#55457 = CARTESIAN_POINT ( 'NONE',  ( -0.1872094492630000107, 1489.066837873730037, 236.5711787574979894 ) ) ;
#55458 = CARTESIAN_POINT ( 'NONE',  ( -1.499721489806784991, 1420.769012360254237, 184.5717010710991701 ) ) ;
#55459 = ORIENTED_EDGE ( 'NONE', *, *, #28161, .F. ) ;
#55460 = CARTESIAN_POINT ( 'NONE',  ( 10.81512807170000023, 1424.921141247430114, 144.1662922863980043 ) ) ;
#55461 = FACE_OUTER_BOUND ( 'NONE', #63696, .T. ) ;
#55462 = CARTESIAN_POINT ( 'NONE',  ( 0.000000000000000000, 1523.051704408389696, 209.1218459616979999 ) ) ;
#55463 = CARTESIAN_POINT ( 'NONE',  ( 7.713117802984999827, 1516.690345681169902, 204.1174038931170003 ) ) ;
#55464 = EDGE_LOOP ( 'NONE', ( #67726, #88657, #12171, #80779 ) ) ;
#55465 = CARTESIAN_POINT ( 'NONE',  ( 9.534480203992039549, 1481.987763606179897, 216.0982299746490014 ) ) ;
#55466 = CIRCLE ( 'NONE', #84057, 30.13701971169416183 ) ;
#55467 = CARTESIAN_POINT ( 'NONE',  ( 12.93986011685568194, 1442.913450493105529, 187.0956378267197238 ) ) ;
#55468 = ORIENTED_EDGE ( 'NONE', *, *, #54207, .T. ) ;
#55469 = VERTEX_POINT ( 'NONE', #31383 ) ;
#55470 = CARTESIAN_POINT ( 'NONE',  ( 2.127574403380531720, 1524.244163922423695, 173.7332312662435925 ) ) ;
#55471 = DIRECTION ( 'NONE',  ( -1.755985294532469921E-16, 1.000000000000000000, -1.338183447452831989E-16 ) ) ;
#55472 = CARTESIAN_POINT ( 'NONE',  ( 10.83634816680000057, 1507.403084768729968, 234.1451693812979897 ) ) ;
#55473 = B_SPLINE_CURVE_WITH_KNOTS ( 'NONE', 3,
 ( #477, #26184, #77174, #59823, #110202, #87220, #10510, #93943, #34601, #97812, #2139, #97266, #96735, #46898, #29509, #37929, #37372, #70450, #11620, #106764, #55294, #21091, #44682, #20542, #36261, #54746 ),
 .UNSPECIFIED., .F., .F.,
 ( 4, 2, 2, 2, 1, 1, 2, 2, 2, 2, 1, 1, 2, 2, 4 ),
 ( 0.000000000000000000, 0.1250000000007177869, 0.2500000000014355739, 0.3750000000021533886, 0.4375000000025118796, 0.4687500000026916247, 0.4843750000027603475, 0.5000000000028289593, 0.6250000000029628522, 0.6875000000030297986, 0.7187500000030208058, 0.7343750000030150327, 0.7421875000029918290, 0.7500000000029686253, 1.000000000000000000 ),
 .UNSPECIFIED. ) ;
#55474 = CARTESIAN_POINT ( 'NONE',  ( -3.364963321921979666, 1469.699125603920038, 218.6607286373120189 ) ) ;
#55475 = CARTESIAN_POINT ( 'NONE',  ( 14.11531660217920070, 1452.420142669970119, 148.4568864021009915 ) ) ;
#55476 = CONICAL_SURFACE ( 'NONE', #98378, 1.000000000000009104, 0.7853981633970000820 ) ;
#55477 = CARTESIAN_POINT ( 'NONE',  ( 8.765535317279999461, 1421.152484001810080, 196.5454161687989938 ) ) ;
#55478 = CARTESIAN_POINT ( 'NONE',  ( 1.874146057977200019, 1474.821289880090035, 220.3858797084459979 ) ) ;
#55479 = CARTESIAN_POINT ( 'NONE',  ( -7.116694769601350501, 1494.227560407549845, 199.0721606401010035 ) ) ;
#55480 = CARTESIAN_POINT ( 'NONE',  ( -119.8718586775642478, 1384.926148861439970, 299.5197653927720580 ) ) ;
#55481 = CARTESIAN_POINT ( 'NONE',  ( -2.500000000000000000, 1440.913060387330006, 209.1218459616979999 ) ) ;
#55483 = CARTESIAN_POINT ( 'NONE',  ( -3.509649680925187365, 1486.092192652074573, 181.9936301291397172 ) ) ;
#55482 = CARTESIAN_POINT ( 'NONE',  ( -18.65765733967990059, 1472.695501767010001, 189.9835944018950329 ) ) ;
#55484 = CARTESIAN_POINT ( 'NONE',  ( -67.00076415386901374, 1379.747503662026475, 277.9341329112440349 ) ) ;
#55485 = CARTESIAN_POINT ( 'NONE',  ( -25.25982536658409927, 1509.711778463150040, 222.8936294031860257 ) ) ;
#55486 = CARTESIAN_POINT ( 'NONE',  ( -7.719525633314999524, 1513.939092156080051, 202.0215813447470055 ) ) ;
#55487 = ORIENTED_EDGE ( 'NONE', *, *, #101556, .F. ) ;
#55488 = CARTESIAN_POINT ( 'NONE',  ( 5.995204332980000249E-15, 1425.981674191730008, 219.6133832206979832 ) ) ;
#55489 = AXIS2_PLACEMENT_3D ( 'NONE', #64370, #99584, #5550 ) ;
#55490 = CARTESIAN_POINT ( 'NONE',  ( -5.257080573758882380, 1517.051704408389924, 199.2452589303538275 ) ) ;
#55491 = CARTESIAN_POINT ( 'NONE',  ( -94.45576590239029713, 1384.959238494370084, 309.9322998303119903 ) ) ;
#55492 = CARTESIAN_POINT ( 'NONE',  ( -9.582177284329999267, 1388.523135097040040, 201.1746843562989966 ) ) ;
#55493 = CARTESIAN_POINT ( 'NONE',  ( -15.48550906000000005, 1416.155796905759871, 210.9866352200689903 ) ) ;
#55495 = ORIENTED_EDGE ( 'NONE', *, *, #80254, .T. ) ;
#55494 = CARTESIAN_POINT ( 'NONE',  ( 3.422247113165846955, 1486.244152127078905, 198.8929547559257287 ) ) ;
#55496 = CARTESIAN_POINT ( 'NONE',  ( 3.483866223379999738, 1429.087410406890058, 216.6553312436790009 ) ) ;
#55497 = DIRECTION ( 'NONE',  ( 0.5224574779883525144, -0.7067418228232951183, -0.4770263929453549823 ) ) ;
#55498 = CARTESIAN_POINT ( 'NONE',  ( -5.569019969264549452, 1475.748224554402441, 217.8649781415279278 ) ) ;
#55499 = CARTESIAN_POINT ( 'NONE',  ( 9.130411372029950456, 1437.290848551490399, 212.9268650149392670 ) ) ;
#55500 = EDGE_CURVE ( 'NONE', #1407, #17819, #52244, .T. ) ;
#55501 = CARTESIAN_POINT ( 'NONE',  ( 14.64758694783500026, 1513.486273623730085, 224.6036928680670144 ) ) ;
#55502 = FACE_OUTER_BOUND ( 'NONE', #45773, .T. ) ;
#55503 = CARTESIAN_POINT ( 'NONE',  ( 2.236590363472370058, 1458.510893503000034, 199.7494169500020007 ) ) ;
#55504 = CARTESIAN_POINT ( 'NONE',  ( 11.87175427299999875, 1419.759279977630058, 229.4984939635980083 ) ) ;
#55505 = CARTESIAN_POINT ( 'NONE',  ( -22.66254714601714326, 1523.342713519622748, 236.8145175431329221 ) ) ;
#55506 = AXIS2_PLACEMENT_3D ( 'NONE', #61340, #95460, #20932 ) ;
#55507 = CARTESIAN_POINT ( 'NONE',  ( -5.013274999515000552, 1517.068517094990057, 206.8347616620369820 ) ) ;
#55508 = CARTESIAN_POINT ( 'NONE',  ( 39.20291624600000091, 1422.646355417429959, 268.9552502776979281 ) ) ;
#55509 = CARTESIAN_POINT ( 'NONE',  ( -18.69670922599999940, 1410.928318842029967, 223.5482325157979915 ) ) ;
#55510 = CARTESIAN_POINT ( 'NONE',  ( 23.19273066879999945, 1435.733997910429935, 140.7572724421980013 ) ) ;
#55511 = CARTESIAN_POINT ( 'NONE',  ( 20.66442127730000067, 1508.014906299830045, 190.0377508468980068 ) ) ;
#55512 = CARTESIAN_POINT ( 'NONE',  ( 19.54819107935938760, 1426.815560993606596, 223.9911639112806654 ) ) ;
#55513 = B_SPLINE_CURVE_WITH_KNOTS ( 'NONE', 3,
 ( #78044, #95956, #44462, #104911, #46134, #96511 ),
 .UNSPECIFIED., .F., .F.,
 ( 4, 2, 4 ),
 ( 8.752084563234713870E-15, 0.0005716314000290802439, 0.001143262800049408374 ),
 .UNSPECIFIED. ) ;
#55514 = CARTESIAN_POINT ( 'NONE',  ( 12.45702690689999947, 1416.837177091229705, 223.4766769983980055 ) ) ;
#55515 = DIRECTION ( 'NONE',  ( -0.000000000000000000, -1.000000000000000000, -0.000000000000000000 ) ) ;
#55516 = CARTESIAN_POINT ( 'NONE',  ( -41.18636360906929639, 1440.753229491839875, 135.3771605954950132 ) ) ;
#55517 = CARTESIAN_POINT ( 'NONE',  ( 0.2111961702294640197, 1456.676537660760005, 183.0956732919689784 ) ) ;
#55518 = CARTESIAN_POINT ( 'NONE',  ( -13.12463360019999925, 1409.312163186730004, 216.5379860103879821 ) ) ;
#55519 = CARTESIAN_POINT ( 'NONE',  ( 0.3823997583379999954, 1418.629108576230010, 184.6943103907979946 ) ) ;
#55520 = VECTOR ( 'NONE', #87014, 1000.000000000000114 ) ;
#55521 = CARTESIAN_POINT ( 'NONE',  ( 20.37381179411471877, 1524.397344074318880, 180.2832293763214579 ) ) ;
#55522 = CARTESIAN_POINT ( 'NONE',  ( 0.1474424791818742808, 1484.358452256622058, 198.4190835461621134 ) ) ;
#55523 = CARTESIAN_POINT ( 'NONE',  ( 13.50135279390000065, 1434.968981356529866, 147.2733250035980177 ) ) ;
#55524 = CARTESIAN_POINT ( 'NONE',  ( -38.86831401713799750, 1437.615293294849835, 134.0999999973729757 ) ) ;
#55525 = CARTESIAN_POINT ( 'NONE',  ( 7.263998328199999577, 1441.808077109380065, 185.0069966186979968 ) ) ;
#55526 = VERTEX_POINT ( 'NONE', #27396 ) ;
#55527 = B_SPLINE_CURVE_WITH_KNOTS ( 'NONE', 3,
 ( #39245, #22412, #56615, #41469, #42558, #76710 ),
 .UNSPECIFIED., .F., .F.,
 ( 4, 2, 4 ),
 ( 1.348807851242469857E-06, 0.1489810127399329998, 0.2938202807443149878 ),
 .UNSPECIFIED. ) ;
#55528 = CARTESIAN_POINT ( 'NONE',  ( 6.023224921602742477, 1510.704533479030715, 216.6230964488122765 ) ) ;
#55529 = CARTESIAN_POINT ( 'NONE',  ( -9.301708524574189951, 1409.237883206610150, 220.8339435818900256 ) ) ;
#55530 = CARTESIAN_POINT ( 'NONE',  ( -11.04529535729999878, 1492.261561399990114, 209.4862125649669906 ) ) ;
#55531 = EDGE_CURVE ( 'NONE', #67122, #99156, #3970, .T. ) ;
#55532 = LINE ( 'NONE', #56070, #24985 ) ;
#55533 = CARTESIAN_POINT ( 'NONE',  ( -15.07741626497340093, 1491.015094518580099, 193.2056053937430136 ) ) ;
#55534 = CARTESIAN_POINT ( 'NONE',  ( 40.49911958459973960, 1425.150115471725485, 269.1156650676614390 ) ) ;
#55535 = CARTESIAN_POINT ( 'NONE',  ( -9.862951377749247683, 1519.551704408389924, 228.3939896778649654 ) ) ;
#55536 = CARTESIAN_POINT ( 'NONE',  ( 18.96350828799999988, 1416.837080254230159, 210.2430641718779896 ) ) ;
#55537 = EDGE_CURVE ( 'NONE', #36366, #77650, #104914, .T. ) ;
#55538 = CARTESIAN_POINT ( 'NONE',  ( 10.73506988043325627, 1424.972993549859893, 139.1354236083641922 ) ) ;
#55539 = CARTESIAN_POINT ( 'NONE',  ( -102.5927908494250005, 1384.595964578270241, 311.0546370185200544 ) ) ;
#55540 = CARTESIAN_POINT ( 'NONE',  ( -32.53064427015559801, 1384.973673283899871, 207.0391211637609956 ) ) ;
#55541 = CARTESIAN_POINT ( 'NONE',  ( -12.02398823846299791, 1491.147743522770043, 206.6805235778679730 ) ) ;
#55542 = CARTESIAN_POINT ( 'NONE',  ( -26.79978786656327827, 1435.433393365130087, 135.4693325801790422 ) ) ;
#55543 = CARTESIAN_POINT ( 'NONE',  ( -27.54197030419999948, 1451.496360562029849, 136.1348864480979728 ) ) ;
#55544 = B_SPLINE_CURVE_WITH_KNOTS ( 'NONE', 5,
 ( #32889, #91153, #99536, #32358, #66537, #92256 ),
 .UNSPECIFIED., .F., .F.,
 ( 6, 6 ),
 ( 330.4685494459999973, 340.5245863399999848 ),
 .UNSPECIFIED. ) ;
#55545 = CARTESIAN_POINT ( 'NONE',  ( -3.350338079455597917, 1523.604703353109699, 176.1628856388066708 ) ) ;
#55547 = EDGE_LOOP ( 'NONE', ( #49595, #89577, #61655, #40431, #77670, #107814 ) ) ;
#55546 = DIRECTION ( 'NONE',  ( -0.6736849260863841948, 0.000000000000000000, 0.7390186874254148774 ) ) ;
#55548 = CARTESIAN_POINT ( 'NONE',  ( -13.92523544520000023, 1509.057792580229943, 183.7758920630979844 ) ) ;
#55549 = CARTESIAN_POINT ( 'NONE',  ( -22.70506393329999995, 1409.705938691230131, 208.9454431684370093 ) ) ;
#55550 = CARTESIAN_POINT ( 'NONE',  ( -4.043437603129999225, 1495.741838748290093, 219.5649473730990167 ) ) ;
#55551 = CARTESIAN_POINT ( 'NONE',  ( -11.59504266670000128, 1415.140114704729967, 195.4687677443980078 ) ) ;
#55552 = AXIS2_PLACEMENT_3D ( 'NONE', #26051, #53512, #44547 ) ;
#55553 = FACE_OUTER_BOUND ( 'NONE', #79822, .T. ) ;
#55554 = CARTESIAN_POINT ( 'NONE',  ( 32.02808312589916540, 1511.187213306747708, 198.2787714533495489 ) ) ;
#55555 = B_SPLINE_SURFACE_WITH_KNOTS ( 'NONE', 5, 1, ( 
 ( #105496, #69147 ),
 ( #53454, #78635 ),
 ( #87599, #9228 ),
 ( #28786, #70830 ),
 ( #37190, #36088 ),
 ( #20362, #10888 ),
 ( #61865, #77534 ),
 ( #43931, #1951 ),
 ( #70273, #104383 ),
 ( #79203, #78075 ),
 ( #69713, #95983 ),
 ( #62986, #103833 ),
 ( #54022, #36634 ),
 ( #27681, #2509 ),
 ( #45060, #97097 ),
 ( #19248, #104940 ),
 ( #28230, #43386 ),
 ( #61319, #62417 ),
 ( #96542, #19817 ),
 ( #88152, #54569 ),
 ( #11440, #3061 ) ),
 .UNSPECIFIED., .F., .F., .F.,
 ( 6, 3, 3, 3, 3, 3, 6 ),
 ( 2, 2 ),
 ( 37.33063420879999939, 38.00991709350000036, 40.59642292560000243, 43.18292875779999918, 44.87875381330000124, 46.52360639289999966, 48.64583233200000478 ),
 ( -0.03002746163920000030, 4.116548514450000695 ),
 .UNSPECIFIED. ) ;
#55556 = CARTESIAN_POINT ( 'NONE',  ( -2.921670480139039849, 1414.947723254120092, 186.4090400968400161 ) ) ;
#55557 = CARTESIAN_POINT ( 'NONE',  ( 0.9782357301829970320, 1463.155161847389991, 230.5295413522989918 ) ) ;
#55558 = CARTESIAN_POINT ( 'NONE',  ( -15.22948377059999814, 1422.122177990030195, 227.7536870161980005 ) ) ;
#55560 = CARTESIAN_POINT ( 'NONE',  ( -12.88669223129999963, 1379.421126886189995, 207.0600552223190221 ) ) ;
#55559 = DIRECTION ( 'NONE',  ( -0.1070030146457249254, 0.000000000000000000, 0.9942586961433763637 ) ) ;
#55561 = CARTESIAN_POINT ( 'NONE',  ( 19.84434320180000100, 1475.251313466289957, 205.2746163281789791 ) ) ;
#55562 = CARTESIAN_POINT ( 'NONE',  ( -102.0933292004540220, 1371.894749952189613, 310.3987085186598165 ) ) ;
#55563 = CARTESIAN_POINT ( 'NONE',  ( 16.69343462643233877, 1526.373507135059526, 234.5422045024349984 ) ) ;
#55564 = CARTESIAN_POINT ( 'NONE',  ( -1.801950444790000105, 1417.382180821630072, 235.5933117588980110 ) ) ;
#55565 = CARTESIAN_POINT ( 'NONE',  ( 9.093835586139999094, 1363.023136422000107, 210.6218459616991936 ) ) ;
#55566 = CARTESIAN_POINT ( 'NONE',  ( -0.7568987378019988999, 1516.805675336850072, 205.0906771642370074 ) ) ;
#55567 = ADVANCED_FACE ( 'NONE', ( #59924 ), #35811, .T. ) ;
#55568 = CARTESIAN_POINT ( 'NONE',  ( -8.437274281626629957, 1485.523202050150076, 184.0031257927479942 ) ) ;
#55569 = ORIENTED_EDGE ( 'NONE', *, *, #82960, .F. ) ;
#55570 = CIRCLE ( 'NONE', #30447, 1.000000000000000888 ) ;
#55571 = CARTESIAN_POINT ( 'NONE',  ( 12.02500756018520178, 1501.456221950489862, 211.6043302210539991 ) ) ;
#55572 = CARTESIAN_POINT ( 'NONE',  ( 17.64235773549999919, 1415.063410501330054, 210.6787325816779912 ) ) ;
#55574 = EDGE_LOOP ( 'NONE', ( #96336, #6244, #98094, #40833 ) ) ;
#55573 = CARTESIAN_POINT ( 'NONE',  ( -68.04880748148440262, 1379.746211451220006, 279.5452075350660266 ) ) ;
#55575 = ORIENTED_EDGE ( 'NONE', *, *, #31533, .T. ) ;
#55576 = CARTESIAN_POINT ( 'NONE',  ( 28.83209696159999780, 1509.870577341629996, 212.5368620444479859 ) ) ;
#55577 = EDGE_LOOP ( 'NONE', ( #13158, #95397, #76100, #9259, #31230 ) ) ;
#55578 = CARTESIAN_POINT ( 'NONE',  ( 5.462208593446796989, 1507.217744690670997, 182.0617134843921292 ) ) ;
#55579 = EDGE_CURVE ( 'NONE', #34578, #66863, #7532, .T. ) ;
#55580 = DIRECTION ( 'NONE',  ( 0.6831251091958939758, -0.2299220283779639940, -0.6931637224008919684 ) ) ;
#55582 = CARTESIAN_POINT ( 'NONE',  ( 33.93019615848946557, 1501.977400791986611, 197.6607374645996060 ) ) ;
#55581 = CARTESIAN_POINT ( 'NONE',  ( 15.78306734642190357, 1414.214202364269795, 191.4131174284399890 ) ) ;
#55583 = CARTESIAN_POINT ( 'NONE',  ( -4.997718276504999224, 1516.693851263360102, 210.2547950466569944 ) ) ;
#55584 = EDGE_CURVE ( 'NONE', #60804, #5142, #38063, .T. ) ;
#55585 = B_SPLINE_CURVE_WITH_KNOTS ( 'NONE', 3,
 ( #42236, #76384, #110533, #70792, #799, #95950, #60721, #1346, #36055, #2478, #8611, #42788, #35485, #76948, #26524, #61285, #257, #87564, #17549, #18664, #69679, #10279, #78038, #62379, #10853, #94843, #43894, #44456, #45025, #52315, #9729 ),
 .UNSPECIFIED., .F., .F.,
 ( 4, 3, 3, 3, 3, 3, 3, 3, 3, 3, 4 ),
 ( -14.48744219459999982, -13.44410458394230012, -12.37566277839809992, -11.18777881828939869, -9.902217085923059159, -8.626592106539620275, -8.281559019981870051, -7.395949616050979891, -6.456807838355668849, -5.467544445957390309, -4.410666364560000829 ),
 .UNSPECIFIED. ) ;
#55586 = CARTESIAN_POINT ( 'NONE',  ( -25.29347491494340261, 1450.804999541210009, 137.5161610977569921 ) ) ;
#55587 = CARTESIAN_POINT ( 'NONE',  ( 10.61724680206623717, 1438.780641373634808, 152.5602674268187400 ) ) ;
#55588 = CARTESIAN_POINT ( 'NONE',  ( 12.45985175859999927, 1409.850499117530035, 228.5793928251979992 ) ) ;
#55589 = CARTESIAN_POINT ( 'NONE',  ( 10.94404851108689947, 1480.986328507249937, 213.6237919197210147 ) ) ;
#55590 = DIRECTION ( 'NONE',  ( 0.000000000000000000, 0.000000000000000000, 1.000000000000000000 ) ) ;
#55591 = ADVANCED_FACE ( 'NONE', ( #68331 ), #61509, .T. ) ;
#55592 = CARTESIAN_POINT ( 'NONE',  ( 41.10614458601939702, 1440.770232258479837, 134.0999999980669770 ) ) ;
#55593 = CARTESIAN_POINT ( 'NONE',  ( -17.68237282055029880, 1517.051704408389924, 205.6847408665509818 ) ) ;
#55594 = ORIENTED_EDGE ( 'NONE', *, *, #64856, .F. ) ;
#55595 = CARTESIAN_POINT ( 'NONE',  ( -8.627754863869999014, 1437.492696374190018, 228.3379673428989918 ) ) ;
#55596 = CARTESIAN_POINT ( 'NONE',  ( -16.73010185348729095, 1410.869507590151898, 226.4351792567899508 ) ) ;
#55597 = EDGE_LOOP ( 'NONE', ( #41198, #35370, #60569, #88764 ) ) ;
#55598 = ORIENTED_EDGE ( 'NONE', *, *, #75383, .F. ) ;
#55599 = EDGE_LOOP ( 'NONE', ( #69142, #110641, #44896, #8700, #45952, #15478, #16694, #14251, #9291, #13801 ) ) ;
#55600 = EDGE_CURVE ( 'NONE', #46077, #2310, #87459, .T. ) ;
#55601 = CARTESIAN_POINT ( 'NONE',  ( -6.321172872105000451, 1513.830194289070278, 216.6922650853570076 ) ) ;
#55602 = CARTESIAN_POINT ( 'NONE',  ( -14.59279134157089963, 1436.244781760590058, 149.8708244536879874 ) ) ;
#55603 = AXIS2_PLACEMENT_3D ( 'NONE', #28623, #104227, #105892 ) ;
#55604 = CARTESIAN_POINT ( 'NONE',  ( 12.30351751032840113, 1499.827690331060012, 206.1221001624080031 ) ) ;
#55605 = CARTESIAN_POINT ( 'NONE',  ( -2.959096334900000347, 1485.522887684729994, 182.9002838673980023 ) ) ;
#55606 = CARTESIAN_POINT ( 'NONE',  ( -17.08557393600510821, 1449.031093638705670, 219.2146613812218447 ) ) ;
#55607 = CARTESIAN_POINT ( 'NONE',  ( -66.61252592013686069, 1379.743324869505159, 275.6254950077977242 ) ) ;
#55608 = CARTESIAN_POINT ( 'NONE',  ( -3.160946274158207281, 1370.089580311054988, 210.3387270294440157 ) ) ;
#55609 = CARTESIAN_POINT ( 'NONE',  ( 28.25086641300000068, 1508.135711190629991, 209.3856964555159834 ) ) ;
#55610 = CARTESIAN_POINT ( 'NONE',  ( 6.194272744020000054, 1415.931669658029932, 192.0649073719980038 ) ) ;
#55611 = EDGE_CURVE ( 'NONE', #105306, #68439, #91553, .T. ) ;
#55612 = CARTESIAN_POINT ( 'NONE',  ( -60.11345111107429773, 1384.673691186940005, 244.2542627049520263 ) ) ;
#55613 = VERTEX_POINT ( 'NONE', #98457 ) ;
#55614 = CARTESIAN_POINT ( 'NONE',  ( 6.546001350565000543, 1516.557392317769882, 207.4118413833070065 ) ) ;
#55615 = ORIENTED_EDGE ( 'NONE', *, *, #27805, .T. ) ;
#55616 = CARTESIAN_POINT ( 'NONE',  ( 11.30241272459999990, 1414.983771848930019, 222.3815203751980221 ) ) ;
#55617 = AXIS2_PLACEMENT_3D ( 'NONE', #64754, #14852, #99405 ) ;
#55618 = CARTESIAN_POINT ( 'NONE',  ( -0.002288667334423727731, 1451.798321715683869, 154.0444463031279270 ) ) ;
#55619 = EDGE_LOOP ( 'NONE', ( #14995, #4831, #71179, #88213 ) ) ;
#55620 = CARTESIAN_POINT ( 'NONE',  ( -17.83486663330526767, 1523.678648413191695, 180.3677388339002334 ) ) ;
#55621 = CARTESIAN_POINT ( 'NONE',  ( -15.43255204080000098, 1409.451976979829851, 192.6616394286979812 ) ) ;
#55622 = CARTESIAN_POINT ( 'NONE',  ( -6.871715297787709176, 1517.299312825780135, 183.7897170437481407 ) ) ;
#55623 = EDGE_CURVE ( 'NONE', #97990, #84088, #41440, .T. ) ;
#55624 = CARTESIAN_POINT ( 'NONE',  ( -24.15153490410000359, 1438.063247892820073, 212.1983423404379892 ) ) ;
#55625 = CARTESIAN_POINT ( 'NONE',  ( -7.163586313923399729, 1435.603035147609944, 215.7022475339200014 ) ) ;
#55626 = CARTESIAN_POINT ( 'NONE',  ( -5.570674267431350302, 1511.275365984429982, 201.2227656140939871 ) ) ;
#55627 = CARTESIAN_POINT ( 'NONE',  ( 21.85509849029999785, 1410.191647020929850, 266.7712709411979972 ) ) ;
#55628 = EDGE_CURVE ( 'NONE', #87844, #80209, #55849, .T. ) ;
#55629 = CARTESIAN_POINT ( 'NONE',  ( -5.707844849875344906, 1510.531931279475430, 201.5760423114203377 ) ) ;
#55630 = CARTESIAN_POINT ( 'NONE',  ( -22.03465957474402259, 1522.644714754858796, 182.8300405912373492 ) ) ;
#55632 = CARTESIAN_POINT ( 'NONE',  ( -23.10442739037580040, 1411.095127590459924, 210.9251608898400150 ) ) ;
#55631 = CARTESIAN_POINT ( 'NONE',  ( 6.158422142889999229, 1465.359135116529842, 233.6544522023980051 ) ) ;
#55633 = CARTESIAN_POINT ( 'NONE',  ( 7.718763505904999711, 1516.905946377369901, 216.0642002436470079 ) ) ;
#55634 = ADVANCED_FACE ( 'NONE', ( #90607 ), #30427, .F. ) ;
#55635 = PLANE ( 'NONE',  #28311 ) ;
#55636 = DIRECTION ( 'NONE',  ( 0.9858563016923833633, 0.000000000000000000, 0.1675928173085483863 ) ) ;
#55637 = CARTESIAN_POINT ( 'NONE',  ( 17.29245831912049525, 1448.484397839388748, 218.0081137152410520 ) ) ;
#55638 = CARTESIAN_POINT ( 'NONE',  ( 5.786527562335000319, 1517.025653221279981, 212.5728793591970032 ) ) ;
#55639 = CARTESIAN_POINT ( 'NONE',  ( -11.67352926041350081, 1482.512923242310080, 206.7897318267789899 ) ) ;
#55640 =( BOUNDED_CURVE ( )  B_SPLINE_CURVE ( 3, ( #32930, #92840, #101220, #16116 ),
 .UNSPECIFIED., .F., .F. ) 
 B_SPLINE_CURVE_WITH_KNOTS ( ( 4, 4 ),
 ( 1.104799058897792063, 2.035744924573262615 ),
 .UNSPECIFIED. ) 
 CURVE ( )  GEOMETRIC_REPRESENTATION_ITEM ( )  RATIONAL_B_SPLINE_CURVE ( ( 1.000000000000000000, 0.9290729278587501749, 0.9290729278587501749, 1.000000000000000000 ) ) 
 REPRESENTATION_ITEM ( '' )  );
#55641 = CARTESIAN_POINT ( 'NONE',  ( 14.63781025022767679, 1454.494882998578305, 195.9652644489082149 ) ) ;
#55643 = EDGE_LOOP ( 'NONE', ( #70556, #27726, #109102, #619, #37117 ) ) ;
#55642 = CARTESIAN_POINT ( 'NONE',  ( -10.31471925920000032, 1423.142082606249915, 193.7320793877989900 ) ) ;
#55644 = CARTESIAN_POINT ( 'NONE',  ( -1.912903644476058096, 1526.104292489130557, 177.3592290664108759 ) ) ;
#55645 = CARTESIAN_POINT ( 'NONE',  ( 4.127212203990000106, 1462.218800617230045, 225.7558667919979882 ) ) ;
#55646 = CARTESIAN_POINT ( 'NONE',  ( -11.86315348299999961, 1432.130050080510046, 149.9794296056979874 ) ) ;
#55647 = CARTESIAN_POINT ( 'NONE',  ( -15.11314298410000134, 1415.677402202029953, 207.9092237183590157 ) ) ;
#55648 = CARTESIAN_POINT ( 'NONE',  ( 1.978507516889999929, 1415.911868808130066, 232.2613842265979827 ) ) ;
#55649 = CARTESIAN_POINT ( 'NONE',  ( 11.29707874440000026, 1420.194464914089849, 198.6147532060990102 ) ) ;
#55650 = CARTESIAN_POINT ( 'NONE',  ( -1.736874410247479794, 1445.847355267769899, 215.2372654443830129 ) ) ;
#55652 = CARTESIAN_POINT ( 'NONE',  ( 2.500000000000000000, 1431.146244464689971, 157.4674042686979760 ) ) ;
#55651 = CARTESIAN_POINT ( 'NONE',  ( -18.83990731639999794, 1444.807220488899929, 226.1209739433980133 ) ) ;
#55653 = CARTESIAN_POINT ( 'NONE',  ( -12.47575420717869932, 1379.153280478169791, 210.8825727293119883 ) ) ;
#55654 = ORIENTED_EDGE ( 'NONE', *, *, #43794, .F. ) ;
#55655 = CARTESIAN_POINT ( 'NONE',  ( -4.622842882315000068, 1516.901952101700090, 205.0913314195169903 ) ) ;
#55656 = CARTESIAN_POINT ( 'NONE',  ( 2.731915039460000028, 1406.836420814830035, 269.6477045013979819 ) ) ;
#55657 = AXIS2_PLACEMENT_3D ( 'NONE', #91406, #65662, #14683 ) ;
#55658 = CARTESIAN_POINT ( 'NONE',  ( -22.62861454470000311, 1507.212883763329955, 208.5231287359179930 ) ) ;
#55659 = EDGE_CURVE ( 'NONE', #7904, #98527, #109627, .T. ) ;
#55660 = CARTESIAN_POINT ( 'NONE',  ( 24.16540420446059656, 1436.369459095317779, 213.4347722490431352 ) ) ;
#55661 = EDGE_CURVE ( 'NONE', #53402, #98048, #59436, .T. ) ;
#55662 = CARTESIAN_POINT ( 'NONE',  ( 3.350944662710000355, 1464.628126271390101, 199.8699733667390035 ) ) ;
#55663 = DIRECTION ( 'NONE',  ( 0.4035202328300511176, 0.000000000000000000, 0.9149707217702551798 ) ) ;
#55664 = CARTESIAN_POINT ( 'NONE',  ( -10.27502231191230031, 1447.498783342189881, 210.3549345117849896 ) ) ;
#55665 = CARTESIAN_POINT ( 'NONE',  ( -2.500592283260189674, 1448.944489445770159, 154.5202668489739892 ) ) ;
#55666 = CARTESIAN_POINT ( 'NONE',  ( -1.574589970354772550, 1451.357591668891246, 183.8674059166829693 ) ) ;
#55667 = CARTESIAN_POINT ( 'NONE',  ( 1.456572784391380049, 1450.690862361819882, 154.5176451698619928 ) ) ;
#55668 = CARTESIAN_POINT ( 'NONE',  ( -105.4624709189999834, 1391.255327103129957, 304.2078109453590287 ) ) ;
#55669 = CARTESIAN_POINT ( 'NONE',  ( 0.000000000000000000, 1523.382868172864164, 209.1218459616979999 ) ) ;
#55670 = VECTOR ( 'NONE', #79755, 999.9999999999998863 ) ;
#55671 = CARTESIAN_POINT ( 'NONE',  ( -21.37693747720000204, 1438.522492593769812, 224.8635562210979799 ) ) ;
#55672 = EDGE_CURVE ( 'NONE', #18275, #107129, #54163, .T. ) ;
#55673 = CARTESIAN_POINT ( 'NONE',  ( 10.85996935512256201, 1424.791572806463819, 138.1869648445997996 ) ) ;
#55674 = CARTESIAN_POINT ( 'NONE',  ( 2.711756486579999681, 1440.323160983029993, 158.1834442036979738 ) ) ;
#55675 = CIRCLE ( 'NONE', #7370, 2.000000000000001776 ) ;
#55676 = CARTESIAN_POINT ( 'NONE',  ( -0.7781449114299999748, 1476.045365520429868, 268.4835185334979997 ) ) ;
#55677 = DIRECTION ( 'NONE',  ( 1.149679124779773953E-17, 1.000000000000000000, -1.829746454213089849E-16 ) ) ;
#55678 = CARTESIAN_POINT ( 'NONE',  ( -11.11248229347330430, 1512.836812602111877, 193.0596162085393814 ) ) ;
#55679 = CARTESIAN_POINT ( 'NONE',  ( -2.971350363272212025, 1448.268441440509150, 184.4301633348362657 ) ) ;
#55680 = CARTESIAN_POINT ( 'NONE',  ( -37.03571219771700385, 1384.800574037690012, 237.2200498466380054 ) ) ;
#55681 = CARTESIAN_POINT ( 'NONE',  ( -3.727807290641250049, 1517.051706635029859, 215.7383534543289727 ) ) ;
#55682 = CARTESIAN_POINT ( 'NONE',  ( 0.7162863658319988946, 1429.709265593189912, 217.4063670190490143 ) ) ;
#55683 = CARTESIAN_POINT ( 'NONE',  ( 30.90487439922549484, 1525.907212628473644, 216.4335774778779466 ) ) ;
#55684 = CARTESIAN_POINT ( 'NONE',  ( 8.335839316101193219, 1511.410080502129176, 204.6879527979276929 ) ) ;
#55685 = CARTESIAN_POINT ( 'NONE',  ( -8.049959547940961357, 1396.194171169660194, 216.6974182996600007 ) ) ;
#55686 = VECTOR ( 'NONE', #29762, 999.9999999999998863 ) ;
#55687 = CARTESIAN_POINT ( 'NONE',  ( -15.51819189429999923, 1420.489765463529920, 227.0243196332980062 ) ) ;
#55688 = EDGE_CURVE ( 'NONE', #85013, #21616, #57039, .T. ) ;
#55689 = CARTESIAN_POINT ( 'NONE',  ( -45.63712941939999723, 1440.717835916950207, 268.9747522934979997 ) ) ;
#55690 = ORIENTED_EDGE ( 'NONE', *, *, #52210, .T. ) ;
#55691 = CARTESIAN_POINT ( 'NONE',  ( -6.907011062519999633, 1472.523400736590020, 209.7330543039639963 ) ) ;
#55692 = CARTESIAN_POINT ( 'NONE',  ( -15.59264667799007498, 1415.962102148422218, 208.0126982715246697 ) ) ;
#55693 = CARTESIAN_POINT ( 'NONE',  ( -11.78818130396880015, 1426.417830932260131, 148.5075460829759777 ) ) ;
#55694 = AXIS2_PLACEMENT_3D ( 'NONE', #98456, #82766, #64889 ) ;
#55696 = CARTESIAN_POINT ( 'NONE',  ( -11.92849872886499973, 1511.839858410419993, 194.1166199672670132 ) ) ;
#55695 = CARTESIAN_POINT ( 'NONE',  ( 11.34209814579999964, 1426.458889724530081, 115.7217992701980052 ) ) ;
#55697 = CARTESIAN_POINT ( 'NONE',  ( 11.62807272172398498, 1428.982488964479899, 136.1186897298417477 ) ) ;
#55698 = EDGE_CURVE ( 'NONE', #34842, #25016, #8698, .T. ) ;
#55699 = CARTESIAN_POINT ( 'NONE',  ( -30.30080019752890053, 1526.189892541618974, 201.5450448376013810 ) ) ;
#55700 = CARTESIAN_POINT ( 'NONE',  ( -6.555393155154999540, 1516.809497469189864, 201.7937966518470034 ) ) ;
#55701 = CARTESIAN_POINT ( 'NONE',  ( 8.054683762439999839, 1427.717696033889979, 212.5858566009490005 ) ) ;
#55702 = CARTESIAN_POINT ( 'NONE',  ( -4.705736654490000781, 1479.984769897790102, 230.9466533013989817 ) ) ;
#55703 = CARTESIAN_POINT ( 'NONE',  ( 5.462208597450000092, 1507.217744391630049, 182.0617134992979800 ) ) ;
#55704 = DIRECTION ( 'NONE',  ( -0.000000000000000000, -1.000000000000000000, -0.000000000000000000 ) ) ;
#55705 = CARTESIAN_POINT ( 'NONE',  ( -86.17839381677090671, 1377.185129373109930, 302.3619043579220147 ) ) ;
#55706 = TOROIDAL_SURFACE ( 'NONE', #48582, 8.013264357029999729, 0.5000000000000000000 ) ;
#55707 = CARTESIAN_POINT ( 'NONE',  ( 6.018929517001535778, 1367.483508091049089, 207.6218459616988241 ) ) ;
#55709 = ORIENTED_EDGE ( 'NONE', *, *, #78836, .F. ) ;
#55708 = CARTESIAN_POINT ( 'NONE',  ( 8.503372964620000474, 1452.005661874290126, 212.9202014103589988 ) ) ;
#55710 = ORIENTED_EDGE ( 'NONE', *, *, #91022, .T. ) ;
#55711 = CARTESIAN_POINT ( 'NONE',  ( -10.86323185920000078, 1396.351599766229810, 203.8926020820279916 ) ) ;
#55712 = DIRECTION ( 'NONE',  ( -0.8926073982886787439, -0.4508348173337058951, 0.000000000000000000 ) ) ;
#55713 = CARTESIAN_POINT ( 'NONE',  ( -0.9518847404100000409, 1415.296882282229944, 227.0497707501980074 ) ) ;
#55714 = CARTESIAN_POINT ( 'NONE',  ( -13.51610093808350754, 1443.925812197481491, 169.3501091255432982 ) ) ;
#55715 = EDGE_CURVE ( 'NONE', #73362, #39044, #21965, .T. ) ;
#55716 = CARTESIAN_POINT ( 'NONE',  ( -113.3764034147090882, 1389.413060387289988, 303.2221243954415968 ) ) ;
#55717 = CARTESIAN_POINT ( 'NONE',  ( 15.23962836178434799, 1416.181292664740113, 211.4166089860522106 ) ) ;
#55719 = CARTESIAN_POINT ( 'NONE',  ( 17.29603771190000217, 1410.862603898330008, 225.9904529778980304 ) ) ;
#55718 = CARTESIAN_POINT ( 'NONE',  ( -7.767750813309999280, 1384.590689248749868, 218.9085672489989918 ) ) ;
#55720 = FACE_OUTER_BOUND ( 'NONE', #84786, .T. ) ;
#55721 = EDGE_CURVE ( 'NONE', #13675, #49086, #110722, .T. ) ;
#55722 = CARTESIAN_POINT ( 'NONE',  ( -2.280862363224759992, 1463.582457375659942, 199.5877073955589935 ) ) ;
#55723 = CARTESIAN_POINT ( 'NONE',  ( -40.62462454117719801, 1446.670089421630109, 136.4950496779409832 ) ) ;
#55724 = CARTESIAN_POINT ( 'NONE',  ( 10.91486054658139970, 1396.294215716539838, 207.2818781998020086 ) ) ;
#55725 = DIRECTION ( 'NONE',  ( 1.836970198721029688E-16, 1.000000000000000000, 0.000000000000000000 ) ) ;
#55726 = CARTESIAN_POINT ( 'NONE',  ( 11.82844634479999968, 1429.628886368029953, 149.7692666886979964 ) ) ;
#55727 = DIRECTION ( 'NONE',  ( 1.224646799147350002E-16, -1.836970198721029688E-16, -1.000000000000000000 ) ) ;
#55728 = EDGE_LOOP ( 'NONE', ( #9167, #64146, #15966, #17662 ) ) ;
#55729 = CARTESIAN_POINT ( 'NONE',  ( 20.92528168611880091, 1525.790286462510039, 233.2531892700154685 ) ) ;
#55730 = EDGE_LOOP ( 'NONE', ( #19760, #100454, #37880 ) ) ;
#55731 = VERTEX_POINT ( 'NONE', #102308 ) ;
#55732 = ADVANCED_FACE ( 'NONE', ( #18300 ), #33443, .T. ) ;
#55733 = CARTESIAN_POINT ( 'NONE',  ( -18.33192216791169926, 1488.027226577300098, 229.1094005703429843 ) ) ;
#55734 = CARTESIAN_POINT ( 'NONE',  ( 20.99932333639999982, 1495.227718574589971, 211.1881774286989923 ) ) ;
#55735 = CARTESIAN_POINT ( 'NONE',  ( -13.34220071569999888, 1434.810047171210044, 195.4053903379979999 ) ) ;
#55736 = CARTESIAN_POINT ( 'NONE',  ( -28.49879435372614722, 1526.382868172571079, 198.4011524119066507 ) ) ;
#55737 = CARTESIAN_POINT ( 'NONE',  ( -3.449777353855000062, 1516.974592746400049, 214.1332139170270068 ) ) ;
#55738 = CARTESIAN_POINT ( 'NONE',  ( -13.07885320302169951, 1380.091007900090062, 209.8378948098500132 ) ) ;
#55739 = PRESENTATION_LAYER_ASSIGNMENT (  '', '', ( #68204 ) ) ;
#55740 = EDGE_CURVE ( 'NONE', #9564, #42097, #73749, .T. ) ;
#55741 = ORIENTED_EDGE ( 'NONE', *, *, #23070, .F. ) ;
#55742 = CARTESIAN_POINT ( 'NONE',  ( -17.90721988768679651, 1508.493835039639862, 211.9093185509239845 ) ) ;
#55743 = CARTESIAN_POINT ( 'NONE',  ( 2.500000000000000000, 1448.668275834809947, 158.2599144857439910 ) ) ;
#55744 = CARTESIAN_POINT ( 'NONE',  ( -50.85477211639999950, 1380.010081756269983, 242.1550097551590000 ) ) ;
#55745 = TOROIDAL_SURFACE ( 'NONE', #57500, 12.73448142120000171, 1.000000000000000000 ) ;
#55746 = CARTESIAN_POINT ( 'NONE',  ( 17.56697300799999795, 1414.971439108430104, 210.2828043877179880 ) ) ;
#55747 = CARTESIAN_POINT ( 'NONE',  ( -5.785582951674999919, 1516.981965530290154, 205.0894480302270040 ) ) ;
#55748 = ORIENTED_EDGE ( 'NONE', *, *, #49017, .F. ) ;
#55749 = CARTESIAN_POINT ( 'NONE',  ( -11.80334333584940154, 1489.554055793390035, 212.2407443684180066 ) ) ;
#55750 = CARTESIAN_POINT ( 'NONE',  ( -39.37261225819499799, 1430.225544555710712, 269.5993096230814672 ) ) ;
#55751 = CARTESIAN_POINT ( 'NONE',  ( -1.541545454019999983, 1409.134736275329942, 232.3518812819980326 ) ) ;
#55753 = ORIENTED_EDGE ( 'NONE', *, *, #106886, .T. ) ;
#55752 = CARTESIAN_POINT ( 'NONE',  ( -1.910176461450000064E-10, 1497.713060387329961, 187.5067198890980080 ) ) ;
#55754 = EDGE_CURVE ( 'NONE', #98450, #44161, #43534, .T. ) ;
#55755 = CYLINDRICAL_SURFACE ( 'NONE', #31497, 0.4999999999999449329 ) ;
#55756 = CARTESIAN_POINT ( 'NONE',  ( -30.92058080866769743, 1440.913060387919813, 241.1530792290629961 ) ) ;
#55757 = CARTESIAN_POINT ( 'NONE',  ( -1.364749936328269942E-15, 1384.563555726449977, 218.6218459572590120 ) ) ;
#55758 = CARTESIAN_POINT ( 'NONE',  ( -0.3266760126305189860, 1466.747039041310018, 235.5969266249480256 ) ) ;
#55759 = AXIS2_PLACEMENT_3D ( 'NONE', #94619, #7316, #101902 ) ;
#55760 = CARTESIAN_POINT ( 'NONE',  ( 19.91918620360440428, 1413.854353960929984, 269.3861823084499747 ) ) ;
#55761 = EDGE_CURVE ( 'NONE', #7383, #62909, #76732, .T. ) ;
#55762 = CARTESIAN_POINT ( 'NONE',  ( -3.253462098795000035, 1516.874084700499907, 212.5832060635069922 ) ) ;
#55763 = CARTESIAN_POINT ( 'NONE',  ( -59.96754922390000075, 1379.749011644449865, 261.8279529299589967 ) ) ;
#55764 = B_SPLINE_CURVE_WITH_KNOTS ( 'NONE', 3,
 ( #36318, #98292, #21566, #95683 ),
 .UNSPECIFIED., .F., .F.,
 ( 4, 4 ),
 ( 55.36930458839999858, 55.41785034089999584 ),
 .UNSPECIFIED. ) ;
#55765 = CARTESIAN_POINT ( 'NONE',  ( 23.71865610989999951, 1410.976819930530155, 207.9578859000980060 ) ) ;
#55766 = FACE_OUTER_BOUND ( 'NONE', #72888, .T. ) ;
#55767 = CARTESIAN_POINT ( 'NONE',  ( 10.29570781656459921, 1425.935951659160082, 194.3061580000300239 ) ) ;
#55768 = CARTESIAN_POINT ( 'NONE',  ( -11.60004869885203505, 1425.328126621067440, 136.8077491627233542 ) ) ;
#55769 = CARTESIAN_POINT ( 'NONE',  ( -1.117840124865000062, 1516.949031626070109, 210.8389850543470061 ) ) ;
#55770 = CARTESIAN_POINT ( 'NONE',  ( 4.173620666753329544, 1421.345241524500125, 185.1232336757030055 ) ) ;
#55771 = CARTESIAN_POINT ( 'NONE',  ( -2.809255954350000195, 1417.912686254329856, 232.9149847042980070 ) ) ;
#55772 = CARTESIAN_POINT ( 'NONE',  ( -89.65022158889999560, 1384.970293222339933, 308.7482827413589348 ) ) ;
#55773 = VERTEX_POINT ( 'NONE', #84421 ) ;
#55775 = VECTOR ( 'NONE', #50537, 1000.000000000000000 ) ;
#55774 = CARTESIAN_POINT ( 'NONE',  ( -28.44980152130050044, 1385.240686751639942, 226.4935510166359904 ) ) ;
#55776 = CARTESIAN_POINT ( 'NONE',  ( 42.46024960829999628, 1454.582938856229930, 266.3335672127980160 ) ) ;
#55777 =( BOUNDED_SURFACE ( )  B_SPLINE_SURFACE ( 3, 2, ( 
 ( #96402, #92659, #35949 ),
 ( #33299, #70135, #76419 ),
 ( #110573, #93745, #16480 ),
 ( #93211, #52754, #19110 ),
 ( #78499, #101597, #1813 ),
 ( #19679, #24882, #104798 ),
 ( #104247, #87455, #79068 ),
 ( #27537, #61720, #95842 ),
 ( #70685, #59089, #28086 ),
 ( #53313, #50670, #15934 ) ),
 .UNSPECIFIED., .F., .F., .T. ) 
 B_SPLINE_SURFACE_WITH_KNOTS ( ( 4, 2, 2, 2, 4 ),
 ( 3, 3 ),
 ( 0.000000000000000000, 0.3926990816987241395, 0.7853981633974482790, 1.178097245096172418, 1.570796326794896558 ),
 ( 0.000000000000000000, 1.000000000000000000 ),
 .UNSPECIFIED. ) 
 GEOMETRIC_REPRESENTATION_ITEM ( )  RATIONAL_B_SPLINE_SURFACE ( (
 ( 1.000000000000000000, 0.7763623250684352772, 1.000000000000000000),
 ( 1.000000000000000000, 0.7763684247034601249, 1.000000000000000000),
 ( 1.000000000000000000, 0.7746454561798020721, 1.000000000000000000),
 ( 1.000000000000000000, 0.7679730451972409666, 1.000000000000000000),
 ( 1.000000000000000000, 0.7630177051947608646, 1.000000000000000000),
 ( 1.000000000000000000, 0.7504512394527353969, 1.000000000000000000),
 ( 1.000000000000000000, 0.7428408967928123996, 1.000000000000000000),
 ( 1.000000000000000000, 0.7259222650909311625, 1.000000000000000000),
 ( 1.000000000000000000, 0.7166207884820420260, 1.000000000000000000),
 ( 1.000000000000000000, 0.7071067811865825448, 1.000000000000000000) ) ) 
 REPRESENTATION_ITEM ( '' )  SURFACE ( )  );
#55778 = CARTESIAN_POINT ( 'NONE',  ( 4.678155166859202296, 1508.611350403214146, 206.6339108396268784 ) ) ;
#55779 = CARTESIAN_POINT ( 'NONE',  ( -108.2502590933346198, 1306.913060387289988, 307.0351622366206357 ) ) ;
#55780 = CARTESIAN_POINT ( 'NONE',  ( 10.94554652600000111, 1425.626382808379958, 206.1464673162289785 ) ) ;
#55781 = CARTESIAN_POINT ( 'NONE',  ( 0.07104776210500948763, 1498.478595971874256, 197.7944178200672809 ) ) ;
#55782 = CARTESIAN_POINT ( 'NONE',  ( 5.005071008295000290, 1516.710692850270107, 216.4473877573669824 ) ) ;
#55783 = CARTESIAN_POINT ( 'NONE',  ( 18.18137294690000161, 1507.546748832429785, 186.5307135875980009 ) ) ;
#55784 = CARTESIAN_POINT ( 'NONE',  ( 10.05617058044520107, 1469.475797196530038, 208.7796867827769915 ) ) ;
#55785 = ORIENTED_EDGE ( 'NONE', *, *, #24089, .T. ) ;
#55786 = CARTESIAN_POINT ( 'NONE',  ( 6.941727252324999320, 1516.882217593000178, 201.7906628411569727 ) ) ;
#55787 = CARTESIAN_POINT ( 'NONE',  ( -15.90990259576500065, 1512.830284628050094, 220.0820010595669771 ) ) ;
#55788 = ORIENTED_EDGE ( 'NONE', *, *, #92675, .F. ) ;
#55789 = VECTOR ( 'NONE', #73107, 1000.000000000000000 ) ;
#55790 = CARTESIAN_POINT ( 'NONE',  ( 12.93678125246493593, 1396.364822743412560, 211.1704015715083358 ) ) ;
#55791 = CARTESIAN_POINT ( 'NONE',  ( 10.76227128012812173, 1434.602751777355252, 151.9483663934211108 ) ) ;
#55792 = CARTESIAN_POINT ( 'NONE',  ( 7.762807725464860198, 1423.432002036965287, 195.8271426519320073 ) ) ;
#55793 = CARTESIAN_POINT ( 'NONE',  ( 2.254749836789999851, 1442.631473631490053, 217.8400976104589972 ) ) ;
#55794 = CARTESIAN_POINT ( 'NONE',  ( -26.60410256373840099, 1508.905103705679949, 201.4398633433799830 ) ) ;
#55795 = CARTESIAN_POINT ( 'NONE',  ( 5.020440211750000437, 1420.408409142929941, 185.9185919516980334 ) ) ;
#55796 = CARTESIAN_POINT ( 'NONE',  ( -18.69185054180000094, 1425.386843902630062, 225.0351303875980022 ) ) ;
#55797 = CARTESIAN_POINT ( 'NONE',  ( -24.31326452180000075, 1436.157794028729995, 139.2594885554979953 ) ) ;
#55798 = CARTESIAN_POINT ( 'NONE',  ( -105.1057160200000027, 1389.703205635770018, 300.9611973728590328 ) ) ;
#55799 = CARTESIAN_POINT ( 'NONE',  ( 17.74011895019999940, 1509.475909745830222, 187.0027172725980051 ) ) ;
#55801 = CARTESIAN_POINT ( 'NONE',  ( 28.47876010940000313, 1509.161042319729859, 209.2859733393400177 ) ) ;
#55800 = CARTESIAN_POINT ( 'NONE',  ( -106.4020475519999991, 1391.913060387289988, 304.2007934394590620 ) ) ;
#55802 = DIRECTION ( 'NONE',  ( 0.3090169943749582204, 0.000000000000000000, 0.9510565162951500895 ) ) ;
#55803 = ORIENTED_EDGE ( 'NONE', *, *, #88465, .T. ) ;
#55804 = CARTESIAN_POINT ( 'NONE',  ( -104.1991720430000186, 1379.825027202220099, 304.0120836943589779 ) ) ;
#55805 = CARTESIAN_POINT ( 'NONE',  ( -8.229715745860000098, 1508.551704408389924, 218.8951070726089938 ) ) ;
#55806 = LINE ( 'NONE', #46853, #8510 ) ;
#55807 = CARTESIAN_POINT ( 'NONE',  ( 11.32877768939290064, 1470.635785175149977, 208.0137898554069977 ) ) ;
#55808 = CARTESIAN_POINT ( 'NONE',  ( -6.025153380789999957, 1484.743691390089907, 198.8560516573990071 ) ) ;
#55809 = CARTESIAN_POINT ( 'NONE',  ( -18.54307511480000059, 1508.238692188029972, 229.7339851843979943 ) ) ;
#55810 = CARTESIAN_POINT ( 'NONE',  ( -2.744860007232919674, 1525.790287071781449, 240.9440838819185160 ) ) ;
#55811 = CARTESIAN_POINT ( 'NONE',  ( -12.71757234210196863, 1442.815512338947428, 186.1937126296973588 ) ) ;
#55812 = CARTESIAN_POINT ( 'NONE',  ( 6.251338861372889966, 1407.163727730510118, 197.0599927605450148 ) ) ;
#55813 = CARTESIAN_POINT ( 'NONE',  ( 2.551826806925589608, 1494.220102795730099, 219.9851886801529872 ) ) ;
#55814 = CARTESIAN_POINT ( 'NONE',  ( -22.19118107542460194, 1483.601927841320048, 216.8115131704170153 ) ) ;
#55815 = CARTESIAN_POINT ( 'NONE',  ( -14.78101880266670065, 1415.677402202059966, 206.5097581168130034 ) ) ;
#55816 = CYLINDRICAL_SURFACE ( 'NONE', #10746, 7.500000000000000000 ) ;
#55817 = CARTESIAN_POINT ( 'NONE',  ( 7.039730798329999928, 1428.888324978490118, 214.9446073011990279 ) ) ;
#55818 = FACE_OUTER_BOUND ( 'NONE', #82007, .T. ) ;
#55819 = CARTESIAN_POINT ( 'NONE',  ( -109.9987472859999968, 1381.043808635240111, 309.4164141372589825 ) ) ;
#55820 = CARTESIAN_POINT ( 'NONE',  ( -0.4967073565345429542, 1415.438070636819930, 233.3911243540180180 ) ) ;
#55821 = VERTEX_POINT ( 'NONE', #7706 ) ;
#55822 = ORIENTED_EDGE ( 'NONE', *, *, #40027, .T. ) ;
#55823 = CARTESIAN_POINT ( 'NONE',  ( 16.93235272047269646, 1414.913060387399810, 210.7966751255959821 ) ) ;
#55824 = CARTESIAN_POINT ( 'NONE',  ( -109.7178227269999979, 1384.906453685299994, 297.0861895859590049 ) ) ;
#55825 = CARTESIAN_POINT ( 'NONE',  ( -8.860592775618536976, 1381.856380555122996, 200.4166704413667333 ) ) ;
#55827 = CARTESIAN_POINT ( 'NONE',  ( -25.82475785010000280, 1456.303105448329916, 244.3435519225979817 ) ) ;
#55826 = CARTESIAN_POINT ( 'NONE',  ( 38.34354232409781815, 1428.425844903683128, 269.5819412675198237 ) ) ;
#55828 = CARTESIAN_POINT ( 'NONE',  ( -19.96238765929999914, 1499.092665092829975, 189.4473116693979762 ) ) ;
#55829 = CARTESIAN_POINT ( 'NONE',  ( -11.30827943520000112, 1433.910506711959897, 151.5171036033979988 ) ) ;
#55830 = CIRCLE ( 'NONE', #7529, 2.000000000000000000 ) ;
#55831 = LINE ( 'NONE', #65877, #106931 ) ;
#55832 = CARTESIAN_POINT ( 'NONE',  ( -19.49048793740000107, 1485.728846214529995, 189.9928713767980071 ) ) ;
#55833 = CARTESIAN_POINT ( 'NONE',  ( 31.54050948178826985, 1436.927678415763012, 136.6348573598288567 ) ) ;
#55834 = CARTESIAN_POINT ( 'NONE',  ( -26.06696396060000254, 1439.602491171669953, 137.5099056270979929 ) ) ;
#55835 = CARTESIAN_POINT ( 'NONE',  ( -1.059358656752720007, 1515.104045403560121, 213.4502668743000129 ) ) ;
#55836 = CARTESIAN_POINT ( 'NONE',  ( 16.73334775859999723, 1413.089575119930259, 226.5682721348979953 ) ) ;
#55837 = CARTESIAN_POINT ( 'NONE',  ( -7.722301029971450070, 1478.317878138009974, 217.8058796438500053 ) ) ;
#55838 = CARTESIAN_POINT ( 'NONE',  ( 5.320869478628496907, 1362.102029591487508, 207.6218459616988241 ) ) ;
#55839 = CARTESIAN_POINT ( 'NONE',  ( 33.45065857238096640, 1524.841055067849084, 198.7780394437808127 ) ) ;
#55841 = ORIENTED_EDGE ( 'NONE', *, *, #41460, .F. ) ;
#55840 = CARTESIAN_POINT ( 'NONE',  ( 6.466160837060870069E-09, 1406.204995675689815, 266.5559840362960244 ) ) ;
#55842 = ORIENTED_EDGE ( 'NONE', *, *, #9048, .F. ) ;
#55843 = CARTESIAN_POINT ( 'NONE',  ( -11.86587318112040101, 1432.320133528169890, 149.9823971726779916 ) ) ;
#55844 = CARTESIAN_POINT ( 'NONE',  ( -22.17228250857910155, 1484.784770550770190, 217.0496227037889980 ) ) ;
#55845 = CARTESIAN_POINT ( 'NONE',  ( -27.66276471549999982, 1464.092292077029924, 269.4444540537980401 ) ) ;
#55846 = CARTESIAN_POINT ( 'NONE',  ( 12.40160258794860049, 1420.584110727309962, 200.5244627772079866 ) ) ;
#55847 = DIRECTION ( 'NONE',  ( 3.828588921590000582E-16, 0.000000000000000000, 1.000000000000000000 ) ) ;
#55848 = CARTESIAN_POINT ( 'NONE',  ( 35.28259859119749819, 1451.607675694110185, 135.1248536069400075 ) ) ;
#55849 = CIRCLE ( 'NONE', #79101, 3.058258088409981923 ) ;
#55850 = EDGE_CURVE ( 'NONE', #61100, #48273, #68206, .T. ) ;
#55851 = CARTESIAN_POINT ( 'NONE',  ( 0.2056231781062039798, 1452.457109619009998, 183.2046317473360091 ) ) ;
#55852 = ADVANCED_FACE ( 'NONE', ( #77139 ), #27513, .T. ) ;
#55853 = CARTESIAN_POINT ( 'NONE',  ( 4.371513128651370650, 1484.373699270089901, 220.1281034412249937 ) ) ;
#55854 = CARTESIAN_POINT ( 'NONE',  ( 2.994691737410922094, 1448.276535295347912, 183.8510770426177885 ) ) ;
#55855 = CARTESIAN_POINT ( 'NONE',  ( -5.518833401969999386, 1458.218094844590041, 217.1129845543590022 ) ) ;
#55856 = CARTESIAN_POINT ( 'NONE',  ( 8.801875223506129942, 1360.481346938555589, 208.3718459617010978 ) ) ;
#55857 = CARTESIAN_POINT ( 'NONE',  ( -37.43441710386299803, 1420.282330175009974, 266.6710652364679959 ) ) ;
#55858 = ORIENTED_EDGE ( 'NONE', *, *, #57013, .T. ) ;
#55859 = CARTESIAN_POINT ( 'NONE',  ( -3.529581353950369760, 1488.333655974519843, 181.7769974444219940 ) ) ;
#55860 = ORIENTED_EDGE ( 'NONE', *, *, #109927, .F. ) ;
#55861 = ORIENTED_EDGE ( 'NONE', *, *, #94562, .T. ) ;
#55862 = CARTESIAN_POINT ( 'NONE',  ( -2.282622950494999969, 1516.861367446839949, 211.4218295478370067 ) ) ;
#55863 = CARTESIAN_POINT ( 'NONE',  ( 38.13540227561171747, 1444.994950788472124, 136.8611909968648490 ) ) ;
#55865 = CARTESIAN_POINT ( 'NONE',  ( -17.62094095786948600, 1419.757685654823035, 206.8396910412140244 ) ) ;
#55864 = CARTESIAN_POINT ( 'NONE',  ( -4.608417544644999531, 1516.691389976299888, 211.6120918846570191 ) ) ;
#55866 = CARTESIAN_POINT ( 'NONE',  ( -16.55052382899999941, 1440.438682495240073, 190.2157002606980143 ) ) ;
#55867 = EDGE_CURVE ( 'NONE', #39608, #35904, #69051, .T. ) ;
#55868 = CARTESIAN_POINT ( 'NONE',  ( -2.430884947309378319, 1449.420338891706024, 183.0400647790289383 ) ) ;
#55869 = ORIENTED_EDGE ( 'NONE', *, *, #101556, .T. ) ;
#55870 = CARTESIAN_POINT ( 'NONE',  ( -26.32958567590000243, 1435.437712720879972, 135.5714638756980150 ) ) ;
#55871 = CARTESIAN_POINT ( 'NONE',  ( -0.01010286742719850028, 1516.939452820819952, 201.4022050290969901 ) ) ;
#55872 = DIRECTION ( 'NONE',  ( 0.8672669759446586246, -1.225281874271768203E-16, -0.4978433412588814111 ) ) ;
#55873 = CARTESIAN_POINT ( 'NONE',  ( -10.32431769148769973, 1384.511448824909849, 200.0654769700809936 ) ) ;
#55874 = CARTESIAN_POINT ( 'NONE',  ( -35.21702932733460045, 1419.789484414370236, 270.0611807039360315 ) ) ;
#55875 = CARTESIAN_POINT ( 'NONE',  ( 4.320487685200830263, 1417.954612720860041, 234.1150779680949938 ) ) ;
#55876 = LINE ( 'NONE', #66908, #26844 ) ;
#55878 = ORIENTED_EDGE ( 'NONE', *, *, #18520, .F. ) ;
#55877 = CARTESIAN_POINT ( 'NONE',  ( -9.934709065799999905, 1365.494406819939968, 207.6218459616989946 ) ) ;
#55879 = VERTEX_POINT ( 'NONE', #88422 ) ;
#55880 = CARTESIAN_POINT ( 'NONE',  ( 42.12435291735053511, 1454.070699221729001, 269.0724519205328988 ) ) ;
#55881 = CARTESIAN_POINT ( 'NONE',  ( 0.2255696094212939762, 1467.412027614160024, 220.2065905680840103 ) ) ;
#55882 = CARTESIAN_POINT ( 'NONE',  ( -13.32470456501929768, 1436.115206346340074, 150.5929143813179962 ) ) ;
#55883 = CARTESIAN_POINT ( 'NONE',  ( -1.590905593539999829, 1484.788648626130225, 182.5874796677979930 ) ) ;
#55884 = EDGE_CURVE ( 'NONE', #24144, #79544, #88054, .T. ) ;
#55885 = CARTESIAN_POINT ( 'NONE',  ( 0.01265818781360149997, 1516.959716008189844, 210.8316124642570060 ) ) ;
#55886 = CARTESIAN_POINT ( 'NONE',  ( -20.58544668775375186, 1506.578946204038630, 217.1750514325470647 ) ) ;
#55887 = CARTESIAN_POINT ( 'NONE',  ( -18.83008980160000334, 1435.775426850719896, 225.4210710169979848 ) ) ;
#55888 = CARTESIAN_POINT ( 'NONE',  ( 15.68102603203800172, 1473.621980054030018, 269.4240265004769981 ) ) ;
#55889 = CARTESIAN_POINT ( 'NONE',  ( 12.71684466930000035, 1416.535385209229844, 223.1239581433979993 ) ) ;
#55890 = CARTESIAN_POINT ( 'NONE',  ( 7.937216453355000034, 1511.802450769970164, 205.9560045756870181 ) ) ;
#55891 = CARTESIAN_POINT ( 'NONE',  ( -2.493073867885000183, 1516.826109302209943, 206.2575198447970024 ) ) ;
#55892 = ADVANCED_FACE ( 'NONE', ( #54837 ), #26155, .F. ) ;
#55893 = EDGE_LOOP ( 'NONE', ( #56698, #60508, #15852, #109078, #85311 ) ) ;
#55894 = CARTESIAN_POINT ( 'NONE',  ( -36.37832870507119765, 1451.642701156129988, 135.0584859581319961 ) ) ;
#55895 = CARTESIAN_POINT ( 'NONE',  ( -3.254300203878770503, 1516.622698719769687, 202.3553198114061047 ) ) ;
#55896 = ORIENTED_EDGE ( 'NONE', *, *, #106249, .T. ) ;
#55897 = CARTESIAN_POINT ( 'NONE',  ( 17.87794079919627066, 1458.605263598233250, 228.2755591390006202 ) ) ;
#55898 = CARTESIAN_POINT ( 'NONE',  ( 24.97086024365579959, 1451.596742172109998, 137.2431907379429958 ) ) ;
#55899 = CARTESIAN_POINT ( 'NONE',  ( -4.096381100208427384, 1440.262533769546963, 185.3780353409536588 ) ) ;
#55900 = CARTESIAN_POINT ( 'NONE',  ( -0.5717982397045180409, 1450.893092752919983, 154.2461502927169761 ) ) ;
#55901 = CARTESIAN_POINT ( 'NONE',  ( 22.12147071639999751, 1410.179604348530120, 204.7719268904379817 ) ) ;
#55902 = CARTESIAN_POINT ( 'NONE',  ( 0.000000000000000000, 1526.382868172863937, 177.3106345060153046 ) ) ;
#55903 = CARTESIAN_POINT ( 'NONE',  ( 11.21247613359999917, 1490.926120241489798, 206.9376360906590264 ) ) ;
#55904 = CARTESIAN_POINT ( 'NONE',  ( 31.33756686635661026, 1523.580204110582372, 221.9021554030050538 ) ) ;
#55905 = CARTESIAN_POINT ( 'NONE',  ( 24.40381529368770330, 1445.062036062823609, 213.9252878650337379 ) ) ;
#55906 = CARTESIAN_POINT ( 'NONE',  ( 2.500000000000000000, 1439.384186984200142, 161.5055418213960081 ) ) ;
#55907 = CARTESIAN_POINT ( 'NONE',  ( -3.257220640824999958, 1517.040132827679827, 214.9086836491569841 ) ) ;
#55908 = ORIENTED_EDGE ( 'NONE', *, *, #69548, .F. ) ;
#55909 = CARTESIAN_POINT ( 'NONE',  ( 7.709748394418160622, 1516.561673159430029, 207.5610261272159960 ) ) ;
#55910 = CARTESIAN_POINT ( 'NONE',  ( -44.93135410500000404, 1442.582777215279975, 269.6838066175980089 ) ) ;
#55911 = LINE ( 'NONE', #90029, #100060 ) ;
#55912 = CARTESIAN_POINT ( 'NONE',  ( 1.887381601534039764E-14, 1421.846727242609859, 101.6566346230980002 ) ) ;
#55913 = CARTESIAN_POINT ( 'NONE',  ( -39.12047235985080107, 1447.561823957390061, 136.5584948024710172 ) ) ;
#55914 = CARTESIAN_POINT ( 'NONE',  ( 10.86957190218895697, 1424.809467336535363, 138.2051722130555333 ) ) ;
#55915 = CARTESIAN_POINT ( 'NONE',  ( 2.501965634382995241, 1417.708848509867494, 233.7485306405076813 ) ) ;
#55916 = CARTESIAN_POINT ( 'NONE',  ( -2.500000000000000000, 1419.365678373030050, 145.1702656710979795 ) ) ;
#55917 = CARTESIAN_POINT ( 'NONE',  ( -0.4564753465201519811, 1455.552155115309915, 198.6001949275529910 ) ) ;
#55918 = CARTESIAN_POINT ( 'NONE',  ( -0.8946033002169070381, 1474.169686496259828, 270.1375980655809599 ) ) ;
#55919 = CARTESIAN_POINT ( 'NONE',  ( 30.68660490123130202, 1440.913060384770006, 240.4674097414240066 ) ) ;
#55920 = CARTESIAN_POINT ( 'NONE',  ( -109.1656546789999993, 1384.956445596120147, 297.1328575266589951 ) ) ;
#55921 = CARTESIAN_POINT ( 'NONE',  ( -4.363122647530000009, 1422.407399603929889, 168.7758374889979791 ) ) ;
#55922 = ORIENTED_EDGE ( 'NONE', *, *, #19245, .T. ) ;
#55923 = ORIENTED_EDGE ( 'NONE', *, *, #20799, .F. ) ;
#55924 = CARTESIAN_POINT ( 'NONE',  ( -3.054816033052110136, 1485.996906143959905, 182.1538611115439892 ) ) ;
#55925 = CARTESIAN_POINT ( 'NONE',  ( -1.356522590142140050, 1410.335674017130032, 185.6037846924129724 ) ) ;
#55926 = CARTESIAN_POINT ( 'NONE',  ( 2.121808125839999892, 1499.002874645929978, 235.8090782458980073 ) ) ;
#55927 = CARTESIAN_POINT ( 'NONE',  ( -15.69795926999090163, 1519.551704408389924, 195.4758181584410011 ) ) ;
#55928 = CARTESIAN_POINT ( 'NONE',  ( -1.506737911117850048, 1508.551704408389924, 220.0821560122830078 ) ) ;
#55929 = CARTESIAN_POINT ( 'NONE',  ( -38.95288734898669958, 1383.829750491509913, 239.9923225223510030 ) ) ;
#55930 =( BOUNDED_SURFACE ( )  B_SPLINE_SURFACE ( 3, 2, ( 
 ( #109355, #41592, #32635 ),
 ( #24210, #75747, #81922 ),
 ( #109891, #67361, #24747 ),
 ( #93076, #16351, #5227 ) ),
 .UNSPECIFIED., .F., .F., .F. ) 
 B_SPLINE_SURFACE_WITH_KNOTS ( ( 4, 4 ),
 ( 3, 3 ),
 ( 0.000000000000000000, 0.0002960034161023851105 ),
 ( 0.000000000000000000, 1.000000000000000000 ),
 .UNSPECIFIED. ) 
 GEOMETRIC_REPRESENTATION_ITEM ( )  RATIONAL_B_SPLINE_SURFACE ( (
 ( 1.000000000000000000, 0.8072480644198088973, 1.000000000000000000),
 ( 1.000000000000000000, 0.8072480346917787486, 1.000000000000000000),
 ( 1.000000000000000000, 0.8071723757218290940, 1.000000000000000000),
 ( 1.000000000000000000, 0.8070209408750043112, 1.000000000000000000) ) ) 
 REPRESENTATION_ITEM ( '' )  SURFACE ( )  );
#55931 = CARTESIAN_POINT ( 'NONE',  ( -4.826478521064999860, 1511.220390575160081, 201.2328893641169714 ) ) ;
#55932 = CARTESIAN_POINT ( 'NONE',  ( 22.83806540279999808, 1452.115537569730122, 139.3226699072980068 ) ) ;
#55933 = CARTESIAN_POINT ( 'NONE',  ( -12.36724210910779931, 1502.518749642870034, 208.9800501045910153 ) ) ;
#55934 = CARTESIAN_POINT ( 'NONE',  ( 1.678290706950000155, 1466.627378388229999, 234.7758880048979790 ) ) ;
#55936 = EDGE_LOOP ( 'NONE', ( #15669, #16950, #4808, #51519, #16947 ) ) ;
#55935 = CARTESIAN_POINT ( 'NONE',  ( 31.79839622030615587, 1525.159196711359755, 216.1507387728551066 ) ) ;
#55937 = CARTESIAN_POINT ( 'NONE',  ( -1.148217067119999824, 1451.929923922529952, 183.5619105232980246 ) ) ;
#55938 = CARTESIAN_POINT ( 'NONE',  ( -25.90756897309999829, 1384.546519395709765, 203.4684288897289832 ) ) ;
#55939 = CARTESIAN_POINT ( 'NONE',  ( 4.141018395973380173, 1508.551704408389924, 204.7583302192930148 ) ) ;
#55941 = ORIENTED_EDGE ( 'NONE', *, *, #81590, .F. ) ;
#55940 = CARTESIAN_POINT ( 'NONE',  ( -31.79806488007560361, 1525.506916460679349, 217.0230655909559800 ) ) ;
#55942 = CARTESIAN_POINT ( 'NONE',  ( 0.9103554862159439764, 1462.760092965149852, 230.5111408766040029 ) ) ;
#55943 = ORIENTED_EDGE ( 'NONE', *, *, #26492, .T. ) ;
#55944 = CARTESIAN_POINT ( 'NONE',  ( -9.285067551966019295, 1387.122678197030154, 218.0550403871500009 ) ) ;
#55945 = CARTESIAN_POINT ( 'NONE',  ( 34.75665256036710105, 1437.096089887269954, 136.5416360476299928 ) ) ;
#55946 = CARTESIAN_POINT ( 'NONE',  ( 3.487592428935230249, 1508.551704408389924, 214.1089243929580164 ) ) ;
#55947 = CARTESIAN_POINT ( 'NONE',  ( -2.372478608332516892, 1512.187213306747481, 174.8996806668726549 ) ) ;
#55948 = CARTESIAN_POINT ( 'NONE',  ( -2.321631234430000301, 1421.242214399630257, 184.0178362275980248 ) ) ;
#55949 = CARTESIAN_POINT ( 'NONE',  ( 7.739917900360000047, 1490.431902873490117, 209.0953228043489958 ) ) ;
#55950 = CARTESIAN_POINT ( 'NONE',  ( 6.155896025694070239, 1409.128029013429796, 195.4707178546539978 ) ) ;
#55951 = CARTESIAN_POINT ( 'NONE',  ( 18.80338089039999971, 1425.953332570529938, 225.0197130250980138 ) ) ;
#55952 = CARTESIAN_POINT ( 'NONE',  ( 18.62883413325391047, 1458.551313265810677, 214.8531784976841550 ) ) ;
#55953 = CARTESIAN_POINT ( 'NONE',  ( -17.63150429730000113, 1440.791932874859867, 190.8949773138979822 ) ) ;
#55954 = CARTESIAN_POINT ( 'NONE',  ( 11.86529747189999817, 1432.285508799240006, 150.3971901177980044 ) ) ;
#55955 = DIRECTION ( 'NONE',  ( 0.9786619618251657382, 0.000000000000000000, 0.2054769195713180285 ) ) ;
#55956 = EDGE_LOOP ( 'NONE', ( #46114, #16529, #101272, #70109 ) ) ;
#55957 = ORIENTED_EDGE ( 'NONE', *, *, #48546, .T. ) ;
#55958 = CARTESIAN_POINT ( 'NONE',  ( 18.72690275719072517, 1526.278758871496393, 236.1309272327557949 ) ) ;
#55959 = CARTESIAN_POINT ( 'NONE',  ( -12.26355851482949966, 1416.702560754919887, 194.6703901714200242 ) ) ;
#55960 =( BOUNDED_CURVE ( )  B_SPLINE_CURVE ( 3, ( #81746, #30246, #55483, #89608 ),
 .UNSPECIFIED., .F., .T. ) 
 B_SPLINE_CURVE_WITH_KNOTS ( ( 4, 4 ),
 ( 0.9859787944923890102, 2.095227079056804609 ),
 .UNSPECIFIED. ) 
 CURVE ( )  GEOMETRIC_REPRESENTATION_ITEM ( )  RATIONAL_B_SPLINE_CURVE ( ( 1.000000000000000000, 0.9000656239593909369, 0.9000656239593909369, 1.000000000000000000 ) ) 
 REPRESENTATION_ITEM ( '' )  );
#55961 = CARTESIAN_POINT ( 'NONE',  ( -11.92218722690000021, 1434.273876409569993, 150.9668191998980262 ) ) ;
#55962 = CARTESIAN_POINT ( 'NONE',  ( 12.62249134276009954, 1420.706334970369880, 201.4123180351149927 ) ) ;
#55963 = CARTESIAN_POINT ( 'NONE',  ( 11.86610049460949945, 1432.336025080309810, 149.9824239092829998 ) ) ;
#55964 = CARTESIAN_POINT ( 'NONE',  ( -14.61959290290000091, 1420.357143390019928, 213.8552925859189884 ) ) ;
#55965 = CARTESIAN_POINT ( 'NONE',  ( -109.5110906019999959, 1386.650732619270002, 311.1668118922589770 ) ) ;
#55966 = CARTESIAN_POINT ( 'NONE',  ( -8.474723756492620552, 1511.779111711370206, 215.2118351801979941 ) ) ;
#55967 = CARTESIAN_POINT ( 'NONE',  ( -11.09489115964376360, 1365.835216822674965, 210.6218459617030021 ) ) ;
#55968 = CARTESIAN_POINT ( 'NONE',  ( -46.16774349130800204, 1440.697242589380039, 266.9714508753160089 ) ) ;
#55969 = CARTESIAN_POINT ( 'NONE',  ( -20.59710966430000312, 1507.771223779230013, 191.2037110683980075 ) ) ;
#55970 = CARTESIAN_POINT ( 'NONE',  ( 4.608021669135000664, 1516.660388280709867, 207.4085285224269910 ) ) ;
#55971 = CARTESIAN_POINT ( 'NONE',  ( -8.796828982357618898, 1448.417242874349995, 211.5920706533679834 ) ) ;
#55972 = CARTESIAN_POINT ( 'NONE',  ( 5.135462867024300770, 1408.035052394380045, 221.3338201871839885 ) ) ;
#55973 = CARTESIAN_POINT ( 'NONE',  ( -13.03770669738669952, 1434.798218780290199, 149.1309000377920029 ) ) ;
#55974 = CARTESIAN_POINT ( 'NONE',  ( -7.556639502920000417, 1385.398637304449949, 219.0631512379790138 ) ) ;
#55975 = CARTESIAN_POINT ( 'NONE',  ( 9.236167301360001858, 1423.625854809029988, 144.1549878472980026 ) ) ;
#55976 = CARTESIAN_POINT ( 'NONE',  ( 7.450732447323310303, 1425.217176014760071, 212.3482398299129841 ) ) ;
#55977 = CARTESIAN_POINT ( 'NONE',  ( 5426.659240076989590, 2833.746317950241519, 8449.939303198118068 ) ) ;
#55978 = ORIENTED_EDGE ( 'NONE', *, *, #17846, .T. ) ;
#55979 = EDGE_CURVE ( 'NONE', #103332, #62022, #102317, .T. ) ;
#55980 = CARTESIAN_POINT ( 'NONE',  ( 36.52133868079999957, 1436.268774900949893, 254.5789811318979616 ) ) ;
#55981 = CARTESIAN_POINT ( 'NONE',  ( -15.22583482770000174, 1419.426620482320004, 199.2582349955389986 ) ) ;
#55983 = CARTESIAN_POINT ( 'NONE',  ( -17.22039985489999836, 1409.679124340329963, 195.0448976402979895 ) ) ;
#55982 = CARTESIAN_POINT ( 'NONE',  ( -3.480938413559999667, 1458.418752667929994, 183.0457556368980079 ) ) ;
#55984 = CARTESIAN_POINT ( 'NONE',  ( 21.97938480441199971, 1506.433683733499947, 208.7396655020440051 ) ) ;
#55985 = CARTESIAN_POINT ( 'NONE',  ( -7.523989352620000126, 1422.078425209429952, 216.2367226431979930 ) ) ;
#55986 = CARTESIAN_POINT ( 'NONE',  ( -4.639453685896637758, 1378.135666831742583, 214.4485485313242066 ) ) ;
#55987 = ADVANCED_FACE ( 'NONE', ( #72199 ), #78367, .F. ) ;
#55988 = CARTESIAN_POINT ( 'NONE',  ( -4.468407265335279988, 1452.757020167219935, 152.1700944353500233 ) ) ;
#55989 = CARTESIAN_POINT ( 'NONE',  ( -18.89924256150000303, 1416.831925117730179, 207.5749492501780082 ) ) ;
#55990 = VERTEX_POINT ( 'NONE', #62714 ) ;
#55991 = CARTESIAN_POINT ( 'NONE',  ( -0.02816757767735129925, 1396.454736580349845, 196.6640986795260062 ) ) ;
#55992 = CARTESIAN_POINT ( 'NONE',  ( 13.24891926068781878, 1513.564960623643401, 225.9057560452617963 ) ) ;
#55993 = CARTESIAN_POINT ( 'NONE',  ( 2.970284549810000119, 1509.150405704829836, 239.1320982052979787 ) ) ;
#55994 = EDGE_LOOP ( 'NONE', ( #29442, #78298 ) ) ;
#55995 = ORIENTED_EDGE ( 'NONE', *, *, #6290, .F. ) ;
#55996 = CARTESIAN_POINT ( 'NONE',  ( -10.62939606198754738, 1424.058470519482398, 137.5671174789835618 ) ) ;
#55997 = CARTESIAN_POINT ( 'NONE',  ( 6.339003235429999883, 1424.106680004219925, 194.5877290424989781 ) ) ;
#55998 = VERTEX_POINT ( 'NONE', #95168 ) ;
#55999 = CARTESIAN_POINT ( 'NONE',  ( 3.487586041942699833, 1508.611352721110052, 204.4436967962270160 ) ) ;
#56000 = CARTESIAN_POINT ( 'NONE',  ( -107.2899050854710055, 1379.886892357829993, 309.1794776302379546 ) ) ;
#56001 = CARTESIAN_POINT ( 'NONE',  ( -16.14907631359999840, 1479.767009654729918, 229.2046367109979883 ) ) ;
#56002 = CARTESIAN_POINT ( 'NONE',  ( -0.7790226144181949808, 1442.687261678630193, 200.2740145696140246 ) ) ;
#56003 = ORIENTED_EDGE ( 'NONE', *, *, #98574, .F. ) ;
#56004 = CARTESIAN_POINT ( 'NONE',  ( 11.43737779389999965, 1425.481201409729920, 144.1652972826979635 ) ) ;
#56005 = CARTESIAN_POINT ( 'NONE',  ( -13.00574619272840060, 1416.230844595159851, 221.8287990380179906 ) ) ;
#56006 = CARTESIAN_POINT ( 'NONE',  ( 19.63722818192610120, 1522.051704408389924, 218.2362632616380154 ) ) ;
#56007 = CARTESIAN_POINT ( 'NONE',  ( 1.705466410464999916, 1517.120861839400050, 204.1076508302870138 ) ) ;
#56008 = ORIENTED_EDGE ( 'NONE', *, *, #36332, .T. ) ;
#56009 = CARTESIAN_POINT ( 'NONE',  ( 10.00658443562149991, 1481.688797028250065, 215.3953389918819710 ) ) ;
#56010 = CARTESIAN_POINT ( 'NONE',  ( 13.31869894295501311, 1443.265307952794501, 187.7487017255434125 ) ) ;
#56011 = ORIENTED_EDGE ( 'NONE', *, *, #104717, .F. ) ;
#56012 = ORIENTED_EDGE ( 'NONE', *, *, #26837, .T. ) ;
#56013 = CARTESIAN_POINT ( 'NONE',  ( 2.397475438394585989, 1525.713797967456685, 175.0187375749330272 ) ) ;
#56014 = CARTESIAN_POINT ( 'NONE',  ( -3.238204166650680005, 1508.087190631079920, 220.8316669474850187 ) ) ;
#56015 = CARTESIAN_POINT ( 'NONE',  ( 4.836615265953239096, 1498.177351943570102, 198.3432821877800052 ) ) ;
#56016 = CARTESIAN_POINT ( 'NONE',  ( -4.653281936863520762, 1425.827070423550140, 186.2156739099499987 ) ) ;
#56017 = CARTESIAN_POINT ( 'NONE',  ( 23.64676265546030010, 1452.087297239420195, 137.4473122821260063 ) ) ;
#56018 = CARTESIAN_POINT ( 'NONE',  ( 0.4742219137227159931, 1409.781081933909945, 270.0713786262579674 ) ) ;
#56019 = LINE ( 'NONE', #89055, #97799 ) ;
#56020 = CARTESIAN_POINT ( 'NONE',  ( -109.0982299788821024, 1382.066543485014108, 297.5654259004551818 ) ) ;
#56021 = CARTESIAN_POINT ( 'NONE',  ( -19.50212806963730472, 1509.609157136526619, 231.3489388162998637 ) ) ;
#56022 = CARTESIAN_POINT ( 'NONE',  ( 0.02070843297204195618, 1409.009641154224255, 232.2968665989713202 ) ) ;
#56024 = CARTESIAN_POINT ( 'NONE',  ( -107.2902884299589914, 1391.913060387289988, 307.3027227297359900 ) ) ;
#56023 = CARTESIAN_POINT ( 'NONE',  ( -13.26406613303420023, 1434.886401268850022, 148.9734610765700040 ) ) ;
#56025 = CARTESIAN_POINT ( 'NONE',  ( 10.72591451257290096, 1424.883072988620142, 206.5517914635169916 ) ) ;
#56026 = CARTESIAN_POINT ( 'NONE',  ( -24.89153249345189778, 1509.523145840989855, 222.7250669980219868 ) ) ;
#56027 = CARTESIAN_POINT ( 'NONE',  ( -7.891962451154999059, 1514.771170611759999, 203.1042818683069981 ) ) ;
#56028 = VERTEX_POINT ( 'NONE', #18424 ) ;
#56029 = CARTESIAN_POINT ( 'NONE',  ( 18.57221589319999921, 1434.150321779219894, 219.6133833291980011 ) ) ;
#56030 = CARTESIAN_POINT ( 'NONE',  ( -10.81518761075750135, 1424.921099531289883, 144.1705495212430037 ) ) ;
#56031 = CARTESIAN_POINT ( 'NONE',  ( -81.22482676457471484, 1384.990768542609885, 304.6421476864239253 ) ) ;
#56032 = CARTESIAN_POINT ( 'NONE',  ( -9.721596386979999949, 1387.218309458520253, 200.7551491867290281 ) ) ;
#56033 = CARTESIAN_POINT ( 'NONE',  ( -15.70029802240000016, 1416.147372738109880, 210.3646106849990076 ) ) ;
#56035 = VERTEX_POINT ( 'NONE', #12252 ) ;
#56034 = CARTESIAN_POINT ( 'NONE',  ( 3.629220049600000220, 1485.493215689190038, 199.0019176958990101 ) ) ;
#56036 = CARTESIAN_POINT ( 'NONE',  ( 2.696703656820000017, 1429.897299915890017, 217.1506436859089888 ) ) ;
#56037 = CARTESIAN_POINT ( 'NONE',  ( 1.300519565079999921E-15, 1440.444625599219989, 150.6821045058979962 ) ) ;
#56038 = CARTESIAN_POINT ( 'NONE',  ( -8.749343725295464225, 1477.568838901969912, 214.8427604742473704 ) ) ;
#56039 = CARTESIAN_POINT ( 'NONE',  ( 1.376928043298436322, 1517.151704408390060, 191.7575736759021936 ) ) ;
#56040 = CARTESIAN_POINT ( 'NONE',  ( 14.32514190893500050, 1513.248517198770060, 225.3451382666669929 ) ) ;
#56041 = CARTESIAN_POINT ( 'NONE',  ( -17.15254157612219643, 1516.551704399882283, 221.3246399025400706 ) ) ;
#56042 = CARTESIAN_POINT ( 'NONE',  ( 1.408266058077070060, 1457.262924391489832, 199.5821088331159956 ) ) ;
#56043 = CARTESIAN_POINT ( 'NONE',  ( 0.000000000000000000, 1512.187213306747481, 243.9330574173806951 ) ) ;
#56044 = CARTESIAN_POINT ( 'NONE',  ( 14.23529166910000043, 1422.104100209229955, 228.4651581752980007 ) ) ;
#56045 = CARTESIAN_POINT ( 'NONE',  ( -32.80316127680809757, 1523.919934424249959, 201.0769002502127023 ) ) ;
#56046 = CARTESIAN_POINT ( 'NONE',  ( 7.321169230994999388, 1516.531533746980131, 207.4131249475269954 ) ) ;
#56047 = DIRECTION ( 'NONE',  ( 1.755985294532469921E-16, -1.000000000000000000, 1.338183447452831989E-16 ) ) ;
#56048 = CARTESIAN_POINT ( 'NONE',  ( -17.84388054299999737, 1409.536182426630148, 223.0592386858980092 ) ) ;
#56049 = CARTESIAN_POINT ( 'NONE',  ( 1.549965084495990020, 1416.007771869960152, 190.4473925629179973 ) ) ;
#56050 = CARTESIAN_POINT ( 'NONE',  ( 4.468129420396740770, 1440.960114341679855, 155.7399635850599680 ) ) ;
#56051 = CARTESIAN_POINT ( 'NONE',  ( 29.35128621234889934, 1441.653456125289949, 137.2693277896180177 ) ) ;
#56052 = CARTESIAN_POINT ( 'NONE',  ( 5.376511155560629973, 1429.663370564680235, 154.2340444031499942 ) ) ;
#56053 = CARTESIAN_POINT ( 'NONE',  ( 12.26979143420000007, 1416.828042686930075, 223.5793547218980279 ) ) ;
#56054 = CARTESIAN_POINT ( 'NONE',  ( -14.75552471225380025, 1417.657372812460153, 203.2383312169210114 ) ) ;
#56055 = CARTESIAN_POINT ( 'NONE',  ( -41.01355532634549661, 1442.086579808119950, 136.7422881729029882 ) ) ;
#56056 = CARTESIAN_POINT ( 'NONE',  ( -1.241866690459999978, 1415.088275290230058, 226.9681039297979908 ) ) ;
#56057 = DIRECTION ( 'NONE',  ( -4.648609652910299899E-17, -1.000000000000000000, 2.252106476759999926E-16 ) ) ;
#56058 = CARTESIAN_POINT ( 'NONE',  ( -8.168076443215248617, 1407.240959200780026, 219.8347814960359869 ) ) ;
#56059 = CARTESIAN_POINT ( 'NONE',  ( 2.248963467334999855, 1512.851027015570025, 217.7347704682469782 ) ) ;
#56060 = CARTESIAN_POINT ( 'NONE',  ( 18.10570579382015310, 1525.713797967457140, 180.1226510103675196 ) ) ;
#56061 = CARTESIAN_POINT ( 'NONE',  ( -29.22959469711409852, 1509.933780326070064, 211.7723416727030212 ) ) ;
#56062 = CARTESIAN_POINT ( 'NONE',  ( 13.80530362780000075, 1434.979595110789887, 149.0261668940979973 ) ) ;
#56063 = CARTESIAN_POINT ( 'NONE',  ( -27.25232428270000185, 1436.344188865190063, 136.7193557181979884 ) ) ;
#56064 = CARTESIAN_POINT ( 'NONE',  ( 7.185297835940000155, 1440.193071586459837, 185.7613749676980035 ) ) ;
#56065 = ORIENTED_EDGE ( 'NONE', *, *, #37244, .T. ) ;
#56066 = CARTESIAN_POINT ( 'NONE',  ( 3.004219500040000046, 1486.176588069189847, 198.6256029144990123 ) ) ;
#56067 = CARTESIAN_POINT ( 'NONE',  ( 7.415490016120000583, 1477.911609511289953, 201.0119040078689920 ) ) ;
#56068 = CARTESIAN_POINT ( 'NONE',  ( -0.6034434167798160553, 1408.934133095820016, 224.1097741871060123 ) ) ;
#56069 = CARTESIAN_POINT ( 'NONE',  ( -11.80902463480000009, 1490.509434397089990, 209.3574457513870186 ) ) ;
#56070 = CARTESIAN_POINT ( 'NONE',  ( -2.234923479105000332, 1512.341036988540054, 201.5226187854269995 ) ) ;
#56071 = CARTESIAN_POINT ( 'NONE',  ( -13.14670073217260082, 1428.477643202489844, 195.1720996079020267 ) ) ;
#56072 = CARTESIAN_POINT ( 'NONE',  ( 31.99315161004722441, 1416.540825925197851, 269.3158597989070131 ) ) ;
#56073 = FACE_OUTER_BOUND ( 'NONE', #3352, .T. ) ;
#56074 = CARTESIAN_POINT ( 'NONE',  ( -13.64835502960000113, 1380.295393291809887, 210.2814589097189923 ) ) ;
#56075 = CARTESIAN_POINT ( 'NONE',  ( -95.83152833198130338, 1384.608534833750127, 310.2052327687620163 ) ) ;
#56076 = B_SPLINE_SURFACE_WITH_KNOTS ( 'NONE', 5, 5, ( 
 ( #94781, #18601, #19150, #102064, #25901, #85262 ),
 ( #52253, #1289, #59539, #104292, #60099, #35429 ),
 ( #53357, #26462, #69616, #43292, #94215, #77440 ),
 ( #86379, #44962, #60657, #17490, #79110, #18059 ),
 ( #741, #9665, #86932, #8559, #34872, #2417 ),
 ( #103737, #67954, #42731, #27038, #61226, #76890 ),
 ( #52801, #51688, #27579, #85828, #10223, #44401 ),
 ( #78543, #35992, #16934, #61764, #51136, #96447 ),
 ( #63967, #98082, #29238, #62896, #97545, #46062 ),
 ( #54470, #81275, #107040, #19726, #38725, #80747 ),
 ( #53927, #98631, #37082, #97006, #38182, #105399 ),
 ( #4056, #89685, #72362, #80195, #29779, #79661 ),
 ( #20269, #28692, #88062, #88608, #106494, #47697 ),
 ( #11347, #63427, #21353, #55560, #12967, #47150 ),
 ( #45519, #2965, #28131, #89141, #11890, #71286 ) ),
 .UNSPECIFIED., .F., .F., .F.,
 ( 6, 3, 3, 3, 6 ),
 ( 6, 6 ),
 ( 7.411273261979999916, 10.46453992930000076, 15.62038767109999959, 19.62991602479999997, 26.81730491820000140 ),
 ( 0.000000000000000000, 2.000000000000000000 ),
 .UNSPECIFIED. ) ;
#56077 = CARTESIAN_POINT ( 'NONE',  ( -50.37285252689139980, 1385.020400592789883, 225.8367497718959953 ) ) ;
#56078 = CARTESIAN_POINT ( 'NONE',  ( -12.11449315257920212, 1490.976347222529967, 207.1920171886079913 ) ) ;
#56079 = DIRECTION ( 'NONE',  ( -0.9455185755993177343, 0.000000000000000000, 0.3255681544571540909 ) ) ;
#56080 = CARTESIAN_POINT ( 'NONE',  ( -27.28811781800000347, 1451.810925661529836, 135.7818030516980059 ) ) ;
#56081 = B_SPLINE_CURVE_WITH_KNOTS ( 'NONE', 3,
 ( #33762, #75248, #25352, #84170 ),
 .UNSPECIFIED., .F., .F.,
 ( 4, 4 ),
 ( 0.000000000000000000, 1.000000000000000000 ),
 .UNSPECIFIED. ) ;
#56082 = CARTESIAN_POINT ( 'NONE',  ( 2.596261494520243573, 1525.907212628473644, 177.4701144822248011 ) ) ;
#56083 = CARTESIAN_POINT ( 'NONE',  ( -16.76087985708559813, 1410.448050361750120, 226.3463234497499741 ) ) ;
#56085 = ORIENTED_EDGE ( 'NONE', *, *, #8408, .T. ) ;
#56084 = CARTESIAN_POINT ( 'NONE',  ( 0.5042866867199140568, 1413.080632846199933, 184.9534695539459790 ) ) ;
#56086 = CARTESIAN_POINT ( 'NONE',  ( -109.8257969779999854, 1384.899434086499923, 311.3808307492589620 ) ) ;
#56087 = CARTESIAN_POINT ( 'NONE',  ( 9.927196207040308806, 1470.874197623729970, 211.7260430095500112 ) ) ;
#56088 = CARTESIAN_POINT ( 'NONE',  ( 24.84138244430000242, 1449.855123928979992, 207.3631881002280295 ) ) ;
#56089 = FILL_AREA_STYLE_COLOUR ( '', #51719 ) ;
#56090 = CARTESIAN_POINT ( 'NONE',  ( -0.3072900061734130106, 1418.957554290649796, 184.6599555451460049 ) ) ;
#56091 = LINE ( 'NONE', #105954, #19291 ) ;
#56092 = CARTESIAN_POINT ( 'NONE',  ( 22.43553758490000050, 1409.860968200830030, 213.4417271402680285 ) ) ;
#56093 = DIRECTION ( 'NONE',  ( 1.224646799147353207E-16, -1.836970198721029688E-16, -1.000000000000000000 ) ) ;
#56094 = CARTESIAN_POINT ( 'NONE',  ( -18.73311320389999679, 1469.013380241389996, 201.1621679275489782 ) ) ;
#56095 = CARTESIAN_POINT ( 'NONE',  ( -17.58819996659999774, 1424.269664099130068, 227.8357312002980279 ) ) ;
#56096 = CARTESIAN_POINT ( 'NONE',  ( -11.30116487869999986, 1432.303974762190137, 151.5220930523979916 ) ) ;
#56097 = CARTESIAN_POINT ( 'NONE',  ( 27.47789372709499744, 1488.737009538180018, 209.0498192191509759 ) ) ;
#56098 = CARTESIAN_POINT ( 'NONE',  ( -104.0812585028399582, 1311.832804576490389, 294.9031044600990867 ) ) ;
#56099 = CARTESIAN_POINT ( 'NONE',  ( 25.48623307864125920, 1509.803059086864550, 194.5187256612674673 ) ) ;
#56100 = CARTESIAN_POINT ( 'NONE',  ( 14.13195592840999915, 1452.421092199690065, 222.7290593210850034 ) ) ;
#56101 = CARTESIAN_POINT ( 'NONE',  ( 3.756023522780000068, 1369.098589419769951, 210.6218459616991936 ) ) ;
#56102 = CARTESIAN_POINT ( 'NONE',  ( -0.01322039564809850132, 1516.939819969850078, 205.0847949345169923 ) ) ;
#56103 = CARTESIAN_POINT ( 'NONE',  ( -17.97825106899999881, 1424.673537191730020, 227.3634650722979984 ) ) ;
#56104 = CARTESIAN_POINT ( 'NONE',  ( 11.46293682908580003, 1502.175680543279896, 213.7711866132059981 ) ) ;
#56105 = CARTESIAN_POINT ( 'NONE',  ( -4.260246875749409412, 1441.234673244090118, 159.4002643389130185 ) ) ;
#56107 = ORIENTED_EDGE ( 'NONE', *, *, #68632, .F. ) ;
#56106 = CARTESIAN_POINT ( 'NONE',  ( -67.33396345445230224, 1379.744479302740046, 278.5401087013319739 ) ) ;
#56108 = EDGE_LOOP ( 'NONE', ( #781, #54303, #33672, #24400 ) ) ;
#56109 = CARTESIAN_POINT ( 'NONE',  ( 4.086314401636647275, 1515.499673572144275, 207.2788822313456762 ) ) ;
#56110 = VERTEX_POINT ( 'NONE', #36356 ) ;
#56111 = CARTESIAN_POINT ( 'NONE',  ( -2.184771148224290194, 1486.435642548830174, 220.8481228361289936 ) ) ;
#56112 = CARTESIAN_POINT ( 'NONE',  ( 12.41076581919999988, 1499.916734172390079, 206.5417464095490061 ) ) ;
#56114 = CARTESIAN_POINT ( 'NONE',  ( 15.70031134094579706, 1410.429114820810128, 191.5836651352509818 ) ) ;
#56113 = CARTESIAN_POINT ( 'NONE',  ( -11.44042036928753170, 1425.479427483456220, 144.3717380689928689 ) ) ;
#56115 = CARTESIAN_POINT ( 'NONE',  ( -7.323390445344999833, 1516.613712827999962, 210.2512321725070024 ) ) ;
#56116 = CARTESIAN_POINT ( 'NONE',  ( -25.25892285357279832, 1450.980737957350129, 137.4961021865089776 ) ) ;
#56117 = CARTESIAN_POINT ( 'NONE',  ( -107.1397530847460047, 1378.913060387289988, 307.3765361525499316 ) ) ;
#56118 = CARTESIAN_POINT ( 'NONE',  ( 11.20515980299999903, 1409.304353190929987, 228.2703101120980023 ) ) ;
#56119 = CARTESIAN_POINT ( 'NONE',  ( 10.42050379654340020, 1481.382441556200092, 211.7093090774899906 ) ) ;
#56120 = CARTESIAN_POINT ( 'NONE',  ( 41.62352936865920583, 1444.515901152170045, 134.0999999983539794 ) ) ;
#56121 = LINE ( 'NONE', #57249, #59726 ) ;
#56122 = CARTESIAN_POINT ( 'NONE',  ( 2.487935123020000194, 1508.551704408389924, 204.1347675455010062 ) ) ;
#56123 = CARTESIAN_POINT ( 'NONE',  ( -8.301987938657498844, 1512.913060387330006, 186.6498241004079262 ) ) ;
#56124 = ORIENTED_EDGE ( 'NONE', *, *, #41183, .T. ) ;
#56125 = ORIENTED_EDGE ( 'NONE', *, *, #20912, .F. ) ;
#56126 = AXIS2_PLACEMENT_3D ( 'NONE', #64547, #90813, #14656 ) ;
#56127 = CARTESIAN_POINT ( 'NONE',  ( 13.23760251530267595, 1410.748325464791151, 228.4239685329596057 ) ) ;
#56128 = CARTESIAN_POINT ( 'NONE',  ( 34.35673732775180156, 1445.503283704120122, 137.0830489816779902 ) ) ;
#56129 = CARTESIAN_POINT ( 'NONE',  ( 12.21820660407649939, 1499.761928509490190, 205.8071831984830169 ) ) ;
#56130 = CARTESIAN_POINT ( 'NONE',  ( -3.066838699319999861, 1484.261994786129890, 183.3371859551980094 ) ) ;
#56131 = CONICAL_SURFACE ( 'NONE', #7831, 23.60271693650006952, 1.047191723200000313 ) ;
#56132 = CARTESIAN_POINT ( 'NONE',  ( -28.19408351100000232, 1508.123162623830012, 208.4952225986349958 ) ) ;
#56133 = CARTESIAN_POINT ( 'NONE',  ( -62.99661746870935275, 1379.733886384323114, 268.0375848082739481 ) ) ;
#56134 = CARTESIAN_POINT ( 'NONE',  ( -21.53565904410000087, 1506.077647802389947, 209.2113159668039941 ) ) ;
#56135 = CARTESIAN_POINT ( 'NONE',  ( 15.72751745975079984, 1517.151704408390060, 206.8816388537309763 ) ) ;
#56136 = CARTESIAN_POINT ( 'NONE',  ( 3.949232805999999929, 1416.520322350429979, 190.9327904293980112 ) ) ;
#56137 = CARTESIAN_POINT ( 'NONE',  ( -86.19296323747759914, 1384.823008793549889, 289.8026865565949493 ) ) ;
#56138 = ORIENTED_EDGE ( 'NONE', *, *, #104725, .F. ) ;
#56139 = CARTESIAN_POINT ( 'NONE',  ( 9.526054245020199929, 1462.325501871250026, 207.0857702337349906 ) ) ;
#56140 = CARTESIAN_POINT ( 'NONE',  ( -4.625790014595000166, 1517.104192383289956, 208.0004623403669939 ) ) ;
#56141 = EDGE_LOOP ( 'NONE', ( #36971, #68718, #27, #43871 ) ) ;
#56142 = CARTESIAN_POINT ( 'NONE',  ( 35.39978664942150033, 1440.913060387330006, 261.4306008630139786 ) ) ;
#56143 = CARTESIAN_POINT ( 'NONE',  ( -0.0007575016918736815529, 1451.923243585050386, 153.9989249036371177 ) ) ;
#56144 = EDGE_LOOP ( 'NONE', ( #58235, #72573, #73244, #40184 ) ) ;
#56145 = CARTESIAN_POINT ( 'NONE',  ( -0.3637087824265209934, 1450.900359396770000, 181.9077912123260035 ) ) ;
#56146 = CARTESIAN_POINT ( 'NONE',  ( -15.57473716419999832, 1409.623569226230074, 191.7218289598980050 ) ) ;
#56147 = CARTESIAN_POINT ( 'NONE',  ( -17.96416104880992748, 1508.456897258907929, 211.9435951326316001 ) ) ;
#56148 = LINE ( 'NONE', #74065, #25721 ) ;
#56149 = CARTESIAN_POINT ( 'NONE',  ( -4.609549296629079862, 1434.018457786650060, 217.5596424976919820 ) ) ;
#56150 = VECTOR ( 'NONE', #39604, 1000.000000000000000 ) ;
#56151 = CARTESIAN_POINT ( 'NONE',  ( 0.8775825618903718706, 1380.371560387289946, 208.6424204230947907 ) ) ;
#56152 = CARTESIAN_POINT ( 'NONE',  ( 6.178286635010000083, 1406.300107697530166, 266.9460459613980561 ) ) ;
#56153 = CARTESIAN_POINT ( 'NONE',  ( -13.19913408319999881, 1434.900406177449895, 146.4345302607979988 ) ) ;
#56155 = ADVANCED_FACE ( 'NONE', ( #96833 ), #84430, .T. ) ;
#56154 = FACE_OUTER_BOUND ( 'NONE', #44704, .T. ) ;
#56157 = CARTESIAN_POINT ( 'NONE',  ( -11.60004869885203682, 1422.941213647143968, 135.6422426697142782 ) ) ;
#56156 = CARTESIAN_POINT ( 'NONE',  ( 17.04804198250000269, 1458.590950340129893, 229.8098020277979856 ) ) ;
#56158 = CARTESIAN_POINT ( 'NONE',  ( 2.873958851594999864, 1516.588006113850042, 216.0563744999969913 ) ) ;
#56159 = LINE ( 'NONE', #47761, #53426 ) ;
#56160 = CARTESIAN_POINT ( 'NONE',  ( -0.1562604339309009993, 1507.298388591709909, 180.8861905666690006 ) ) ;
#56161 = CARTESIAN_POINT ( 'NONE',  ( 16.95285180472732378, 1449.028869222066305, 218.6259880166646496 ) ) ;
#56162 = CARTESIAN_POINT ( 'NONE',  ( 0.7568986996720019622, 1516.805675336850072, 213.1530147380969993 ) ) ;
#56163 = CARTESIAN_POINT ( 'NONE',  ( 18.62830136119999835, 1508.852446408229753, 188.2546778553979721 ) ) ;
#56164 = CARTESIAN_POINT ( 'NONE',  ( -1.191524307911311809, 1526.382868172863937, 179.0083900503167911 ) ) ;
#56166 = EDGE_LOOP ( 'NONE', ( #73916, #35845, #91528 ) ) ;
#56165 = CARTESIAN_POINT ( 'NONE',  ( -13.33252017900000119, 1422.271663147810159, 196.2999248757990074 ) ) ;
#56167 = CARTESIAN_POINT ( 'NONE',  ( -8.847782810029999112, 1384.881200155019997, 199.9249090898990175 ) ) ;
#56168 = CARTESIAN_POINT ( 'NONE',  ( 16.14278285189999806, 1456.434606976529949, 217.4272506521679702 ) ) ;
#56169 = CARTESIAN_POINT ( 'NONE',  ( -11.57591907649999996, 1432.294438222789950, 151.1967649998980221 ) ) ;
#56170 = CARTESIAN_POINT ( 'NONE',  ( -15.51493367179999971, 1415.867981975840166, 207.8251654569390325 ) ) ;
#56171 = CARTESIAN_POINT ( 'NONE',  ( -8.228434171293290689, 1441.487951933999966, 203.2737819892520008 ) ) ;
#56172 = CARTESIAN_POINT ( 'NONE',  ( 2.425235212390000061, 1410.367075232029947, 231.7449734550979770 ) ) ;
#56173 = CARTESIAN_POINT ( 'NONE',  ( 16.56816485275348683, 1526.186458717539153, 182.6341057012125191 ) ) ;
#56174 = CARTESIAN_POINT ( 'NONE',  ( 12.08639211120000034, 1446.204391809530080, 187.8374895246980145 ) ) ;
#56176 = CARTESIAN_POINT ( 'NONE',  ( 19.46473663940000165, 1455.600668601630105, 226.0207017425979927 ) ) ;
#56175 = CARTESIAN_POINT ( 'NONE',  ( -20.58378676590000111, 1457.443618353330066, 224.2614987732980012 ) ) ;
#56177 = CARTESIAN_POINT ( 'NONE',  ( -2.153510090440000191, 1485.578724168830149, 182.5440842283980203 ) ) ;
#56178 = B_SPLINE_CURVE_WITH_KNOTS ( 'NONE', 3,
 ( #76546, #8779, #92796, #68185, #59767, #100632, #23918, #93888, #23379, #58113, #109607, #50270, #92246 ),
 .UNSPECIFIED., .F., .F.,
 ( 4, 3, 3, 3, 4 ),
 ( 0.9325643982709880264, 0.9611848085218949178, 1.006251133202479942, 1.031824629410019956, 1.051317457883059969 ),
 .UNSPECIFIED. ) ;
#56179 = VERTEX_POINT ( 'NONE', #95716 ) ;
#56180 = CARTESIAN_POINT ( 'NONE',  ( -2.490245952555000031, 1516.691389976299888, 204.5134284255869943 ) ) ;
#56181 = CARTESIAN_POINT ( 'NONE',  ( 6.178286635010000083, 1406.300107697530166, 266.9460459613980561 ) ) ;
#56182 = CARTESIAN_POINT ( 'NONE',  ( 0.7398872337349989836, 1515.545288638290003, 213.2458252406289887 ) ) ;
#56183 = DIRECTION ( 'NONE',  ( -0.1669062194215500117, 0.3715217273458689684, 0.9132983740423209484 ) ) ;
#56184 = EDGE_CURVE ( 'NONE', #97980, #23359, #58110, .T. ) ;
#56185 = CARTESIAN_POINT ( 'NONE',  ( 23.66594833135497566, 1434.290763647069980, 214.6250708475496936 ) ) ;
#56186 = EDGE_CURVE ( 'NONE', #30404, #76248, #3888, .T. ) ;
#56187 = CARTESIAN_POINT ( 'NONE',  ( -7.150360519070535936, 1512.239113741255551, 202.0236829662010791 ) ) ;
#56188 = CARTESIAN_POINT ( 'NONE',  ( 17.14319438672604434, 1499.112856636860215, 222.9242983244725167 ) ) ;
#56189 = EDGE_CURVE ( 'NONE', #96843, #35341, #49739, .T. ) ;
#56190 = FACE_OUTER_BOUND ( 'NONE', #33041, .T. ) ;
#56191 = CARTESIAN_POINT ( 'NONE',  ( -0.8767898181709999905, 1450.882442212199976, 155.6080925170979867 ) ) ;
#56192 = CARTESIAN_POINT ( 'NONE',  ( -1.673374938852186133, 1450.582197054855669, 183.1029605669776288 ) ) ;
#56193 = ADVANCED_FACE ( 'NONE', ( #70547 ), #82770, .F. ) ;
#56194 = CARTESIAN_POINT ( 'NONE',  ( 2.500000002650000219, 1449.201558846790022, 155.6080914321979947 ) ) ;
#56195 = EDGE_CURVE ( 'NONE', #84984, #110163, #87005, .T. ) ;
#56196 = CARTESIAN_POINT ( 'NONE',  ( -13.46591419205600104, 1415.020374539180011, 220.3865122175670024 ) ) ;
#56197 = CARTESIAN_POINT ( 'NONE',  ( 11.99447453070000158, 1410.787978747230227, 219.9627944869979785 ) ) ;
#56198 = CARTESIAN_POINT ( 'NONE',  ( -23.03655027839999647, 1423.631548418229841, 255.3819207742980097 ) ) ;
#56199 = B_SPLINE_CURVE_WITH_KNOTS ( 'NONE', 5,
 ( #41957, #92899, #15613, #85589, #76111, #528, #8885, #17265, #50913, #94001, #102938, #49820 ),
 .UNSPECIFIED., .F., .F.,
 ( 6, 3, 3, 6 ),
 ( 0.000000000000000000, 0.2862565181357951682, 0.7620907940255700064, 1.000000000000000000 ),
 .UNSPECIFIED. ) ;
#56200 = B_SPLINE_CURVE_WITH_KNOTS ( 'NONE', 3,
 ( #70395, #104513, #11011, #94434, #12660, #29449, #72055, #64188, #56325, #63646, #71513, #46839, #3190, #80425, #39519, #55794, #65288, #105632, #98310, #55236, #99401, #38403, #80968, #89369, #72579, #29997, #4273, #79876, #38944, #3737, #46297, #37318, #106170, #21588, #54141, #106707, #13735, #28919, #89909, #13183, #47372, #81497, #4799 ),
 .UNSPECIFIED., .F., .F.,
 ( 4, 3, 3, 3, 3, 3, 3, 3, 3, 3, 3, 3, 3, 3, 4 ),
 ( -1.999999996503429855, -1.941402971639760056, -1.796657287308599971, -1.649920620429889961, -1.501917604718239874, -1.352028961624889947, -1.201168230678989923, -1.049651953167649809, -0.8978420048550590504, -0.7403908631910058880, -0.5896658738122080301, -0.4400322845055311127, -0.2917605857772640476, -0.1450427803553220318, 0.000000000000000000 ),
 .UNSPECIFIED. ) ;
#56201 = CARTESIAN_POINT ( 'NONE',  ( -27.33473054107770039, 1507.985401980800134, 210.9306764114709836 ) ) ;
#56202 = CARTESIAN_POINT ( 'NONE',  ( 2.500000000000000000, 1439.245504089100223, 159.3587695534980071 ) ) ;
#56203 = CARTESIAN_POINT ( 'NONE',  ( -2.776816374990000114, 1476.015124969530007, 267.5339340712980061 ) ) ;
#56204 = CARTESIAN_POINT ( 'NONE',  ( -11.44378745049835544, 1425.812029265508500, 138.6329405890633666 ) ) ;
#56205 = CARTESIAN_POINT ( 'NONE',  ( -21.12212911286992068, 1511.187213306747708, 235.8226600804187285 ) ) ;
#56206 = DIRECTION ( 'NONE',  ( 0.000000000000000000, 1.000000000000000000, 0.000000000000000000 ) ) ;
#56207 = CARTESIAN_POINT ( 'NONE',  ( -27.53652019058529987, 1384.837329755710016, 225.6946210897860112 ) ) ;
#56208 = FACE_OUTER_BOUND ( 'NONE', #32284, .T. ) ;
#56209 = CIRCLE ( 'NONE', #106313, 24.69926344187880929 ) ;
#56210 = DIRECTION ( 'NONE',  ( -1.755985294532469921E-16, 1.000000000000000000, -1.338183447452831989E-16 ) ) ;
#56211 = B_SPLINE_SURFACE_WITH_KNOTS ( 'NONE', 4, 5, ( 
 ( #89404, #11597, #46873, #71550, #19983, #38435 ),
 ( #47409, #53626, #19424, #106742, #54177, #30029 ),
 ( #54726, #64223, #107302, #88305, #105671, #89944 ),
 ( #30595, #64783, #14880, #107849, #5394, #41748 ),
 ( #49071, #74818, #31138, #57478, #56361, #66974 ) ),
 .UNSPECIFIED., .F., .F., .F.,
 ( 5, 5 ),
 ( 6, 6 ),
 ( 0.000000000000000000, 1.224053340420000024 ),
 ( 0.000000000000000000, 2.000000000000000000 ),
 .UNSPECIFIED. ) ;
#56212 = CARTESIAN_POINT ( 'NONE',  ( -105.1701305670000011, 1379.114535495230029, 304.0350737403589960 ) ) ;
#56213 = CARTESIAN_POINT ( 'NONE',  ( 32.16567119605107195, 1524.523992613102564, 216.1007008506254579 ) ) ;
#56214 = CARTESIAN_POINT ( 'NONE',  ( 0.2253789646234576893, 1420.493552874686429, 182.7575710290123823 ) ) ;
#56215 = CARTESIAN_POINT ( 'NONE',  ( -1.793404623366990247, 1395.975687456799960, 219.9892326746640094 ) ) ;
#56216 = ADVANCED_FACE ( 'NONE', ( #12805 ), #48642, .F. ) ;
#56217 = CARTESIAN_POINT ( 'NONE',  ( 12.51197819060429950, 1421.582269804420093, 207.2823425885030133 ) ) ;
#56218 = CARTESIAN_POINT ( 'NONE',  ( 19.57339925981531792, 1455.491367452954591, 225.8543147067736641 ) ) ;
#56219 = ORIENTED_EDGE ( 'NONE', *, *, #27677, .F. ) ;
#56220 = CARTESIAN_POINT ( 'NONE',  ( -5.074604691638342047, 1410.465630996212440, 231.8427962307575001 ) ) ;
#56222 = EDGE_CURVE ( 'NONE', #108882, #89343, #62590, .T. ) ;
#56221 = DIRECTION ( 'NONE',  ( 4.465978680329379737E-17, 1.000000000000000000, -2.349386720892264891E-16 ) ) ;
#56223 = CARTESIAN_POINT ( 'NONE',  ( 19.03958014025380052, 1453.804227312760077, 200.7927590372679845 ) ) ;
#56225 = CARTESIAN_POINT ( 'NONE',  ( -11.46842534956499904, 1512.169992403149990, 193.0028033113669892 ) ) ;
#56224 = CARTESIAN_POINT ( 'NONE',  ( 11.67304687340000058, 1426.321999969329909, 139.6389216567980043 ) ) ;
#56226 = CARTESIAN_POINT ( 'NONE',  ( 10.47043688597563005, 1517.151704408390060, 197.0050518223378333 ) ) ;
#56227 = EDGE_CURVE ( 'NONE', #51438, #53542, #98150, .T. ) ;
#56228 = CARTESIAN_POINT ( 'NONE',  ( -5.788280361890000059, 1452.919697783089987, 200.3898760574089977 ) ) ;
#56229 = CARTESIAN_POINT ( 'NONE',  ( 1.124894050234999998, 1517.194816588360027, 202.1703287997270309 ) ) ;
#56230 = CARTESIAN_POINT ( 'NONE',  ( 11.45577226660000036, 1502.286415424589904, 208.3140783707030153 ) ) ;
#56231 = CARTESIAN_POINT ( 'NONE',  ( -18.80014186020000011, 1505.319236276690162, 222.5373108268989881 ) ) ;
#56232 = CARTESIAN_POINT ( 'NONE',  ( 6.820844401089999565, 1507.852259759629987, 182.4337134681979933 ) ) ;
#56233 = CARTESIAN_POINT ( 'NONE',  ( -20.32951113500139684, 1418.531963503440011, 207.2355206635010063 ) ) ;
#56234 = CARTESIAN_POINT ( 'NONE',  ( -55.69680533319999682, 1376.605089213109977, 260.2049226822590526 ) ) ;
#56235 = EDGE_CURVE ( 'NONE', #76242, #94251, #46018, .T. ) ;
#56236 = CARTESIAN_POINT ( 'NONE',  ( 3.756023522788400015, 1369.098589419797918, 210.6218459616987957 ) ) ;
#56238 = ORIENTED_EDGE ( 'NONE', *, *, #102675, .T. ) ;
#56237 = CARTESIAN_POINT ( 'NONE',  ( 3.487592431604999987, 1508.551704408389924, 204.1347675156769981 ) ) ;
#56239 = ORIENTED_EDGE ( 'NONE', *, *, #18001, .F. ) ;
#56240 = CARTESIAN_POINT ( 'NONE',  ( -11.64940060459999849, 1396.319866421030156, 207.5851092805380063 ) ) ;
#56241 = CARTESIAN_POINT ( 'NONE',  ( -20.51953016590000090, 1409.793898084230023, 218.1559997793979733 ) ) ;
#56242 = CARTESIAN_POINT ( 'NONE',  ( 0.04641543339558022729, 1519.551704408389924, 187.8934844797931305 ) ) ;
#56243 = CARTESIAN_POINT ( 'NONE',  ( -13.05984560479545209, 1444.833622568467035, 169.4122135708499286 ) ) ;
#56244 = CARTESIAN_POINT ( 'NONE',  ( 21.29766439678459733, 1509.704854597507619, 229.9147211563969506 ) ) ;
#56245 = CARTESIAN_POINT ( 'NONE',  ( -7.684243113244999535, 1511.930588878439949, 211.8885908927369996 ) ) ;
#56247 = CARTESIAN_POINT ( 'NONE',  ( 17.00560939319999676, 1410.862827255230059, 226.2920145422980340 ) ) ;
#56246 = CARTESIAN_POINT ( 'NONE',  ( -7.991901621120000243, 1383.415651595959844, 218.6863616538790041 ) ) ;
#56248 = CARTESIAN_POINT ( 'NONE',  ( 8.785620242860000317, 1429.761447237529865, 187.0031388449980057 ) ) ;
#56249 = CARTESIAN_POINT ( 'NONE',  ( -7.388976461649999550, 1415.087797054229895, 193.5183541347980167 ) ) ;
#56250 = CARTESIAN_POINT ( 'NONE',  ( -41.63068410086079751, 1444.585398277480181, 136.0329946082410117 ) ) ;
#56251 = FILL_AREA_STYLE ('',( #23179 ) ) ;
#56252 = CARTESIAN_POINT ( 'NONE',  ( 10.35233951385729867, 1396.274572049960170, 213.0386826886810070 ) ) ;
#56253 = DIRECTION ( 'NONE',  ( 0.9995237709234254808, 0.03085824620771311644, 1.984178880230842443E-13 ) ) ;
#56254 = CARTESIAN_POINT ( 'NONE',  ( 11.82873555240000130, 1429.816408930329999, 149.3973828046979975 ) ) ;
#56255 = CARTESIAN_POINT ( 'NONE',  ( 8.991744574390811096, 1509.227061438039982, 181.2342617849590169 ) ) ;
#56256 = ORIENTED_EDGE ( 'NONE', *, *, #15827, .F. ) ;
#56257 = CARTESIAN_POINT ( 'NONE',  ( 4.156129378920000228, 1425.920013205530040, 185.3798846555979765 ) ) ;
#56258 = FACE_OUTER_BOUND ( 'NONE', #106106, .T. ) ;
#56259 = ORIENTED_EDGE ( 'NONE', *, *, #64711, .F. ) ;
#56260 = ORIENTED_EDGE ( 'NONE', *, *, #31669, .T. ) ;
#56261 = CARTESIAN_POINT ( 'NONE',  ( -15.22583482770000174, 1419.426620482320004, 199.2582349955389986 ) ) ;
#56262 = CARTESIAN_POINT ( 'NONE',  ( 3.756023522790000069, 1369.098589419769951, 207.6218459616989946 ) ) ;
#56263 = CARTESIAN_POINT ( 'NONE',  ( -108.7866006633440179, 1388.050027694506070, 310.6579109707056432 ) ) ;
#56264 = CARTESIAN_POINT ( 'NONE',  ( -28.54794148642340090, 1526.382868172864164, 198.4382598900959351 ) ) ;
#56265 = CARTESIAN_POINT ( 'NONE',  ( -7.716252091104999877, 1516.810037859429940, 216.0641906620670056 ) ) ;
#56266 = CARTESIAN_POINT ( 'NONE',  ( -3.054816033052110136, 1485.996906143959905, 182.1538611115439892 ) ) ;
#56267 = ORIENTED_EDGE ( 'NONE', *, *, #34587, .T. ) ;
#56268 = CARTESIAN_POINT ( 'NONE',  ( -16.66297624725529758, 1508.551704407369925, 213.1726019329240103 ) ) ;
#56269 = CARTESIAN_POINT ( 'NONE',  ( 2.500000000000000000, 1448.594374933610197, 159.2313818852420013 ) ) ;
#56270 = CARTESIAN_POINT ( 'NONE',  ( -36.43074434249999172, 1375.172836988449944, 219.9641098163590129 ) ) ;
#56271 =( BOUNDED_CURVE ( )  B_SPLINE_CURVE ( 3, ( #13705, #47892, #12636, #4242 ),
 .UNSPECIFIED., .F., .F. ) 
 B_SPLINE_CURVE_WITH_KNOTS ( ( 4, 4 ),
 ( 5.474490172796000031, 5.884916938985190527 ),
 .UNSPECIFIED. ) 
 CURVE ( )  GEOMETRIC_REPRESENTATION_ITEM ( )  RATIONAL_B_SPLINE_CURVE ( ( 1.000000000000000000, 0.9860116829598833954, 0.9860116829598833954, 1.000000000000000000 ) ) 
 REPRESENTATION_ITEM ( '' )  );
#56272 = CARTESIAN_POINT ( 'NONE',  ( 0.2707600216770000290, 1415.088016306429836, 226.0844321790980018 ) ) ;
#56273 = CARTESIAN_POINT ( 'NONE',  ( 4.611879685325000366, 1516.858533673840157, 204.4999481076869756 ) ) ;
#56274 = ORIENTED_EDGE ( 'NONE', *, *, #35047, .T. ) ;
#56275 = CARTESIAN_POINT ( 'NONE',  ( -0.7468175536419978666, 1517.006509894990131, 209.1289748073840258 ) ) ;
#56276 = CARTESIAN_POINT ( 'NONE',  ( -20.81411743600000008, 1509.690291818130163, 230.4138254417979681 ) ) ;
#56277 = CARTESIAN_POINT ( 'NONE',  ( -38.90820051305949079, 1429.376674070663967, 269.5913902092726744 ) ) ;
#56278 = CARTESIAN_POINT ( 'NONE',  ( 6.681558910155000142, 1511.816633140289923, 216.4059013884869955 ) ) ;
#56280 = ORIENTED_EDGE ( 'NONE', *, *, #49510, .T. ) ;
#56279 = CARTESIAN_POINT ( 'NONE',  ( -45.97229537702650504, 1578.884344667429787, 229.9350315244390117 ) ) ;
#56281 = CARTESIAN_POINT ( 'NONE',  ( 2.500000000000000000, 1432.232933817210096, 157.4922851969979831 ) ) ;
#56282 = CARTESIAN_POINT ( 'NONE',  ( -30.14115132559009780, 1440.913060386970074, 238.7996103749989913 ) ) ;
#56283 = VECTOR ( 'NONE', #22647, 1000.000000000000227 ) ;
#56284 = CARTESIAN_POINT ( 'NONE',  ( -47.43982414079999899, 1384.124103258099922, 256.2477275100589509 ) ) ;
#56286 = EDGE_CURVE ( 'NONE', #8260, #51946, #108868, .T. ) ;
#56285 = CARTESIAN_POINT ( 'NONE',  ( -0.06137319429855010722, 1466.040928358300107, 235.8553063735670037 ) ) ;
#56287 = CARTESIAN_POINT ( 'NONE',  ( 20.06106135328079887, 1413.496800473840267, 269.8982105628270460 ) ) ;
#56288 = AXIS2_PLACEMENT_3D ( 'NONE', #109335, #48333, #57836 ) ;
#56289 = CARTESIAN_POINT ( 'NONE',  ( 6.561686423234999843, 1517.069378699710114, 212.5741351528070027 ) ) ;
#56290 = CARTESIAN_POINT ( 'NONE',  ( -62.81000518919999109, 1379.749407722699971, 268.0377337381589768 ) ) ;
#56291 = VECTOR ( 'NONE', #88283, 1000.000000000000000 ) ;
#56292 = CARTESIAN_POINT ( 'NONE',  ( 22.92012589049999960, 1409.721659010730036, 209.2345283292779925 ) ) ;
#56293 = CARTESIAN_POINT ( 'NONE',  ( -20.99310762600000047, 1509.712614273529880, 187.9175820947980071 ) ) ;
#56294 = CARTESIAN_POINT ( 'NONE',  ( 11.86100282799569960, 1492.894947744830006, 212.5846961511890072 ) ) ;
#56295 = CARTESIAN_POINT ( 'NONE',  ( -11.60004869885203505, 1425.798876189259772, 137.3569514552391695 ) ) ;
#56296 = CARTESIAN_POINT ( 'NONE',  ( -6.546001388695000145, 1516.557392317769882, 210.8318505190270002 ) ) ;
#56297 = CARTESIAN_POINT ( 'NONE',  ( 4.235082444282669556, 1421.836746427100024, 184.3796511902140196 ) ) ;
#56298 = CARTESIAN_POINT ( 'NONE',  ( 0.4649457434059999783, 1418.687271102530076, 184.7086881091979933 ) ) ;
#56299 = CARTESIAN_POINT ( 'NONE',  ( 6.736113117885867752, 1420.681901958687149, 137.0999999980981841 ) ) ;
#56301 = ORIENTED_EDGE ( 'NONE', *, *, #15964, .F. ) ;
#56300 = CARTESIAN_POINT ( 'NONE',  ( -22.66379694789999988, 1390.973251371299966, 211.6870299638790129 ) ) ;
#56302 = CARTESIAN_POINT ( 'NONE',  ( -33.87156971251739890, 1385.214877942069961, 232.6218372687270062 ) ) ;
#56303 = ADVANCED_FACE ( 'NONE', ( #107965 ), #51372, .T. ) ;
#56304 = CARTESIAN_POINT ( 'NONE',  ( 31.32995031131192931, 1523.678648413191695, 196.3423562208913324 ) ) ;
#56305 = CARTESIAN_POINT ( 'NONE',  ( 0.5533832822140000163, 1417.008313040729945, 234.1272609293980054 ) ) ;
#56306 = DIRECTION ( 'NONE',  ( -0.02616798426450838572, 0.9993150019883944024, -0.02616798426450848286 ) ) ;
#56307 = CARTESIAN_POINT ( 'NONE',  ( -24.90665996499999935, 1442.497388197319879, 210.4939798944579934 ) ) ;
#56308 = CARTESIAN_POINT ( 'NONE',  ( 10.66733264550000015, 1424.097486430830031, 205.6386333492189920 ) ) ;
#56309 = PLANE ( 'NONE',  #89802 ) ;
#56311 = CARTESIAN_POINT ( 'NONE',  ( 21.54116136303176532, 1523.462669333491021, 183.9310736449011188 ) ) ;
#56310 = CARTESIAN_POINT ( 'NONE',  ( -3.453544863754999472, 1517.106845464700200, 216.4586906126469898 ) ) ;
#56312 = DIRECTION ( 'NONE',  ( -0.9993902469235412811, -0.03489947644508390595, 0.001077449749359510062 ) ) ;
#56313 = CARTESIAN_POINT ( 'NONE',  ( 33.42844755915471211, 1522.861859112238790, 222.1271778627165929 ) ) ;
#56314 = ORIENTED_EDGE ( 'NONE', *, *, #51655, .T. ) ;
#56315 = CARTESIAN_POINT ( 'NONE',  ( -4.617490504904999682, 1516.685667699390024, 201.7969310139470167 ) ) ;
#56316 = CARTESIAN_POINT ( 'NONE',  ( -15.00522600296499931, 1511.839858410419993, 221.0503446609669993 ) ) ;
#56317 = EDGE_LOOP ( 'NONE', ( #69669, #67825, #8952, #100834 ) ) ;
#56318 = DIRECTION ( 'NONE',  ( -0.000000000000000000, -1.000000000000000000, -0.000000000000000000 ) ) ;
#56319 = B_SPLINE_CURVE_WITH_KNOTS ( 'NONE', 3,
 ( #38054, #71137, #3373, #81145, #20137, #53790, #72231, #47020, #29641, #61621, #53220 ),
 .UNSPECIFIED., .F., .F.,
 ( 4, 2, 1, 2, 2, 4 ),
 ( 0.000000000000000000, 0.2500000000000126565, 0.3750000000000736078, 0.4375000000000877076, 0.5000000000001018075, 1.000000000000000000 ),
 .UNSPECIFIED. ) ;
#56320 = EDGE_CURVE ( 'NONE', #79053, #28929, #25945, .T. ) ;
#56321 = CARTESIAN_POINT ( 'NONE',  ( 23.85401727289999840, 1447.123143008870102, 216.1985342456480055 ) ) ;
#56322 = CARTESIAN_POINT ( 'NONE',  ( 8.292451526740862278, 1437.777547255205945, 153.5278875412344632 ) ) ;
#56323 = CARTESIAN_POINT ( 'NONE',  ( 9.439522638037985303, 1425.330077423237753, 195.5546044094537876 ) ) ;
#56324 = CARTESIAN_POINT ( 'NONE',  ( 2.723688281249999843, 1443.346472895189891, 217.6079121182089864 ) ) ;
#56325 = CARTESIAN_POINT ( 'NONE',  ( -26.41719155878330128, 1508.429547602710045, 201.5167586753940157 ) ) ;
#56326 = CARTESIAN_POINT ( 'NONE',  ( -3.117854675340000270, 1446.609948778509988, 165.9235426434980241 ) ) ;
#56328 = EDGE_CURVE ( 'NONE', #51048, #37552, #37627, .T. ) ;
#56327 = CARTESIAN_POINT ( 'NONE',  ( -19.80431309490000302, 1426.801393628430105, 224.9940485357979867 ) ) ;
#56329 = CARTESIAN_POINT ( 'NONE',  ( -24.39385583620000020, 1435.492268184149907, 137.6392094220979914 ) ) ;
#56330 = CARTESIAN_POINT ( 'NONE',  ( -103.8055019550000111, 1389.814814112089834, 301.7479020532589971 ) ) ;
#56331 = CARTESIAN_POINT ( 'NONE',  ( 17.25705130249999897, 1509.016679772330008, 187.6328010954979959 ) ) ;
#56333 = CARTESIAN_POINT ( 'NONE',  ( -18.83575481127647677, 1438.179160179573500, 211.0549776618481701 ) ) ;
#56332 = CARTESIAN_POINT ( 'NONE',  ( 0.2723178306860529752, 1409.428891657669737, 233.0102446141029873 ) ) ;
#56334 = AXIS2_PLACEMENT_3D ( 'NONE', #100724, #8325, #110795 ) ;
#56335 = CARTESIAN_POINT ( 'NONE',  ( -30.25377815386013935, 1462.061561754708464, 269.4735075012114294 ) ) ;
#56336 = ORIENTED_EDGE ( 'NONE', *, *, #33687, .T. ) ;
#56337 = CARTESIAN_POINT ( 'NONE',  ( 10.41132050455482982, 1517.151704408390060, 228.7775216444308342 ) ) ;
#56338 = CARTESIAN_POINT ( 'NONE',  ( -11.44378878220000040, 1508.484295304989928, 218.0962685049790082 ) ) ;
#56339 = CARTESIAN_POINT ( 'NONE',  ( -10.76706410755489429, 1424.951753425542847, 141.1458295590867067 ) ) ;
#56340 = EDGE_CURVE ( 'NONE', #98544, #43306, #49091, .T. ) ;
#56341 = CARTESIAN_POINT ( 'NONE',  ( 10.82738100200000098, 1427.328250305469965, 209.3702396267119923 ) ) ;
#56342 = CARTESIAN_POINT ( 'NONE',  ( -8.407921469289998839, 1475.513060387329915, 228.4380765505979980 ) ) ;
#56343 = CARTESIAN_POINT ( 'NONE',  ( 1.460159494251919821, 1495.777843760759879, 181.6077353377199870 ) ) ;
#56344 = CARTESIAN_POINT ( 'NONE',  ( -0.1157304452309999981, 1415.757619356030091, 233.4560891803980098 ) ) ;
#56345 = CARTESIAN_POINT ( 'NONE',  ( -13.47420130509332914, 1443.596551666932100, 187.1131726174379821 ) ) ;
#56346 = B_SPLINE_SURFACE_WITH_KNOTS ( 'NONE', 5, 5, ( 
 ( #45629, #78651, #27694, #10332, #71396, #106058 ),
 ( #35534, #44504, #20374, #28802, #88165, #54579 ),
 ( #71946, #105512, #88714, #69729, #3075, #87613 ),
 ( #103847, #11994, #63537, #11453, #55127, #29336 ),
 ( #79216, #1966, #19830, #45073, #89249, #18716 ),
 ( #37202, #80857, #36103, #97653, #20923, #12545 ),
 ( #46723, #46177, #2524, #27147, #80307, #95451 ),
 ( #36646, #37752, #28243, #61880, #70289, #52912 ),
 ( #87044, #104399, #95996, #19265, #53468, #10900 ) ),
 .UNSPECIFIED., .F., .F., .F.,
 ( 6, 3, 6 ),
 ( 6, 6 ),
 ( 8.882670574839030664, 17.48889048929999745, 28.89006134397099856 ),
 ( -0.0006675929709739749978, 2.000000000000000000 ),
 .UNSPECIFIED. ) ;
#56347 = CARTESIAN_POINT ( 'NONE',  ( -17.09817538394500147, 1414.913526854310021, 207.6506234252330216 ) ) ;
#56348 = CARTESIAN_POINT ( 'NONE',  ( -4.987078467906759904, 1508.551704408389924, 213.0804802153340063 ) ) ;
#56349 = EDGE_CURVE ( 'NONE', #52504, #16564, #101839, .T. ) ;
#56350 = CARTESIAN_POINT ( 'NONE',  ( -13.86092847646930082, 1410.765486861110048, 227.1170286572800023 ) ) ;
#56351 = CARTESIAN_POINT ( 'NONE',  ( -15.23530766198840247, 1415.677402202029953, 208.5045630004590009 ) ) ;
#56352 = CARTESIAN_POINT ( 'NONE',  ( 23.87593678670000230, 1435.337375081109940, 137.1350274835979803 ) ) ;
#56353 = FACE_OUTER_BOUND ( 'NONE', #94472, .T. ) ;
#56355 = EDGE_LOOP ( 'NONE', ( #104692, #2272, #89177, #107319 ) ) ;
#56354 = CARTESIAN_POINT ( 'NONE',  ( -18.26023438560000045, 1443.256148476890075, 213.5656046648789754 ) ) ;
#56356 = CARTESIAN_POINT ( 'NONE',  ( -96.92558477839999398, 1380.099996794379877, 306.8584593190589658 ) ) ;
#56357 = CARTESIAN_POINT ( 'NONE',  ( 14.35493910357529934, 1513.426431439630278, 224.2887426523980139 ) ) ;
#56358 = VERTEX_POINT ( 'NONE', #93912 ) ;
#56359 = ORIENTED_EDGE ( 'NONE', *, *, #64067, .T. ) ;
#56360 = CARTESIAN_POINT ( 'NONE',  ( -11.59590396400000145, 1501.577258705189934, 209.7806602242469864 ) ) ;
#56361 = CARTESIAN_POINT ( 'NONE',  ( 12.70314174409999985, 1508.075973130829880, 233.3727141454980085 ) ) ;
#56363 = CARTESIAN_POINT ( 'NONE',  ( -30.28727319840000121, 1444.847842080029977, 240.1330978262979841 ) ) ;
#56362 = CARTESIAN_POINT ( 'NONE',  ( 20.75139895264628009, 1414.320554380318072, 269.3935123240341341 ) ) ;
#56364 = CARTESIAN_POINT ( 'NONE',  ( -20.51588922700000239, 1505.140427506229798, 190.4683942995980033 ) ) ;
#56365 = EDGE_CURVE ( 'NONE', #50617, #53780, #32374, .T. ) ;
#56366 = CARTESIAN_POINT ( 'NONE',  ( -11.87470928319999963, 1433.125601036669877, 150.1735720417980247 ) ) ;
#56367 = CARTESIAN_POINT ( 'NONE',  ( -3.744312463830716364, 1509.032014876046560, 213.3627910111590325 ) ) ;
#56368 = CARTESIAN_POINT ( 'NONE',  ( 11.69192323821640045, 1426.725590720729997, 140.9428211002000069 ) ) ;
#56369 = CARTESIAN_POINT ( 'NONE',  ( 9.379383068953968561, 1464.448945081789816, 212.0712950165349753 ) ) ;
#56370 = CARTESIAN_POINT ( 'NONE',  ( -0.4681535437661810684, 1524.397344074319335, 244.4282029790937827 ) ) ;
#56372 = EDGE_CURVE ( 'NONE', #30502, #106529, #67097, .T. ) ;
#56371 = CARTESIAN_POINT ( 'NONE',  ( -1.364625987752019931, 1515.082030188920044, 213.4508433624550037 ) ) ;
#56373 = CARTESIAN_POINT ( 'NONE',  ( 5.630091722370000440, 1441.487383641189808, 154.7801822668979810 ) ) ;
#56374 = CARTESIAN_POINT ( 'NONE',  ( -11.31069869211509982, 1480.704413556870122, 212.4820440049689978 ) ) ;
#56375 = CARTESIAN_POINT ( 'NONE',  ( 3.426613460960000079, 1360.656565846710009, 207.6218459616989946 ) ) ;
#56376 = CARTESIAN_POINT ( 'NONE',  ( -10.68607904894687444, 1509.411632735550029, 237.1549078682182312 ) ) ;
#56378 = ORIENTED_EDGE ( 'NONE', *, *, #75055, .T. ) ;
#56377 = CARTESIAN_POINT ( 'NONE',  ( -1.599724557440349957E-10, 1412.168762487870026, 253.0958361106100369 ) ) ;
#56379 = ORIENTED_EDGE ( 'NONE', *, *, #87675, .T. ) ;
#56380 = DIRECTION ( 'NONE',  ( 0.9858563016923833633, 0.000000000000000000, 0.1675928173085483863 ) ) ;
#56381 = AXIS2_PLACEMENT_3D ( 'NONE', #24087, #66146, #7851 ) ;
#56382 = CARTESIAN_POINT ( 'NONE',  ( 24.14616426090000090, 1497.622512133290002, 206.6541300447790093 ) ) ;
#56383 = CARTESIAN_POINT ( 'NONE',  ( -28.35914775050000003, 1465.186344805629915, 270.3509322670980168 ) ) ;
#56384 = CARTESIAN_POINT ( 'NONE',  ( 0.1569171403356077743, 1473.463532820902628, 219.3464626023122150 ) ) ;
#56385 = CARTESIAN_POINT ( 'NONE',  ( -107.2836002040342152, 1378.528619065189787, 314.5328508192586128 ) ) ;
#56386 = CARTESIAN_POINT ( 'NONE',  ( 33.91363303768119408, 1450.440614253119975, 136.2454530761589808 ) ) ;
#56387 = CARTESIAN_POINT ( 'NONE',  ( 0.2058156135791029961, 1452.245535141509890, 183.1437243635440097 ) ) ;
#56388 = DIRECTION ( 'NONE',  ( -0.9417419115949053898, -0.3363363969979660806, 0.000000000000000000 ) ) ;
#56389 = CARTESIAN_POINT ( 'NONE',  ( -2.470168521978398424, 1523.382868172864164, 175.3649660270905315 ) ) ;
#56390 = CARTESIAN_POINT ( 'NONE',  ( -4.816250906239999630, 1456.991639154389986, 217.3233113361989979 ) ) ;
#56391 = CARTESIAN_POINT ( 'NONE',  ( 10.88871838020139826, 1364.006426590386127, 207.6218459616987673 ) ) ;
#56392 = CARTESIAN_POINT ( 'NONE',  ( -42.13315488374279738, 1426.265673821560085, 268.3403209545570007 ) ) ;
#56393 = ORIENTED_EDGE ( 'NONE', *, *, #54357, .F. ) ;
#56394 = CARTESIAN_POINT ( 'NONE',  ( -20.99310762600000047, 1509.712614273529880, 187.9175820947980071 ) ) ;
#56395 = ORIENTED_EDGE ( 'NONE', *, *, #2861, .T. ) ;
#56396 = EDGE_LOOP ( 'NONE', ( #3549, #4851, #1452, #93135, #12878 ) ) ;
#56397 = CARTESIAN_POINT ( 'NONE',  ( 4.625693865015000128, 1517.042661899400173, 211.4082922958669997 ) ) ;
#56398 = PLANE ( 'NONE',  #51963 ) ;
#56399 = B_SPLINE_CURVE_WITH_KNOTS ( 'NONE', 3,
 ( #11314, #37046, #96971, #20235, #54436, #11853, #86345, #35396, #46026, #80154 ),
 .UNSPECIFIED., .F., .F.,
 ( 4, 2, 2, 2, 4 ),
 ( 0.000000000000000000, 0.2500000000000000000, 0.5000000000000000000, 0.7500000000000000000, 1.000000000000000000 ),
 .UNSPECIFIED. ) ;
#56401 = CARTESIAN_POINT ( 'NONE',  ( -17.63428006580305762, 1419.704475380900021, 206.9647618039389272 ) ) ;
#56400 = CARTESIAN_POINT ( 'NONE',  ( -6.934528567894999718, 1516.588006113850042, 211.9958048218269937 ) ) ;
#56402 = CARTESIAN_POINT ( 'NONE',  ( -12.73123357059999883, 1455.447220867429905, 187.4137537217980025 ) ) ;
#56403 = CARTESIAN_POINT ( 'NONE',  ( -2.399591520910798970, 1449.521109860346769, 183.0206712615461413 ) ) ;
#56404 = VERTEX_POINT ( 'NONE', #43538 ) ;
#56405 = CARTESIAN_POINT ( 'NONE',  ( -26.65016812680000058, 1436.423441677409983, 136.7215463643979945 ) ) ;
#56406 = CIRCLE ( 'NONE', #108260, 12.50000000000001066 ) ;
#56407 = B_SPLINE_CURVE_WITH_KNOTS ( 'NONE', 3,
 ( #84132, #8521, #66275, #57859, #94184, #41598, #42698 ),
 .UNSPECIFIED., .F., .F.,
 ( 4, 3, 4 ),
 ( -157.7301682620000065, -100.4765462162850014, -30.40177460649999830 ),
 .UNSPECIFIED. ) ;
#56408 = CARTESIAN_POINT ( 'NONE',  ( 7.328676169885000036, 1516.833844030519913, 202.1788723028969912 ) ) ;
#56409 = CARTESIAN_POINT ( 'NONE',  ( 1.546943247107299912, 1416.828039266790029, 190.2227890105679933 ) ) ;
#56411 = AXIS2_PLACEMENT_3D ( 'NONE', #17102, #67023, #24425 ) ;
#56410 = CARTESIAN_POINT ( 'NONE',  ( -20.87069991009999725, 1506.658021081189872, 214.5368842940590071 ) ) ;
#56412 =( BOUNDED_CURVE ( )  B_SPLINE_CURVE ( 3, ( #23585, #65619, #58860, #16266 ),
 .UNSPECIFIED., .F., .T. ) 
 B_SPLINE_CURVE_WITH_KNOTS ( ( 4, 4 ),
 ( 5.447131716497097820, 6.315249268837944463 ),
 .UNSPECIFIED. ) 
 CURVE ( )  GEOMETRIC_REPRESENTATION_ITEM ( )  RATIONAL_B_SPLINE_CURVE ( ( 1.000000000000000000, 0.9381775213689819148, 0.9381775213689819148, 1.000000000000000000 ) ) 
 REPRESENTATION_ITEM ( '' )  );
#56413 = CARTESIAN_POINT ( 'NONE',  ( -17.66551557828621455, 1519.551704408389924, 200.3426142980228519 ) ) ;
#56414 = CARTESIAN_POINT ( 'NONE',  ( -11.15625518848249875, 1488.131838085029813, 191.4014358787470087 ) ) ;
#56415 = CARTESIAN_POINT ( 'NONE',  ( -1.248605592450000135, 1397.026870444829910, 196.3012639762980029 ) ) ;
#56417 = EDGE_LOOP ( 'NONE', ( #48497, #34235, #18749, #40058 ) ) ;
#56416 = CARTESIAN_POINT ( 'NONE',  ( -8.988712649806421595, 1365.105188660967315, 207.6218459616988241 ) ) ;
#56418 = VERTEX_POINT ( 'NONE', #109092 ) ;
#56419 = CARTESIAN_POINT ( 'NONE',  ( 3.756948166784984444, 1425.519882450703790, 185.1998084200467360 ) ) ;
#56420 = CARTESIAN_POINT ( 'NONE',  ( -9.171139168049998958, 1384.273561242960113, 200.0050165398689899 ) ) ;
#56421 = EDGE_CURVE ( 'NONE', #80510, #15749, #32904, .T. ) ;
#56422 = CARTESIAN_POINT ( 'NONE',  ( -14.15891404902520101, 1436.253324085039822, 150.1419714444780027 ) ) ;
#56423 = CARTESIAN_POINT ( 'NONE',  ( -0.03301841822632249623, 1409.280491802830056, 185.5015438497439959 ) ) ;
#56424 = CARTESIAN_POINT ( 'NONE',  ( 2.882325979385000014, 1516.969638403840008, 210.8235757905769674 ) ) ;
#56425 = CARTESIAN_POINT ( 'NONE',  ( -68.78237022239999021, 1379.747949065490047, 280.2620412852589880 ) ) ;
#56426 = CARTESIAN_POINT ( 'NONE',  ( 2.877999451269170006, 1440.267615723689914, 157.3979800045339914 ) ) ;
#56427 = CARTESIAN_POINT ( 'NONE',  ( 6.020898984694619038, 1441.354597694899894, 215.7047724842319667 ) ) ;
#56428 = CARTESIAN_POINT ( 'NONE',  ( -0.3530891408735000181, 1467.116854267079816, 235.6078141451939985 ) ) ;
#56429 = CARTESIAN_POINT ( 'NONE',  ( 7.556166211784999476, 1510.696675236759802, 204.6602201360370259 ) ) ;
#56430 = CARTESIAN_POINT ( 'NONE',  ( 6.935801261535000428, 1516.621991115350056, 207.9918434378369909 ) ) ;
#56431 = ORIENTED_EDGE ( 'NONE', *, *, #71701, .T. ) ;
#56432 = CARTESIAN_POINT ( 'NONE',  ( -40.71747596219490362, 1448.637563214449983, 135.0584856682299915 ) ) ;
#56433 = CARTESIAN_POINT ( 'NONE',  ( -1.275439650553358728, 1516.597747113053174, 201.7236143332039546 ) ) ;
#56434 = ORIENTED_EDGE ( 'NONE', *, *, #106265, .T. ) ;
#56435 = CARTESIAN_POINT ( 'NONE',  ( 6.284459336901857540, 1456.900407391064164, 227.9284455267091971 ) ) ;
#56436 = EDGE_CURVE ( 'NONE', #27843, #56695, #24496, .T. ) ;
#56437 = CARTESIAN_POINT ( 'NONE',  ( 24.04111616115019956, 1452.073549554080046, 136.7274035651190047 ) ) ;
#56438 = CARTESIAN_POINT ( 'NONE',  ( -4.120589916571496758, 1440.000613734177932, 185.4544762516224807 ) ) ;
#56439 = CARTESIAN_POINT ( 'NONE',  ( 2.439001525050000119, 1430.488531030629929, 150.2249694046979869 ) ) ;
#56440 = CARTESIAN_POINT ( 'NONE',  ( 22.00429000609999974, 1410.601272653630076, 203.2767770488879933 ) ) ;
#56441 = CARTESIAN_POINT ( 'NONE',  ( -25.47400523009999773, 1435.387084339240118, 135.4904355849980107 ) ) ;
#56442 = CARTESIAN_POINT ( 'NONE',  ( -14.07423802120690759, 1379.606304211416273, 211.7193776285950833 ) ) ;
#56443 = FACE_OUTER_BOUND ( 'NONE', #68217, .T. ) ;
#56444 = CARTESIAN_POINT ( 'NONE',  ( 4.264584969141440141, 1441.193324268380138, 158.8347230198679938 ) ) ;
#56445 = DIRECTION ( 'NONE',  ( -0.6736849260863841948, 0.000000000000000000, 0.7390186874254148774 ) ) ;
#56446 = CARTESIAN_POINT ( 'NONE',  ( -1.708102627415000185, 1517.199196846569976, 215.6864246554469844 ) ) ;
#56447 = ORIENTED_EDGE ( 'NONE', *, *, #54906, .T. ) ;
#56448 = CARTESIAN_POINT ( 'NONE',  ( 7.708922318049459932, 1516.530126575629993, 206.7990132384589970 ) ) ;
#56449 = CARTESIAN_POINT ( 'NONE',  ( -7.722580352405000070, 1517.051704408389924, 207.5526846776770071 ) ) ;
#56450 = CARTESIAN_POINT ( 'NONE',  ( 31.22294729666630531, 1523.678648413191695, 222.8955943986478019 ) ) ;
#56451 = CYLINDRICAL_SURFACE ( 'NONE', #80591, 1.000000000000000888 ) ;
#56452 = AXIS2_PLACEMENT_3D ( 'NONE', #62006, #11028, #96126 ) ;
#56453 = CARTESIAN_POINT ( 'NONE',  ( -0.3775284373670010352, 1473.627497755890090, 219.3729426502989952 ) ) ;
#56454 = CARTESIAN_POINT ( 'NONE',  ( 10.88555504727585799, 1424.831830838460974, 138.2234079619712190 ) ) ;
#56455 = CARTESIAN_POINT ( 'NONE',  ( -21.38516915558007270, 1522.382868172863937, 180.3939891059723664 ) ) ;
#56456 = CARTESIAN_POINT ( 'NONE',  ( 17.86566981212778416, 1423.742594241267398, 225.9114519548369913 ) ) ;
#56458 = EDGE_CURVE ( 'NONE', #81793, #93757, #59505, .T. ) ;
#56457 = CARTESIAN_POINT ( 'NONE',  ( -105.3716458700000089, 1379.306619424940209, 302.1984682570590053 ) ) ;
#56459 = CARTESIAN_POINT ( 'NONE',  ( -22.08327125186962192, 1523.604703353109699, 184.4267662568473725 ) ) ;
#56460 = B_SPLINE_SURFACE_WITH_KNOTS ( 'NONE', 5, 5, ( 
 ( #6648, #47019, #4988, #109128, #91203, #4459, #74980, #21207, #81144 ),
 ( #13371, #83349, #72766, #30743, #23441, #106893, #32409, #49223, #30181 ),
 ( #21764, #15025, #57635, #22314, #12839, #81682, #82252, #31294, #31847 ),
 ( #66590, #65478, #99587, #64373, #55416, #39703, #89550, #98496, #39132 ),
 ( #14484, #55965, #90088, #47560, #73311, #107447, #82800, #64924, #22870 ),
 ( #13927, #99037, #56517, #90644, #73869, #48114, #107997, #57079, #6094 ),
 ( #48677, #74431, #66033, #108557, #100156, #60382, #75532, #16130, #23977 ),
 ( #9413, #94502, #8842, #7209, #17219, #33484, #50868, #93952, #34609 ),
 ( #58171, #101231, #85546, #67686, #17775, #84997, #100693, #50336, #24531 ),
 ( #77183, #101794, #102356, #76068, #110211, #2563, #93405, #25084, #51977 ),
 ( #36686, #59287, #8292, #15570, #76614, #7749, #43025, #110766, #86119 ),
 ( #34056, #43575, #68248, #41365, #16670, #42455, #51414, #68795, #25639 ),
 ( #59831, #58719, #486, #92854, #92300, #102895, #26194, #84462, #77724 ),
 ( #49772, #83903, #41914, #109667, #32942, #67132, #107192, #106634, #29923 ),
 ( #88199, #80896, #22049, #3665, #54618, #4728, #47843, #30481, #38872 ) ),
 .UNSPECIFIED., .F., .F., .F.,
 ( 6, 3, 3, 3, 6 ),
 ( 6, 3, 6 ),
 ( 7.927024885419999833, 11.42826484960000144, 13.38558606099999970, 18.01519608889999802, 29.56630841140000143 ),
 ( 0.000000000000000000, 1.000000000000000000, 2.000000000000000000 ),
 .UNSPECIFIED. ) ;
#56461 = CARTESIAN_POINT ( 'NONE',  ( 28.04879799853789990, 1440.913060387349788, 231.3508241056970292 ) ) ;
#56462 = CARTESIAN_POINT ( 'NONE',  ( -10.91660068633870040, 1470.741030163299911, 210.0515589738539859 ) ) ;
#56463 = DIRECTION ( 'NONE',  ( 1.000000000000000000, 2.249639673992789970E-32, 1.224646799147350002E-16 ) ) ;
#56464 = VERTEX_POINT ( 'NONE', #110726 ) ;
#56465 = EDGE_CURVE ( 'NONE', #33840, #42195, #103621, .T. ) ;
#56466 = ORIENTED_EDGE ( 'NONE', *, *, #39576, .F. ) ;
#56467 = CARTESIAN_POINT ( 'NONE',  ( 11.31759557404070016, 1479.526143735280129, 208.6190374719330123 ) ) ;
#56468 = EDGE_CURVE ( 'NONE', #1934, #70504, #91420, .T. ) ;
#56469 = CARTESIAN_POINT ( 'NONE',  ( -19.06723915664710134, 1485.490521620860136, 189.6150037022410118 ) ) ;
#56470 = CARTESIAN_POINT ( 'NONE',  ( -3.888849094689999841, 1441.863784636489981, 201.1563154678690069 ) ) ;
#56471 = DIRECTION ( 'NONE',  ( -0.03489949669041918917, 0.9993908270195176469, 2.562551298407829116E-09 ) ) ;
#56472 = LINE ( 'NONE', #90604, #60760 ) ;
#56473 = ADVANCED_FACE ( 'NONE', ( #56208 ), #87188, .T. ) ;
#56474 = CARTESIAN_POINT ( 'NONE',  ( -11.00301372470000061, 1492.094802143589959, 210.0154403701209844 ) ) ;
#56475 = DIRECTION ( 'NONE',  ( -1.956929670128506950E-14, 1.000000000000000000, 0.000000000000000000 ) ) ;
#56476 = CARTESIAN_POINT ( 'NONE',  ( -49.38114550753920184, 1383.812931905830055, 260.0689200899579419 ) ) ;
#56477 = CIRCLE ( 'NONE', #106585, 8.013264357029999729 ) ;
#56478 = CARTESIAN_POINT ( 'NONE',  ( -3.173602190014999991, 1510.830536680500245, 201.5621726280170094 ) ) ;
#56479 = CARTESIAN_POINT ( 'NONE',  ( 2.499945018050090173, 1419.382888684849831, 144.1035832394360057 ) ) ;
#56480 = CARTESIAN_POINT ( 'NONE',  ( -9.095279969299012279, 1384.912302393732489, 199.9427318356120793 ) ) ;
#56481 = CARTESIAN_POINT ( 'NONE',  ( 1.522424741549999849, 1465.680318652129927, 235.2040100185980123 ) ) ;
#56483 = EDGE_LOOP ( 'NONE', ( #36420, #86482, #103461, #60978 ) ) ;
#56482 = CARTESIAN_POINT ( 'NONE',  ( -6.958472253045926870, 1439.213523565861578, 154.2072493331847056 ) ) ;
#56484 = CARTESIAN_POINT ( 'NONE',  ( -0.5568085941520000137, 1452.298961472929932, 183.2685725910980068 ) ) ;
#56485 = CARTESIAN_POINT ( 'NONE',  ( -15.77939734220000112, 1380.225294738999992, 203.9934837876090228 ) ) ;
#56486 = CARTESIAN_POINT ( 'NONE',  ( 2.801140078911729780, 1508.551704408389924, 204.1530204508169959 ) ) ;
#56488 = VERTEX_POINT ( 'NONE', #90340 ) ;
#56487 = FACE_OUTER_BOUND ( 'NONE', #63137, .T. ) ;
#56489 = CARTESIAN_POINT ( 'NONE',  ( -2.775532924494999776, 1468.867458220450089, 187.4507044347560054 ) ) ;
#56490 = ORIENTED_EDGE ( 'NONE', *, *, #65041, .T. ) ;
#56491 = CIRCLE ( 'NONE', #31454, 3.000000000000002665 ) ;
#56492 = B_SPLINE_CURVE_WITH_KNOTS ( 'NONE', 3,
 ( #11411, #10281, #36596, #103803, #45579, #10855, #52865, #79721, #37151, #71347 ),
 .UNSPECIFIED., .F., .F.,
 ( 4, 2, 2, 2, 4 ),
 ( 4.187893579585400145E-10, 0.05103584884158749585, 0.1118202684977770006, 0.1535261566792579802, 0.2248365559521849910 ),
 .UNSPECIFIED. ) ;
#56493 = CARTESIAN_POINT ( 'NONE',  ( -10.77049225859999915, 1390.002812723860188, 215.5109487511890052 ) ) ;
#56494 = CARTESIAN_POINT ( 'NONE',  ( -3.542288683788669790, 1515.375307391110027, 205.1014397700139966 ) ) ;
#56495 = CARTESIAN_POINT ( 'NONE',  ( -1.368191914778909890, 1419.344528075180278, 185.2221190139939893 ) ) ;
#56496 = CARTESIAN_POINT ( 'NONE',  ( -11.60004869885204037, 1426.320647100494170, 137.6121510302394029 ) ) ;
#56497 = CARTESIAN_POINT ( 'NONE',  ( -105.6627448849999951, 1378.306900235799958, 302.9594593028589884 ) ) ;
#56498 = CARTESIAN_POINT ( 'NONE',  ( 4.334458048930000196, 1466.050308755590095, 219.2818749650989787 ) ) ;
#56499 = CARTESIAN_POINT ( 'NONE',  ( -10.06503061548759881, 1473.016423777250111, 207.3581855507599983 ) ) ;
#56500 = CARTESIAN_POINT ( 'NONE',  ( 0.9835760575869921807, 1408.947407620089962, 194.1588551325519916 ) ) ;
#56501 = CARTESIAN_POINT ( 'NONE',  ( 18.02091189525600257, 1424.326076159014065, 225.2020075002020008 ) ) ;
#56502 = CARTESIAN_POINT ( 'NONE',  ( 0.4863421998530879642, 1418.702335047680208, 184.7127968358159933 ) ) ;
#56503 = EDGE_CURVE ( 'NONE', #94490, #73277, #5314, .T. ) ;
#56504 = CARTESIAN_POINT ( 'NONE',  ( -19.68379069659999914, 1478.188077225129973, 191.4618426609980020 ) ) ;
#56505 = CARTESIAN_POINT ( 'NONE',  ( 20.71343476517535365, 1524.726013923371511, 238.3377464195763764 ) ) ;
#56506 = B_SPLINE_CURVE_WITH_KNOTS ( 'NONE', 3,
 ( #72233, #37502, #98499, #2283, #105259, #88997, #20674, #53222, #97942, #55419, #44826, #89553, #104703, #21210, #106357, #105826, #27998, #87929, #29643, #62183, #96870, #54333, #80054, #29104, #96309, #12842, #12285 ),
 .UNSPECIFIED., .F., .F.,
 ( 4, 2, 2, 1, 2, 2, 2, 2, 2, 2, 1, 1, 2, 2, 4 ),
 ( 0.000000000000000000, 0.06250000000007284451, 0.09375000000011163293, 0.1093750000001466327, 0.1171875000001659506, 0.1250000000001852685, 0.1875000000003016198, 0.2187500000003661516, 0.2500000000004307110, 0.3750000000006306067, 0.4375000000007188694, 0.4687500000007518430, 0.4843750000007574497, 0.5000000000007630563, 1.000000000000000000 ),
 .UNSPECIFIED. ) ;
#56507 = CARTESIAN_POINT ( 'NONE',  ( -3.697944654365331818, 1424.333247977674091, 185.3305522059991972 ) ) ;
#56508 = ORIENTED_EDGE ( 'NONE', *, *, #83012, .F. ) ;
#56509 = EDGE_LOOP ( 'NONE', ( #1604, #74180, #30420, #29815, #83360, #2019, #109312, #85402, #1210, #107345, #28171, #32244 ) ) ;
#56510 = ADVANCED_FACE ( 'NONE', ( #2661 ), #69863, .F. ) ;
#56511 = CARTESIAN_POINT ( 'NONE',  ( -6.766140062282060441, 1508.878901399440110, 216.3823901328790100 ) ) ;
#56512 = CARTESIAN_POINT ( 'NONE',  ( 18.18178698398020288, 1457.548798095479924, 228.6382434660380056 ) ) ;
#56513 = CARTESIAN_POINT ( 'NONE',  ( -11.56247775979999837, 1434.196947835160017, 151.3456684532980034 ) ) ;
#56514 = CARTESIAN_POINT ( 'NONE',  ( 12.87775475449820028, 1420.952780459589803, 203.1693138811060066 ) ) ;
#56515 = CARTESIAN_POINT ( 'NONE',  ( -31.81407709659898941, 1522.644714754857659, 221.9534378623325210 ) ) ;
#56516 = CARTESIAN_POINT ( 'NONE',  ( -15.41602167210000118, 1420.398127465669859, 211.2285070405490046 ) ) ;
#56517 = CARTESIAN_POINT ( 'NONE',  ( -109.1219531280000012, 1387.080370060750056, 310.9323500322590235 ) ) ;
#56518 = CARTESIAN_POINT ( 'NONE',  ( -7.494431781837549877, 1510.714321716100130, 215.2145461046430057 ) ) ;
#56519 = CARTESIAN_POINT ( 'NONE',  ( -8.538839991170000587, 1362.569232148550100, 207.6218459616989946 ) ) ;
#56520 = CARTESIAN_POINT ( 'NONE',  ( -45.66496797010459829, 1440.259989335280125, 266.1886939491620296 ) ) ;
#56521 = CARTESIAN_POINT ( 'NONE',  ( 3.351013500467394213, 1524.082740465118604, 176.2279750478597862 ) ) ;
#56522 = CARTESIAN_POINT ( 'NONE',  ( -2.881325412095000260, 1517.003078582959688, 208.0029426616869728 ) ) ;
#56523 = CARTESIAN_POINT ( 'NONE',  ( -9.035311967128309973, 1449.310921972689812, 210.7160965195329823 ) ) ;
#56524 = DIRECTION ( 'NONE',  ( -0.9455185755993177343, 0.000000000000000000, 0.3255681544571540909 ) ) ;
#56525 = CARTESIAN_POINT ( 'NONE',  ( -13.45595297782609912, 1435.788356003630042, 150.3939031303400213 ) ) ;
#56526 = CARTESIAN_POINT ( 'NONE',  ( -8.860009088490000906, 1384.987333740160011, 218.6842292965490060 ) ) ;
#56527 = CARTESIAN_POINT ( 'NONE',  ( -14.40559916593009859, 1379.612683021279963, 208.0847104623620112 ) ) ;
#56528 = CARTESIAN_POINT ( 'NONE',  ( 7.356777505606249434, 1425.075287227600029, 212.5424154620459944 ) ) ;
#56529 = AXIS2_PLACEMENT_3D ( 'NONE', #103640, #79555, #53258 ) ;
#56530 = VERTEX_POINT ( 'NONE', #54168 ) ;
#56531 = CARTESIAN_POINT ( 'NONE',  ( 9.545816653330000179, 1416.905270224830019, 240.4008508550979855 ) ) ;
#56532 = CARTESIAN_POINT ( 'NONE',  ( -28.02912970359999889, 1508.133041382029887, 207.5417885384179897 ) ) ;
#56534 = CARTESIAN_POINT ( 'NONE',  ( 26.80143075489152693, 1509.848986972751618, 220.9835789632684850 ) ) ;
#56533 = CARTESIAN_POINT ( 'NONE',  ( -11.54280425992789993, 1491.460494414069899, 206.8284951956839848 ) ) ;
#56535 = CARTESIAN_POINT ( 'NONE',  ( -0.6192716172230079419, 1407.650954247345226, 270.1377424647723728 ) ) ;
#56536 = CARTESIAN_POINT ( 'NONE',  ( -29.87496801699999693, 1440.913060384889832, 238.0574310451980296 ) ) ;
#56537 = CARTESIAN_POINT ( 'NONE',  ( -2.298816249929999778, 1486.462377136390160, 220.8289805357989906 ) ) ;
#56538 = CARTESIAN_POINT ( 'NONE',  ( -13.00495165122699959, 1452.458917468459958, 149.1238935609289911 ) ) ;
#56539 = CARTESIAN_POINT ( 'NONE',  ( -18.90720652019999903, 1416.826388498430106, 208.2175296474880213 ) ) ;
#56540 = EDGE_LOOP ( 'NONE', ( #80515, #10383, #91899, #2305 ) ) ;
#56541 = CARTESIAN_POINT ( 'NONE',  ( -108.0096200556839960, 1378.913060387299993, 299.9536600820459853 ) ) ;
#56542 = CARTESIAN_POINT ( 'NONE',  ( 5.170554601400000116, 1484.055082523290139, 219.7711189574989703 ) ) ;
#56543 = CARTESIAN_POINT ( 'NONE',  ( 14.39613795285440112, 1421.809772777419994, 229.5322598158189749 ) ) ;
#56544 = CARTESIAN_POINT ( 'NONE',  ( 11.45170634509999985, 1502.273088946489906, 208.2658935923350043 ) ) ;
#56545 = ORIENTED_EDGE ( 'NONE', *, *, #20171, .F. ) ;
#56546 = VERTEX_POINT ( 'NONE', #52497 ) ;
#56547 = CARTESIAN_POINT ( 'NONE',  ( -10.43328091272586455, 1423.403754337453620, 137.2810607916168522 ) ) ;
#56548 = CARTESIAN_POINT ( 'NONE',  ( -23.34267830565680057, 1409.843235500860146, 209.1109834998750046 ) ) ;
#56549 = EDGE_LOOP ( 'NONE', ( #35762, #1151, #77879, #13361 ) ) ;
#56550 = CARTESIAN_POINT ( 'NONE',  ( 3.958644637644479491, 1508.551704408389924, 204.1347649932010029 ) ) ;
#56551 = CARTESIAN_POINT ( 'NONE',  ( -9.126915939008458878, 1516.551188146008599, 204.3103848001327663 ) ) ;
#56552 = CARTESIAN_POINT ( 'NONE',  ( -21.65994954781430337, 1436.484406330281899, 143.5049664100171185 ) ) ;
#56554 = AXIS2_PLACEMENT_3D ( 'NONE', #89053, #21266, #105874 ) ;
#56553 = CARTESIAN_POINT ( 'NONE',  ( 5.430576746648560160, 1440.816380464289978, 154.8042786433940137 ) ) ;
#56555 = ORIENTED_EDGE ( 'NONE', *, *, #51379, .T. ) ;
#56556 = CARTESIAN_POINT ( 'NONE',  ( 45.02435768011299899, 1448.514094220139896, 266.7106273715389761 ) ) ;
#56557 = CARTESIAN_POINT ( 'NONE',  ( -3.801724410738229754, 1509.034524880150002, 204.6344874940000125 ) ) ;
#56558 = CARTESIAN_POINT ( 'NONE',  ( -0.1387231356229999824, 1418.535612649829773, 184.6749245791980059 ) ) ;
#56559 = CARTESIAN_POINT ( 'NONE',  ( -0.01322039564809850132, 1516.939819969850078, 205.0847949345169923 ) ) ;
#56560 = VERTEX_POINT ( 'NONE', #35675 ) ;
#56561 = CARTESIAN_POINT ( 'NONE',  ( 8.026143276357348810, 1482.798742743219918, 217.8006291142289967 ) ) ;
#56562 = CARTESIAN_POINT ( 'NONE',  ( 13.47253432440122367, 1443.597697226354512, 187.9990502360145683 ) ) ;
#56563 = ORIENTED_EDGE ( 'NONE', *, *, #104723, .T. ) ;
#56564 = ORIENTED_EDGE ( 'NONE', *, *, #85787, .T. ) ;
#56565 = CARTESIAN_POINT ( 'NONE',  ( -10.53746316515110060, 1480.488129968620115, 209.0885347073749756 ) ) ;
#56566 = PLANE ( 'NONE',  #59171 ) ;
#56567 = CARTESIAN_POINT ( 'NONE',  ( -4.491579513878525276, 1425.338252514831993, 186.1547051059805540 ) ) ;
#56568 = CARTESIAN_POINT ( 'NONE',  ( 6.210571358314980195, 1452.696182456529868, 151.8216972714639894 ) ) ;
#56569 = CARTESIAN_POINT ( 'NONE',  ( 0.4691007450668729928, 1410.389848773719905, 269.3346290167360166 ) ) ;
#56570 = CARTESIAN_POINT ( 'NONE',  ( 19.32263322520000060, 1455.378559704889767, 209.1218459616989946 ) ) ;
#56571 = CARTESIAN_POINT ( 'NONE',  ( -109.0845216409653489, 1382.044982048102383, 297.5749921241352922 ) ) ;
#56572 = DIRECTION ( 'NONE',  ( 5.980589973904019347E-17, -1.000000000000000000, 1.736889445713099699E-16 ) ) ;
#56573 = FACE_OUTER_BOUND ( 'NONE', #81529, .T. ) ;
#56575 = DIRECTION ( 'NONE',  ( -1.000000000000000000, 0.000000000000000000, 0.000000000000000000 ) ) ;
#56574 = CARTESIAN_POINT ( 'NONE',  ( -13.56684817831589918, 1434.956907115119748, 148.7388511781440172 ) ) ;
#56576 = CARTESIAN_POINT ( 'NONE',  ( 10.98521726274509902, 1425.641609558600067, 206.4994411935269909 ) ) ;
#56577 = CARTESIAN_POINT ( 'NONE',  ( -9.801729170509650757, 1440.029616514400004, 207.0728283516110082 ) ) ;
#56578 = CARTESIAN_POINT ( 'NONE',  ( 7.320561577120000329, 1432.353341358199941, 149.5448088695980005 ) ) ;
#56579 = ORIENTED_EDGE ( 'NONE', *, *, #45387, .T. ) ;
#56580 = CARTESIAN_POINT ( 'NONE',  ( 18.41412373400000035, 1436.828957585569924, 209.1218459616979999 ) ) ;
#56581 = CARTESIAN_POINT ( 'NONE',  ( -11.73652925619994569, 1426.280330920429833, 144.1708004945943173 ) ) ;
#56582 = CARTESIAN_POINT ( 'NONE',  ( -91.62647196664750027, 1384.965762749710166, 309.2156490120800072 ) ) ;
#56583 = CARTESIAN_POINT ( 'NONE',  ( -9.503490513250000049, 1386.215136675220037, 200.2136258941289952 ) ) ;
#56584 =( BOUNDED_CURVE ( )  B_SPLINE_CURVE ( 5, ( #109191, #8907, #43084, #18399, #33005, #94019 ),
 .UNSPECIFIED., .F., .F. ) 
 B_SPLINE_CURVE_WITH_KNOTS ( ( 6, 6 ),
 ( 0.000000000000000000, 1.000000000000000000 ),
 .UNSPECIFIED. ) 
 CURVE ( )  GEOMETRIC_REPRESENTATION_ITEM ( )  RATIONAL_B_SPLINE_CURVE ( ( 1.000000000000000000, 0.8718535683296719796, 0.7642340215966414441, 0.6738533009783809202, 0.5979500389088989731, 0.5342895590787407611 ) ) 
 REPRESENTATION_ITEM ( '' )  );
#56585 = CARTESIAN_POINT ( 'NONE',  ( 9.687496139252409932, 1422.985733114659979, 210.5042674169859822 ) ) ;
#56587 = ORIENTED_EDGE ( 'NONE', *, *, #104725, .T. ) ;
#56586 = CARTESIAN_POINT ( 'NONE',  ( -15.84429307296400147, 1419.853224566099925, 210.7451948333090002 ) ) ;
#56588 = CARTESIAN_POINT ( 'NONE',  ( 2.370970874524633398, 1427.002265528473799, 137.0999999980980135 ) ) ;
#56589 = CARTESIAN_POINT ( 'NONE',  ( -2.953748537521290185, 1440.359176245339995, 157.3263145227589916 ) ) ;
#56590 = CARTESIAN_POINT ( 'NONE',  ( -14.20165763179999807, 1416.819759806430056, 221.7375114452979972 ) ) ;
#56592 = EDGE_CURVE ( 'NONE', #4376, #43234, #106087, .T. ) ;
#56591 = DIRECTION ( 'NONE',  ( -1.755985294532469921E-16, 1.000000000000000000, -1.338183447452831989E-16 ) ) ;
#56593 = DIRECTION ( 'NONE',  ( 0.06989148164378741757, -0.9716773222564312196, -0.2257395893639560502 ) ) ;
#56594 = DIRECTION ( 'NONE',  ( -0.4978433412588795792, 0.000000000000000000, -0.8672669759446596238 ) ) ;
#56595 = CARTESIAN_POINT ( 'NONE',  ( 1.676153920926429786, 1456.565163720139935, 199.0597771984899964 ) ) ;
#56596 = CARTESIAN_POINT ( 'NONE',  ( -107.6011828208343672, 1389.768012669342397, 298.8907520829743021 ) ) ;
#56597 = DIRECTION ( 'NONE',  ( -9.056288633775531119E-47, 1.000000000000000000, -1.836970198721029688E-16 ) ) ;
#56598 = CARTESIAN_POINT ( 'NONE',  ( -21.41758936356487908, 1524.330813522192102, 234.0369194964266626 ) ) ;
#56599 = CARTESIAN_POINT ( 'NONE',  ( 2.051922892142530319, 1474.778080336890071, 220.3551958197380145 ) ) ;
#56600 = CARTESIAN_POINT ( 'NONE',  ( 44.93138466476950299, 1440.913053015859987, 269.6837875441360097 ) ) ;
#56601 = DIRECTION ( 'NONE',  ( 0.000000000000000000, 1.000000000000000000, 0.000000000000000000 ) ) ;
#56602 = CARTESIAN_POINT ( 'NONE',  ( -1.546097701929999957, 1418.675484806429949, 228.1029857612980152 ) ) ;
#56603 = PRODUCT_DEFINITION_FORMATION_WITH_SPECIFIED_SOURCE ( 'ANY', '', #14279, .NOT_KNOWN. ) ;
#56604 = CARTESIAN_POINT ( 'NONE',  ( -3.200208250563545853, 1370.366478648552174, 206.6667948705140532 ) ) ;
#56605 = CARTESIAN_POINT ( 'NONE',  ( 20.69714284706258312, 1525.848196786131666, 184.2818640063567557 ) ) ;
#56606 = EDGE_CURVE ( 'NONE', #38713, #35962, #13620, .T. ) ;
#56607 = CARTESIAN_POINT ( 'NONE',  ( 1.205374332583420191E-06, 1407.922920318890192, 195.8673945273630181 ) ) ;
#56608 = CARTESIAN_POINT ( 'NONE',  ( -14.65960690603279915, 1417.542028598340039, 203.2496943021490097 ) ) ;
#56609 = CARTESIAN_POINT ( 'NONE',  ( -6.587888517611229844, 1432.346495048320094, 154.2385474615439875 ) ) ;
#56610 = CARTESIAN_POINT ( 'NONE',  ( -1.543257077560000079, 1416.522662137829911, 228.0084432390979998 ) ) ;
#56611 = CARTESIAN_POINT ( 'NONE',  ( 0.2117380174047990005, 1456.372610658380154, 183.1087122574759860 ) ) ;
#56612 = CARTESIAN_POINT ( 'NONE',  ( -12.51283845067499989, 1408.316739414530048, 203.8172553575790005 ) ) ;
#56613 = CARTESIAN_POINT ( 'NONE',  ( -16.04707966200000158, 1416.518532928429977, 200.6156669267779762 ) ) ;
#56614 = ADVANCED_FACE ( 'NONE', ( #27276 ), #110811, .T. ) ;
#56615 = CARTESIAN_POINT ( 'NONE',  ( -7.229059265610779939, 1441.096153944170055, 154.2643636803950073 ) ) ;
#56616 = CARTESIAN_POINT ( 'NONE',  ( 11.87965657760000049, 1433.311156085379935, 147.2728768370980106 ) ) ;
#56617 = CARTESIAN_POINT ( 'NONE',  ( -28.12790489320000020, 1436.808336956589756, 136.7412132036979813 ) ) ;
#56618 = CARTESIAN_POINT ( 'NONE',  ( 10.30092211480000053, 1440.660729465949998, 187.2403783651980120 ) ) ;
#56619 = ORIENTED_EDGE ( 'NONE', *, *, #106908, .F. ) ;
#56620 = CARTESIAN_POINT ( 'NONE',  ( -0.6157351208539989518, 1485.064490564490143, 198.2544660199990005 ) ) ;
#56621 = CARTESIAN_POINT ( 'NONE',  ( 5.452465356810000330, 1477.448037175989839, 199.6888371653989793 ) ) ;
#56622 = CARTESIAN_POINT ( 'NONE',  ( -103.9443829322484447, 1380.156439096358099, 306.3198609861664750 ) ) ;
#56623 = CARTESIAN_POINT ( 'NONE',  ( -11.65409527809999979, 1491.241274884490167, 207.0635266648489790 ) ) ;
#56624 = DIRECTION ( 'NONE',  ( -0.000000000000000000, -1.000000000000000000, -0.000000000000000000 ) ) ;
#56625 = CARTESIAN_POINT ( 'NONE',  ( 14.12036593068209989, 1509.406339180530040, 234.8413270297230042 ) ) ;
#56626 = CARTESIAN_POINT ( 'NONE',  ( 2.852619981334113763, 1406.777728849647247, 269.6500679739756947 ) ) ;
#56627 = CARTESIAN_POINT ( 'NONE',  ( -5.080289282479999002, 1480.093209919690253, 228.8812397303989883 ) ) ;
#56628 = CARTESIAN_POINT ( 'NONE',  ( -13.53521852579999951, 1379.959041148089909, 211.1154580547890021 ) ) ;
#56629 = CARTESIAN_POINT ( 'NONE',  ( 2.984390131719999673, 1428.733266614430022, 184.7181844846980141 ) ) ;
#56630 = CARTESIAN_POINT ( 'NONE',  ( -66.14216747191879620, 1385.092570033629954, 257.5864158085420286 ) ) ;
#56631 = FACE_OUTER_BOUND ( 'NONE', #15069, .T. ) ;
#56632 = CARTESIAN_POINT ( 'NONE',  ( -26.81185573016960078, 1435.692944580150424, 136.1507310960283235 ) ) ;
#56633 = CARTESIAN_POINT ( 'NONE',  ( -28.30911832768390113, 1508.554176145409883, 208.8345150349300070 ) ) ;
#56634 = AXIS2_PLACEMENT_3D ( 'NONE', #69484, #77859, #18471 ) ;
#56635 = CARTESIAN_POINT ( 'NONE',  ( -15.97071713983319974, 1409.722728690500162, 226.1176614794329964 ) ) ;
#56637 = EDGE_LOOP ( 'NONE', ( #32016, #36421, #101958, #65221 ) ) ;
#56636 = FACE_OUTER_BOUND ( 'NONE', #36681, .T. ) ;
#56638 = DIRECTION ( 'NONE',  ( 0.4794255386042021172, -2.935634756405659236E-17, -0.8775825618903732028 ) ) ;
#56639 = CARTESIAN_POINT ( 'NONE',  ( 11.16766711165429982, 1471.636180864200014, 211.5731661215769748 ) ) ;
#56640 = EDGE_CURVE ( 'NONE', #21777, #38998, #996, .T. ) ;
#56641 = DIRECTION ( 'NONE',  ( -5.980589973904019347E-17, 1.000000000000000000, -1.736889445713099699E-16 ) ) ;
#56642 = CARTESIAN_POINT ( 'NONE',  ( -109.3106548430000089, 1384.781303703980029, 311.2625950142589772 ) ) ;
#56643 = CARTESIAN_POINT ( 'NONE',  ( -0.1427736395143110182, 1420.459881824180002, 182.9082046469020213 ) ) ;
#56644 = CARTESIAN_POINT ( 'NONE',  ( 1.121350373659999899, 1465.842768926529970, 235.5471876029980081 ) ) ;
#56645 = CARTESIAN_POINT ( 'NONE',  ( 23.01825460670000112, 1410.638272742329946, 213.3724494741479987 ) ) ;
#56646 = DIRECTION ( 'NONE',  ( 0.000000000000000000, 1.000000000000000000, 0.000000000000000000 ) ) ;
#56647 = CARTESIAN_POINT ( 'NONE',  ( -18.28219863529999856, 1466.655046000689936, 217.8387514274990053 ) ) ;
#56648 = CARTESIAN_POINT ( 'NONE',  ( -17.85552477759999945, 1424.537816727530071, 227.5382918161980115 ) ) ;
#56649 = B_SPLINE_CURVE_WITH_KNOTS ( 'NONE', 1,
 ( #6390, #55717 ),
 .UNSPECIFIED., .F., .F.,
 ( 2, 2 ),
 ( -0.4927803034759909440, 3.525362120492052220 ),
 .UNSPECIFIED. ) ;
#56651 = FACE_OUTER_BOUND ( 'NONE', #64412, .T. ) ;
#56650 = CARTESIAN_POINT ( 'NONE',  ( -4.873140598966017478, 1511.395875706939250, 200.6411893189262798 ) ) ;
#56652 = CARTESIAN_POINT ( 'NONE',  ( 20.14625858819999848, 1475.555764171690043, 207.1910292336289672 ) ) ;
#56653 = CARTESIAN_POINT ( 'NONE',  ( -123.6375682760757115, 1340.114449826969576, 286.9633900369482831 ) ) ;
#56654 = CARTESIAN_POINT ( 'NONE',  ( 16.65100080374359237, 1526.335487865669847, 234.8974115816864128 ) ) ;
#56655 = CARTESIAN_POINT ( 'NONE',  ( -18.11269319780000231, 1504.989642490190136, 208.9951304212659977 ) ) ;
#56656 = CARTESIAN_POINT ( 'NONE',  ( -5.187810489148779958, 1375.027207977500211, 203.4482692765930096 ) ) ;
#56657 = CARTESIAN_POINT ( 'NONE',  ( 3.447264348965000558, 1516.858765657450249, 205.6607986404769974 ) ) ;
#56658 = CARTESIAN_POINT ( 'NONE',  ( -17.64330431710000013, 1423.732166419529904, 226.4225726569979997 ) ) ;
#56659 = ORIENTED_EDGE ( 'NONE', *, *, #96826, .F. ) ;
#56660 = DIRECTION ( 'NONE',  ( 0.000000000000000000, 0.8286769424886156754, -0.5597271880011900347 ) ) ;
#56661 = CARTESIAN_POINT ( 'NONE',  ( -4.222911213134699970, 1441.593106041759938, 167.4128785044850076 ) ) ;
#56663 = ORIENTED_EDGE ( 'NONE', *, *, #94287, .F. ) ;
#56662 = CARTESIAN_POINT ( 'NONE',  ( -67.99816612459999021, 1379.747625308320039, 279.4122903082590028 ) ) ;
#56664 = ORIENTED_EDGE ( 'NONE', *, *, #6690, .T. ) ;
#56665 = CARTESIAN_POINT ( 'NONE',  ( -8.813399063861234950, 1381.146817608087304, 217.8464237413924707 ) ) ;
#56666 = VERTEX_POINT ( 'NONE', #36786 ) ;
#56667 = CARTESIAN_POINT ( 'NONE',  ( 8.313287170068500487, 1507.316777277299934, 183.0869016502879845 ) ) ;
#56668 = CARTESIAN_POINT ( 'NONE',  ( 11.15438547699999994, 1501.800732394090119, 206.4593492666689940 ) ) ;
#56670 = CARTESIAN_POINT ( 'NONE',  ( 15.82996380996429941, 1409.474171035389872, 192.7642349844859950 ) ) ;
#56669 = FACE_OUTER_BOUND ( 'NONE', #67597, .T. ) ;
#56671 = CARTESIAN_POINT ( 'NONE',  ( 5.788691325514999875, 1517.157901477309906, 210.2449475486469908 ) ) ;
#56672 = CARTESIAN_POINT ( 'NONE',  ( -26.88456506701299986, 1450.694694235800171, 136.4506520073810236 ) ) ;
#56673 = CARTESIAN_POINT ( 'NONE',  ( -11.43732278620000109, 1425.481241381329937, 144.1613654190979901 ) ) ;
#56674 = CARTESIAN_POINT ( 'NONE',  ( 2.326513286163319538, 1476.258183507229887, 197.8633931498989966 ) ) ;
#56675 = CARTESIAN_POINT ( 'NONE',  ( 16.33500296837753041, 1517.051704408389924, 214.0369884316988305 ) ) ;
#56676 = APPLICATION_PROTOCOL_DEFINITION ( 'draft international standard', 'automotive_design', 1998, #43481 ) ;
#56677 = CARTESIAN_POINT ( 'NONE',  ( 36.91977620337090116, 1451.033275236259897, 134.0999999987079718 ) ) ;
#56678 = ORIENTED_EDGE ( 'NONE', *, *, #82141, .T. ) ;
#56679 = CARTESIAN_POINT ( 'NONE',  ( 16.66442743440000029, 1492.498864364090196, 193.3249227319990098 ) ) ;
#56680 = DIRECTION ( 'NONE',  ( 0.000000000000000000, 1.000000000000000000, 0.000000000000000000 ) ) ;
#56681 = ORIENTED_EDGE ( 'NONE', *, *, #63863, .F. ) ;
#56682 = ORIENTED_EDGE ( 'NONE', *, *, #39094, .T. ) ;
#56683 = CARTESIAN_POINT ( 'NONE',  ( -7.100264625464999924, 1513.939092156100060, 216.8413715654270106 ) ) ;
#56684 = CARTESIAN_POINT ( 'NONE',  ( 31.34491295179421400, 1525.848198008145346, 217.0523385987458482 ) ) ;
#56685 = CARTESIAN_POINT ( 'NONE',  ( 0.05562598889329999768, 1452.349460780129903, 183.2669973655980016 ) ) ;
#56686 = CARTESIAN_POINT ( 'NONE',  ( -3.176595525550000243, 1485.137864157130025, 183.1894384333979815 ) ) ;
#56687 = CARTESIAN_POINT ( 'NONE',  ( -2.500000000000000000, 1439.396215995059947, 161.7067243754309800 ) ) ;
#56688 = CIRCLE ( 'NONE', #35173, 11.73448142120001059 ) ;
#56689 = CARTESIAN_POINT ( 'NONE',  ( -2.470168521978409970, 1523.382868172864164, 242.8787258963054398 ) ) ;
#56690 = CARTESIAN_POINT ( 'NONE',  ( -66.04910042496936740, 1379.741981372295641, 274.4777133012353261 ) ) ;
#56691 = CARTESIAN_POINT ( 'NONE',  ( -3.088273073808346147, 1369.577046551927879, 210.5855487400704078 ) ) ;
#56692 = CARTESIAN_POINT ( 'NONE',  ( 7.509485228916700454E-15, 1517.551704408389924, 209.1218459616989946 ) ) ;
#56693 = CARTESIAN_POINT ( 'NONE',  ( 22.12673984907599944, 1409.685743169220132, 208.3470065775269973 ) ) ;
#56694 = CARTESIAN_POINT ( 'NONE',  ( -79.38279021894339849, 1384.791171274589942, 282.2745212356039701 ) ) ;
#56695 = VERTEX_POINT ( 'NONE', #70979 ) ;
#56696 = CARTESIAN_POINT ( 'NONE',  ( 9.664422427686080397, 1462.605350418599983, 207.8072316276789877 ) ) ;
#56697 = CARTESIAN_POINT ( 'NONE',  ( 1.701850457105000158, 1516.908147884120126, 207.9845492812970065 ) ) ;
#56698 = ORIENTED_EDGE ( 'NONE', *, *, #31621, .F. ) ;
#56699 = CARTESIAN_POINT ( 'NONE',  ( 36.38905843718290356, 1440.913060387330006, 262.8310855799430215 ) ) ;
#56700 = CARTESIAN_POINT ( 'NONE',  ( -0.0002653596066196077410, 1452.517597898977101, 153.5752998968471275 ) ) ;
#56701 = EDGE_LOOP ( 'NONE', ( #107384, #91364 ) ) ;
#56702 = CARTESIAN_POINT ( 'NONE',  ( -0.1174241404373970038, 1452.347189664339794, 183.2668478624919999 ) ) ;
#56703 = CARTESIAN_POINT ( 'NONE',  ( -16.57642552269999925, 1409.993768750830213, 191.9233248414979869 ) ) ;
#56704 = CARTESIAN_POINT ( 'NONE',  ( 4.602958218326069779E-16, 1426.918876943007945, 134.0999999980979851 ) ) ;
#56705 = CARTESIAN_POINT ( 'NONE',  ( -9.403517712975409282, 1461.589092010630111, 206.6946280230779962 ) ) ;
#56706 = B_SPLINE_CURVE_WITH_KNOTS ( 'NONE', 5,
 ( #48702, #20859, #40827, #56544, #75005, #90672, #6118, #66062, #13956, #99613, #48145, #109155 ),
 .UNSPECIFIED., .F., .F.,
 ( 6, 3, 3, 6 ),
 ( -7.762943620309999737, -7.625232449769999477, -3.361916338479999489, -3.182123501529999565 ),
 .UNSPECIFIED. ) ;
#56707 = CARTESIAN_POINT ( 'NONE',  ( -13.25186809610000083, 1419.889586077830018, 222.0034080458980270 ) ) ;
#56708 = CARTESIAN_POINT ( 'NONE',  ( 16.50400130224750583, 1525.907212628473644, 181.9890130758377040 ) ) ;
#56709 = CARTESIAN_POINT ( 'NONE',  ( -1.436086187699999961, 1508.900106475729899, 179.8313947826979984 ) ) ;
#56710 = CARTESIAN_POINT ( 'NONE',  ( -13.80580293259999891, 1434.979613021240084, 147.1507279520979807 ) ) ;
#56711 = CARTESIAN_POINT ( 'NONE',  ( -20.98221433428875216, 1524.841055067848174, 181.0917269138568884 ) ) ;
#56713 = CARTESIAN_POINT ( 'NONE',  ( -11.60004869885203682, 1424.622146315513419, 136.2523473544339083 ) ) ;
#56712 = CARTESIAN_POINT ( 'NONE',  ( 13.80393196719999871, 1462.044328216929898, 230.7224726401980206 ) ) ;
#56714 = FACE_OUTER_BOUND ( 'NONE', #92580, .T. ) ;
#56715 = TOROIDAL_SURFACE ( 'NONE', #35273, 1.000000000000000000, 1.000000000000000000 ) ;
#56716 = CARTESIAN_POINT ( 'NONE',  ( -2.872836660654999985, 1517.158319634930194, 216.8472181024670249 ) ) ;
#56717 = ORIENTED_EDGE ( 'NONE', *, *, #28161, .T. ) ;
#56718 = CARTESIAN_POINT ( 'NONE',  ( -0.3657342159832346895, 1486.413194173067495, 181.7790224318463856 ) ) ;
#56719 = CARTESIAN_POINT ( 'NONE',  ( -10.01326586723869916, 1481.014341800280135, 205.7823588363200145 ) ) ;
#56720 = CARTESIAN_POINT ( 'NONE',  ( 4.311024656403059652, 1407.085546270103578, 221.5801435630039009 ) ) ;
#56721 = CARTESIAN_POINT ( 'NONE',  ( 6.561686423234999843, 1517.069378699710114, 212.5741351528070027 ) ) ;
#56722 = FACE_OUTER_BOUND ( 'NONE', #78737, .T. ) ;
#56723 = CARTESIAN_POINT ( 'NONE',  ( -1.637258856660000150, 1483.893433971690001, 198.5669146070989939 ) ) ;
#56725 = ORIENTED_EDGE ( 'NONE', *, *, #39266, .F. ) ;
#56724 = CARTESIAN_POINT ( 'NONE',  ( 3.487587010931929576, 1508.884219112060009, 213.6131341179649894 ) ) ;
#56726 = DIRECTION ( 'NONE',  ( -0.1402804634180424004, -0.9901118076173111016, 0.000000000000000000 ) ) ;
#56727 = CARTESIAN_POINT ( 'NONE',  ( 1.871813672400000073, 1508.233053297490187, 220.5554446848989869 ) ) ;
#56728 = CARTESIAN_POINT ( 'NONE',  ( -11.55098531880000046, 1430.396653715230059, 150.9171824720979771 ) ) ;
#56729 = DIRECTION ( 'NONE',  ( -0.6736849260863841948, 0.000000000000000000, 0.7390186874254148774 ) ) ;
#56730 = CARTESIAN_POINT ( 'NONE',  ( -109.6762529225470075, 1383.331248784420040, 311.2558314816980101 ) ) ;
#56731 = CARTESIAN_POINT ( 'NONE',  ( -3.774750576832590096E-15, 1432.353310171170051, 155.3998098058200128 ) ) ;
#56732 = DIRECTION ( 'NONE',  ( 1.755985294532464991E-16, -1.000000000000000000, 1.338183447452830017E-16 ) ) ;
#56733 = CARTESIAN_POINT ( 'NONE',  ( 12.54302623819999951, 1445.073512831690095, 186.6024346732980064 ) ) ;
#56734 = B_SPLINE_CURVE_WITH_KNOTS ( 'NONE', 3,
 ( #72743, #11191, #63802, #80587, #12264, #97918 ),
 .UNSPECIFIED., .F., .F.,
 ( 4, 2, 4 ),
 ( 0.000000000000000000, 0.5000000000000000000, 1.000000000000000000 ),
 .UNSPECIFIED. ) ;
#56736 = CARTESIAN_POINT ( 'NONE',  ( -11.12625634799329966, 1482.488446798920222, 206.3854409893099842 ) ) ;
#56735 = CARTESIAN_POINT ( 'NONE',  ( -23.70830759550000266, 1457.436638280929856, 216.7744869258079916 ) ) ;
#56738 = FACE_OUTER_BOUND ( 'NONE', #34922, .T. ) ;
#56737 = AXIS2_PLACEMENT_3D ( 'NONE', #70527, #79997, #43642 ) ;
#56739 = VERTEX_POINT ( 'NONE', #45208 ) ;
#56740 = CARTESIAN_POINT ( 'NONE',  ( -5.009478105444999940, 1516.886345593249871, 204.5093386581970094 ) ) ;
#56741 = CARTESIAN_POINT ( 'NONE',  ( 3.776163893200000121, 1405.832946398430067, 267.8478556236980239 ) ) ;
#56742 = CARTESIAN_POINT ( 'NONE',  ( 0.1886752042949999819, 1409.088270638030053, 185.5766010327979814 ) ) ;
#56743 = CARTESIAN_POINT ( 'NONE',  ( 18.18607966929999975, 1410.878986942329902, 193.7902918041979774 ) ) ;
#56744 = EDGE_CURVE ( 'NONE', #36172, #101207, #39278, .T. ) ;
#56745 = CARTESIAN_POINT ( 'NONE',  ( 23.62496399655424284, 1434.148717771737438, 214.7198664209217611 ) ) ;
#56746 = CARTESIAN_POINT ( 'NONE',  ( 8.991744574390811096, 1509.227061438039982, 181.2342617849590169 ) ) ;
#56747 = CARTESIAN_POINT ( 'NONE',  ( 27.12603011487975380, 1508.017486813007508, 214.4686767731490988 ) ) ;
#56748 = B_SPLINE_CURVE_WITH_KNOTS ( 'NONE', 3,
 ( #99179, #22459, #82411, #39850, #67820, #68378, #51008, #51558, #85141, #52119, #8429, #52669 ),
 .UNSPECIFIED., .F., .F.,
 ( 4, 2, 2, 2, 2, 4 ),
 ( 0.000000000000000000, 0.0007194225121792416702, 0.001079133768269177141, 0.001438845024359112828, 0.002158267536538995262, 0.002877690048718877912 ),
 .UNSPECIFIED. ) ;
#56749 = CARTESIAN_POINT ( 'NONE',  ( -6.588623528374058402, 1439.966844091445864, 203.3438421578153168 ) ) ;
#56750 = CARTESIAN_POINT ( 'NONE',  ( -2.310870060038839657, 1449.824111060830091, 154.7919463925260004 ) ) ;
#56751 = CARTESIAN_POINT ( 'NONE',  ( -1.595915170252538928, 1451.462758934706926, 183.9376596482218815 ) ) ;
#56752 = EDGE_CURVE ( 'NONE', #40624, #98891, #30321, .T. ) ;
#56753 = DIRECTION ( 'NONE',  ( 0.000000000000000000, 1.000000000000000000, 0.000000000000000000 ) ) ;
#56754 = DIRECTION ( 'NONE',  ( -0.6736849260149578855, 0.000000000000000000, 0.7390186874905266823 ) ) ;
#56755 = CARTESIAN_POINT ( 'NONE',  ( -3.829620175029999629, 1515.551704176389876, 210.9648099296190082 ) ) ;
#56756 = CARTESIAN_POINT ( 'NONE',  ( -7.417345643215089268, 1409.172079804809982, 196.1196827968989851 ) ) ;
#56757 = CIRCLE ( 'NONE', #65712, 1.638701816490922836 ) ;
#56758 = CARTESIAN_POINT ( 'NONE',  ( -27.19943328049049924, 1507.991540615329995, 211.1058746345759971 ) ) ;
#56759 = CARTESIAN_POINT ( 'NONE',  ( 2.500000004939999965, 1439.742886558890177, 158.2293697702980069 ) ) ;
#56760 = CARTESIAN_POINT ( 'NONE',  ( -3.426102627740000184, 1475.665556257130220, 269.0410120623980106 ) ) ;
#56761 = CARTESIAN_POINT ( 'NONE',  ( -105.4624709189999834, 1391.255327103129957, 304.2078109453590287 ) ) ;
#56762 = DIRECTION ( 'NONE',  ( -0.000000000000000000, -1.000000000000000000, -0.000000000000000000 ) ) ;
#56763 = CARTESIAN_POINT ( 'NONE',  ( 1.336192060408132321, 1526.382868172863937, 239.5677422944788475 ) ) ;
#56764 = CARTESIAN_POINT ( 'NONE',  ( -23.61108870869020393, 1384.850736334059775, 222.7912172758710199 ) ) ;
#56765 = CARTESIAN_POINT ( 'NONE',  ( -30.17514222261029744, 1525.712835404586031, 221.2664189270033432 ) ) ;
#56766 = VECTOR ( 'NONE', #99570, 1000.000000000000114 ) ;
#56767 = CARTESIAN_POINT ( 'NONE',  ( 2.487935142314050108, 1509.038615934839981, 213.6090957367470082 ) ) ;
#56768 = CARTESIAN_POINT ( 'NONE',  ( -105.9362968920000014, 1378.913060259759959, 302.4576468725590530 ) ) ;
#56769 = CARTESIAN_POINT ( 'NONE',  ( 31.79805362023550330, 1525.506926151470907, 217.0230659451404733 ) ) ;
#56770 = CARTESIAN_POINT ( 'NONE',  ( 8.100258108500456800, 1511.553933485576636, 205.4225227818773476 ) ) ;
#56771 = CARTESIAN_POINT ( 'NONE',  ( -21.62801678940000016, 1409.668327376230081, 205.1400470743279811 ) ) ;
#56772 = CARTESIAN_POINT ( 'NONE',  ( 12.65229159338619880, 1421.485625842520221, 206.6964318454880072 ) ) ;
#56773 = CARTESIAN_POINT ( 'NONE',  ( 19.56843215269274339, 1455.495710568705817, 225.8468362473698505 ) ) ;
#56774 = ORIENTED_EDGE ( 'NONE', *, *, #62048, .T. ) ;
#56775 = CARTESIAN_POINT ( 'NONE',  ( -3.500000000000000000, 1420.857604035629947, 170.3256330572980062 ) ) ;
#56776 = CARTESIAN_POINT ( 'NONE',  ( -7.428892777654675150, 1510.947107019768737, 215.4107650370616795 ) ) ;
#56777 = CARTESIAN_POINT ( 'NONE',  ( -17.51440058699769864, 1442.103999578969933, 219.2287822569540197 ) ) ;
#56779 = CARTESIAN_POINT ( 'NONE',  ( -14.08099615227689938, 1379.586030346570169, 211.7531778911580034 ) ) ;
#56778 = CARTESIAN_POINT ( 'NONE',  ( 11.73643847070000135, 1426.280399246029901, 144.1643001595979854 ) ) ;
#56780 = CARTESIAN_POINT ( 'NONE',  ( 16.66231036550726685, 1523.604703353109699, 237.7554842931445478 ) ) ;
#56781 = CARTESIAN_POINT ( 'NONE',  ( -3.827327205999999649, 1424.046157813729906, 172.2701767054979882 ) ) ;
#56782 = CARTESIAN_POINT ( 'NONE',  ( -4.668925449930000582, 1453.940455793189813, 200.5491111697690201 ) ) ;
#56783 = CARTESIAN_POINT ( 'NONE',  ( -4.618119704395000191, 1516.706638732659940, 202.1845071865270143 ) ) ;
#56784 = CARTESIAN_POINT ( 'NONE',  ( 7.589021600739999762, 1426.918624641610222, 212.4071224751090199 ) ) ;
#56786 = CARTESIAN_POINT ( 'NONE',  ( -11.91590827042684886, 1398.266372442801185, 203.9246104138306350 ) ) ;
#56785 = VECTOR ( 'NONE', #74109, 1000.000000000000227 ) ;
#56787 = CARTESIAN_POINT ( 'NONE',  ( 15.56957301243500069, 1512.571022561229938, 195.5563796964669905 ) ) ;
#56788 = FACE_BOUND ( 'NONE', #13584, .T. ) ;
#56789 = CARTESIAN_POINT ( 'NONE',  ( -7.513427089629229449, 1380.366186910970100, 210.0680633349269897 ) ) ;
#56790 = CARTESIAN_POINT ( 'NONE',  ( 8.040263484913412029, 1366.379670611970141, 207.6218459616988241 ) ) ;
#56792 = EDGE_LOOP ( 'NONE', ( #100280, #65597, #9507, #28240, #56395, #90132, #12443, #7105, #24380 ) ) ;
#56791 = CARTESIAN_POINT ( 'NONE',  ( -19.23044006891440105, 1379.597748850580047, 212.7363834275300007 ) ) ;
#56793 = ORIENTED_EDGE ( 'NONE', *, *, #49993, .T. ) ;
#56794 = CARTESIAN_POINT ( 'NONE',  ( -12.78033923309999942, 1396.878026447830052, 207.4324367705480086 ) ) ;
#56795 = CARTESIAN_POINT ( 'NONE',  ( -20.84521127210000202, 1410.135590990030096, 218.2730277501279943 ) ) ;
#56796 = CARTESIAN_POINT ( 'NONE',  ( -1.249587849150000096, 1415.128105756529976, 226.9283669200980000 ) ) ;
#56797 = CARTESIAN_POINT ( 'NONE',  ( -12.80792181777679239, 1444.977435535784252, 169.4484251894283489 ) ) ;
#56798 = CARTESIAN_POINT ( 'NONE',  ( -24.66760647159999920, 1507.924356353729991, 197.5571972356979984 ) ) ;
#56799 = CARTESIAN_POINT ( 'NONE',  ( -7.594504679555000415, 1512.160709093490141, 211.5076181542869733 ) ) ;
#56801 = CARTESIAN_POINT ( 'NONE',  ( -21.53022416006009720, 1505.950189135809978, 209.2005961044559967 ) ) ;
#56800 = CARTESIAN_POINT ( 'NONE',  ( 2.737982081959999814, 1444.818524895790006, 200.5605189733490192 ) ) ;
#56802 = CARTESIAN_POINT ( 'NONE',  ( 2.254275791129999984, 1429.771643255829986, 184.6574991238979919 ) ) ;
#56803 = FACE_OUTER_BOUND ( 'NONE', #25203, .T. ) ;
#56804 = DIRECTION ( 'NONE',  ( 0.000000000000000000, 1.000000000000000000, 0.000000000000000000 ) ) ;
#56805 = CARTESIAN_POINT ( 'NONE',  ( 10.74800670940959968, 1396.288389052329876, 211.7634410043349931 ) ) ;
#56806 = CARTESIAN_POINT ( 'NONE',  ( 14.44521984438589968, 1416.640375558050209, 196.8647061789440045 ) ) ;
#56807 = CARTESIAN_POINT ( 'NONE',  ( 11.73918745480000148, 1430.041041296030016, 150.4070077459980155 ) ) ;
#56808 = CARTESIAN_POINT ( 'NONE',  ( 8.778933807423072722, 1427.705008372408884, 144.1938086916980524 ) ) ;
#56809 = ORIENTED_EDGE ( 'NONE', *, *, #19177, .F. ) ;
#56810 = CYLINDRICAL_SURFACE ( 'NONE', #33948, 1.999999999999995559 ) ;
#56811 = CARTESIAN_POINT ( 'NONE',  ( -22.75273496409615603, 1518.913060387330006, 183.6728937936775310 ) ) ;
#56812 = VERTEX_POINT ( 'NONE', #27835 ) ;
#56813 = EDGE_LOOP ( 'NONE', ( #102002, #103346, #70912, #63141 ) ) ;
#56814 = FACE_OUTER_BOUND ( 'NONE', #99316, .T. ) ;
#56815 = CARTESIAN_POINT ( 'NONE',  ( -14.41342808100000106, 1461.324647189130246, 229.5770031318979818 ) ) ;
#56816 = AXIS2_PLACEMENT_3D ( 'NONE', #47387, #5372, #105646 ) ;
#56817 = CARTESIAN_POINT ( 'NONE',  ( -108.5763715352423162, 1388.342241357154990, 310.4916696162636640 ) ) ;
#56818 = B_SPLINE_CURVE_WITH_KNOTS ( 'NONE', 3,
 ( #58918, #83543, #24179, #17420 ),
 .UNSPECIFIED., .F., .F.,
 ( 4, 4 ),
 ( -0.5072555466292649751, -1.464889561797466655E-05 ),
 .UNSPECIFIED. ) ;
#56819 = CARTESIAN_POINT ( 'NONE',  ( -33.28034951413935971, 1512.187213306747481, 200.8029765415142549 ) ) ;
#56820 = CARTESIAN_POINT ( 'NONE',  ( -2.290256301855000398, 1517.170721208160103, 216.0730210990169837 ) ) ;
#56821 = CARTESIAN_POINT ( 'NONE',  ( -13.15130281770530019, 1380.001591251920217, 209.0581075734310161 ) ) ;
#56822 = ORIENTED_EDGE ( 'NONE', *, *, #46251, .F. ) ;
#56823 = CARTESIAN_POINT ( 'NONE',  ( -12.78494549719999895, 1502.727917388590186, 208.9468085136539912 ) ) ;
#56824 = CARTESIAN_POINT ( 'NONE',  ( -5.967056112589649075, 1509.202713547270150, 179.6294632429990088 ) ) ;
#56825 = CARTESIAN_POINT ( 'NONE',  ( -44.32302097390000029, 1375.083786706710043, 232.1686497034590104 ) ) ;
#56826 = EDGE_CURVE ( 'NONE', #26117, #61054, #15232, .T. ) ;
#56827 = EDGE_CURVE ( 'NONE', #18900, #32788, #79526, .T. ) ;
#56828 = CARTESIAN_POINT ( 'NONE',  ( 1.702754371344999962, 1517.014196759610059, 205.6580786742169948 ) ) ;
#56829 = ORIENTED_EDGE ( 'NONE', *, *, #40810, .T. ) ;
#56830 = CARTESIAN_POINT ( 'NONE',  ( -2.480427292634999947, 1516.872851364150165, 209.8797317620669673 ) ) ;
#56831 = CARTESIAN_POINT ( 'NONE',  ( -20.81915287150000182, 1509.403205472729951, 229.3701441624979793 ) ) ;
#56832 = EDGE_CURVE ( 'NONE', #61362, #41878, #27345, .T. ) ;
#56834 = EDGE_CURVE ( 'NONE', #39961, #54634, #81944, .T. ) ;
#56833 = CARTESIAN_POINT ( 'NONE',  ( -37.04769550936495648, 1426.517324163738976, 269.5612620262075438 ) ) ;
#56835 = CARTESIAN_POINT ( 'NONE',  ( -2.295852000570000495, 1409.930597616830028, 232.7102332357979719 ) ) ;
#56837 = ORIENTED_EDGE ( 'NONE', *, *, #37742, .T. ) ;
#56836 = CARTESIAN_POINT ( 'NONE',  ( -30.87183381296014062, 1524.816846803860926, 196.4948539558456844 ) ) ;
#56838 = CARTESIAN_POINT ( 'NONE',  ( -0.01061436087871939909, 1451.719132097020065, 182.8647455669690203 ) ) ;
#56839 = CARTESIAN_POINT ( 'NONE',  ( -33.56105288671160025, 1440.913060389879774, 247.8846291584730182 ) ) ;
#56841 = CARTESIAN_POINT ( 'NONE',  ( -32.10112702670000573, 1384.491500786489951, 229.9526432747589979 ) ) ;
#56840 = AXIS2_PLACEMENT_3D ( 'NONE', #2387, #43804, #105929 ) ;
#56842 = CARTESIAN_POINT ( 'NONE',  ( -0.1401266656683599898, 1467.139399683509737, 235.6380456311810008 ) ) ;
#56843 = CARTESIAN_POINT ( 'NONE',  ( 5.184301943030460436, 1410.264407675250141, 269.8675697800640023 ) ) ;
#56844 = CARTESIAN_POINT ( 'NONE',  ( 3.265407117845000151, 1516.754149861460064, 213.7315192116670062 ) ) ;
#56845 = AXIS2_PLACEMENT_3D ( 'NONE', #33782, #25369, #36013 ) ;
#56846 = CARTESIAN_POINT ( 'NONE',  ( 24.11881256550000074, 1411.115306210429708, 209.4847445257949801 ) ) ;
#56847 = CARTESIAN_POINT ( 'NONE',  ( -20.42683341999999769, 1508.879048844430145, 189.1348644687979856 ) ) ;
#56848 = CARTESIAN_POINT ( 'NONE',  ( 12.32325568688510131, 1492.223109645010027, 209.7154455344569897 ) ) ;
#56849 = CARTESIAN_POINT ( 'NONE',  ( -11.60004869885203505, 1424.622146314968859, 136.2523473539528140 ) ) ;
#56850 = CARTESIAN_POINT ( 'NONE',  ( -7.708745685915000756, 1516.523379810429788, 210.8299382363969983 ) ) ;
#56851 = CARTESIAN_POINT ( 'NONE',  ( 4.192373415348820131, 1421.117595978020063, 185.3194811860539915 ) ) ;
#56853 = EDGE_CURVE ( 'NONE', #8029, #57810, #23164, .T. ) ;
#56852 = CARTESIAN_POINT ( 'NONE',  ( -109.8896697524407671, 1305.913060387289988, 306.1395481116745145 ) ) ;
#56854 = CARTESIAN_POINT ( 'NONE',  ( 3.187570095870436937, 1421.874552375644726, 137.0999999983294799 ) ) ;
#56856 = ORIENTED_EDGE ( 'NONE', *, *, #9110, .T. ) ;
#56855 = CARTESIAN_POINT ( 'NONE',  ( -36.25711517340000256, 1386.837822767809939, 235.3814274622590119 ) ) ;
#56857 = CARTESIAN_POINT ( 'NONE',  ( -43.39262373593199840, 1385.162178046419967, 248.3670905914219986 ) ) ;
#56858 = CARTESIAN_POINT ( 'NONE',  ( 16.66094735743510213, 1410.867388111209948, 226.5061907891179942 ) ) ;
#56859 = DIRECTION ( 'NONE',  ( 0.7384854939282339270, -4.299975059343909233E-13, -0.6742693640212139572 ) ) ;
#56860 = EDGE_CURVE ( 'NONE', #93599, #57270, #106296, .T. ) ;
#56861 = CARTESIAN_POINT ( 'NONE',  ( 0.7236364578855678520, 1494.203192619447236, 220.2307484109624909 ) ) ;
#56862 = CARTESIAN_POINT ( 'NONE',  ( -5.387550183790000169, 1432.551483143010046, 154.6121797508980080 ) ) ;
#56863 = CARTESIAN_POINT ( 'NONE',  ( 11.15048149399999922, 1425.206633195839913, 203.7517032637389889 ) ) ;
#56864 = CARTESIAN_POINT ( 'NONE',  ( -19.37374569213963582, 1526.382868172863937, 183.8768763279542213 ) ) ;
#56866 = CARTESIAN_POINT ( 'NONE',  ( -8.861964488639999971, 1384.888492400790028, 218.6850885747989821 ) ) ;
#56865 = CARTESIAN_POINT ( 'NONE',  ( 7.329925222404999552, 1516.833976295079992, 216.8387248732070134 ) ) ;
#56867 = CARTESIAN_POINT ( 'NONE',  ( -21.13431252044160047, 1409.651086843229905, 211.8287216663260040 ) ) ;
#56868 = CARTESIAN_POINT ( 'NONE',  ( -1.249673188667893342, 1515.565594798684742, 205.1760501711441691 ) ) ;
#56869 = AXIS2_PLACEMENT_3D ( 'NONE', #103556, #53756, #68892 ) ;
#56870 = EDGE_LOOP ( 'NONE', ( #87828, #96666, #9519, #75278 ) ) ;
#56871 = CARTESIAN_POINT ( 'NONE',  ( 4.034908559714999399, 1517.068717944079935, 201.7859449365070077 ) ) ;
#56872 = CARTESIAN_POINT ( 'NONE',  ( 10.33096665759340027, 1480.828053585820044, 206.9964859125329895 ) ) ;
#56873 = ORIENTED_EDGE ( 'NONE', *, *, #6407, .F. ) ;
#56874 = CARTESIAN_POINT ( 'NONE',  ( -0.1685274451060000123, 1477.411888517829993, 230.0191311744979998 ) ) ;
#56875 = CARTESIAN_POINT ( 'NONE',  ( 23.84753075949999968, 1447.297452739720029, 215.9843744054980164 ) ) ;
#56876 = CARTESIAN_POINT ( 'NONE',  ( 10.78336580500200093, 1461.892577084380036, 211.1578546862259884 ) ) ;
#56877 = CARTESIAN_POINT ( 'NONE',  ( 9.412160733855756689, 1425.314313998383568, 195.5625766667135395 ) ) ;
#56878 = CARTESIAN_POINT ( 'NONE',  ( 0.7253268807889989844, 1442.591808607289977, 218.6790638971189935 ) ) ;
#56879 = CARTESIAN_POINT ( 'NONE',  ( 10.69985963648862004, 1418.135228670047809, 229.9018306247701275 ) ) ;
#56880 = CARTESIAN_POINT ( 'NONE',  ( 10.99882366966150116, 1470.803487868729917, 192.2106042945659965 ) ) ;
#56881 = CARTESIAN_POINT ( 'NONE',  ( -19.05061113289999852, 1426.018939432130082, 224.9263685105979960 ) ) ;
#56882 = CARTESIAN_POINT ( 'NONE',  ( 6.857062643409833846, 1486.827203759812164, 200.7504989922479979 ) ) ;
#56883 = CARTESIAN_POINT ( 'NONE',  ( -104.1870796810000002, 1390.019597513000008, 303.0474178122589706 ) ) ;
#56884 = EDGE_CURVE ( 'NONE', #86968, #53118, #83058, .T. ) ;
#56885 = CARTESIAN_POINT ( 'NONE',  ( 17.18006689280000288, 1461.960330296729808, 189.9390536651980028 ) ) ;
#56886 = CARTESIAN_POINT ( 'NONE',  ( -105.5460821599999974, 1391.484866075830041, 304.2071864700590140 ) ) ;
#56887 = CARTESIAN_POINT ( 'NONE',  ( -34.42417634216256772, 1458.387040857726333, 269.5237062428848844 ) ) ;
#56888 = ORIENTED_EDGE ( 'NONE', *, *, #51811, .T. ) ;
#56889 = CARTESIAN_POINT ( 'NONE',  ( -104.4934867380000014, 1379.706082156179946, 304.0189722064590114 ) ) ;
#56890 = CARTESIAN_POINT ( 'NONE',  ( -14.11093413346683612, 1408.367734284578319, 269.5873373858704554 ) ) ;
#56891 = VECTOR ( 'NONE', #20682, 1000.000000000000114 ) ;
#56892 = CARTESIAN_POINT ( 'NONE',  ( 11.22682033204820051, 1470.417118964590145, 207.3383776542460168 ) ) ;
#56893 = CARTESIAN_POINT ( 'NONE',  ( -5.020870921430000244, 1483.991119631089987, 199.5319357661589947 ) ) ;
#56894 = CARTESIAN_POINT ( 'NONE',  ( -15.48407483730515644, 1451.379909330961709, 222.5591913156476949 ) ) ;
#56895 = CARTESIAN_POINT ( 'NONE',  ( -13.15765241484907300, 1444.750370938229707, 186.5139969393457307 ) ) ;
#56896 = LINE ( 'NONE', #108393, #84254 ) ;
#56897 = CARTESIAN_POINT ( 'NONE',  ( -5.276062718737005497, 1507.211508871218712, 236.2464138374867844 ) ) ;
#56898 = DIRECTION ( 'NONE',  ( 0.000000000000000000, -1.000000000000000000, -2.307067265786200309E-16 ) ) ;
#56899 = DIRECTION ( 'NONE',  ( 0.000000000000000000, 1.000000000000000000, 0.000000000000000000 ) ) ;
#56900 = CARTESIAN_POINT ( 'NONE',  ( 24.92861831849999987, 1436.146573568669965, 137.7188798219979731 ) ) ;
#56901 = CARTESIAN_POINT ( 'NONE',  ( -17.18726318579999912, 1440.321463842890125, 217.4344804300990290 ) ) ;
#56903 = ORIENTED_EDGE ( 'NONE', *, *, #97593, .F. ) ;
#56902 = CARTESIAN_POINT ( 'NONE',  ( -14.52033150799999994, 1409.926738554830081, 226.5601352792980094 ) ) ;
#56904 = CARTESIAN_POINT ( 'NONE',  ( -106.4241660069999966, 1383.759861017009825, 311.1380007012590454 ) ) ;
#56905 = CARTESIAN_POINT ( 'NONE',  ( 12.57832847022450018, 1512.205851781549882, 224.1512894226670198 ) ) ;
#56906 = ORIENTED_EDGE ( 'NONE', *, *, #38752, .T. ) ;
#56907 = ORIENTED_EDGE ( 'NONE', *, *, #18438, .T. ) ;
#56908 = CARTESIAN_POINT ( 'NONE',  ( -11.39916848899999913, 1500.963021451090071, 210.1012423875770025 ) ) ;
#56909 = CARTESIAN_POINT ( 'NONE',  ( 6.354226016189142179, 1516.697111559987889, 205.1358369536649775 ) ) ;
#56911 = CARTESIAN_POINT ( 'NONE',  ( 3.176504636720000085E-09, 1468.737548874529921, 250.5651368536980215 ) ) ;
#56910 = CARTESIAN_POINT ( 'NONE',  ( 5.126901366830000306, 1455.691003689690206, 218.4326852860489794 ) ) ;
#56912 = B_SPLINE_CURVE_WITH_KNOTS ( 'NONE', 3,
 ( #63532, #71940, #28795, #104392 ),
 .UNSPECIFIED., .F., .F.,
 ( 4, 4 ),
 ( 1.502771284927900908, 1.508489632590340079 ),
 .UNSPECIFIED. ) ;
#56913 = CARTESIAN_POINT ( 'NONE',  ( -20.02495950560000182, 1491.257731268429779, 190.2391440648979994 ) ) ;
#56914 = CIRCLE ( 'NONE', #46231, 4.004360693725719678 ) ;
#56915 = CARTESIAN_POINT ( 'NONE',  ( -11.00793686009999917, 1433.412981438380029, 151.7533247267980130 ) ) ;
#56916 = EDGE_CURVE ( 'NONE', #20305, #7608, #61216, .T. ) ;
#56917 = DIRECTION ( 'NONE',  ( 0.9455185755993178454, 0.000000000000000000, -0.3255681544571537578 ) ) ;
#56918 = CARTESIAN_POINT ( 'NONE',  ( -5.106893094710000192, 1391.877272790489997, 203.8075142969990168 ) ) ;
#56919 = CARTESIAN_POINT ( 'NONE',  ( 9.492563787872798642, 1464.256798853970167, 211.6513489870939964 ) ) ;
#56920 = ADVANCED_FACE ( 'NONE', ( #43818 ), #51121, .F. ) ;
#56921 = CARTESIAN_POINT ( 'NONE',  ( -25.59514252499999998, 1439.610094980949953, 138.2637330278979846 ) ) ;
#56922 = CARTESIAN_POINT ( 'NONE',  ( -0.7783252048265130174, 1515.125841190099891, 213.4496961315290093 ) ) ;
#56923 = CARTESIAN_POINT ( 'NONE',  ( -3.271538019026510202, 1454.292002138270163, 199.1638778078030043 ) ) ;
#56924 = CARTESIAN_POINT ( 'NONE',  ( 3.102049425449999731, 1451.170629086630015, 183.9343634219979720 ) ) ;
#56925 = VECTOR ( 'NONE', #104809, 1000.000000000000000 ) ;
#56926 = CARTESIAN_POINT ( 'NONE',  ( -5.364860563355343004, 1363.173009576943059, 209.6218459617148824 ) ) ;
#56927 = CARTESIAN_POINT ( 'NONE',  ( -12.51566962417496143, 1509.474120198974106, 236.3954631667255626 ) ) ;
#56930 = VERTEX_POINT ( 'NONE', #61208 ) ;
#56929 = CARTESIAN_POINT ( 'NONE',  ( 1.013095580766330129E-08, 1409.267137198459977, 260.2682267152229656 ) ) ;
#56928 = B_SPLINE_CURVE_WITH_KNOTS ( 'NONE', 3,
 ( #36443, #103656, #36994, #35348, #26383, #104757 ),
 .UNSPECIFIED., .F., .F.,
 ( 4, 2, 4 ),
 ( 0.4999572393258174818, 0.7499786196629087964, 1.000000000000000000 ),
 .UNSPECIFIED. ) ;
#56931 = ORIENTED_EDGE ( 'NONE', *, *, #25623, .F. ) ;
#56932 = CARTESIAN_POINT ( 'NONE',  ( -11.85846968594809958, 1431.803688344790089, 149.9564276896689989 ) ) ;
#56933 = CIRCLE ( 'NONE', #39071, 4.000000000000003553 ) ;
#56934 = CARTESIAN_POINT ( 'NONE',  ( -0.1743923092878569836, 1501.248403096799848, 233.2153375875180075 ) ) ;
#56935 = CARTESIAN_POINT ( 'NONE',  ( -7.395436080089999642, 1472.163566644230059, 270.3697506832979798 ) ) ;
#56936 = CARTESIAN_POINT ( 'NONE',  ( -21.38516915557943321, 1501.977400791986611, 237.8497028174240313 ) ) ;
#56937 =( BOUNDED_CURVE ( )  B_SPLINE_CURVE ( 3, ( #88953, #70540, #72724, #3882 ),
 .UNSPECIFIED., .F., .T. ) 
 B_SPLINE_CURVE_WITH_KNOTS ( ( 4, 4 ),
 ( 4.310049633749867937, 4.645868665744727011 ),
 .UNSPECIFIED. ) 
 CURVE ( )  GEOMETRIC_REPRESENTATION_ITEM ( )  RATIONAL_B_SPLINE_CURVE ( ( 1.000000000000000000, 0.9906241907223192200, 0.9906241907223192200, 1.000000000000000000 ) ) 
 REPRESENTATION_ITEM ( '' )  );
#56938 = CARTESIAN_POINT ( 'NONE',  ( 1.600048698852036821, 1411.254281879943164, 137.0999999980979851 ) ) ;
#56939 = CARTESIAN_POINT ( 'NONE',  ( 35.80456163590090313, 1451.000443318900125, 135.9277141877360293 ) ) ;
#56940 = CIRCLE ( 'NONE', #26544, 11.73460161499999899 ) ;
#56941 = CARTESIAN_POINT ( 'NONE',  ( 0.2335509722129010257, 1451.541237093220161, 182.7232813895910226 ) ) ;
#56942 = CARTESIAN_POINT ( 'NONE',  ( -9.093004793099998651, 1384.764870898179879, 199.9460030570490119 ) ) ;
#56943 = CARTESIAN_POINT ( 'NONE',  ( 12.27023112330000032, 1416.839692136459917, 223.5796784318309847 ) ) ;
#56944 = CARTESIAN_POINT ( 'NONE',  ( -4.228037575960000183, 1457.658301557489949, 217.8226702182289785 ) ) ;
#56945 = CARTESIAN_POINT ( 'NONE',  ( 10.80894745490800624, 1367.705630506329499, 208.3718459617010978 ) ) ;
#56946 = CARTESIAN_POINT ( 'NONE',  ( -39.78160441305559658, 1422.810119569090148, 268.4168317394310179 ) ) ;
#56947 = ORIENTED_EDGE ( 'NONE', *, *, #59577, .T. ) ;
#56948 = CARTESIAN_POINT ( 'NONE',  ( -3.534341588258910427, 1492.696478981339851, 181.5914780206049954 ) ) ;
#56949 = VERTEX_POINT ( 'NONE', #51672 ) ;
#56950 = VERTEX_POINT ( 'NONE', #110464 ) ;
#56951 = CARTESIAN_POINT ( 'NONE',  ( -6.935801299664999142, 1516.621991115350056, 210.2518484644969874 ) ) ;
#56952 = CARTESIAN_POINT ( 'NONE',  ( -8.866734544810560337, 1447.658174592660089, 212.1401281790719793 ) ) ;
#56953 = CARTESIAN_POINT ( 'NONE',  ( -2.500000000000000000, 1425.929641636930000, 184.1455913746980002 ) ) ;
#56954 = CIRCLE ( 'NONE', #10498, 2.000000000000003553 ) ;
#56955 = EDGE_CURVE ( 'NONE', #101745, #94269, #98437, .T. ) ;
#56957 = CARTESIAN_POINT ( 'NONE',  ( -3.497130751176168673, 1441.358031377314319, 170.5351636631657755 ) ) ;
#56956 = CARTESIAN_POINT ( 'NONE',  ( -6.547556969464999987, 1516.633288330999903, 212.3841106205370011 ) ) ;
#56958 = CARTESIAN_POINT ( 'NONE',  ( -16.07232597160000154, 1440.437412726279945, 189.9216664607980078 ) ) ;
#56959 = CARTESIAN_POINT ( 'NONE',  ( -17.74184486700000107, 1415.163755984229965, 208.0694140301980326 ) ) ;
#56960 = ORIENTED_EDGE ( 'NONE', *, *, #16997, .F. ) ;
#56961 = CARTESIAN_POINT ( 'NONE',  ( -25.99289974769999745, 1436.215948439619979, 136.7796492369979831 ) ) ;
#56962 = EDGE_CURVE ( 'NONE', #110163, #91726, #103274, .T. ) ;
#56963 = ADVANCED_FACE ( 'NONE', ( #15012 ), #73298, .F. ) ;
#56964 = CARTESIAN_POINT ( 'NONE',  ( -3.456007423304999993, 1516.647534046129977, 202.5739645571870255 ) ) ;
#56965 = CARTESIAN_POINT ( 'NONE',  ( 1.999999980934999977, 1520.551704408390151, 195.7913026028670060 ) ) ;
#56966 = CARTESIAN_POINT ( 'NONE',  ( -21.15898116937230000, 1384.535980822740157, 202.0007022378129875 ) ) ;
#56967 = CARTESIAN_POINT ( 'NONE',  ( 0.06333900032629999344, 1408.725629451930217, 195.0481631164979888 ) ) ;
#56968 = CARTESIAN_POINT ( 'NONE',  ( -111.6465390607511097, 1305.714868215269917, 299.0089331859842332 ) ) ;
#56969 = FACE_OUTER_BOUND ( 'NONE', #41485, .T. ) ;
#56971 = ORIENTED_EDGE ( 'NONE', *, *, #57916, .F. ) ;
#56970 = CARTESIAN_POINT ( 'NONE',  ( -8.725041378416754867, 1365.289353615551363, 210.6218459617142003 ) ) ;
#56972 = ORIENTED_EDGE ( 'NONE', *, *, #7034, .T. ) ;
#56973 = B_SPLINE_CURVE_WITH_KNOTS ( 'NONE', 3,
 ( #47270, #57886, #81953, #100419, #64641, #5260, #74138, #57349, #92021, #49483, #31554, #98762, #74687, #23702, #108820, #73590, #56220, #15291, #14197, #83606, #6904, #32665, #90351, #31005, #66843, #65185, #91474, #90913, #100953, #89813, #82526, #13084, #5823, #39962, #108268, #65732, #77977, #58429 ),
 .UNSPECIFIED., .F., .F.,
 ( 4, 2, 2, 1, 1, 1, 1, 2, 2, 2, 1, 1, 1, 1, 2, 2, 2, 2, 2, 2, 2, 2, 4 ),
 ( 0.000000000000000000, 0.2499999999999851230, 0.3749999999999770184, 0.4374999999999749090, 0.4687499999999736877, 0.4843749999999719669, 0.4921874999999717448, 0.4960937499999722444, 0.4999999999999726885, 0.6249999999999740208, 0.6874999999999745759, 0.7187499999999750200, 0.7343749999999742428, 0.7421874999999739098, 0.7460937499999727995, 0.7499999999999716893, 0.8124999999999706901, 0.8437499999999695799, 0.8593749999999681366, 0.8671874999999682476, 0.8710937499999690248, 0.8749999999999698019, 1.000000000000000000 ),
 .UNSPECIFIED. ) ;
#56974 = PLANE ( 'NONE',  #38601 ) ;
#56975 = CARTESIAN_POINT ( 'NONE',  ( 32.52417149305044575, 1464.889216426557823, 269.3047436042317599 ) ) ;
#56976 = ADVANCED_FACE ( 'NONE', ( #5539 ), #14471, .F. ) ;
#56977 = CARTESIAN_POINT ( 'NONE',  ( 4.900781089548089220, 1426.655589109569746, 191.7260386988809842 ) ) ;
#56978 = CARTESIAN_POINT ( 'NONE',  ( 2.500574528909250027, 1448.942056006560051, 154.5733147652059927 ) ) ;
#56979 = CARTESIAN_POINT ( 'NONE',  ( -1.857324058419999924, 1485.892948864229993, 182.0392558147979969 ) ) ;
#56980 = CARTESIAN_POINT ( 'NONE',  ( -2.477975353594999763, 1516.839862955080207, 210.2583935552169976 ) ) ;
#56981 = ADVANCED_FACE ( 'NONE', ( #99573 ), #40789, .F. ) ;
#56982 = CARTESIAN_POINT ( 'NONE',  ( -68.78439012009999942, 1379.747952156290012, 280.2618955346589473 ) ) ;
#56983 = CARTESIAN_POINT ( 'NONE',  ( -1.725662463192670248, 1484.236887848700007, 182.7463278875050037 ) ) ;
#56984 = CARTESIAN_POINT ( 'NONE',  ( 7.716990237357959970, 1439.907775640959926, 213.4893468860780104 ) ) ;
#56985 = CARTESIAN_POINT ( 'NONE',  ( 18.80431614589912925, 1425.839298383276855, 225.4579118312513799 ) ) ;
#56986 = CARTESIAN_POINT ( 'NONE',  ( 7.983219816825001480, 1511.369014903080142, 203.7222546344770251 ) ) ;
#56987 = CARTESIAN_POINT ( 'NONE',  ( 2.476450664134999702, 1516.843453247299749, 206.8221896160070230 ) ) ;
#56988 = ORIENTED_EDGE ( 'NONE', *, *, #106963, .F. ) ;
#56989 = CARTESIAN_POINT ( 'NONE',  ( -38.81202643688960308, 1436.797832322100021, 134.7398497853949948 ) ) ;
#56991 = ADVANCED_FACE ( 'NONE', ( #39690 ), #65466, .F. ) ;
#56990 = CARTESIAN_POINT ( 'NONE',  ( -11.22397442029999937, 1471.293743228789936, 207.0223102294889941 ) ) ;
#56992 = CARTESIAN_POINT ( 'NONE',  ( -12.78749341904959991, 1416.842625005220043, 196.1051283137009875 ) ) ;
#56993 = EDGE_LOOP ( 'NONE', ( #35344, #46974, #400, #84474 ) ) ;
#56994 = DIRECTION ( 'NONE',  ( -0.9996573249755574819, -0.02617694830786557875, 0.000000000000000000 ) ) ;
#56995 = CARTESIAN_POINT ( 'NONE',  ( 12.52716981047909961, 1435.792588977599962, 150.9477529820620134 ) ) ;
#56996 = CARTESIAN_POINT ( 'NONE',  ( 13.36846539799999967, 1415.041103189330215, 197.6149988125980030 ) ) ;
#56997 = EDGE_CURVE ( 'NONE', #104898, #105852, #72575, .T. ) ;
#56998 = CARTESIAN_POINT ( 'NONE',  ( 22.96901158543817090, 1517.151704408390060, 206.5493031772561778 ) ) ;
#56999 = DIRECTION ( 'NONE',  ( 1.000000000000000000, 0.000000000000000000, 0.000000000000000000 ) ) ;
#57000 = CARTESIAN_POINT ( 'NONE',  ( 17.13440814598840234, 1415.954755712160022, 210.5946189592040128 ) ) ;
#57001 = CARTESIAN_POINT ( 'NONE',  ( -23.77630258579999634, 1416.435788914229988, 210.4864640035480079 ) ) ;
#57002 = EDGE_CURVE ( 'NONE', #50173, #2195, #81868, .T. ) ;
#57003 = CARTESIAN_POINT ( 'NONE',  ( -0.02610323598444003190, 1506.535970902593817, 187.0533209056380315 ) ) ;
#57004 = CARTESIAN_POINT ( 'NONE',  ( 4.273772382725350205, 1441.086506954710103, 157.4487869396440090 ) ) ;
#57005 = CARTESIAN_POINT ( 'NONE',  ( 2.500000000000000000, 1439.396215927459934, 161.7067232356089903 ) ) ;
#57006 = AXIS2_PLACEMENT_3D ( 'NONE', #35153, #52526, #69896 ) ;
#57007 = CARTESIAN_POINT ( 'NONE',  ( -16.68599179819999989, 1461.099982565929849, 230.2790296985980092 ) ) ;
#57008 = CARTESIAN_POINT ( 'NONE',  ( 3.261007131564999995, 1516.596789218710001, 216.4445556570670135 ) ) ;
#57009 = EDGE_LOOP ( 'NONE', ( #65070, #2520, #62910, #71488, #104468 ) ) ;
#57010 = CARTESIAN_POINT ( 'NONE',  ( 7.709220066765960055, 1516.541497140389993, 207.3539078949219743 ) ) ;
#57011 = CARTESIAN_POINT ( 'NONE',  ( -22.59589776172869691, 1507.700906949889941, 190.9355226902430047 ) ) ;
#57012 = AXIS2_PLACEMENT_3D ( 'NONE', #45395, #35876, #96882 ) ;
#57013 = EDGE_CURVE ( 'NONE', #30027, #72223, #66169, .T. ) ;
#57014 = DIRECTION ( 'NONE',  ( -0.8775825618903760894, 0.000000000000000000, -0.4794255386041968436 ) ) ;
#57015 = CIRCLE ( 'NONE', #31973, 2.000006057866878351 ) ;
#57016 = CARTESIAN_POINT ( 'NONE',  ( -16.43897083077359866, 1508.454179826399923, 213.9817428091590159 ) ) ;
#57017 = CARTESIAN_POINT ( 'NONE',  ( 1.396949333800000081, 1473.097534632089946, 219.2356275978989970 ) ) ;
#57018 = CARTESIAN_POINT ( 'NONE',  ( 12.92703571545800045, 1509.364482422050060, 181.5834217730510147 ) ) ;
#57019 = CARTESIAN_POINT ( 'NONE',  ( 11.11955572112504598, 1425.169096886590978, 138.4856970310274278 ) ) ;
#57020 = CARTESIAN_POINT ( 'NONE',  ( 3.043251597425320032, 1417.779699503100119, 234.3208248802520188 ) ) ;
#57021 = CARTESIAN_POINT ( 'NONE',  ( -2.500000000000000000, 1421.191390850129892, 151.1105839291980146 ) ) ;
#57022 = CARTESIAN_POINT ( 'NONE',  ( -109.1672625384930058, 1385.040948060030132, 297.1348415520359367 ) ) ;
#57023 = CARTESIAN_POINT ( 'NONE',  ( -21.54116136303384721, 1523.462669333493295, 183.9310736449068884 ) ) ;
#57024 = CARTESIAN_POINT ( 'NONE',  ( 31.09959380193599898, 1440.913060384139953, 241.6673604977229957 ) ) ;
#57026 = CARTESIAN_POINT ( 'NONE',  ( 33.36586802512172767, 1518.913060387330006, 201.9069332299488622 ) ) ;
#57025 = FACE_OUTER_BOUND ( 'NONE', #110513, .T. ) ;
#57027 = LINE ( 'NONE', #6049, #68968 ) ;
#57028 = ORIENTED_EDGE ( 'NONE', *, *, #66126, .T. ) ;
#57029 = ORIENTED_EDGE ( 'NONE', *, *, #70627, .F. ) ;
#57030 = CARTESIAN_POINT ( 'NONE',  ( -2.487935123034410001, 1508.551704413348716, 213.9802063494123558 ) ) ;
#57031 = CARTESIAN_POINT ( 'NONE',  ( -11.66183466779353672, 1506.404057808254720, 227.7379997552472730 ) ) ;
#57032 = CARTESIAN_POINT ( 'NONE',  ( -3.463912908579999783, 1443.361677142989947, 200.0971741339589869 ) ) ;
#57033 = CARTESIAN_POINT ( 'NONE',  ( 11.81247832421080091, 1501.731194366300087, 211.4919564201209710 ) ) ;
#57034 = AXIS2_PLACEMENT_3D ( 'NONE', #56135, #9851, #106538 ) ;
#57035 = CARTESIAN_POINT ( 'NONE',  ( 2.688586027246119947, 1509.006950727750109, 238.2845013960090057 ) ) ;
#57036 = CARTESIAN_POINT ( 'NONE',  ( 10.60523232130659999, 1422.322173433070020, 211.3613908351649968 ) ) ;
#57037 = CARTESIAN_POINT ( 'NONE',  ( -11.00154618500000048, 1492.089968578990010, 210.0309033811119832 ) ) ;
#57038 = EDGE_CURVE ( 'NONE', #35225, #24399, #3185, .T. ) ;
#57039 = LINE ( 'NONE', #73268, #50480 ) ;
#57040 = CARTESIAN_POINT ( 'NONE',  ( -45.63068801059250035, 1383.819138085639906, 252.4128947413499873 ) ) ;
#57041 = CARTESIAN_POINT ( 'NONE',  ( -4.542415428115000431, 1511.388520542559945, 200.7513169665770079 ) ) ;
#57042 = CARTESIAN_POINT ( 'NONE',  ( -13.59753454029999808, 1453.151875978430098, 193.6408191069980091 ) ) ;
#57043 = ADVANCED_FACE ( 'NONE', ( #74418 ), #108544, .T. ) ;
#57044 = CARTESIAN_POINT ( 'NONE',  ( -11.88383462049809935, 1433.642778087510123, 147.6544717980860355 ) ) ;
#57045 = CARTESIAN_POINT ( 'NONE',  ( -23.55087667009999919, 1411.110693366829764, 210.4794020521279947 ) ) ;
#57047 = EDGE_LOOP ( 'NONE', ( #87804, #50655, #64904, #60828 ) ) ;
#57046 = CARTESIAN_POINT ( 'NONE',  ( -1.008560136250000072, 1456.416633368590055, 218.7046624972589939 ) ) ;
#57048 = DIRECTION ( 'NONE',  ( -0.03489949670246857150, 0.9993908270190969834, 0.000000000000000000 ) ) ;
#57049 = CARTESIAN_POINT ( 'NONE',  ( -9.645382992169999170, 1380.202965523560124, 203.3638893722689716 ) ) ;
#57050 = CARTESIAN_POINT ( 'NONE',  ( -3.739222493130000213, 1474.769836386989937, 198.3144648466990247 ) ) ;
#57052 = ORIENTED_EDGE ( 'NONE', *, *, #51473, .F. ) ;
#57051 = CARTESIAN_POINT ( 'NONE',  ( -17.55992563626299940, 1415.427621830080170, 208.9996007598010124 ) ) ;
#57053 = ORIENTED_EDGE ( 'NONE', *, *, #95934, .T. ) ;
#57054 = CARTESIAN_POINT ( 'NONE',  ( -7.720734276493420367, 1386.472163584720192, 218.9022333215830258 ) ) ;
#57055 = CARTESIAN_POINT ( 'NONE',  ( -4.329448802989709577, 1515.064791341159889, 206.7919475917079808 ) ) ;
#57056 = LINE ( 'NONE', #80588, #26150 ) ;
#57057 = CARTESIAN_POINT ( 'NONE',  ( 5.597778194180000888, 1506.679269386989972, 219.3685102149989916 ) ) ;
#57058 = CARTESIAN_POINT ( 'NONE',  ( -106.7722198320000047, 1381.894365751589930, 298.4459716942589580 ) ) ;
#57059 = EDGE_CURVE ( 'NONE', #35548, #21410, #64659, .T. ) ;
#57060 = CARTESIAN_POINT ( 'NONE',  ( -8.991629940588330427, 1509.227055023859975, 237.0095830223739881 ) ) ;
#57061 = APPLICATION_CONTEXT ( 'automotive_design' ) ;
#57062 = CARTESIAN_POINT ( 'NONE',  ( -3.327638442502410143, 1485.035901024235045, 183.3370786331138902 ) ) ;
#57063 = CARTESIAN_POINT ( 'NONE',  ( 4.898545953690760513, 1409.084121381390105, 194.9685614766650019 ) ) ;
#57064 = CARTESIAN_POINT ( 'NONE',  ( 18.52260186970000433, 1425.593317732829973, 225.5454236923980034 ) ) ;
#57065 = CARTESIAN_POINT ( 'NONE',  ( 3.741709429870000214, 1419.924742150030170, 185.5167356432980057 ) ) ;
#57066 = CARTESIAN_POINT ( 'NONE',  ( -19.82310150189999831, 1485.643326822829977, 190.4781767699980151 ) ) ;
#57067 = CARTESIAN_POINT ( 'NONE',  ( 11.57581721370000061, 1432.288378390559956, 151.1967356790979977 ) ) ;
#57068 = DIRECTION ( 'NONE',  ( 0.000000000000000000, 1.000000000000000000, 0.000000000000000000 ) ) ;
#57069 = ORIENTED_EDGE ( 'NONE', *, *, #48250, .T. ) ;
#57070 = CARTESIAN_POINT ( 'NONE',  ( -2.189600725003922665, 1397.978978549970634, 196.1218685907498696 ) ) ;
#57071 = CARTESIAN_POINT ( 'NONE',  ( 19.01768856890259940, 1456.707458847550015, 226.2400544105869926 ) ) ;
#57072 = CARTESIAN_POINT ( 'NONE',  ( -12.28572370999999919, 1434.398876809329977, 150.4686729132979792 ) ) ;
#57073 = AXIS2_PLACEMENT_3D ( 'NONE', #107036, #64512, #30323 ) ;
#57074 = EDGE_CURVE ( 'NONE', #59250, #35478, #98265, .T. ) ;
#57075 = AXIS2_PLACEMENT_3D ( 'NONE', #99481, #5995, #40147 ) ;
#57076 = CARTESIAN_POINT ( 'NONE',  ( -6.617837785385730167E-10, 1467.263505378270111, 245.8824296936540179 ) ) ;
#57077 = CARTESIAN_POINT ( 'NONE',  ( -20.20716384489490025, 1495.140560500310130, 190.7583971611010156 ) ) ;
#57078 = CARTESIAN_POINT ( 'NONE',  ( -15.32768421809999992, 1420.023183193880186, 211.9636741928989920 ) ) ;
#57079 = CARTESIAN_POINT ( 'NONE',  ( -108.3907530290000096, 1386.531684817010046, 310.8877082452589775 ) ) ;
#57080 = CARTESIAN_POINT ( 'NONE',  ( -8.424736004331359496, 1511.534310205860038, 214.8401254943979950 ) ) ;
#57081 = CARTESIAN_POINT ( 'NONE',  ( -10.47377929740979141, 1362.785267724748564, 210.6218459617030021 ) ) ;
#57082 = CARTESIAN_POINT ( 'NONE',  ( -45.85451249346039759, 1440.699916666199897, 268.7563676993480044 ) ) ;
#57083 = CARTESIAN_POINT ( 'NONE',  ( -20.07368861760000200, 1427.190829891029807, 224.4645657875979907 ) ) ;
#57084 = EDGE_CURVE ( 'NONE', #51188, #105370, #47188, .T. ) ;
#57085 = CARTESIAN_POINT ( 'NONE',  ( -20.01067139950000140, 1507.877425041529932, 188.9709217985979706 ) ) ;
#57086 = CARTESIAN_POINT ( 'NONE',  ( 1.117840086735000016, 1516.949031626070109, 207.4047068479870006 ) ) ;
#57087 = DIRECTION ( 'NONE',  ( -1.000000000000000000, 0.000000000000000000, 0.000000000000000000 ) ) ;
#57088 = CARTESIAN_POINT ( 'NONE',  ( 30.45769963431402871, 1526.208281990536307, 201.0929247824067829 ) ) ;
#57089 = CARTESIAN_POINT ( 'NONE',  ( -2.320366121469999879E-14, 1422.005499580429841, 112.3240130698980010 ) ) ;
#57090 = CARTESIAN_POINT ( 'NONE',  ( 7.481606250500309585, 1425.290164852929820, 212.2841966316389914 ) ) ;
#57091 = CIRCLE ( 'NONE', #62467, 2.000000000549930324 ) ;
#57092 = ORIENTED_EDGE ( 'NONE', *, *, #40027, .F. ) ;
#57093 = CARTESIAN_POINT ( 'NONE',  ( 29.66529949999999971, 1430.834809503430051, 244.2516413529979786 ) ) ;
#57094 = CARTESIAN_POINT ( 'NONE',  ( -6.466996272939999457, 1422.019461440550231, 192.0563668886989888 ) ) ;
#57096 = CARTESIAN_POINT ( 'NONE',  ( -15.00007760880209950, 1512.191474810040063, 221.6539140102569831 ) ) ;
#57095 = CARTESIAN_POINT ( 'NONE',  ( -2.509552835650000091, 1469.876049247530091, 182.4287443342980168 ) ) ;
#57097 = CARTESIAN_POINT ( 'NONE',  ( -19.75056259240000145, 1465.177823603190063, 209.1218459616989946 ) ) ;
#57098 = CARTESIAN_POINT ( 'NONE',  ( -4.694071438699999987, 1416.682256490530108, 238.2947547715980079 ) ) ;
#57099 = CARTESIAN_POINT ( 'NONE',  ( -4.642747618861698733, 1378.261778813269530, 214.5306460145334313 ) ) ;
#57100 = EDGE_CURVE ( 'NONE', #89175, #27764, #29912, .T. ) ;
#57101 = CARTESIAN_POINT ( 'NONE',  ( -19.22419269387500051, 1452.241736785570083, 144.1488803750449961 ) ) ;
#57102 = CARTESIAN_POINT ( 'NONE',  ( 27.43971470800000034, 1451.956092027530076, 135.3397597194980051 ) ) ;
#57103 = ORIENTED_EDGE ( 'NONE', *, *, #35723, .F. ) ;
#57104 = CARTESIAN_POINT ( 'NONE',  ( -5.366169653819650165, 1425.895367196510051, 152.2258176257520290 ) ) ;
#57105 = CARTESIAN_POINT ( 'NONE',  ( 16.10004403616710178, 1421.719552068429948, 227.3840503930599937 ) ) ;
#57106 = CARTESIAN_POINT ( 'NONE',  ( -3.708479360574112871, 1448.977613576670137, 184.9605879005348470 ) ) ;
#57107 = ORIENTED_EDGE ( 'NONE', *, *, #83741, .F. ) ;
#57108 = ORIENTED_EDGE ( 'NONE', *, *, #34951, .T. ) ;
#57109 = CARTESIAN_POINT ( 'NONE',  ( -58.30163007960000243, 1385.052442321870103, 240.0694839391589994 ) ) ;
#57110 = CARTESIAN_POINT ( 'NONE',  ( -24.09440364030000126, 1410.858583525330005, 209.4069519282039948 ) ) ;
#57111 = EDGE_CURVE ( 'NONE', #40948, #17784, #41033, .T. ) ;
#57112 = ORIENTED_EDGE ( 'NONE', *, *, #33184, .T. ) ;
#57113 = CARTESIAN_POINT ( 'NONE',  ( 0.2223819999059999941, 1416.825245919329973, 227.1889460349979970 ) ) ;
#57114 = AXIS2_PLACEMENT_3D ( 'NONE', #17178, #44090, #50826 ) ;
#57115 = ADVANCED_FACE ( 'NONE', ( #25066 ), #10530, .F. ) ;
#57116 = CARTESIAN_POINT ( 'NONE',  ( -4.763329158539999497, 1498.348145572129852, 235.9684822528980135 ) ) ;
#57117 = CARTESIAN_POINT ( 'NONE',  ( 4.987078397334300028, 1508.551704408389924, 211.6097676058329853 ) ) ;
#57118 = CARTESIAN_POINT ( 'NONE',  ( 44.98134005857980355, 1448.496320712010174, 268.5302312373070208 ) ) ;
#57119 = B_SPLINE_CURVE_WITH_KNOTS ( 'NONE', 3,
 ( #22581, #6918, #75252, #23712, #109942, #93128, #48395, #108830, #109401, #50590, #32127, #24262, #83082, #32677, #56786, #58442, #15841, #16395, #50046, #7473, #91484, #24795, #99861, #82538, #23158, #5834, #8019, #14763, #25354, #59547, #51695, #102608, #18067, #34332, #85836, #93660, #51143, #16941, #94223, #8567, #18609, #35436, #25908, #60106, #9674, #85269, #77990, #208, #94790, #68510, #42738, #9136, #52261, #27047, #110488, #86386, #76899, #52808, #102072, #69068, #17498, #43299 ),
 .UNSPECIFIED., .F., .F.,
 ( 4, 2, 2, 2, 1, 1, 1, 1, 2, 2, 2, 2, 2, 1, 1, 1, 2, 2, 2, 2, 2, 1, 1, 1, 1, 2, 2, 2, 2, 2, 1, 1, 1, 1, 1, 2, 2, 2, 4 ),
 ( 0.000000000000000000, 0.1249999999997849776, 0.1874999999996783406, 0.2187499999996239675, 0.2343749999995965727, 0.2421874999995830280, 0.2460937499995761168, 0.2480468749995727862, 0.2490234374995723421, 0.2499999999995718425, 0.3749999999996110334, 0.4374999999996306843, 0.4687499999996404543, 0.4843749999996453948, 0.4921874999996478373, 0.4960937499996490030, 0.4980468749996495581, 0.4999999999996500577, 0.6249999999997927214, 0.6874999999998652189, 0.7187499999999015232, 0.7343749999999198419, 0.7421874999999285016, 0.7460937499999318323, 0.7480468749999337197, 0.7490234374999340528, 0.7499999999999342748, 0.8124999999999202860, 0.8437499999999132916, 0.8593749999999095168, 0.8671874999999076294, 0.8710937499999068523, 0.8730468749999071854, 0.8740234374999071854, 0.8745117187499068523, 0.8747558593749064082, 0.8749999999999058531, 0.9374999999999529265, 1.000000000000000000 ),
 .UNSPECIFIED. ) ;
#57120 = CARTESIAN_POINT ( 'NONE',  ( -4.115862995762159748, 1509.032029411810072, 204.7576468414000033 ) ) ;
#57121 = CARTESIAN_POINT ( 'NONE',  ( -6.632177051280000235, 1428.092653318189832, 204.0245593685589824 ) ) ;
#57122 = CARTESIAN_POINT ( 'NONE',  ( -4.622842882315000068, 1516.901952101700090, 205.0913314195169903 ) ) ;
#57123 = EDGE_LOOP ( 'NONE', ( #55176, #20589, #18616, #78136 ) ) ;
#57124 = CYLINDRICAL_SURFACE ( 'NONE', #23956, 2.000000000000040856 ) ;
#57125 = CARTESIAN_POINT ( 'NONE',  ( 14.82736035860130031, 1512.135905030570029, 196.8226469024940002 ) ) ;
#57126 = CARTESIAN_POINT ( 'NONE',  ( 13.49999674949678763, 1444.108888658031219, 187.9769059414830963 ) ) ;
#57127 = ORIENTED_EDGE ( 'NONE', *, *, #96749, .T. ) ;
#57128 = ORIENTED_EDGE ( 'NONE', *, *, #44360, .F. ) ;
#57129 = DIRECTION ( 'NONE',  ( 0.9993902469235412811, -0.03489947644508390595, -0.001077449749359510062 ) ) ;
#57130 = CARTESIAN_POINT ( 'NONE',  ( -2.636066701933580170, 1508.551704408389924, 220.0370691182650091 ) ) ;
#57131 = CARTESIAN_POINT ( 'NONE',  ( -12.26154103078309987, 1512.129944624190102, 194.3268994079789991 ) ) ;
#57132 = CARTESIAN_POINT ( 'NONE',  ( 7.938530459438009501, 1504.028730547460100, 219.0969020694710139 ) ) ;
#57133 = CARTESIAN_POINT ( 'NONE',  ( 12.24199275630000017, 1420.231738084499966, 199.7476432072489843 ) ) ;
#57134 = ADVANCED_FACE ( 'NONE', ( #88314 ), #11607, .F. ) ;
#57135 = CARTESIAN_POINT ( 'NONE',  ( 19.01172303400000274, 1456.124536704289767, 212.8719163663189988 ) ) ;
#57136 = CARTESIAN_POINT ( 'NONE',  ( -109.4064894422378558, 1382.584668033352500, 297.3600029045636006 ) ) ;
#57137 = CARTESIAN_POINT ( 'NONE',  ( 10.33130932227850174, 1479.485470067400001, 205.9989652718629713 ) ) ;
#57138 = CARTESIAN_POINT ( 'NONE',  ( 0.03595598587303577842, 1409.477698216540603, 232.9236783021701171 ) ) ;
#57140 = CARTESIAN_POINT ( 'NONE',  ( -18.18137495006879689, 1507.546748573479817, 231.7129843945920129 ) ) ;
#57139 = CARTESIAN_POINT ( 'NONE',  ( 30.36938634820355176, 1525.506926151471134, 196.8236402350184449 ) ) ;
#57141 = CARTESIAN_POINT ( 'NONE',  ( 12.19798263851669873, 1426.952519236690023, 206.6044100701579680 ) ) ;
#57142 = CARTESIAN_POINT ( 'NONE',  ( -25.65004514716680362, 1509.804860194309867, 223.0705507710869995 ) ) ;
#57143 = EDGE_CURVE ( 'NONE', #104582, #65829, #18873, .T. ) ;
#57144 = CARTESIAN_POINT ( 'NONE',  ( 11.44291537990000052, 1428.994970000029980, 123.0297916884979941 ) ) ;
#57145 = ORIENTED_EDGE ( 'NONE', *, *, #109801, .F. ) ;
#57146 = CARTESIAN_POINT ( 'NONE',  ( 16.27172383310000114, 1476.104910058290216, 222.3698031616989965 ) ) ;
#57147 = CARTESIAN_POINT ( 'NONE',  ( -0.1806136374258420219, 1424.270560426740076, 227.7175953970750015 ) ) ;
#57148 = CARTESIAN_POINT ( 'NONE',  ( -89.61126119283551361, 1384.970433313389776, 308.5825330499230290 ) ) ;
#57149 = B_SPLINE_CURVE_WITH_KNOTS ( 'NONE', 3,
 ( #31906, #109186, #30245, #24032, #75035, #39767, #56574, #6151, #39197, #13991, #40859, #32471, #74490, #56023, #48178, #108617, #66645, #22934, #66094, #15087, #100221, #58230 ),
 .UNSPECIFIED., .F., .F.,
 ( 4, 3, 3, 3, 3, 3, 3, 4 ),
 ( -8.338844738667910761, -8.272689705420921413, -7.702803945130000329, -7.620147254847129403, -7.073208901094860224, -6.549836289219999941, -6.379554812754880011, -5.901451788533909948 ),
 .UNSPECIFIED. ) ;
#57150 = B_SPLINE_SURFACE_WITH_KNOTS ( 'NONE', 5, 5, ( 
 ( #98049, #108104, #73426, #81248, #89654, #65023 ),
 ( #72334, #20784, #4563, #54984, #22418, #106464 ),
 ( #21323, #31400, #38697, #96978, #107008, #30296 ),
 ( #14036, #20241, #64489, #56621, #54442, #88576 ),
 ( #98604, #21868, #46032, #56067, #90194, #13478 ),
 ( #48227, #82367, #47668, #81796, #5098, #40904 ),
 ( #110316, #59391, #57740, #41475, #42565, #49876 ),
 ( #8395, #91313, #66689, #42020, #33590, #75084 ),
 ( #84009, #33051, #7310, #91859, #24624, #15134 ) ),
 .UNSPECIFIED., .F., .F., .F.,
 ( 6, 3, 6 ),
 ( 6, 6 ),
 ( 13.60177910350000019, 23.50904048570000171, 33.41630186789999613 ),
 ( 0.000000000000000000, 2.000000000000000000 ),
 .UNSPECIFIED. ) ;
#57151 = CARTESIAN_POINT ( 'NONE',  ( -8.978047223340000826, 1387.343619535879952, 200.4278112474989939 ) ) ;
#57152 = CARTESIAN_POINT ( 'NONE',  ( 10.14203510082409920, 1422.829087935100006, 209.7690348518279961 ) ) ;
#57154 = VERTEX_POINT ( 'NONE', #5957 ) ;
#57153 = CARTESIAN_POINT ( 'NONE',  ( 11.07868621362170103, 1422.904854153429824, 203.3190901071859855 ) ) ;
#57155 = CARTESIAN_POINT ( 'NONE',  ( 1.398091756599999957, 1429.447055348990034, 217.3181151331990009 ) ) ;
#57156 = CARTESIAN_POINT ( 'NONE',  ( -0.8307690413430001142, 1441.600846913440137, 150.7224806086979640 ) ) ;
#57157 = AXIS2_PLACEMENT_3D ( 'NONE', #107588, #22448, #1160 ) ;
#57158 = CARTESIAN_POINT ( 'NONE',  ( -16.75075978319999948, 1417.136094290510073, 208.0073609310889822 ) ) ;
#57159 = CARTESIAN_POINT ( 'NONE',  ( 11.69137462480000167, 1433.691468119869796, 151.0156487431979997 ) ) ;
#57160 = CARTESIAN_POINT ( 'NONE',  ( -17.54272989919999759, 1417.931783365949968, 206.8684744458689977 ) ) ;
#57161 = B_SPLINE_SURFACE_WITH_KNOTS ( 'NONE', 5, 5, ( 
 ( #62017, #102860, #35125, #69307, #44652, #87759 ),
 ( #60343, #104541, #17181, #26157, #76576, #34018 ),
 ( #103414, #27837, #94464, #42419, #26720, #18308 ),
 ( #96137, #110729, #51375, #35676, #69865, #103982 ),
 ( #95587, #78793, #81524, #54719, #21060, #55266 ),
 ( #62588, #63136, #30022, #3765, #88846, #36789 ),
 ( #70981, #12685, #79349, #12131, #37899, #19976 ),
 ( #28947, #22153, #11041, #88296, #3216, #46324 ),
 ( #45210, #89396, #97237, #11590, #64776, #46865 ) ),
 .UNSPECIFIED., .F., .F., .F.,
 ( 6, 3, 6 ),
 ( 6, 6 ),
 ( 52.44345828979999879, 59.24089506869999866, 65.18833056040000429 ),
 ( 0.000000000000000000, 2.000000000000000000 ),
 .UNSPECIFIED. ) ;
#57162 = CARTESIAN_POINT ( 'NONE',  ( 0.6690161404288550440, 1450.887226503660031, 181.3223526815230002 ) ) ;
#57163 = CARTESIAN_POINT ( 'NONE',  ( -16.19492410612830113, 1409.478599598990058, 194.0661808939520085 ) ) ;
#57164 = TOROIDAL_SURFACE ( 'NONE', #87610, 1.000000000000000000, 1.000000000000000000 ) ;
#57165 = CARTESIAN_POINT ( 'NONE',  ( 9.267170318294839504, 1460.193123049920132, 205.0415981645240038 ) ) ;
#57166 = CARTESIAN_POINT ( 'NONE',  ( -108.3688902241231062, 1388.809589294943862, 298.1335643587438540 ) ) ;
#57167 = CARTESIAN_POINT ( 'NONE',  ( 2.948872346249999943, 1422.097626302630033, 232.1500477468979966 ) ) ;
#57168 = CARTESIAN_POINT ( 'NONE',  ( -21.61625474793734369, 1526.178928173327904, 234.4801574852453996 ) ) ;
#57169 = CARTESIAN_POINT ( 'NONE',  ( 8.178501070643639181, 1441.152429762079919, 153.9860758848200248 ) ) ;
#57170 = CARTESIAN_POINT ( 'NONE',  ( -18.19301384260000276, 1410.911466596229957, 224.4445374971980129 ) ) ;
#57171 = AXIS2_PLACEMENT_3D ( 'NONE', #106584, #64058, #98177 ) ;
#57172 = CARTESIAN_POINT ( 'NONE',  ( -20.61932039460000254, 1486.434366909889832, 211.1021073309690053 ) ) ;
#57173 = FACE_OUTER_BOUND ( 'NONE', #31042, .T. ) ;
#57174 = CARTESIAN_POINT ( 'NONE',  ( -17.29627815805059754, 1410.879850359289776, 192.2521459216479798 ) ) ;
#57175 = FACE_OUTER_BOUND ( 'NONE', #26516, .T. ) ;
#57176 = CARTESIAN_POINT ( 'NONE',  ( -2.792392588003332232, 1526.382868172863937, 176.8996806668727118 ) ) ;
#57177 = CARTESIAN_POINT ( 'NONE',  ( 19.66678637246580053, 1517.151704408390060, 202.3500283489900085 ) ) ;
#57178 = CARTESIAN_POINT ( 'NONE',  ( -8.513184503609998899, 1416.823418193129783, 225.1807616044980023 ) ) ;
#57179 = CARTESIAN_POINT ( 'NONE',  ( 0.2095880431046339976, 1457.579896474360112, 183.0569165344279838 ) ) ;
#57181 = ORIENTED_EDGE ( 'NONE', *, *, #101059, .T. ) ;
#57180 = CARTESIAN_POINT ( 'NONE',  ( 17.99954443082109989, 1410.904693892220166, 222.9872220945560173 ) ) ;
#57182 = CARTESIAN_POINT ( 'NONE',  ( -14.17095083369999919, 1415.425644477329797, 198.8594078928979911 ) ) ;
#57183 = CARTESIAN_POINT ( 'NONE',  ( -28.69260574566120070, 1509.783796149900127, 211.3048446392940320 ) ) ;
#57184 = CARTESIAN_POINT ( 'NONE',  ( 12.06097065039999983, 1433.903642588860066, 149.1895464303979963 ) ) ;
#57185 = CARTESIAN_POINT ( 'NONE',  ( -36.90142499642229978, 1436.372079655220205, 134.0999999968939846 ) ) ;
#57186 = CARTESIAN_POINT ( 'NONE',  ( 8.884500389519999430, 1442.039659523320097, 185.7099986671979934 ) ) ;
#57187 = ORIENTED_EDGE ( 'NONE', *, *, #106350, .T. ) ;
#57188 = CARTESIAN_POINT ( 'NONE',  ( -16.55384015340527526, 1524.739915903632664, 180.7880258469990338 ) ) ;
#57189 = CARTESIAN_POINT ( 'NONE',  ( -33.36586802512182715, 1511.187213306747708, 201.9069332299493169 ) ) ;
#57190 = CARTESIAN_POINT ( 'NONE',  ( -104.5461312646103949, 1380.583296262659132, 307.6660463617352548 ) ) ;
#57191 = CARTESIAN_POINT ( 'NONE',  ( -12.25773961910000054, 1490.408449763890076, 209.0370346857240236 ) ) ;
#57192 = CARTESIAN_POINT ( 'NONE',  ( 19.79581223833070069, 1456.560079648279952, 208.7498543415190113 ) ) ;
#57193 = CARTESIAN_POINT ( 'NONE',  ( -4.992349863779999453, 1391.620913471789891, 214.4361776263990009 ) ) ;
#57194 = CARTESIAN_POINT ( 'NONE',  ( 30.61211140304735423, 1415.566367963669336, 269.3440436895404559 ) ) ;
#57195 = CIRCLE ( 'NONE', #46482, 9.341369339569999042 ) ;
#57196 = CARTESIAN_POINT ( 'NONE',  ( 8.482142651180000215, 1423.325760005520124, 211.9865074947389871 ) ) ;
#57197 = CARTESIAN_POINT ( 'NONE',  ( -12.32664273690000023, 1378.996295195989887, 209.7960013046609902 ) ) ;
#57198 = CARTESIAN_POINT ( 'NONE',  ( 2.662122199679999746, 1434.188649408250058, 184.0358250344979751 ) ) ;
#57199 = CARTESIAN_POINT ( 'NONE',  ( -67.03515295860771062, 1385.097188996120167, 259.5578629473649812 ) ) ;
#57200 = CARTESIAN_POINT ( 'NONE',  ( -9.200421138165051360, 1422.937291722789951, 210.7384568321920142 ) ) ;
#57201 = CARTESIAN_POINT ( 'NONE',  ( -4.958796112629440422, 1508.551704408389924, 206.2486321841020072 ) ) ;
#57202 = ORIENTED_EDGE ( 'NONE', *, *, #5421, .F. ) ;
#57203 = CARTESIAN_POINT ( 'NONE',  ( -27.53435635780000013, 1451.950595041229917, 135.3364336049980068 ) ) ;
#57204 = CARTESIAN_POINT ( 'NONE',  ( -15.90322118183840061, 1409.851032194339950, 226.2872105686589919 ) ) ;
#57206 = ORIENTED_EDGE ( 'NONE', *, *, #82268, .F. ) ;
#57205 = CARTESIAN_POINT ( 'NONE',  ( 0.4931964325117270675, 1416.531771736229985, 184.8057391746860105 ) ) ;
#57207 = CARTESIAN_POINT ( 'NONE',  ( -109.6579480409999974, 1384.895131905899916, 311.3230545792589510 ) ) ;
#57208 = CARTESIAN_POINT ( 'NONE',  ( 40.26396420611710170, 1444.186530323160014, 137.1012295353969819 ) ) ;
#57209 = CARTESIAN_POINT ( 'NONE',  ( 22.05719136570000316, 1509.683314482830156, 226.9345908605980071 ) ) ;
#57210 = SURFACE_STYLE_USAGE ( .BOTH. , #5688 ) ;
#57211 = CARTESIAN_POINT ( 'NONE',  ( -11.27186231780000014, 1414.983773854429955, 195.8113391393980294 ) ) ;
#57212 = CARTESIAN_POINT ( 'NONE',  ( 1.140627099109999820, 1464.949969008629978, 237.1896079457980022 ) ) ;
#57213 = AXIS2_PLACEMENT_3D ( 'NONE', #70420, #104538, #35123 ) ;
#57214 = CARTESIAN_POINT ( 'NONE',  ( 22.19412108519999904, 1411.048331459529891, 215.6222843390580124 ) ) ;
#57215 = DIRECTION ( 'NONE',  ( 0.4826573169212934888, -0.01052729488162659072, -0.8757460193942152582 ) ) ;
#57216 = CARTESIAN_POINT ( 'NONE',  ( -9.792514563870629019, 1462.664719234569930, 228.0127671146719877 ) ) ;
#57217 = CARTESIAN_POINT ( 'NONE',  ( -17.51054297519999992, 1422.888992222730167, 226.4554417862979960 ) ) ;
#57219 = CARTESIAN_POINT ( 'NONE',  ( -2.695375846180000146, 1439.665988598389958, 184.6458907360980106 ) ) ;
#57218 = DIRECTION ( 'NONE',  ( 5.980589973904019347E-17, -1.000000000000000000, 1.736889445713099699E-16 ) ) ;
#57220 = CARTESIAN_POINT ( 'NONE',  ( 28.30907522670739951, 1508.149947046400030, 209.0156582300560331 ) ) ;
#57221 = CARTESIAN_POINT ( 'NONE',  ( -117.5191658986970253, 1358.631207110789092, 297.2777708435188515 ) ) ;
#57222 = CARTESIAN_POINT ( 'NONE',  ( 22.66506344571072162, 1509.725666982945995, 190.0484376440009271 ) ) ;
#57223 = CARTESIAN_POINT ( 'NONE',  ( -1.182106891199999898, 1417.417339269829881, 235.0246372144980000 ) ) ;
#57224 = CARTESIAN_POINT ( 'NONE',  ( -6.561686461364999445, 1517.069378699710114, 205.6695567495270041 ) ) ;
#57225 = CARTESIAN_POINT ( 'NONE',  ( -12.72876562435690140, 1485.205841511860172, 185.8648739181089979 ) ) ;
#57226 = ORIENTED_EDGE ( 'NONE', *, *, #3811, .T. ) ;
#57227 = CARTESIAN_POINT ( 'NONE',  ( -109.1205638390440100, 1384.635319001860125, 311.2541790391259724 ) ) ;
#57228 = CARTESIAN_POINT ( 'NONE',  ( -4.223394594500030408, 1441.589115646509981, 167.1325015425969980 ) ) ;
#57230 = ORIENTED_EDGE ( 'NONE', *, *, #68778, .T. ) ;
#57229 = CARTESIAN_POINT ( 'NONE',  ( -68.43942151631850379, 1379.747151545919905, 280.0290128201230573 ) ) ;
#57231 = EDGE_LOOP ( 'NONE', ( #73351, #69671, #69116, #72797 ) ) ;
#57232 = CARTESIAN_POINT ( 'NONE',  ( -18.00891391817198439, 1424.550919037707899, 228.0707037805817663 ) ) ;
#57233 = ORIENTED_EDGE ( 'NONE', *, *, #50557, .F. ) ;
#57234 = CARTESIAN_POINT ( 'NONE',  ( -1.104917627860029894, 1486.166445081519896, 220.9774509037769974 ) ) ;
#57235 = DIRECTION ( 'NONE',  ( 0.2054769195713296581, -0.000000000000000000, 0.9786619618251632957 ) ) ;
#57237 = CARTESIAN_POINT ( 'NONE',  ( 15.78068549015720201, 1410.430256014650013, 191.5841938278840075 ) ) ;
#57236 = CARTESIAN_POINT ( 'NONE',  ( 2.244413413239999766, 1428.081157166129969, 101.8807690336980016 ) ) ;
#57238 = CARTESIAN_POINT ( 'NONE',  ( 7.726684687535000151, 1517.208444099459939, 210.2479840788170122 ) ) ;
#57239 = CARTESIAN_POINT ( 'NONE',  ( 35.93245376812059533, 1437.277850137440055, 136.5217339136529802 ) ) ;
#57240 = ADVANCED_FACE ( 'NONE', ( #39560 ), #32195, .F. ) ;
#57241 = AXIS2_PLACEMENT_3D ( 'NONE', #8862, #79828, #58736 ) ;
#57242 = CARTESIAN_POINT ( 'NONE',  ( -106.1750857939740058, 1378.913060388029862, 305.7883907182979897 ) ) ;
#57243 = DIRECTION ( 'NONE',  ( -9.066331650111889066E-17, 1.000000000000000000, -7.714096702464409664E-17 ) ) ;
#57245 = ADVANCED_FACE ( 'NONE', ( #4317 ), #90501, .F. ) ;
#57244 = CARTESIAN_POINT ( 'NONE',  ( 17.10909533037560948, 1460.315389741178024, 228.6693725169167521 ) ) ;
#57246 = DIRECTION ( 'NONE',  ( 1.000000000000000000, 0.000000000000000000, 0.000000000000000000 ) ) ;
#57247 = PRODUCT_DEFINITION_SHAPE ( 'NONE', 'NONE',  #61723 ) ;
#57248 = CARTESIAN_POINT ( 'NONE',  ( 34.20278863698899841, 1451.714767517949895, 134.0999999981149813 ) ) ;
#57249 = CARTESIAN_POINT ( 'NONE',  ( -9.849896899200842881, 1512.913060387330006, 185.5490084180013923 ) ) ;
#57250 = ORIENTED_EDGE ( 'NONE', *, *, #57628, .T. ) ;
#57251 = CARTESIAN_POINT ( 'NONE',  ( 22.24401587272570069, 1475.958667601430079, 209.7631782834160106 ) ) ;
#57252 = AXIS2_PLACEMENT_3D ( 'NONE', #63180, #44702, #97286 ) ;
#57253 = CARTESIAN_POINT ( 'NONE',  ( -18.58939038020000112, 1457.838465768930064, 227.5494389216979982 ) ) ;
#57254 = ORIENTED_EDGE ( 'NONE', *, *, #105505, .T. ) ;
#57255 = EDGE_LOOP ( 'NONE', ( #49125, #49237, #107922, #85294 ) ) ;
#57256 = CARTESIAN_POINT ( 'NONE',  ( -7.179127119344999919, 1513.978875661350230, 216.9309098834470149 ) ) ;
#57257 = CARTESIAN_POINT ( 'NONE',  ( -16.63505975150000182, 1409.493969474430060, 194.0661809352979787 ) ) ;
#57258 = CARTESIAN_POINT ( 'NONE',  ( 0.07955197424319999933, 1452.993118421130021, 183.2407363517980343 ) ) ;
#57259 = CARTESIAN_POINT ( 'NONE',  ( -2.330134118790000208, 1515.551704408389924, 212.9514660756190096 ) ) ;
#57260 = CARTESIAN_POINT ( 'NONE',  ( -2.500000000000000000, 1439.569237629489862, 165.5254341707220078 ) ) ;
#57261 = AXIS2_PLACEMENT_3D ( 'NONE', #1882, #60685, #52281 ) ;
#57262 = CARTESIAN_POINT ( 'NONE',  ( -13.84960889600000122, 1379.721631702780087, 208.1907843145939694 ) ) ;
#57263 = EDGE_CURVE ( 'NONE', #12028, #84553, #83213, .T. ) ;
#57264 = CARTESIAN_POINT ( 'NONE',  ( 38.81202643689640297, 1450.612734567539974, 134.7402675994790116 ) ) ;
#57265 = CARTESIAN_POINT ( 'NONE',  ( 17.71193101246160140, 1517.051704408389924, 196.6727161460330251 ) ) ;
#57266 = CARTESIAN_POINT ( 'NONE',  ( 26.25207344680000077, 1438.555629842469898, 137.1352270321980029 ) ) ;
#57267 =( BOUNDED_CURVE ( )  B_SPLINE_CURVE ( 3, ( #94641, #84586, #103599, #17916 ),
 .UNSPECIFIED., .F., .F. ) 
 B_SPLINE_CURVE_WITH_KNOTS ( ( 4, 4 ),
 ( 2.055417531154359878, 2.292695976159725202 ),
 .UNSPECIFIED. ) 
 CURVE ( )  GEOMETRIC_REPRESENTATION_ITEM ( )  RATIONAL_B_SPLINE_CURVE ( ( 1.000000000000000000, 0.9953137455213650897, 0.9953137455213650897, 1.000000000000000000 ) ) 
 REPRESENTATION_ITEM ( '' )  );
#57268 = CARTESIAN_POINT ( 'NONE',  ( 3.954004997530000232, 1416.825421875629900, 190.9202402641980143 ) ) ;
#57269 = CARTESIAN_POINT ( 'NONE',  ( -67.24941355666288700, 1384.719574498639986, 260.0378906380789772 ) ) ;
#57270 = VERTEX_POINT ( 'NONE', #32259 ) ;
#57271 = CARTESIAN_POINT ( 'NONE',  ( 5.778999773775000293, 1516.955859323880077, 201.7887757972170277 ) ) ;
#57272 = CARTESIAN_POINT ( 'NONE',  ( -2.299668004004999933, 1516.965971551240045, 208.0037412025070012 ) ) ;
#57273 = VERTEX_POINT ( 'NONE', #47419 ) ;
#57274 = CARTESIAN_POINT ( 'NONE',  ( 39.56090833897850700, 1440.913060387330006, 266.8640727595400222 ) ) ;
#57275 = CARTESIAN_POINT ( 'NONE',  ( -5.623474965688048840E-07, 1451.660737107639989, 154.0815186765750013 ) ) ;
#57276 = VERTEX_POINT ( 'NONE', #97802 ) ;
#57277 = CARTESIAN_POINT ( 'NONE',  ( -15.12003195112066933, 1522.051704408389924, 218.5174026476448432 ) ) ;
#57278 = CYLINDRICAL_SURFACE ( 'NONE', #5507, 0.9999999999999988898 ) ;
#57279 = CARTESIAN_POINT ( 'NONE',  ( -4.329448776040000446, 1515.064792882589927, 211.4519800877889963 ) ) ;
#57280 = CARTESIAN_POINT ( 'NONE',  ( 8.212347910089999203, 1503.127208973789948, 210.4119479190490267 ) ) ;
#57281 = CARTESIAN_POINT ( 'NONE',  ( -12.83610317870000017, 1419.900230477330069, 222.0779048188979914 ) ) ;
#57282 = DIRECTION ( 'NONE',  ( 0.000000000000000000, -1.000000000000000000, 6.123233995736769734E-17 ) ) ;
#57283 = CARTESIAN_POINT ( 'NONE',  ( -0.7774504691479999785, 1508.162354399930109, 180.6410561175979979 ) ) ;
#57284 = CARTESIAN_POINT ( 'NONE',  ( -13.50121300870000063, 1434.968976328030067, 147.8555663532980020 ) ) ;
#57285 = CARTESIAN_POINT ( 'NONE',  ( 11.73700276280139931, 1426.696010850159837, 144.1682878426319974 ) ) ;
#57287 = FACE_OUTER_BOUND ( 'NONE', #1569, .T. ) ;
#57286 = CARTESIAN_POINT ( 'NONE',  ( 11.98966118179999896, 1463.071801668629860, 231.6035992477980017 ) ) ;
#57288 = CARTESIAN_POINT ( 'NONE',  ( 3.535327679399999923, 1487.160995988090008, 197.6951163675990131 ) ) ;
#57289 = AXIS2_PLACEMENT_3D ( 'NONE', #48223, #5661, #5094 ) ;
#57290 = B_SPLINE_SURFACE_WITH_KNOTS ( 'NONE', 5, 5, ( 
 ( #12184, #29003, #54226, #86689, #35183, #9983 ),
 ( #28446, #53678, #95645, #53111, #45819, #80509 ),
 ( #52555, #18913, #44153, #37399, #103477, #62640 ),
 ( #78289, #88353, #63189, #1603, #11641, #35740 ),
 ( #79952, #54766, #18361, #44713, #79407, #2718 ),
 ( #78865, #26782, #20566, #61518, #46377, #3269 ),
 ( #60970, #71598, #69927, #95095, #104040, #105719 ),
 ( #27332, #87248, #87820, #36286, #36841, #71033 ),
 ( #70478, #96201, #104598, #27892, #62075, #19476 ) ),
 .UNSPECIFIED., .F., .F., .F.,
 ( 6, 3, 6 ),
 ( 6, 6 ),
 ( 3.013370279934989959, 5.176304934450000061, 7.339239588965010164 ),
 ( -1.897240500978929716E-05, 2.000000000000000000 ),
 .UNSPECIFIED. ) ;
#57291 = EDGE_CURVE ( 'NONE', #2313, #75650, #64793, .T. ) ;
#57292 = CARTESIAN_POINT ( 'NONE',  ( -7.717505791104999346, 1516.857914730730045, 216.8393517232070167 ) ) ;
#57293 = ORIENTED_EDGE ( 'NONE', *, *, #4212, .F. ) ;
#57294 = DIRECTION ( 'NONE',  ( 0.000000000000000000, 0.06174578541841399537, -0.9980919085851078787 ) ) ;
#57295 = CARTESIAN_POINT ( 'NONE',  ( -0.1382356955943349897, 1507.743408363169920, 180.7718112797529955 ) ) ;
#57296 = CARTESIAN_POINT ( 'NONE',  ( 5.157704406284129827E-09, 1406.911841301380036, 222.1218459627310153 ) ) ;
#57297 = CARTESIAN_POINT ( 'NONE',  ( 3.267291605165000057, 1516.842852731759876, 212.5687880419470162 ) ) ;
#57298 = CARTESIAN_POINT ( 'NONE',  ( 3.368571795365570054, 1515.551842517600107, 212.9003862705719996 ) ) ;
#57299 = ADVANCED_FACE ( 'NONE', ( #99442 ), #10479, .T. ) ;
#57300 = CARTESIAN_POINT ( 'NONE',  ( 2.344512076345889984, 1516.526058371499857, 216.8306617650070223 ) ) ;
#57302 = VERTEX_POINT ( 'NONE', #85967 ) ;
#57301 = CARTESIAN_POINT ( 'NONE',  ( -12.35342891082190064, 1501.830731195820135, 211.5811800714079993 ) ) ;
#57303 = CIRCLE ( 'NONE', #78690, 1.999999943602009500 ) ;
#57304 = CARTESIAN_POINT ( 'NONE',  ( 23.90675415119999769, 1449.162507167900003, 221.6525748645979945 ) ) ;
#57305 = CARTESIAN_POINT ( 'NONE',  ( -10.96880036559999816, 1432.299257934029811, 151.7701915755980053 ) ) ;
#57306 = DIRECTION ( 'NONE',  ( 1.755985294532469921E-16, -1.000000000000000000, 1.338183447452831989E-16 ) ) ;
#57307 = CARTESIAN_POINT ( 'NONE',  ( -5.010111490926330013, 1441.342207431860061, 201.8184694356190221 ) ) ;
#57308 = DIRECTION ( 'NONE',  ( -1.755985294532469921E-16, 1.000000000000000000, -1.338183447452831989E-16 ) ) ;
#57309 = CARTESIAN_POINT ( 'NONE',  ( -1.906499758064230099E-08, 1508.551704408389924, 201.6218459511669892 ) ) ;
#57310 = CARTESIAN_POINT ( 'NONE',  ( -9.360712814986960950, 1480.861369530930006, 227.8151877844180149 ) ) ;
#57311 = CARTESIAN_POINT ( 'NONE',  ( -21.63676776550000014, 1444.797379379979930, 220.8518329349979865 ) ) ;
#57312 = CARTESIAN_POINT ( 'NONE',  ( -2.695946308289999926, 1485.848501370129952, 182.4462471358980054 ) ) ;
#57313 = ORIENTED_EDGE ( 'NONE', *, *, #100040, .F. ) ;
#57314 = CARTESIAN_POINT ( 'NONE',  ( -2.298048961635000165, 1516.764084769670262, 205.6764383981169715 ) ) ;
#57315 = CARTESIAN_POINT ( 'NONE',  ( 6.156919420700000423, 1406.564961868729824, 269.2805947264979523 ) ) ;
#57316 = CARTESIAN_POINT ( 'NONE',  ( -21.39772323737049931, 1509.704958956720020, 229.7894127843639751 ) ) ;
#57317 = CARTESIAN_POINT ( 'NONE',  ( 10.89207644999670066, 1489.857914366469913, 208.0657199684020213 ) ) ;
#57318 = CARTESIAN_POINT ( 'NONE',  ( 22.91784880816845771, 1432.059886029948530, 216.2703706859424813 ) ) ;
#57319 = CARTESIAN_POINT ( 'NONE',  ( 3.111939779091150271, 1454.307961065650034, 217.9820244081379883 ) ) ;
#57320 = CARTESIAN_POINT ( 'NONE',  ( -15.73574044604409927, 1409.462552572229924, 225.2910003602459881 ) ) ;
#57321 = DIRECTION ( 'NONE',  ( 1.407418274235009893E-17, 1.000000000000000000, -2.576261870300909820E-17 ) ) ;
#57322 = VECTOR ( 'NONE', #15437, 1000.000000000000000 ) ;
#57323 = FACE_OUTER_BOUND ( 'NONE', #62798, .T. ) ;
#57324 = CARTESIAN_POINT ( 'NONE',  ( -11.97778741359999977, 1446.811539678010149, 187.5041641196980038 ) ) ;
#57325 = CARTESIAN_POINT ( 'NONE',  ( 9.722206599239999747, 1428.114070706089933, 212.2005358146490153 ) ) ;
#57326 = DIRECTION ( 'NONE',  ( 1.755985294532469921E-16, -1.000000000000000000, 1.338183447452831989E-16 ) ) ;
#57327 = CARTESIAN_POINT ( 'NONE',  ( -4.217994498519999524, 1515.470302801990101, 209.8638807055999962 ) ) ;
#57328 = VECTOR ( 'NONE', #23146, 999.9999999999998863 ) ;
#57329 = CARTESIAN_POINT ( 'NONE',  ( -9.623804485526918029, 1409.249131045419745, 197.6748203005379878 ) ) ;
#57330 = AXIS2_PLACEMENT_3D ( 'NONE', #22476, #98662, #57246 ) ;
#57331 = DIRECTION ( 'NONE',  ( -5.980589973904019347E-17, 1.000000000000000000, -1.736889445713099699E-16 ) ) ;
#57332 = CARTESIAN_POINT ( 'NONE',  ( 3.116195436109999939, 1441.243535601449821, 166.9150391423980011 ) ) ;
#57333 = CARTESIAN_POINT ( 'NONE',  ( -2.764108551270000103, 1475.699858318429960, 269.0427152816980083 ) ) ;
#57334 = CARTESIAN_POINT ( 'NONE',  ( 3.045280019940000305, 1464.258769156330118, 233.3054829794980094 ) ) ;
#57335 = CARTESIAN_POINT ( 'NONE',  ( -8.178330991719999332, 1439.186084948589951, 206.0664693636589959 ) ) ;
#57336 = CARTESIAN_POINT ( 'NONE',  ( 17.72813534363540100, 1410.891380463280029, 223.4205987578280030 ) ) ;
#57337 = CARTESIAN_POINT ( 'NONE',  ( -49.49141214366390074, 1384.742493838780092, 260.6926740138409855 ) ) ;
#57338 = CARTESIAN_POINT ( 'NONE',  ( -30.47385413848724411, 1525.394081235439444, 221.5015873865095841 ) ) ;
#57339 = VECTOR ( 'NONE', #54759, 999.9999999999998863 ) ;
#57340 = FACE_OUTER_BOUND ( 'NONE', #105196, .T. ) ;
#57341 = CARTESIAN_POINT ( 'NONE',  ( -105.6396896030000079, 1378.913059593480057, 303.5072247312590434 ) ) ;
#57342 = CARTESIAN_POINT ( 'NONE',  ( 31.81429855202634727, 1524.964158026965833, 216.6572713097424128 ) ) ;
#57343 = CARTESIAN_POINT ( 'NONE',  ( 8.480624627922136227, 1511.395873689150676, 204.2487940905495236 ) ) ;
#57344 = CARTESIAN_POINT ( 'NONE',  ( -20.29148499160000085, 1410.117176396729974, 199.0828523262979957 ) ) ;
#57345 = B_SPLINE_CURVE_WITH_KNOTS ( 'NONE', 3,
 ( #79841, #106133, #105032, #87692, #28878, #88236 ),
 .UNSPECIFIED., .F., .F.,
 ( 4, 2, 4 ),
 ( 2.081668171172168513E-17, 0.001087661325621749582, 0.002175322651243478348 ),
 .UNSPECIFIED. ) ;
#57346 = CARTESIAN_POINT ( 'NONE',  ( 12.91341498353999917, 1421.147458452220235, 204.5103631683240337 ) ) ;
#57347 = CARTESIAN_POINT ( 'NONE',  ( -6.597068289630000137, 1407.874253871329756, 270.1316426411979705 ) ) ;
#57348 = VERTEX_POINT ( 'NONE', #101092 ) ;
#57349 = CARTESIAN_POINT ( 'NONE',  ( -7.990695852699508883, 1410.564740250183377, 230.6243468353451078 ) ) ;
#57350 = CARTESIAN_POINT ( 'NONE',  ( -7.481780884509355189, 1510.769285161464495, 215.2273066580793852 ) ) ;
#57351 = CARTESIAN_POINT ( 'NONE',  ( -13.05162051234070120, 1467.538720776440186, 191.8992815354449988 ) ) ;
#57353 = CARTESIAN_POINT ( 'NONE',  ( -14.08980430995099908, 1379.613307177060051, 211.6683369410179978 ) ) ;
#57352 = CARTESIAN_POINT ( 'NONE',  ( 11.60353182090000068, 1425.885547122130220, 141.8419080669979735 ) ) ;
#57354 = CARTESIAN_POINT ( 'NONE',  ( 16.99775931995016620, 1524.964230758899930, 237.0504197537864286 ) ) ;
#57355 = CARTESIAN_POINT ( 'NONE',  ( -124.1574587857000012, 1375.179104070690073, 298.3450194382389782 ) ) ;
#57356 = CARTESIAN_POINT ( 'NONE',  ( 27.42679559861360161, 1448.207338318150050, 136.8613456938669799 ) ) ;
#57357 = AXIS2_PLACEMENT_3D ( 'NONE', #103584, #17903, #27425 ) ;
#57358 = CARTESIAN_POINT ( 'NONE',  ( 4.033653264325000265, 1517.028034847769959, 202.5611037067669997 ) ) ;
#57359 = CARTESIAN_POINT ( 'NONE',  ( 7.517994368920000170, 1425.903866193129943, 212.2671131861389995 ) ) ;
#57360 = CARTESIAN_POINT ( 'NONE',  ( -13.57909981250000087, 1416.568813547830132, 221.8977233994979770 ) ) ;
#57361 = CARTESIAN_POINT ( 'NONE',  ( 15.25940256903500014, 1512.044075975079977, 196.5523931850670181 ) ) ;
#57362 = CARTESIAN_POINT ( 'NONE',  ( -21.60434909035369699, 1417.942671029680014, 208.5651389465070054 ) ) ;
#57363 = CARTESIAN_POINT ( 'NONE',  ( -24.78061434722729928, 1379.805010702669961, 214.9158369873429990 ) ) ;
#57364 = CARTESIAN_POINT ( 'NONE',  ( 20.56174574396830224, 1508.351243507949903, 228.2043451791550126 ) ) ;
#57366 = EDGE_LOOP ( 'NONE', ( #7301, #37476, #103557, #74274, #20976, #5178, #95192, #12185, #17095 ) ) ;
#57365 = CARTESIAN_POINT ( 'NONE',  ( -25.94019285366969996, 1379.613529776539963, 215.4482193062259796 ) ) ;
#57367 = ORIENTED_EDGE ( 'NONE', *, *, #99676, .F. ) ;
#57368 = CARTESIAN_POINT ( 'NONE',  ( -7.841281984380000125, 1397.234782632230008, 219.8176822113979938 ) ) ;
#57369 = CARTESIAN_POINT ( 'NONE',  ( -18.97336374349999844, 1409.575624849130008, 219.6734443658980069 ) ) ;
#57370 = ORIENTED_EDGE ( 'NONE', *, *, #11025, .F. ) ;
#57371 = CARTESIAN_POINT ( 'NONE',  ( -12.98571499817150610, 1444.884868618428754, 169.4235797359238518 ) ) ;
#57372 = CARTESIAN_POINT ( 'NONE',  ( -31.34137657934027388, 1512.187213306747481, 196.3411265156551906 ) ) ;
#57373 = CARTESIAN_POINT ( 'NONE',  ( -7.599119446864999183, 1512.336926113599930, 211.5138630182570125 ) ) ;
#57375 = CARTESIAN_POINT ( 'NONE',  ( -14.25772450459819929, 1509.411936130120012, 183.1493227206160270 ) ) ;
#57374 = CARTESIAN_POINT ( 'NONE',  ( 2.925585596869999527, 1446.021080118789996, 199.8385306598290185 ) ) ;
#57376 = VECTOR ( 'NONE', #42678, 1000.000000000000000 ) ;
#57377 = CARTESIAN_POINT ( 'NONE',  ( 3.333430315160000212, 1468.704004404630041, 183.2171971980980061 ) ) ;
#57378 = CARTESIAN_POINT ( 'NONE',  ( -4.875278699166510243, 1464.496074833199827, 199.2309655485080100 ) ) ;
#57379 = CARTESIAN_POINT ( 'NONE',  ( -17.19445149659999572, 1417.679469902730034, 207.4067394929689954 ) ) ;
#57380 = SURFACE_STYLE_FILL_AREA ( #56251 ) ;
#57381 = CARTESIAN_POINT ( 'NONE',  ( 5.535200594421139542, 1396.106353873259877, 199.5716390489739922 ) ) ;
#57382 = CARTESIAN_POINT ( 'NONE',  ( 0.7692391029780000222, 1415.628674266529742, 190.8565233057979924 ) ) ;
#57383 = CARTESIAN_POINT ( 'NONE',  ( 11.63669227459999966, 1425.864836378729933, 144.1684971660979784 ) ) ;
#57384 = CARTESIAN_POINT ( 'NONE',  ( 6.466214386739325803, 1509.141720294096103, 180.4348274801477316 ) ) ;
#57385 = ORIENTED_EDGE ( 'NONE', *, *, #80132, .F. ) ;
#57386 = CARTESIAN_POINT ( 'NONE',  ( 12.94454588817750107, 1434.758408665909883, 149.3917831800590079 ) ) ;
#57387 = ORIENTED_EDGE ( 'NONE', *, *, #54464, .F. ) ;
#57388 = ORIENTED_EDGE ( 'NONE', *, *, #105951, .F. ) ;
#57389 = CARTESIAN_POINT ( 'NONE',  ( -16.53125420670000167, 1418.541487540729804, 202.7561987471289910 ) ) ;
#57390 = CARTESIAN_POINT ( 'NONE',  ( -8.376976394739999776, 1464.979757639830041, 233.1143827394980121 ) ) ;
#57391 = CARTESIAN_POINT ( 'NONE',  ( -107.8702472922463045, 1389.245402359266791, 309.8450691920539839 ) ) ;
#57392 = CARTESIAN_POINT ( 'NONE',  ( 6.556022194504999234, 1516.833525648419936, 216.0623193043769845 ) ) ;
#57393 = CARTESIAN_POINT ( 'NONE',  ( -12.59193496205820040, 1379.616147050329801, 209.6906596629179944 ) ) ;
#57394 = ORIENTED_EDGE ( 'NONE', *, *, #53523, .F. ) ;
#57395 = DIRECTION ( 'NONE',  ( 0.000000000000000000, -1.000000000000000000, 0.000000000000000000 ) ) ;
#57396 = CARTESIAN_POINT ( 'NONE',  ( -8.998910544736714812, 1424.786834349990158, 213.7129700835037909 ) ) ;
#57397 = CARTESIAN_POINT ( 'NONE',  ( -35.85007572059999603, 1380.172836988449944, 220.5090016197590046 ) ) ;
#57398 = ADVANCED_FACE ( 'NONE', ( #110616 ), #87432, .F. ) ;
#57399 = ORIENTED_EDGE ( 'NONE', *, *, #31524, .F. ) ;
#57400 = CARTESIAN_POINT ( 'NONE',  ( 4.609996581545000360, 1516.769879638719885, 205.6626893540170329 ) ) ;
#57401 = ORIENTED_EDGE ( 'NONE', *, *, #36296, .T. ) ;
#57402 = CARTESIAN_POINT ( 'NONE',  ( -6.556851034704999748, 1516.939568781210028, 209.1335575761840175 ) ) ;
#57403 = CIRCLE ( 'NONE', #39318, 30.13701971169416183 ) ;
#57404 = CARTESIAN_POINT ( 'NONE',  ( -8.320045427150200013, 1452.334357641350152, 204.9523858405019894 ) ) ;
#57405 = EDGE_CURVE ( 'NONE', #4789, #37845, #101877, .T. ) ;
#57406 = CARTESIAN_POINT ( 'NONE',  ( -30.02908938876808875, 1419.599146942571451, 269.4711195632991689 ) ) ;
#57407 = CARTESIAN_POINT ( 'NONE',  ( 6.843878216475000720, 1512.371933174400056, 217.6246419884270153 ) ) ;
#57409 = ORIENTED_EDGE ( 'NONE', *, *, #52057, .T. ) ;
#57408 = CARTESIAN_POINT ( 'NONE',  ( -0.2112786387671690136, 1416.230844595159851, 227.3034699774860030 ) ) ;
#57410 = DIRECTION ( 'NONE',  ( 0.000000000000000000, 1.000000000000000000, 0.000000000000000000 ) ) ;
#57411 = CARTESIAN_POINT ( 'NONE',  ( -34.73433026547840541, 1440.913060388860004, 250.3950812228370353 ) ) ;
#57412 = CARTESIAN_POINT ( 'NONE',  ( -73.55923423229999969, 1384.652831667379814, 298.9494481685590017 ) ) ;
#57413 = CARTESIAN_POINT ( 'NONE',  ( -0.2112467950247060022, 1467.134318679190073, 235.6312670970790180 ) ) ;
#57414 = CARTESIAN_POINT ( 'NONE',  ( 7.260534597404889823, 1410.692748237529941, 269.6205518878410317 ) ) ;
#57415 = CARTESIAN_POINT ( 'NONE',  ( 5.009478067315000338, 1516.886345593249871, 213.7343532441369973 ) ) ;
#57416 = CARTESIAN_POINT ( 'NONE',  ( 24.08125413579999829, 1410.714371472329958, 209.1807164637870073 ) ) ;
#57417 = CARTESIAN_POINT ( 'NONE',  ( -21.07299109810000104, 1509.588070516929974, 188.6993481227979998 ) ) ;
#57418 = FACE_OUTER_BOUND ( 'NONE', #71593, .T. ) ;
#57419 = CARTESIAN_POINT ( 'NONE',  ( -7.708976442096130199, 1516.532192033489991, 211.5084644598540251 ) ) ;
#57420 = CARTESIAN_POINT ( 'NONE',  ( 7.339749335215000059, 1517.224900789629828, 210.8312305431869902 ) ) ;
#57421 = CARTESIAN_POINT ( 'NONE',  ( 9.438883731854119219, 1434.537705308250224, 206.5784376637019761 ) ) ;
#57422 = CARTESIAN_POINT ( 'NONE',  ( 0.07980232208509999148, 1420.214783457930025, 183.9037909274979938 ) ) ;
#57423 = AXIS2_PLACEMENT_3D ( 'NONE', #1349, #58497, #109995 ) ;
#57424 = CARTESIAN_POINT ( 'NONE',  ( -11.64460141611553290, 1486.022579393844580, 184.5329476470979841 ) ) ;
#57426 = ORIENTED_EDGE ( 'NONE', *, *, #92734, .T. ) ;
#57425 = CARTESIAN_POINT ( 'NONE',  ( -58.25011577389999928, 1386.675189637609947, 240.0949551211589892 ) ) ;
#57427 = CARTESIAN_POINT ( 'NONE',  ( -52.23529040485620101, 1385.108628416219972, 266.3036918333839935 ) ) ;
#57428 = CARTESIAN_POINT ( 'NONE',  ( 18.79678650740000023, 1416.830000968129980, 209.8350674583659838 ) ) ;
#57429 = CARTESIAN_POINT ( 'NONE',  ( -4.404634328387945885, 1370.457478306087751, 209.4202803877028600 ) ) ;
#57430 = CIRCLE ( 'NONE', #19826, 1.999999999999999556 ) ;
#57431 = CARTESIAN_POINT ( 'NONE',  ( -12.81872062859999950, 1420.998869512129886, 230.6915806954980042 ) ) ;
#57432 = CARTESIAN_POINT ( 'NONE',  ( -5.519906363166400709, 1440.499855196290127, 154.7645174855159951 ) ) ;
#57433 = CARTESIAN_POINT ( 'NONE',  ( 11.90565451390000007, 1426.735011702260181, 206.1879629638889924 ) ) ;
#57434 = CARTESIAN_POINT ( 'NONE',  ( 0.3863944528677800139, 1452.976072371400051, 183.2761518715429929 ) ) ;
#57435 = AXIS2_PLACEMENT_3D ( 'NONE', #50975, #85653, #43126 ) ;
#57437 = CARTESIAN_POINT ( 'NONE',  ( -7.544964967010000301, 1384.904326039650186, 219.0876571199189868 ) ) ;
#57436 = CARTESIAN_POINT ( 'NONE',  ( 6.942344691835000248, 1516.810037859429940, 216.8380980232070101 ) ) ;
#57438 = FACE_OUTER_BOUND ( 'NONE', #59467, .T. ) ;
#57439 = CARTESIAN_POINT ( 'NONE',  ( 0.3104492304326414986, 1515.598602702714061, 205.0832592253421751 ) ) ;
#57440 = ORIENTED_EDGE ( 'NONE', *, *, #92589, .T. ) ;
#57441 = CARTESIAN_POINT ( 'NONE',  ( -4.618119704395000191, 1516.706638732659940, 202.1845071865270143 ) ) ;
#57442 = CARTESIAN_POINT ( 'NONE',  ( -15.40521419186499941, 1513.907445464710236, 224.1476389979669932 ) ) ;
#57443 = CYLINDRICAL_SURFACE ( 'NONE', #48209, 33.13701971169416538 ) ;
#57444 = CARTESIAN_POINT ( 'NONE',  ( 20.46945555039999931, 1454.918353507129950, 222.9273423791979951 ) ) ;
#57445 = CARTESIAN_POINT ( 'NONE',  ( 7.175204869421878406, 1438.963982221705010, 154.0862487876218836 ) ) ;
#57446 = CARTESIAN_POINT ( 'NONE',  ( 8.390996307492248008, 1424.412614569296466, 195.8273022863984067 ) ) ;
#57447 = CARTESIAN_POINT ( 'NONE',  ( -0.6587146994840009651, 1442.893519126590036, 219.0943606518089837 ) ) ;
#57448 = CARTESIAN_POINT ( 'NONE',  ( 13.48815433605667558, 1419.590937927324376, 228.7311886359687776 ) ) ;
#57449 = VECTOR ( 'NONE', #7567, 1000.000000000000000 ) ;
#57450 = DIRECTION ( 'NONE',  ( -1.755985294532469921E-16, 1.000000000000000000, -1.338183447452831989E-16 ) ) ;
#57451 = CARTESIAN_POINT ( 'NONE',  ( -18.66067488629999715, 1424.984128575629938, 224.8203133075979849 ) ) ;
#57452 = CARTESIAN_POINT ( 'NONE',  ( 1.704192342800000001E-13, 1475.048391919030109, 269.6500679772980220 ) ) ;
#57453 = CARTESIAN_POINT ( 'NONE',  ( -106.6967271639999950, 1389.794052426160079, 299.6927497095589956 ) ) ;
#57454 = DIRECTION ( 'NONE',  ( 3.828568698926946970E-16, 0.000000000000000000, -1.000000000000000000 ) ) ;
#57455 = CARTESIAN_POINT ( 'NONE',  ( 0.003646682923689930148, 1409.082053264339947, 232.6631847236010060 ) ) ;
#57456 = CARTESIAN_POINT ( 'NONE',  ( -28.87437517114842933, 1463.054888223776970, 269.4592160712932127 ) ) ;
#57457 = ORIENTED_EDGE ( 'NONE', *, *, #58975, .F. ) ;
#57458 = DIRECTION ( 'NONE',  ( -5.980589973904019347E-17, 1.000000000000000000, -1.736889445713099699E-16 ) ) ;
#57459 = CARTESIAN_POINT ( 'NONE',  ( 11.66183224573578592, 1506.404057882402867, 190.5056905578398982 ) ) ;
#57460 = CARTESIAN_POINT ( 'NONE',  ( -17.83486663330464950, 1523.678648413191695, 237.8759530894961074 ) ) ;
#57461 = CARTESIAN_POINT ( 'NONE',  ( -0.9786431567949999133, 1497.713060387329961, 231.7156151907979904 ) ) ;
#57462 = CARTESIAN_POINT ( 'NONE',  ( -0.2057087554429999909, 1415.760339075730144, 233.4522620454979744 ) ) ;
#57463 = CARTESIAN_POINT ( 'NONE',  ( -13.13022493104261912, 1443.049912350888235, 186.7023179654335081 ) ) ;
#57464 = CARTESIAN_POINT ( 'NONE',  ( -9.536809216310290438, 1439.025537637410025, 209.1065069698359764 ) ) ;
#57465 = CARTESIAN_POINT ( 'NONE',  ( 1.901515396933940005, 1494.834309937820080, 220.2474388463949992 ) ) ;
#57466 = AXIS2_PLACEMENT_3D ( 'NONE', #39054, #13295, #105748 ) ;
#57467 = CARTESIAN_POINT ( 'NONE',  ( -15.05358279999999915, 1410.831827720429828, 226.7261506157979909 ) ) ;
#57468 = CARTESIAN_POINT ( 'NONE',  ( -107.0308341067140105, 1383.759393728520081, 311.0596185783539340 ) ) ;
#57469 = CARTESIAN_POINT ( 'NONE',  ( 23.92297853920000250, 1435.332916329309910, 136.8723201152980096 ) ) ;
#57470 = CARTESIAN_POINT ( 'NONE',  ( 4.805077557904999352, 1510.399296111369949, 216.6702268425969748 ) ) ;
#57472 = ORIENTED_EDGE ( 'NONE', *, *, #95210, .F. ) ;
#57471 = CARTESIAN_POINT ( 'NONE',  ( -14.54195348929999909, 1410.802016793630173, 226.7659970022979792 ) ) ;
#57473 = CARTESIAN_POINT ( 'NONE',  ( 0.08631495460215440896, 1416.225364278609959, 191.0306605155550130 ) ) ;
#57474 = CARTESIAN_POINT ( 'NONE',  ( -4.049849602479999255, 1409.054484251730173, 230.6815826274979884 ) ) ;
#57475 = ORIENTED_EDGE ( 'NONE', *, *, #5143, .F. ) ;
#57476 = ORIENTED_EDGE ( 'NONE', *, *, #103236, .F. ) ;
#57477 = CARTESIAN_POINT ( 'NONE',  ( -11.42922335639999964, 1500.819224853989908, 209.0445494132570161 ) ) ;
#57478 = CARTESIAN_POINT ( 'NONE',  ( 12.78641131260000030, 1508.670053872629978, 233.6149044717980132 ) ) ;
#57480 = CARTESIAN_POINT ( 'NONE',  ( -21.03384925780000003, 1451.606557712130098, 216.4230814408879837 ) ) ;
#57479 = CARTESIAN_POINT ( 'NONE',  ( -11.60004869885203682, 1428.983126981193436, 134.0999999980979851 ) ) ;
#57481 = CARTESIAN_POINT ( 'NONE',  ( -3.677001408430000229, 1443.877114344990105, 218.5311880179489776 ) ) ;
#57482 = CARTESIAN_POINT ( 'NONE',  ( -11.89654451160000015, 1433.279017673690078, 150.0536589393980194 ) ) ;
#57483 = CYLINDRICAL_SURFACE ( 'NONE', #48131, 3.750000000000000000 ) ;
#57484 = CARTESIAN_POINT ( 'NONE',  ( 9.643555441329038302, 1463.923096898180120, 210.9171137617960028 ) ) ;
#57485 = CARTESIAN_POINT ( 'NONE',  ( -25.67332895650000069, 1437.578766584980031, 137.2860071276980136 ) ) ;
#57486 = CARTESIAN_POINT ( 'NONE',  ( -14.76828617137338284, 1430.034860089873064, 221.9615281545119956 ) ) ;
#57487 = DIRECTION ( 'NONE',  ( 1.000000000000000000, 0.000000000000000000, 0.000000000000000000 ) ) ;
#57488 = CARTESIAN_POINT ( 'NONE',  ( -0.3530891408735000181, 1467.116854267079816, 235.6078141451939985 ) ) ;
#57490 = CARTESIAN_POINT ( 'NONE',  ( 8.257515364769007604, 1363.888049817303681, 210.6218459617142003 ) ) ;
#57489 = B_SPLINE_CURVE_WITH_KNOTS ( 'NONE', 3,
 ( #64300, #98420, #5469, #46403, #39629, #81609 ),
 .UNSPECIFIED., .F., .F.,
 ( 4, 2, 4 ),
 ( 0.000000000000000000, 0.2499786196629087409, 0.4999572393258174818 ),
 .UNSPECIFIED. ) ;
#57491 = CARTESIAN_POINT ( 'NONE',  ( 34.68852446352943986, 1522.382868172864164, 199.9946320047951076 ) ) ;
#57493 = EDGE_LOOP ( 'NONE', ( #11132, #48847, #27552, #63567 ) ) ;
#57492 = CARTESIAN_POINT ( 'NONE',  ( -9.976795219788707390E-10, 1413.055502352579879, 250.5859860138529598 ) ) ;
#57494 = ORIENTED_EDGE ( 'NONE', *, *, #89809, .T. ) ;
#57495 = CARTESIAN_POINT ( 'NONE',  ( -11.73709356416840066, 1426.695943276110029, 144.1748013770919954 ) ) ;
#57496 = CARTESIAN_POINT ( 'NONE',  ( -0.2450088331967839872, 1500.853325256900007, 233.1959501652279982 ) ) ;
#57497 = CARTESIAN_POINT ( 'NONE',  ( -3.437536580710000234, 1471.945857284229987, 270.0719186626980104 ) ) ;
#57498 = CARTESIAN_POINT ( 'NONE',  ( -2.413383470617591620, 1474.356824845931897, 219.0989264923542521 ) ) ;
#57500 = AXIS2_PLACEMENT_3D ( 'NONE', #41543, #101970, #58895 ) ;
#57499 = CARTESIAN_POINT ( 'NONE',  ( -130.5852908491499136, 1331.448250124730293, 321.4071368064091985 ) ) ;
#57501 = CARTESIAN_POINT ( 'NONE',  ( 3.614223185718036913, 1512.187213306747481, 237.6097657867469195 ) ) ;
#57502 = CARTESIAN_POINT ( 'NONE',  ( 0.4151546846821903003, 1512.187213306747481, 244.9330574173806951 ) ) ;
#57503 = CARTESIAN_POINT ( 'NONE',  ( -8.602588863709998535, 1384.842044605820092, 199.8691280033089868 ) ) ;
#57504 = LINE ( 'NONE', #108433, #61013 ) ;
#57505 = CARTESIAN_POINT ( 'NONE',  ( -3.542891930950000212, 1457.744368643689995, 218.3958059026789726 ) ) ;
#57506 = CARTESIAN_POINT ( 'NONE',  ( 10.53407823797624232, 1366.566494964519279, 207.6218459616987673 ) ) ;
#57507 = CARTESIAN_POINT ( 'NONE',  ( -29.09911720097530008, 1413.508132907530126, 267.4910557585119477 ) ) ;
#57508 = ORIENTED_EDGE ( 'NONE', *, *, #26859, .T. ) ;
#57509 = CARTESIAN_POINT ( 'NONE',  ( -4.329294185584100063, 1515.070696454100016, 210.6909417500819757 ) ) ;
#57510 = VERTEX_POINT ( 'NONE', #90360 ) ;
#57511 = ORIENTED_EDGE ( 'NONE', *, *, #60329, .F. ) ;
#57512 = CARTESIAN_POINT ( 'NONE',  ( -7.321455911854999776, 1516.545806094630279, 211.6076919691270177 ) ) ;
#57513 = AXIS2_PLACEMENT_3D ( 'NONE', #81958, #97127, #12566 ) ;
#57514 = CARTESIAN_POINT ( 'NONE',  ( 4.636884161006338267, 1423.705390323189931, 183.8726706823395887 ) ) ;
#57515 = CARTESIAN_POINT ( 'NONE',  ( 40.87172354942210006, 1444.180909089139959, 136.9416239419680039 ) ) ;
#57517 = CARTESIAN_POINT ( 'NONE',  ( -17.64826220104147581, 1419.426078558765312, 207.1977041188345083 ) ) ;
#57516 = CARTESIAN_POINT ( 'NONE',  ( 6.561686423234999843, 1517.069378699710114, 212.5741351528070027 ) ) ;
#57518 = CARTESIAN_POINT ( 'NONE',  ( -17.33962123819999945, 1455.455747421229944, 189.9678388033980241 ) ) ;
#57519 = CARTESIAN_POINT ( 'NONE',  ( -2.500000000000000000, 1448.894380913990062, 183.1110264324979937 ) ) ;
#57520 = ORIENTED_EDGE ( 'NONE', *, *, #15359, .T. ) ;
#57521 = CARTESIAN_POINT ( 'NONE',  ( -26.49667341909999863, 1436.410274429069887, 136.7318106552980055 ) ) ;
#57522 = CARTESIAN_POINT ( 'NONE',  ( 2.870951667784999994, 1517.111322026010157, 202.5592101095969895 ) ) ;
#57523 = AXIS2_PLACEMENT_3D ( 'NONE', #70983, #48932, #21471 ) ;
#57524 = EDGE_CURVE ( 'NONE', #46347, #33692, #32500, .T. ) ;
#57525 = LINE ( 'NONE', #83800, #94564 ) ;
#57526 = CARTESIAN_POINT ( 'NONE',  ( 0.2333221319680495176, 1508.978111603873231, 238.8758415329143645 ) ) ;
#57527 = CARTESIAN_POINT ( 'NONE',  ( -42.28242670489790100, 1436.141010253410059, 269.8809773090360409 ) ) ;
#57528 = PLANE ( 'NONE',  #41827 ) ;
#57529 = CARTESIAN_POINT ( 'NONE',  ( -4.911963663459999907, 1396.617948295830047, 197.5941244856979893 ) ) ;
#57531 = ORIENTED_EDGE ( 'NONE', *, *, #35735, .F. ) ;
#57530 = CARTESIAN_POINT ( 'NONE',  ( 30.87201549882245644, 1524.816548299036640, 196.4947534715130644 ) ) ;
#57532 = ORIENTED_EDGE ( 'NONE', *, *, #33087, .F. ) ;
#57533 = CARTESIAN_POINT ( 'NONE',  ( 0.3241978586559999820, 1451.160671602629918, 182.5582981364979958 ) ) ;
#57534 = CARTESIAN_POINT ( 'NONE',  ( 22.50300749498944342, 1470.712031562941547, 269.4864744541472987 ) ) ;
#57535 = CARTESIAN_POINT ( 'NONE',  ( 1.842963219480119985, 1515.064792700640055, 213.4512947425059792 ) ) ;
#57536 = CARTESIAN_POINT ( 'NONE',  ( -24.93017278910000201, 1436.287966887830180, 137.8924530763979988 ) ) ;
#57537 = CARTESIAN_POINT ( 'NONE',  ( -0.5825634934640000484, 1486.373388144130104, 181.7400882333980121 ) ) ;
#57538 = CARTESIAN_POINT ( 'NONE',  ( 4.625359524845000792, 1517.025470194390209, 211.6020329869469947 ) ) ;
#57539 = AXIS2_PLACEMENT_3D ( 'NONE', #7417, #57308, #16341 ) ;
#57540 = CARTESIAN_POINT ( 'NONE',  ( 6.042571514009714484, 1460.034219164688011, 201.6114123766374462 ) ) ;
#57541 = CARTESIAN_POINT ( 'NONE',  ( 4.500000000000000000, 1411.429641636930000, 146.1721969590979882 ) ) ;
#57542 = CARTESIAN_POINT ( 'NONE',  ( 7.994156842015020636, 1438.386042044900250, 214.3897529291720048 ) ) ;
#57543 = CARTESIAN_POINT ( 'NONE',  ( 11.36018332919999985, 1414.996444518330009, 222.2791104509979903 ) ) ;
#57544 = CARTESIAN_POINT ( 'NONE',  ( 7.888956567984999779, 1511.220390575160081, 204.2953674491570268 ) ) ;
#57545 = CARTESIAN_POINT ( 'NONE',  ( -2.494758036134999912, 1516.937508036699910, 207.4208181092269854 ) ) ;
#57546 = ORIENTED_EDGE ( 'NONE', *, *, #20664, .T. ) ;
#57547 = PLANE ( 'NONE',  #84871 ) ;
#57548 = CARTESIAN_POINT ( 'NONE',  ( -8.809027987900540424, 1438.685400005079828, 208.2563316356740017 ) ) ;
#57549 = CARTESIAN_POINT ( 'NONE',  ( -19.63352108752347291, 1457.018114316206947, 225.8333846437924421 ) ) ;
#57550 = ORIENTED_EDGE ( 'NONE', *, *, #55672, .T. ) ;
#57551 = CARTESIAN_POINT ( 'NONE',  ( -2.857353854284550021, 1525.661275128775742, 241.0960500474518255 ) ) ;
#57552 = CARTESIAN_POINT ( 'NONE',  ( -23.60843796118631488, 1509.747304671633628, 226.8699424759173269 ) ) ;
#57553 = CARTESIAN_POINT ( 'NONE',  ( -4.115381908448215498, 1440.053995635950969, 185.4419112703371013 ) ) ;
#57554 = LINE ( 'NONE', #91677, #12757 ) ;
#57555 = DIRECTION ( 'NONE',  ( -5.980589973904019347E-17, 1.000000000000000000, -1.736889445713099699E-16 ) ) ;
#57556 = CARTESIAN_POINT ( 'NONE',  ( 3.615556770349780180, 1450.594495358166796, 184.1047078091952471 ) ) ;
#57557 = CARTESIAN_POINT ( 'NONE',  ( 6.340491506960000301, 1486.594081419090116, 200.3538830581090053 ) ) ;
#57558 = CARTESIAN_POINT ( 'NONE',  ( -13.10606021074817029, 1522.051704408389924, 192.4222450282478292 ) ) ;
#57559 = CARTESIAN_POINT ( 'NONE',  ( 23.25291252615955884, 1449.806690063141104, 217.4642867579325411 ) ) ;
#57560 = EDGE_CURVE ( 'NONE', #50150, #9923, #75251, .T. ) ;
#57561 = DIRECTION ( 'NONE',  ( 0.9993902469228813645, -0.03489947646212200605, -0.001077449809515390556 ) ) ;
#57562 = CARTESIAN_POINT ( 'NONE',  ( -7.500000019064997581, 1516.051704408390151, 209.1218459511669892 ) ) ;
#57563 = CARTESIAN_POINT ( 'NONE',  ( -6.552897405075000847, 1516.858146885269889, 215.6784973415170157 ) ) ;
#57564 = ORIENTED_EDGE ( 'NONE', *, *, #51073, .T. ) ;
#57565 = CARTESIAN_POINT ( 'NONE',  ( 7.714629857204999830, 1516.748088702300038, 208.4722268118290174 ) ) ;
#57566 = CARTESIAN_POINT ( 'NONE',  ( -13.58968549449999941, 1472.672770405929896, 270.0972160539979541 ) ) ;
#57567 = CARTESIAN_POINT ( 'NONE',  ( 1.326685568770000101, 1419.628109660430027, 184.8664938030979954 ) ) ;
#57568 = CARTESIAN_POINT ( 'NONE',  ( -8.320723051859999941, 1424.406562835429895, 91.09139192869778867 ) ) ;
#57569 = DIRECTION ( 'NONE',  ( -0.9125304618754027652, 0.000000000000000000, -0.4090087482554184417 ) ) ;
#57570 = CARTESIAN_POINT ( 'NONE',  ( 0.6932908832194439874, 1423.656777452399865, 191.1977553446599813 ) ) ;
#57571 = CARTESIAN_POINT ( 'NONE',  ( -31.50799703744288749, 1526.382868172863937, 201.8203724569134749 ) ) ;
#57572 = CARTESIAN_POINT ( 'NONE',  ( -3.990972504867622117, 1508.152871093448766, 220.6701910291383797 ) ) ;
#57573 = CARTESIAN_POINT ( 'NONE',  ( 17.37532935126821698, 1422.700099411153360, 226.5752429006997204 ) ) ;
#57574 = CARTESIAN_POINT ( 'NONE',  ( 0.07025850623888389712, 1455.755685241430001, 198.5793256795659829 ) ) ;
#57575 = CARTESIAN_POINT ( 'NONE',  ( -4.270716396233116718, 1515.320037055801777, 210.9648094544856178 ) ) ;
#57576 = CARTESIAN_POINT ( 'NONE',  ( 35.42325710281800610, 1440.913060386559891, 251.7637193835429628 ) ) ;
#57578 = CARTESIAN_POINT ( 'NONE',  ( 4.327403558811209194, 1515.142896577510101, 208.5979656133399942 ) ) ;
#57577 = CARTESIAN_POINT ( 'NONE',  ( -11.25747325112660135, 1470.382999096749927, 210.8897107907189934 ) ) ;
#57579 = CARTESIAN_POINT ( 'NONE',  ( 13.02791634859999803, 1419.893455390129930, 221.8345185033979874 ) ) ;
#57580 = ORIENTED_EDGE ( 'NONE', *, *, #990, .T. ) ;
#57581 = EDGE_LOOP ( 'NONE', ( #60860, #83869, #106809, #49124, #17962, #64936 ) ) ;
#57582 = CARTESIAN_POINT ( 'NONE',  ( 8.565021413077344548, 1438.455202895904222, 210.8457856774827803 ) ) ;
#57583 = FACE_OUTER_BOUND ( 'NONE', #103037, .T. ) ;
#57584 = TOROIDAL_SURFACE ( 'NONE', #32303, 1.000000000000000000, 1.000000000000000000 ) ;
#57585 = CARTESIAN_POINT ( 'NONE',  ( -5.303263976000000213, 1442.879268891389984, 200.5942805944989971 ) ) ;
#57586 = CARTESIAN_POINT ( 'NONE',  ( 8.228876175890000866, 1424.472806264060182, 195.8277277863990093 ) ) ;
#57587 = B_SPLINE_CURVE_WITH_KNOTS ( 'NONE', 5,
 ( #91693, #14969, #102290, #93339, #32881, #101177 ),
 .UNSPECIFIED., .F., .F.,
 ( 6, 6 ),
 ( 496.9173868270000298, 501.6444997780000108 ),
 .UNSPECIFIED. ) ;
#57588 = CARTESIAN_POINT ( 'NONE',  ( -2197.008826411130485, 11216.44053380570767, 1944.533671213028583 ) ) ;
#57589 = CARTESIAN_POINT ( 'NONE',  ( 21.51466898170138720, 1509.781121651418061, 230.0944450856692640 ) ) ;
#57590 = CARTESIAN_POINT ( 'NONE',  ( -5.389719915088219793, 1440.971386074470047, 154.8246291213590098 ) ) ;
#57591 = CARTESIAN_POINT ( 'NONE',  ( -51.92790261707470023, 1383.808767396460098, 265.2969453248350078 ) ) ;
#57592 = EDGE_CURVE ( 'NONE', #43913, #94111, #19195, .T. ) ;
#57593 = CARTESIAN_POINT ( 'NONE',  ( -5.399591335754999832, 1511.369014903080142, 201.1386261152769919 ) ) ;
#57594 = EDGE_CURVE ( 'NONE', #104584, #64002, #92031, .T. ) ;
#57595 = DIRECTION ( 'NONE',  ( 0.8529498740721102035, 0.5214612423255851059, 0.02355175306912486027 ) ) ;
#57597 =( BOUNDED_SURFACE ( )  B_SPLINE_SURFACE ( 3, 2, ( 
 ( #14408, #74361, #81076 ),
 ( #4392, #106821, #108489 ),
 ( #30112, #21699, #55904 ),
 ( #2032, #34934, #103806 ) ),
 .UNSPECIFIED., .F., .F., .T. ) 
 B_SPLINE_SURFACE_WITH_KNOTS ( ( 4, 4 ),
 ( 3, 3 ),
 ( 0.000000000000000000, 0.0002960034161023845684 ),
 ( 0.000000000000000000, 1.000000000000000000 ),
 .UNSPECIFIED. ) 
 GEOMETRIC_REPRESENTATION_ITEM ( )  RATIONAL_B_SPLINE_SURFACE ( (
 ( 1.000000000000000000, 0.8072480644198078981, 1.000000000000000000),
 ( 1.000000000000000000, 0.8072480346917859650, 1.000000000000000000),
 ( 1.000000000000000000, 0.8071723757218217665, 1.000000000000000000),
 ( 1.000000000000000000, 0.8070209408750090851, 1.000000000000000000) ) ) 
 REPRESENTATION_ITEM ( '' )  SURFACE ( )  );
#57596 = CARTESIAN_POINT ( 'NONE',  ( -12.49544828328139978, 1502.589285090969952, 208.9951533569199853 ) ) ;
#57598 = CARTESIAN_POINT ( 'NONE',  ( 11.40015074134580075, 1491.987826722599948, 210.4762200410769992 ) ) ;
#57599 = EDGE_CURVE ( 'NONE', #23656, #21237, #101507, .T. ) ;
#57601 = EDGE_LOOP ( 'NONE', ( #53762, #100038, #34670, #64241, #60310, #51478 ) ) ;
#57600 = CARTESIAN_POINT ( 'NONE',  ( -3.179033953939999879, 1457.997354107289993, 219.3203918675989996 ) ) ;
#57602 = CARTESIAN_POINT ( 'NONE',  ( 4.873735476160000246, 1472.089320948289924, 218.0431589096889695 ) ) ;
#57603 = AXIS2_PLACEMENT_3D ( 'NONE', #51086, #146, #52743 ) ;
#57604 = B_SPLINE_CURVE_WITH_KNOTS ( 'NONE', 5,
 ( #93715, #92626, #51756, #93177, #16447, #84228, #84773, #263, #78042 ),
 .UNSPECIFIED., .F., .F.,
 ( 6, 3, 6 ),
 ( -13.00939335640000039, -6.504696678220000194, 0.000000000000000000 ),
 .UNSPECIFIED. ) ;
#57605 = CARTESIAN_POINT ( 'NONE',  ( -22.76979002380000239, 1383.850662563309925, 221.8906633995589743 ) ) ;
#57606 = ADVANCED_FACE ( 'NONE', ( #78407 ), #49495, .F. ) ;
#57607 = CARTESIAN_POINT ( 'NONE',  ( 4.804127539630909105, 1508.551704408389924, 205.6959211417370170 ) ) ;
#57608 = ORIENTED_EDGE ( 'NONE', *, *, #74787, .F. ) ;
#57609 = ORIENTED_EDGE ( 'NONE', *, *, #50453, .F. ) ;
#57610 = ADVANCED_FACE ( 'NONE', ( #35858 ), #16394, .F. ) ;
#57611 = CARTESIAN_POINT ( 'NONE',  ( -4.138326088228239996, 1515.492270357839971, 206.7919250756299903 ) ) ;
#57613 = DIRECTION ( 'NONE',  ( 0.5969061220947440294, -0.8023110876747339137, 0.000000000000000000 ) ) ;
#57612 = CARTESIAN_POINT ( 'NONE',  ( -11.87908931286030167, 1481.928125358580019, 208.8953011241800084 ) ) ;
#57615 = EDGE_CURVE ( 'NONE', #61659, #64952, #18961, .T. ) ;
#57614 = CARTESIAN_POINT ( 'NONE',  ( 11.77367730374300159, 1479.442738960109864, 208.9990535504570062 ) ) ;
#57616 = B_SPLINE_CURVE_WITH_KNOTS ( 'NONE', 3,
 ( #23619, #79889, #30009, #11575 ),
 .UNSPECIFIED., .F., .F.,
 ( 4, 4 ),
 ( 0.000000000000000000, 0.0002220129587134777476 ),
 .UNSPECIFIED. ) ;
#57617 = CARTESIAN_POINT ( 'NONE',  ( -105.3098427040000047, 1380.581413796420065, 300.2387618876589954 ) ) ;
#57618 = CARTESIAN_POINT ( 'NONE',  ( -15.16921353568702102, 1420.050152274720858, 212.3982990353912328 ) ) ;
#57619 = FACE_OUTER_BOUND ( 'NONE', #78087, .T. ) ;
#57620 = CARTESIAN_POINT ( 'NONE',  ( 7.365073210101819257, 1409.170254411169935, 196.0898092898519849 ) ) ;
#57621 = CARTESIAN_POINT ( 'NONE',  ( 18.03147918629399982, 1424.668369977461907, 225.2961251598460137 ) ) ;
#57622 = CARTESIAN_POINT ( 'NONE',  ( -109.1450416020000063, 1385.242479493820156, 297.1468691531589457 ) ) ;
#57623 = CARTESIAN_POINT ( 'NONE',  ( 11.86629849080000021, 1432.349867597399907, 149.9824147457980246 ) ) ;
#57624 = AXIS2_PLACEMENT_3D ( 'NONE', #59911, #34682, #97345 ) ;
#57625 = CARTESIAN_POINT ( 'NONE',  ( -3.768408416969716068, 1424.792709689574167, 185.8089501202686904 ) ) ;
#57626 = ORIENTED_EDGE ( 'NONE', *, *, #5898, .T. ) ;
#57628 = EDGE_CURVE ( 'NONE', #5019, #27860, #7072, .T. ) ;
#57627 = CARTESIAN_POINT ( 'NONE',  ( -1.613214857710000061, 1426.534415841129885, 146.0564723340980038 ) ) ;
#57629 = CARTESIAN_POINT ( 'NONE',  ( 18.94445953561779916, 1457.057774993960038, 226.8190492099999744 ) ) ;
#57630 = CIRCLE ( 'NONE', #9328, 2.000000000000003553 ) ;
#57631 = CARTESIAN_POINT ( 'NONE',  ( -12.21221065219999957, 1435.118595363520171, 151.0037181377979891 ) ) ;
#57632 = CARTESIAN_POINT ( 'NONE',  ( -8.040235583480250031E-10, 1467.681589800659822, 247.2443817431000070 ) ) ;
#57633 = DIRECTION ( 'NONE',  ( -1.755985294532469921E-16, 1.000000000000000000, -1.338183447452831989E-16 ) ) ;
#57634 = CARTESIAN_POINT ( 'NONE',  ( 31.32995031131189378, 1523.678648413191695, 196.3423562208913324 ) ) ;
#57635 = CARTESIAN_POINT ( 'NONE',  ( -109.7841757200000075, 1385.685848889800127, 311.3436617802590263 ) ) ;
#57636 = EDGE_CURVE ( 'NONE', #75664, #67655, #50045, .T. ) ;
#57637 = FACE_OUTER_BOUND ( 'NONE', #12044, .T. ) ;
#57638 = CARTESIAN_POINT ( 'NONE',  ( -10.08466507605109719, 1362.620900815653613, 207.6218459616987673 ) ) ;
#57639 = CARTESIAN_POINT ( 'NONE',  ( 3.406450987864870328, 1507.508084575899829, 220.3277226881679951 ) ) ;
#57640 = CARTESIAN_POINT ( 'NONE',  ( 3.959152859930000101, 1428.396642669490120, 216.3690266601789745 ) ) ;
#57641 = CARTESIAN_POINT ( 'NONE',  ( -3.648559762950000174, 1443.531551953690041, 199.7293442341890000 ) ) ;
#57642 = EDGE_CURVE ( 'NONE', #13824, #50505, #78620, .T. ) ;
#57643 = CARTESIAN_POINT ( 'NONE',  ( 4.612671339784999880, 1516.783665406140017, 208.3654117178780041 ) ) ;
#57644 = CARTESIAN_POINT ( 'NONE',  ( 1.398757667669989990, 1408.961906081389998, 223.8083846529389973 ) ) ;
#57645 = CARTESIAN_POINT ( 'NONE',  ( 29.00779973304118542, 1526.382868172864164, 200.9494832830835378 ) ) ;
#57646 = CARTESIAN_POINT ( 'NONE',  ( -14.46232908324019917, 1379.641877967650089, 208.1640365550420029 ) ) ;
#57647 = CARTESIAN_POINT ( 'NONE',  ( 7.506537366674529643, 1425.371641708889911, 212.2338419592690002 ) ) ;
#57648 = EDGE_CURVE ( 'NONE', #105791, #2110, #58953, .T. ) ;
#57649 = ORIENTED_EDGE ( 'NONE', *, *, #72947, .T. ) ;
#57650 = CARTESIAN_POINT ( 'NONE',  ( 25.15583052659999908, 1440.913060404589942, 217.2951523031179875 ) ) ;
#57651 = CARTESIAN_POINT ( 'NONE',  ( -27.95183976699999917, 1508.132394783229984, 207.1324980664579982 ) ) ;
#57653 = CARTESIAN_POINT ( 'NONE',  ( -2.121003584631406813, 1512.187213306747481, 239.6750300321239138 ) ) ;
#57652 = CARTESIAN_POINT ( 'NONE',  ( -3.536030895419999709, 1494.220633993530100, 181.5266943534980157 ) ) ;
#57654 = CARTESIAN_POINT ( 'NONE',  ( -2.050401568548840370, 1419.506371351020107, 185.8591288081520077 ) ) ;
#57655 = CARTESIAN_POINT ( 'NONE',  ( -22.53454638039999836, 1427.366758238030116, 231.7401250235980115 ) ) ;
#57656 = CARTESIAN_POINT ( 'NONE',  ( -29.52155729519625638, 1509.963968224940345, 206.5808354184737254 ) ) ;
#57657 = CARTESIAN_POINT ( 'NONE',  ( -16.66634793421699712, 1452.331058692820079, 146.5832199163500036 ) ) ;
#57658 = CARTESIAN_POINT ( 'NONE',  ( 27.86016249569999914, 1451.782569911029896, 135.7658021331980081 ) ) ;
#57659 = ORIENTED_EDGE ( 'NONE', *, *, #81221, .T. ) ;
#57660 = DIRECTION ( 'NONE',  ( -1.000000000000000000, 0.000000000000000000, 0.000000000000000000 ) ) ;
#57661 = CARTESIAN_POINT ( 'NONE',  ( 6.167425625146620593E-05, 1410.034441586050207, 269.8654409432670036 ) ) ;
#57662 = CARTESIAN_POINT ( 'NONE',  ( 14.47776787345340033, 1421.911392191610048, 229.8149983301250074 ) ) ;
#57663 = CARTESIAN_POINT ( 'NONE',  ( -17.73406580063780069, 1423.343214054229975, 226.1884525926029994 ) ) ;
#57664 = ORIENTED_EDGE ( 'NONE', *, *, #35036, .F. ) ;
#57665 = VERTEX_POINT ( 'NONE', #7472 ) ;
#57666 = CARTESIAN_POINT ( 'NONE',  ( -46.07807520840000137, 1384.601971911739838, 219.0368719419589922 ) ) ;
#57667 = CARTESIAN_POINT ( 'NONE',  ( -23.03199747460190139, 1409.747173909519915, 209.2136270135010250 ) ) ;
#57668 = CARTESIAN_POINT ( 'NONE',  ( -3.853475927979999938, 1424.036818987829975, 184.7819380313979991 ) ) ;
#57669 = CARTESIAN_POINT ( 'NONE',  ( 3.822989240696690327, 1508.729442775010057, 204.5649349260539793 ) ) ;
#57670 = CARTESIAN_POINT ( 'NONE',  ( -10.10023367162169983, 1517.051704408389924, 185.1638560673330005 ) ) ;
#57671 = CARTESIAN_POINT ( 'NONE',  ( -22.69601814784311955, 1436.519530016244289, 142.0928716636521472 ) ) ;
#57672 = ADVANCED_FACE ( 'NONE', ( #109941 ), #33219, .F. ) ;
#57673 = CARTESIAN_POINT ( 'NONE',  ( 4.410752497883399847, 1508.610338626970133, 212.9872707138450210 ) ) ;
#57674 = CARTESIAN_POINT ( 'NONE',  ( 41.87330120854969806, 1455.441274400750217, 268.6302085777389834 ) ) ;
#57675 = CARTESIAN_POINT ( 'NONE',  ( -4.668116808335850187, 1508.551704407329908, 204.7884564220910022 ) ) ;
#57676 = ADVANCED_FACE ( 'NONE', ( #42186 ), #76336, .T. ) ;
#57677 = CARTESIAN_POINT ( 'NONE',  ( -0.01077498392880000058, 1420.442501270029879, 183.2891594270980136 ) ) ;
#57678 = CARTESIAN_POINT ( 'NONE',  ( -6.560742263465000335, 1517.028034847769959, 205.0881926677770082 ) ) ;
#57679 = ORIENTED_EDGE ( 'NONE', *, *, #74922, .F. ) ;
#57680 = CARTESIAN_POINT ( 'NONE',  ( -3.220674668504990290, 1433.265634988960073, 218.1214075394389909 ) ) ;
#57681 = CARTESIAN_POINT ( 'NONE',  ( 15.27803604049760011, 1512.526687531830021, 195.8825387542129874 ) ) ;
#57682 = CARTESIAN_POINT ( 'NONE',  ( 7.605328049712762883, 1479.456294567033865, 201.8411987916495889 ) ) ;
#57683 = VERTEX_POINT ( 'NONE', #63290 ) ;
#57684 = CARTESIAN_POINT ( 'NONE',  ( -10.47977169157950073, 1480.135362529120130, 210.0653170854480152 ) ) ;
#57685 = CARTESIAN_POINT ( 'NONE',  ( 26.81776656861889663, 1451.507007085510168, 136.0705416397969998 ) ) ;
#57686 = CARTESIAN_POINT ( 'NONE',  ( -13.77006425889850050, 1512.900351074040145, 193.8161084199589936 ) ) ;
#57687 = CARTESIAN_POINT ( 'NONE',  ( 9.054615469453679566, 1503.552526581200027, 218.0929084609520032 ) ) ;
#57688 = CARTESIAN_POINT ( 'NONE',  ( 7.403717961100000799, 1422.895866474680133, 195.5966881380989832 ) ) ;
#57689 = CARTESIAN_POINT ( 'NONE',  ( 22.50003437009999629, 1409.698778901130254, 210.1517532643880202 ) ) ;
#57690 = CARTESIAN_POINT ( 'NONE',  ( -8.429455138962469007, 1493.667170337469997, 200.1551273359310130 ) ) ;
#57691 = CARTESIAN_POINT ( 'NONE',  ( 10.03076429248900148, 1480.391079390540199, 205.9105066912069617 ) ) ;
#57692 = CARTESIAN_POINT ( 'NONE',  ( 2.084502382137720211, 1408.985852814510054, 186.9511601598070172 ) ) ;
#57694 = DIRECTION ( 'NONE',  ( 4.657277648632380671E-10, -1.836970198721029688E-16, -1.000000000000000000 ) ) ;
#57693 = CARTESIAN_POINT ( 'NONE',  ( -16.74159367139499821, 1413.343547140530063, 191.6682803937200106 ) ) ;
#57695 = CARTESIAN_POINT ( 'NONE',  ( 2.499999999999999556, 1439.922972988470519, 170.5265280345823840 ) ) ;
#57696 = ADVANCED_FACE ( 'NONE', ( #97404 ), #39365, .T. ) ;
#57697 = CARTESIAN_POINT ( 'NONE',  ( -13.25845773799999883, 1379.879620654849987, 213.4412146779690147 ) ) ;
#57698 = FACE_OUTER_BOUND ( 'NONE', #47302, .T. ) ;
#57699 = ORIENTED_EDGE ( 'NONE', *, *, #261, .F. ) ;
#57700 = CARTESIAN_POINT ( 'NONE',  ( 9.145222436810001909, 1428.303966710129998, 214.3676144192479853 ) ) ;
#57701 = TOROIDAL_SURFACE ( 'NONE', #52349, 30.13701971169416538, 3.000000000000000000 ) ;
#57702 = CARTESIAN_POINT ( 'NONE',  ( 31.41104781486818354, 1511.187213306747708, 202.3296363711535264 ) ) ;
#57703 = CARTESIAN_POINT ( 'NONE',  ( 19.96892221239929910, 1487.423719650039857, 226.6548282969219770 ) ) ;
#57704 = CARTESIAN_POINT ( 'NONE',  ( -9.369334600000000179, 1386.273946184829811, 200.2255685364590079 ) ) ;
#57705 = CARTESIAN_POINT ( 'NONE',  ( 9.089240498862510620, 1424.967503372909960, 209.7705479972250089 ) ) ;
#57706 = CARTESIAN_POINT ( 'NONE',  ( 11.73306708689199951, 1421.776606475200197, 203.4167027637400338 ) ) ;
#57707 = LINE ( 'NONE', #92366, #20902 ) ;
#57708 = CARTESIAN_POINT ( 'NONE',  ( -36.99165393020000181, 1454.692295987030093, 268.3665355201979992 ) ) ;
#57709 = EDGE_CURVE ( 'NONE', #71433, #91018, #7147, .T. ) ;
#57710 = CARTESIAN_POINT ( 'NONE',  ( -14.35456885730000032, 1416.827520116029973, 221.5785008559980156 ) ) ;
#57711 = DIRECTION ( 'NONE',  ( -0.6736849260863841948, 0.000000000000000000, 0.7390186874254148774 ) ) ;
#57712 = CARTESIAN_POINT ( 'NONE',  ( 2.220446049249999903E-15, 1468.063065667029832, 262.6648722463980334 ) ) ;
#57713 = CARTESIAN_POINT ( 'NONE',  ( -16.33500296837753041, 1517.051704408389924, 204.2067034917001536 ) ) ;
#57714 = CARTESIAN_POINT ( 'NONE',  ( -11.60004869885203860, 1428.965959225140750, 137.0999999980979851 ) ) ;
#57715 = EDGE_CURVE ( 'NONE', #100441, #61012, #71708, .T. ) ;
#57716 = CARTESIAN_POINT ( 'NONE',  ( -0.9786431567949999133, 1497.713060387329961, 231.7156151907979904 ) ) ;
#57717 = CARTESIAN_POINT ( 'NONE',  ( 8.605022022878770827, 1464.162231465259993, 214.7347089345799986 ) ) ;
#57718 = CARTESIAN_POINT ( 'NONE',  ( -10.97570570419999925, 1482.624300662889937, 205.8415957027289949 ) ) ;
#57719 = CARTESIAN_POINT ( 'NONE',  ( 2.098165248435849950, 1474.766810392649859, 220.3465733394599795 ) ) ;
#57720 = CARTESIAN_POINT ( 'NONE',  ( -17.37381263529999842, 1410.444759175830086, 225.7669571254979815 ) ) ;
#57721 = CARTESIAN_POINT ( 'NONE',  ( 20.79873180490000095, 1508.014473405230092, 190.2288953139980094 ) ) ;
#57722 = CARTESIAN_POINT ( 'NONE',  ( 15.66262490570000132, 1454.743832497789981, 196.6949010879989999 ) ) ;
#57723 = CARTESIAN_POINT ( 'NONE',  ( -16.47946788473430146, 1409.488508717739933, 192.8607469751509882 ) ) ;
#57724 = CARTESIAN_POINT ( 'NONE',  ( 1.486478317020000217, 1515.456929490889934, 204.9468604023890066 ) ) ;
#57725 = CARTESIAN_POINT ( 'NONE',  ( -2.792392588003544507, 1524.382868172863937, 176.8996806668726549 ) ) ;
#57726 = ADVANCED_FACE ( 'NONE', ( #38590 ), #106897, .F. ) ;
#57727 = CARTESIAN_POINT ( 'NONE',  ( -9.104803375611409066, 1421.479062203829926, 192.1853131441990001 ) ) ;
#57728 = CARTESIAN_POINT ( 'NONE',  ( -0.9908514633770000302, 1414.913060387329779, 226.1016495930979886 ) ) ;
#57729 = CARTESIAN_POINT ( 'NONE',  ( 0.2062144740239800211, 1459.480533006769974, 182.9753669427479963 ) ) ;
#57731 = VERTEX_POINT ( 'NONE', #11749 ) ;
#57730 = CARTESIAN_POINT ( 'NONE',  ( -3.043893720480000287, 1408.958240104829883, 223.4965448387980018 ) ) ;
#57732 = CARTESIAN_POINT ( 'NONE',  ( -27.73716673060003757, 1444.324653571829003, 175.8274728504979976 ) ) ;
#57733 = EDGE_CURVE ( 'NONE', #8806, #78872, #6873, .T. ) ;
#57734 = CARTESIAN_POINT ( 'NONE',  ( -29.12047489647090259, 1509.926054659589909, 211.6780493401929846 ) ) ;
#57735 = CARTESIAN_POINT ( 'NONE',  ( 13.50089340029999896, 1434.968964830010236, 149.1899395279980070 ) ) ;
#57736 = CARTESIAN_POINT ( 'NONE',  ( -40.55649113755679736, 1439.640597909599819, 134.0999999981079895 ) ) ;
#57737 = CARTESIAN_POINT ( 'NONE',  ( -109.1647465200000084, 1384.889898235899864, 297.1327028377589841 ) ) ;
#57738 = ORIENTED_EDGE ( 'NONE', *, *, #15109, .F. ) ;
#57739 = CARTESIAN_POINT ( 'NONE',  ( -17.53704155054333214, 1524.872178180564788, 180.8015429009317074 ) ) ;
#57740 = CARTESIAN_POINT ( 'NONE',  ( 9.336549371730001212, 1479.069783892889973, 203.8813761292790048 ) ) ;
#57741 = CARTESIAN_POINT ( 'NONE',  ( -103.8697664565839887, 1380.102834777972475, 306.0827998670219472 ) ) ;
#57742 = DIRECTION ( 'NONE',  ( -5.980589973904019347E-17, 1.000000000000000000, -1.736889445713099699E-16 ) ) ;
#57744 = EDGE_CURVE ( 'NONE', #3563, #66206, #56506, .T. ) ;
#57743 = CARTESIAN_POINT ( 'NONE',  ( 0.1712571669960009924, 1463.663764520790210, 202.0829161578890023 ) ) ;
#57745 = CARTESIAN_POINT ( 'NONE',  ( 39.76850916013371062, 1424.133492658783780, 269.1346536228787727 ) ) ;
#57746 = CARTESIAN_POINT ( 'NONE',  ( -17.54272989919999759, 1417.931783365949968, 206.8684744458689977 ) ) ;
#57747 = CARTESIAN_POINT ( 'NONE',  ( -14.11636927220000004, 1379.895574107790026, 211.3023527909790005 ) ) ;
#57748 = CARTESIAN_POINT ( 'NONE',  ( 2.982880056399999980, 1425.995092949029868, 184.8396490932979930 ) ) ;
#57749 = CARTESIAN_POINT ( 'NONE',  ( -63.27217475398849444, 1385.077751352280075, 251.1831659201390039 ) ) ;
#57750 = CARTESIAN_POINT ( 'NONE',  ( -18.00465857450842933, 1523.390106123591067, 238.0296012445041072 ) ) ;
#57751 = CARTESIAN_POINT ( 'NONE',  ( 11.18429024643810088, 1422.356073855499972, 207.3872344669040331 ) ) ;
#57752 = ORIENTED_EDGE ( 'NONE', *, *, #22062, .F. ) ;
#57753 = CARTESIAN_POINT ( 'NONE',  ( -32.07183325839999810, 1451.793158448429949, 135.2032643032979990 ) ) ;
#57754 = EDGE_CURVE ( 'NONE', #96120, #101013, #13833, .T. ) ;
#57755 = ADVANCED_FACE ( 'NONE', ( #47022 ), #81147, .F. ) ;
#57756 = CARTESIAN_POINT ( 'NONE',  ( -16.03272477472199853, 1410.858313914460041, 226.7018033498140142 ) ) ;
#57758 = ORIENTED_EDGE ( 'NONE', *, *, #96690, .T. ) ;
#57757 = CARTESIAN_POINT ( 'NONE',  ( 4.026786250540000722, 1422.913060387330006, 172.2701767054979882 ) ) ;
#57759 = CARTESIAN_POINT ( 'NONE',  ( 4.475229445540000128, 1473.172248456590069, 218.4600389222289891 ) ) ;
#57760 = CARTESIAN_POINT ( 'NONE',  ( 11.03246124568249975, 1471.772754036200013, 212.1253387598690097 ) ) ;
#57761 = DIRECTION ( 'NONE',  ( 0.000000000000000000, -1.000000000000000000, 6.123233995736769734E-17 ) ) ;
#57762 = CARTESIAN_POINT ( 'NONE',  ( -109.3085292789999983, 1384.876463481600013, 311.2645431242589780 ) ) ;
#57763 = FACE_OUTER_BOUND ( 'NONE', #25199, .T. ) ;
#57764 = CARTESIAN_POINT ( 'NONE',  ( 19.23182685600000141, 1409.584650579829940, 218.5516146816480045 ) ) ;
#57765 = CARTESIAN_POINT ( 'NONE',  ( -2.184990249054419742, 1419.511891907180143, 185.9735355207210148 ) ) ;
#57766 = CARTESIAN_POINT ( 'NONE',  ( -17.61956548329999706, 1424.285584503029895, 227.5004880819979860 ) ) ;
#57767 = CARTESIAN_POINT ( 'NONE',  ( -4.584004161252830833, 1511.400228778165001, 200.7368584331096599 ) ) ;
#57768 = CARTESIAN_POINT ( 'NONE',  ( 7.875427937609998708, 1449.003968285089968, 202.2333506183190082 ) ) ;
#57769 = CARTESIAN_POINT ( 'NONE',  ( -105.3788045886400369, 1309.112692017090239, 306.2699934482469075 ) ) ;
#57770 = CARTESIAN_POINT ( 'NONE',  ( 25.17249022504864797, 1509.792581934430245, 193.9320483668153088 ) ) ;
#57771 = CARTESIAN_POINT ( 'NONE',  ( -3.835404308833623155, 1396.046995657106436, 202.1011854665750036 ) ) ;
#57772 = CARTESIAN_POINT ( 'NONE',  ( 4.029572640705000985, 1516.858649670339901, 205.0803734583570019 ) ) ;
#57773 = CARTESIAN_POINT ( 'NONE',  ( -10.31340658039999880, 1484.355420805929953, 185.0384118475980131 ) ) ;
#57774 = ORIENTED_EDGE ( 'NONE', *, *, #99266, .F. ) ;
#57775 = EDGE_CURVE ( 'NONE', #7587, #9541, #91223, .T. ) ;
#57776 = CARTESIAN_POINT ( 'NONE',  ( -1.551161424019060098, 1463.265709907049995, 199.4650991780359846 ) ) ;
#57777 = CARTESIAN_POINT ( 'NONE',  ( -4.238155808035029892, 1441.456966744900001, 163.0959397596959946 ) ) ;
#57779 = VERTEX_POINT ( 'NONE', #32413 ) ;
#57778 = CARTESIAN_POINT ( 'NONE',  ( -68.45798957863590317, 1379.747194436310110, 280.0509092537030256 ) ) ;
#57780 = CARTESIAN_POINT ( 'NONE',  ( -11.14562751756762893, 1378.415159664945577, 214.3954126917513179 ) ) ;
#57781 = VERTEX_POINT ( 'NONE', #57639 ) ;
#57782 = CARTESIAN_POINT ( 'NONE',  ( 2.338461258401872023, 1507.140902121078398, 181.2734692029360986 ) ) ;
#57783 = CARTESIAN_POINT ( 'NONE',  ( 12.67382636239999982, 1500.337692531689981, 208.3527651524340172 ) ) ;
#57785 = CARTESIAN_POINT ( 'NONE',  ( 15.85937203857169742, 1410.570398459279886, 191.5484927328450055 ) ) ;
#57784 = CARTESIAN_POINT ( 'NONE',  ( -10.82351740951083308, 1424.916036605491399, 144.6924919310794735 ) ) ;
#57786 = CARTESIAN_POINT ( 'NONE',  ( 1.718203463455000080, 1516.898441858519845, 210.8221056461869978 ) ) ;
#57787 = CARTESIAN_POINT ( 'NONE',  ( 36.33913412423270017, 1436.158733022410161, 135.8962114937069714 ) ) ;
#57788 = CARTESIAN_POINT ( 'NONE',  ( -107.9890416813189944, 1378.913060387289988, 308.4545676344260414 ) ) ;
#57789 = CARTESIAN_POINT ( 'NONE',  ( 10.35181298299999852, 1478.133428305090092, 203.4857779180190107 ) ) ;
#57790 = CARTESIAN_POINT ( 'NONE',  ( 12.65062378175580093, 1500.863489648990026, 210.3581148444430085 ) ) ;
#57791 = CARTESIAN_POINT ( 'NONE',  ( 4.987078416198220232, 1508.551704408389924, 211.6097810847190033 ) ) ;
#57792 = DIRECTION ( 'NONE',  ( 0.000000000000000000, 1.000000000000000000, 0.000000000000000000 ) ) ;
#57793 = EDGE_LOOP ( 'NONE', ( #1827, #35476 ) ) ;
#57794 = CARTESIAN_POINT ( 'NONE',  ( -21.59687355579729839, 1507.523430265019897, 209.4572628990989926 ) ) ;
#57795 = CARTESIAN_POINT ( 'NONE',  ( -20.50000000000000000, 1442.773887286369927, 169.0968414572980123 ) ) ;
#57796 = ORIENTED_EDGE ( 'NONE', *, *, #101731, .T. ) ;
#57797 = ORIENTED_EDGE ( 'NONE', *, *, #180, .F. ) ;
#57798 = FACE_OUTER_BOUND ( 'NONE', #33155, .T. ) ;
#57799 = CARTESIAN_POINT ( 'NONE',  ( 10.39188998415169962, 1453.184289048810115, 211.2438860691320031 ) ) ;
#57800 = DIRECTION ( 'NONE',  ( 0.000000000000000000, -1.000000000000000000, 0.000000000000000000 ) ) ;
#57801 = CARTESIAN_POINT ( 'NONE',  ( -3.344758901520000105, 1485.137791545830169, 183.2117113689980101 ) ) ;
#57802 = CARTESIAN_POINT ( 'NONE',  ( -2.742048936847579998, 1367.348608298013232, 208.3718459617061285 ) ) ;
#57803 = CARTESIAN_POINT ( 'NONE',  ( 2.330134126090001701, 1515.320037165148278, 204.8511296415418599 ) ) ;
#57804 = CARTESIAN_POINT ( 'NONE',  ( 12.12358720160000125, 1442.555572165430021, 187.1519726473979972 ) ) ;
#57805 = CARTESIAN_POINT ( 'NONE',  ( 38.81202641429280220, 1450.612734560829949, 135.3769929298369732 ) ) ;
#57806 = CARTESIAN_POINT ( 'NONE',  ( 3.956111774270300696, 1516.693880335250014, 215.4951837019553977 ) ) ;
#57807 = CARTESIAN_POINT ( 'NONE',  ( 25.97440777459999950, 1440.634477712889975, 137.9745259500980126 ) ) ;
#57808 = CARTESIAN_POINT ( 'NONE',  ( -11.19935432940000020, 1391.089542290570080, 214.3845121043189863 ) ) ;
#57809 = CARTESIAN_POINT ( 'NONE',  ( -67.03180608143330232, 1384.718158239579907, 259.5610210531770008 ) ) ;
#57810 = VERTEX_POINT ( 'NONE', #48680 ) ;
#57811 = CARTESIAN_POINT ( 'NONE',  ( -0.01073133209419849937, 1516.939491476980038, 201.7897819926569980 ) ) ;
#57812 = CARTESIAN_POINT ( 'NONE',  ( -2.493697079054999932, 1516.977201124959947, 208.0034927161370035 ) ) ;
#57813 = ORIENTED_EDGE ( 'NONE', *, *, #45442, .F. ) ;
#57814 = CARTESIAN_POINT ( 'NONE',  ( 37.43385382341080003, 1440.913060387330006, 264.2305522244909639 ) ) ;
#57815 = CARTESIAN_POINT ( 'NONE',  ( -0.002187845253017860030, 1451.807059146780375, 154.0416503108188806 ) ) ;
#57816 = VERTEX_POINT ( 'NONE', #23444 ) ;
#57817 = CARTESIAN_POINT ( 'NONE',  ( -13.50890991390000018, 1415.048591094029916, 220.5416762897979766 ) ) ;
#57818 = CARTESIAN_POINT ( 'NONE',  ( -10.96946876072200006, 1432.347663854339999, 151.7701362700559855 ) ) ;
#57819 = CARTESIAN_POINT ( 'NONE',  ( -3.586377584040013833, 1515.071394843999997, 213.2045508750898364 ) ) ;
#57820 = DIRECTION ( 'NONE',  ( 1.755985294532469921E-16, -1.000000000000000000, 1.338183447452831989E-16 ) ) ;
#57821 = CARTESIAN_POINT ( 'NONE',  ( 21.52851668485050141, 1409.719277583649955, 206.3559433526420150 ) ) ;
#57822 = CARTESIAN_POINT ( 'NONE',  ( -10.80134480061119895, 1446.564900598669965, 153.0805715986579969 ) ) ;
#57823 = CARTESIAN_POINT ( 'NONE',  ( -0.08880850522610000963, 1508.134875444430236, 180.6958675522979831 ) ) ;
#57824 = CARTESIAN_POINT ( 'NONE',  ( -12.91333420139999966, 1434.774326854220135, 147.1504880069980175 ) ) ;
#57825 = CARTESIAN_POINT ( 'NONE',  ( 25.92223975860549601, 1486.880094622480101, 206.2257269294839830 ) ) ;
#57827 = CARTESIAN_POINT ( 'NONE',  ( 0.000000000000000000, 1395.913060387330006, 215.6218459616979999 ) ) ;
#57826 = CARTESIAN_POINT ( 'NONE',  ( 13.66288860260000071, 1461.271167413530065, 231.3349181382980078 ) ) ;
#57828 = DIRECTION ( 'NONE',  ( 5.980589973904019347E-17, -1.000000000000000000, 1.736889445713099699E-16 ) ) ;
#57829 = CARTESIAN_POINT ( 'NONE',  ( -3.259729335964999919, 1517.119374999550018, 216.4589997383470177 ) ) ;
#57830 = ORIENTED_EDGE ( 'NONE', *, *, #95886, .F. ) ;
#57831 = CARTESIAN_POINT ( 'NONE',  ( -11.60004869885203682, -0.000000000000000000, 134.0999999980979851 ) ) ;
#57832 = CYLINDRICAL_SURFACE ( 'NONE', #71458, 1.000000000000070166 ) ;
#57833 = DIRECTION ( 'NONE',  ( -1.836970198721029688E-16, -1.000000000000000000, 0.000000000000000000 ) ) ;
#57834 = CARTESIAN_POINT ( 'NONE',  ( 4.042417777704999438, 1516.904492006980036, 212.5700528489170154 ) ) ;
#57835 = CARTESIAN_POINT ( 'NONE',  ( 18.47399033419999981, 1509.320896582529940, 187.7622940971980086 ) ) ;
#57836 = DIRECTION ( 'NONE',  ( 0.000000000000000000, 0.000000000000000000, 1.000000000000000000 ) ) ;
#57838 = ORIENTED_EDGE ( 'NONE', *, *, #108440, .F. ) ;
#57837 = CARTESIAN_POINT ( 'NONE',  ( -11.93094903640050042, 1501.580206583630115, 211.4284354873250038 ) ) ;
#57839 = CARTESIAN_POINT ( 'NONE',  ( -8.371033105309999556, 1384.892342680180036, 199.7750073836789966 ) ) ;
#57840 = CARTESIAN_POINT ( 'NONE',  ( 7.330199424109999917, 1459.209061203830061, 213.1419610028279692 ) ) ;
#57841 = EDGE_CURVE ( 'NONE', #42229, #25915, #61886, .T. ) ;
#57842 = CARTESIAN_POINT ( 'NONE',  ( -10.96944975070000083, 1432.346411317189904, 151.7703430070979778 ) ) ;
#57843 = CARTESIAN_POINT ( 'NONE',  ( -0.2348491764560019790, 1435.893188924790138, 227.6464390018990116 ) ) ;
#57844 = CARTESIAN_POINT ( 'NONE',  ( -6.176626807815939202, 1440.736226183980079, 202.7885005142740056 ) ) ;
#57845 = CARTESIAN_POINT ( 'NONE',  ( 27.02609455570868846, 1451.901622450774539, 135.4159887955381123 ) ) ;
#57846 = CARTESIAN_POINT ( 'NONE',  ( 3.897009772517886272, 1521.951704408389787, 231.0205787110200788 ) ) ;
#57847 = CARTESIAN_POINT ( 'NONE',  ( 12.71634176899999957, 1445.234570782009996, 187.5504093200979980 ) ) ;
#57849 = CARTESIAN_POINT ( 'NONE',  ( -10.01325982467770004, 1481.014320843050200, 205.7823435180839908 ) ) ;
#57848 = CARTESIAN_POINT ( 'NONE',  ( -20.08153501109999794, 1482.731068538430009, 227.1550935146979953 ) ) ;
#57850 = DIRECTION ( 'NONE',  ( -0.7067625924915348357, 0.03085858548585030531, -0.7067774653711429433 ) ) ;
#57851 = ORIENTED_EDGE ( 'NONE', *, *, #11225, .F. ) ;
#57852 = CARTESIAN_POINT ( 'NONE',  ( 7.710285837685000310, 1516.582197289609894, 205.8614676770269796 ) ) ;
#57853 = CARTESIAN_POINT ( 'NONE',  ( 6.971297644939999039, 1407.166808755230022, 269.6344828128980566 ) ) ;
#57854 = CARTESIAN_POINT ( 'NONE',  ( 38.64592363763749461, 1443.862568456519739, 137.1880729169230051 ) ) ;
#57855 = CARTESIAN_POINT ( 'NONE',  ( 19.76388419090000070, 1410.871606390429861, 196.8289662879980142 ) ) ;
#57856 = CARTESIAN_POINT ( 'NONE',  ( 22.05653339442196881, 1430.082789188892320, 217.9551595525637993 ) ) ;
#57857 = CARTESIAN_POINT ( 'NONE',  ( -7.625768530968147552, 1386.113582989909901, 218.9869377475604324 ) ) ;
#57858 = CARTESIAN_POINT ( 'NONE',  ( -5.992819232552545117, 1413.913060387330006, 198.1520639380683235 ) ) ;
#57859 = CARTESIAN_POINT ( 'NONE',  ( 14.41568985214449938, 1457.296265504200164, 195.0854293786359790 ) ) ;
#57860 = CARTESIAN_POINT ( 'NONE',  ( -15.58996755230000097, 1417.047973859700051, 206.0392561205590027 ) ) ;
#57861 = CARTESIAN_POINT ( 'NONE',  ( -1.554783491535979723, 1451.149365618095544, 183.7066068396813137 ) ) ;
#57862 = EDGE_CURVE ( 'NONE', #22264, #85592, #105557, .T. ) ;
#57863 = CARTESIAN_POINT ( 'NONE',  ( 2.323033503200000460, 1449.800808688150028, 155.6080914323979982 ) ) ;
#57864 = CARTESIAN_POINT ( 'NONE',  ( -8.643932593178378809, 1437.446544997869978, 208.6934462458000041 ) ) ;
#57865 = DIRECTION ( 'NONE',  ( -0.7074300732573280959, -0.02470400251971145017, 0.7063514732133270302 ) ) ;
#57866 = ADVANCED_FACE ( 'NONE', ( #66037 ), #82275, .F. ) ;
#57867 = CARTESIAN_POINT ( 'NONE',  ( -14.97660074589999901, 1430.165149044129976, 219.6133834379979817 ) ) ;
#57868 = EDGE_CURVE ( 'NONE', #108592, #84410, #100159, .T. ) ;
#57869 = CARTESIAN_POINT ( 'NONE',  ( 3.691107917770000135, 1441.076188144620119, 158.1238300962979793 ) ) ;
#57870 = CARTESIAN_POINT ( 'NONE',  ( -3.415211038299999835, 1475.467544519530065, 269.2902994287979936 ) ) ;
#57871 = CARTESIAN_POINT ( 'NONE',  ( -4.222486080285369425, 1446.229412297520184, 167.6242796896230232 ) ) ;
#57872 = CARTESIAN_POINT ( 'NONE',  ( -12.83553538817613671, 1513.363077551962306, 192.3415662781734454 ) ) ;
#57873 = CARTESIAN_POINT ( 'NONE',  ( -109.1450416020000063, 1385.242479493820156, 297.1468691531589457 ) ) ;
#57874 = CARTESIAN_POINT ( 'NONE',  ( -54.14820250061879392, 1384.720608453650129, 270.1448835903210011 ) ) ;
#57875 = CARTESIAN_POINT ( 'NONE',  ( 1.622533071855516207, 1508.277906825712080, 236.9750079835338852 ) ) ;
#57876 = CARTESIAN_POINT ( 'NONE',  ( 16.71439081581360142, 1507.439214557219884, 193.5758153730089930 ) ) ;
#57877 = EDGE_CURVE ( 'NONE', #10824, #53407, #6097, .T. ) ;
#57878 = CARTESIAN_POINT ( 'NONE',  ( -24.61074716929270068, 1457.438344121399950, 212.0276960468289928 ) ) ;
#57879 = CARTESIAN_POINT ( 'NONE',  ( 32.32093690483868187, 1524.075000532257491, 216.0999125871069850 ) ) ;
#57880 = CARTESIAN_POINT ( 'NONE',  ( -2.469737631213410278, 1507.227429411520006, 221.7265308815400147 ) ) ;
#57881 = DIRECTION ( 'NONE',  ( 1.836970198721029688E-16, 1.000000000000000000, 0.000000000000000000 ) ) ;
#57882 = CARTESIAN_POINT ( 'NONE',  ( -8.366802890251092251, 1382.852348275100667, 199.9076995699032011 ) ) ;
#57883 = CARTESIAN_POINT ( 'NONE',  ( 12.46461103178539886, 1421.611150248099875, 207.4535745979419801 ) ) ;
#57884 = CARTESIAN_POINT ( 'NONE',  ( 10.10911558311959979, 1480.122050019980179, 206.2115462197010061 ) ) ;
#57885 = ORIENTED_EDGE ( 'NONE', *, *, #4271, .T. ) ;
#57886 = CARTESIAN_POINT ( 'NONE',  ( -12.90880567115966926, 1410.732768988275666, 227.8208098478615398 ) ) ;
#57887 = CARTESIAN_POINT ( 'NONE',  ( 12.98226713004290112, 1414.913060387349788, 198.3280232619060257 ) ) ;
#57888 = CARTESIAN_POINT ( 'NONE',  ( 7.755379691283469157, 1459.738853292250042, 228.9106028236209909 ) ) ;
#57890 = CARTESIAN_POINT ( 'NONE',  ( -15.12442022026499977, 1514.217947259989842, 194.2848590935669790 ) ) ;
#57889 = CARTESIAN_POINT ( 'NONE',  ( 10.79283000909999934, 1424.934955034829727, 142.7668711269979838 ) ) ;
#57891 = CARTESIAN_POINT ( 'NONE',  ( 17.62867182259785181, 1524.547873515805350, 237.6135799091316585 ) ) ;
#57892 = CARTESIAN_POINT ( 'NONE',  ( -14.38014760757803145, 1517.051704408389924, 209.8840156948171511 ) ) ;
#57893 = CARTESIAN_POINT ( 'NONE',  ( -4.267145232369999874, 1453.908306873689980, 199.9833667514089939 ) ) ;
#57894 = CIRCLE ( 'NONE', #32841, 1.999994602259566712 ) ;
#57895 = CARTESIAN_POINT ( 'NONE',  ( -5.780232115465000042, 1516.760434454289907, 201.7950504087270076 ) ) ;
#57896 = CARTESIAN_POINT ( 'NONE',  ( -8.793958255968036042, 1511.660055404817513, 215.2685923549327924 ) ) ;
#57897 = PLANE ( 'NONE',  #97640 ) ;
#57898 = CARTESIAN_POINT ( 'NONE',  ( 15.69395956763500166, 1511.900571936589813, 196.7363318035669977 ) ) ;
#57899 = CARTESIAN_POINT ( 'NONE',  ( -22.72857882966620124, 1417.467434011349951, 209.9112631640360007 ) ) ;
#57900 = CARTESIAN_POINT ( 'NONE',  ( -34.09660006530000231, 1376.882267573399986, 222.1544401288590223 ) ) ;
#57901 = ADVANCED_FACE ( 'NONE', ( #91753 ), #88346, .T. ) ;
#57902 = CARTESIAN_POINT ( 'NONE',  ( 20.25098345587720061, 1508.866247531380168, 229.1419343274569940 ) ) ;
#57904 = EDGE_LOOP ( 'NONE', ( #107437, #28447, #3395, #44099, #53837 ) ) ;
#57903 = CARTESIAN_POINT ( 'NONE',  ( -40.81304585960000253, 1379.731884794059852, 229.1715070859589787 ) ) ;
#57905 = ORIENTED_EDGE ( 'NONE', *, *, #82339, .T. ) ;
#57906 = CARTESIAN_POINT ( 'NONE',  ( 11.98438189353099936, 1433.653085447690046, 150.0614181868770061 ) ) ;
#57907 = CARTESIAN_POINT ( 'NONE',  ( -10.55476389820000094, 1396.804446593130024, 216.5457841514580082 ) ) ;
#57908 = CARTESIAN_POINT ( 'NONE',  ( -18.50902411670000447, 1409.559409753030195, 221.7674460617980117 ) ) ;
#57909 = EDGE_LOOP ( 'NONE', ( #20322, #22199, #418, #83787, #63535, #24001 ) ) ;
#57910 = CARTESIAN_POINT ( 'NONE',  ( -12.96794556044444846, 1444.895936098864695, 169.4262985252806004 ) ) ;
#57911 = CARTESIAN_POINT ( 'NONE',  ( -28.15442719050000164, 1509.896234649429971, 200.8410286188979796 ) ) ;
#57912 = CARTESIAN_POINT ( 'NONE',  ( 14.43289921540000087, 1509.539432541030010, 235.4218729623979982 ) ) ;
#57913 =( BOUNDED_CURVE ( )  B_SPLINE_CURVE ( 3, ( #51870, #103339, #77072, #381 ),
 .UNSPECIFIED., .F., .T. ) 
 B_SPLINE_CURVE_WITH_KNOTS ( ( 4, 4 ),
 ( 0.5395807524033044977, 1.539014399147148771 ),
 .UNSPECIFIED. ) 
 CURVE ( )  GEOMETRIC_REPRESENTATION_ITEM ( )  RATIONAL_B_SPLINE_CURVE ( ( 1.000000000000000000, 0.9184788592065064039, 0.9184788592065064039, 1.000000000000000000 ) ) 
 REPRESENTATION_ITEM ( '' )  );
#57916 = EDGE_CURVE ( 'NONE', #85844, #94873, #94745, .T. ) ;
#57915 = CARTESIAN_POINT ( 'NONE',  ( -13.96774116474500005, 1509.007359028199971, 183.7017197760899876 ) ) ;
#57914 = CARTESIAN_POINT ( 'NONE',  ( 0.1168726624490010052, 1443.529164943789965, 200.1804741532190235 ) ) ;
#57917 = CARTESIAN_POINT ( 'NONE',  ( 16.38783789769999899, 1488.166949629130158, 188.7551421073980009 ) ) ;
#57918 = CARTESIAN_POINT ( 'NONE',  ( -7.747669800249999739, 1416.518938591829965, 192.4898468467980024 ) ) ;
#57919 = DIRECTION ( 'NONE',  ( 0.6742693640212139572, 4.521919481779822175E-17, 0.7384854939282339270 ) ) ;
#57920 = B_SPLINE_SURFACE_WITH_KNOTS ( 'NONE', 5, 1, ( 
 ( #97518, #19128 ),
 ( #53330, #11863 ),
 ( #89112, #87477 ),
 ( #35404, #10767 ),
 ( #27010, #18576 ),
 ( #60391, #94512 ),
 ( #110774, #25092 ),
 ( #50344, #51424 ),
 ( #67140, #76622 ),
 ( #77733, #77191 ),
 ( #17228, #17786 ),
 ( #42463, #34065 ),
 ( #102364, #85554 ),
 ( #494, #109675 ),
 ( #93963, #8851 ),
 ( #32951, #59840 ),
 ( #25649, #35169 ),
 ( #101238, #24538 ) ),
 .UNSPECIFIED., .F., .F., .F.,
 ( 6, 3, 3, 3, 3, 6 ),
 ( 2, 2 ),
 ( 14.02535798500000119, 16.90079360149999843, 18.14364336469999728, 21.12354018079999918, 24.53920724549999832, 25.26141522939999717 ),
 ( -0.02999077828059999729, 4.111335363550000288 ),
 .UNSPECIFIED. ) ;
#57921 = CARTESIAN_POINT ( 'NONE',  ( 10.95578817948159944, 1396.295644941000091, 210.7241490613100154 ) ) ;
#57922 = CARTESIAN_POINT ( 'NONE',  ( 1.383992982660000148, 1414.983773852829927, 191.7538276128979930 ) ) ;
#57923 = CARTESIAN_POINT ( 'NONE',  ( 11.76383611999999879, 1431.900461285729989, 150.7976845351980160 ) ) ;
#57924 = CARTESIAN_POINT ( 'NONE',  ( 41.15111437360000224, 1443.645439461449996, 136.9181462705980152 ) ) ;
#57925 = EDGE_LOOP ( 'NONE', ( #36795, #46467, #93192, #88809 ) ) ;
#57926 = CARTESIAN_POINT ( 'NONE',  ( 13.01599729242529868, 1434.868266845640164, 149.7301032413199948 ) ) ;
#57927 = ORIENTED_EDGE ( 'NONE', *, *, #59785, .F. ) ;
#57928 = ORIENTED_EDGE ( 'NONE', *, *, #5896, .T. ) ;
#57929 = CARTESIAN_POINT ( 'NONE',  ( -18.62426299532670271, 1497.950872138800150, 229.4157727875710009 ) ) ;
#57930 = CARTESIAN_POINT ( 'NONE',  ( -8.257462432719998802, 1464.334752889730225, 233.3822669687979783 ) ) ;
#57931 = CARTESIAN_POINT ( 'NONE',  ( -108.3146325907701026, 1388.689630667613756, 310.2700825005108527 ) ) ;
#57932 = CARTESIAN_POINT ( 'NONE',  ( 7.718763505904999711, 1516.905946377369901, 216.0642002436470079 ) ) ;
#57933 = CARTESIAN_POINT ( 'NONE',  ( -6.960528455329999531, 1472.781863690589944, 209.0507852043539856 ) ) ;
#57934 = B_SPLINE_SURFACE_WITH_KNOTS ( 'NONE', 5, 5, ( 
 ( #99245, #56724, #62967, #90860, #14148, #48334 ),
 ( #82474, #39916, #28764, #108768, #100370, #16876 ),
 ( #91964, #7410, #85207, #15772, #7956, #99800 ),
 ( #66250, #48891, #49432, #83019, #49974, #51081 ),
 ( #15240, #41008, #76271, #74633, #92505, #24731 ),
 ( #23094, #8497, #25287, #23655, #101441, #109337 ) ),
 .UNSPECIFIED., .F., .F., .F.,
 ( 6, 6 ),
 ( 6, 6 ),
 ( 4.250940516431700011, 7.082035122218299783 ),
 ( -9.670478296250548992E-06, 0.5000000000000000000 ),
 .UNSPECIFIED. ) ;
#57935 = ORIENTED_EDGE ( 'NONE', *, *, #48738, .T. ) ;
#57936 = CARTESIAN_POINT ( 'NONE',  ( -12.78943259969999957, 1502.708798733090134, 209.0180537489830215 ) ) ;
#57937 = CARTESIAN_POINT ( 'NONE',  ( 2.500000000000000000, 1448.261000471720081, 165.3796186243569935 ) ) ;
#57938 = CARTESIAN_POINT ( 'NONE',  ( -11.40322695539999920, 1380.342188321789990, 209.3118815522890088 ) ) ;
#57939 = ORIENTED_EDGE ( 'NONE', *, *, #65330, .T. ) ;
#57940 = CARTESIAN_POINT ( 'NONE',  ( -2.879642191334999879, 1516.812046502680005, 205.6755161564470313 ) ) ;
#57941 = VERTEX_POINT ( 'NONE', #27737 ) ;
#57942 = CARTESIAN_POINT ( 'NONE',  ( -6.944466780504999548, 1516.939530130779985, 209.1331108864249870 ) ) ;
#57943 = CARTESIAN_POINT ( 'NONE',  ( -7.000175857517819900, 1453.642846852349976, 202.9077934395569969 ) ) ;
#57944 = CARTESIAN_POINT ( 'NONE',  ( -16.66453347706279686, 1412.909409113607126, 269.3720812842371970 ) ) ;
#57945 = CARTESIAN_POINT ( 'NONE',  ( -1.647892026280000088, 1409.908608567930060, 232.8799286543980145 ) ) ;
#57947 = ORIENTED_EDGE ( 'NONE', *, *, #18770, .T. ) ;
#57946 = CARTESIAN_POINT ( 'NONE',  ( -0.1687944357496000136, 1416.535698381769862, 227.3595857086420153 ) ) ;
#57948 = CARTESIAN_POINT ( 'NONE',  ( 2.500000000000000000, 1431.135902250849995, 157.4660731311979873 ) ) ;
#57949 = CARTESIAN_POINT ( 'NONE',  ( -29.77671877493460073, 1440.913060386769985, 237.6287523421349874 ) ) ;
#57950 = CARTESIAN_POINT ( 'NONE',  ( -86.96730326719999482, 1384.052306858670136, 307.6473153112589785 ) ) ;
#57951 = CARTESIAN_POINT ( 'NONE',  ( -0.3222280624858790410, 1466.023156909590170, 235.8295839634860158 ) ) ;
#57952 = CARTESIAN_POINT ( 'NONE',  ( 5.377271148049999283, 1408.165475900730144, 270.2871877487980328 ) ) ;
#57953 = CARTESIAN_POINT ( 'NONE',  ( 2.296124850935000072, 1516.677239312369920, 213.7299927514870319 ) ) ;
#57954 = CARTESIAN_POINT ( 'NONE',  ( 22.81920077950000092, 1409.709825997729922, 209.2267294936970075 ) ) ;
#57955 = CARTESIAN_POINT ( 'NONE',  ( -21.47210458610000217, 1509.724521920430107, 188.4228462942980116 ) ) ;
#57956 = CARTESIAN_POINT ( 'NONE',  ( 3.074703527060000052, 1441.333178254290033, 218.5515148082390056 ) ) ;
#57957 = CARTESIAN_POINT ( 'NONE',  ( -7.721293097101060710, 1517.002586324550066, 208.8777730749319801 ) ) ;
#57958 = CARTESIAN_POINT ( 'NONE',  ( -4.610079871555000430, 1516.713079096360161, 210.2553629353369899 ) ) ;
#57959 = CARTESIAN_POINT ( 'NONE',  ( -21.10561344245444815, 1525.661275128775742, 233.3100099925564450 ) ) ;
#57960 = CARTESIAN_POINT ( 'NONE',  ( -13.96267725510150193, 1502.379640760292432, 226.3091245870000989 ) ) ;
#57961 = CARTESIAN_POINT ( 'NONE',  ( -15.24860744008350544, 1486.073951134501840, 186.4853819756072255 ) ) ;
#57963 = ORIENTED_EDGE ( 'NONE', *, *, #39113, .F. ) ;
#57962 = CARTESIAN_POINT ( 'NONE',  ( -70.43097214809999684, 1389.502223237589988, 273.8077508712590316 ) ) ;
#57964 = CARTESIAN_POINT ( 'NONE',  ( -38.79897580568190563, 1385.188763823109866, 240.0467092869539840 ) ) ;
#57965 = B_SPLINE_CURVE_WITH_KNOTS ( 'NONE', 5,
 ( #40033, #91544, #82025, #13701, #14268, #83684, #82597, #32735, #66915, #83144, #74215, #50108, #65803, #23218, #14821, #24322, #15908, #49008, #40584, #66369, #57956 ),
 .UNSPECIFIED., .F., .F.,
 ( 6, 3, 3, 3, 3, 3, 6 ),
 ( 0.000000000000000000, 0.3516404420329832248, 0.7013045389776026983, 0.8764775333732340856, 0.9202713844326411152, 0.9640652354931900092, 1.000000000000000000 ),
 .UNSPECIFIED. ) ;
#57966 = CARTESIAN_POINT ( 'NONE',  ( 17.19449137966054053, 1410.877584405873222, 226.0689879175218948 ) ) ;
#57967 = DIRECTION ( 'NONE',  ( 0.000000000000000000, 1.000000000000000000, 0.000000000000000000 ) ) ;
#57968 = CARTESIAN_POINT ( 'NONE',  ( -1.801950444790000105, 1417.382180821630072, 235.5933117588980110 ) ) ;
#57969 = CARTESIAN_POINT ( 'NONE',  ( 5.033939915584520364, 1484.257078321549898, 219.3935248400869966 ) ) ;
#57970 = CARTESIAN_POINT ( 'NONE',  ( -10.44087869485973030, 1517.151704408390060, 205.3524051900861593 ) ) ;
#57971 = CARTESIAN_POINT ( 'NONE',  ( 12.56945274703499926, 1512.044075975079977, 224.3812485392670055 ) ) ;
#57972 = CIRCLE ( 'NONE', #32920, 1.999999999999999556 ) ;
#57974 = CYLINDRICAL_SURFACE ( 'NONE', #26272, 2.000000000000007550 ) ;
#57973 = CARTESIAN_POINT ( 'NONE',  ( -6.554778571775000451, 1516.929962200689943, 216.8412383526069789 ) ) ;
#57975 = CARTESIAN_POINT ( 'NONE',  ( -27.01380866140000236, 1450.681584507220123, 136.4483241423979791 ) ) ;
#57976 = CARTESIAN_POINT ( 'NONE',  ( 10.23156695028191621, 1422.701445000401236, 137.1234503073714563 ) ) ;
#57977 = ORIENTED_EDGE ( 'NONE', *, *, #61267, .T. ) ;
#57978 = CARTESIAN_POINT ( 'NONE',  ( 2.289624432225000117, 1517.154223579619838, 202.5582500624169882 ) ) ;
#57979 = CARTESIAN_POINT ( 'NONE',  ( -16.65017492986500258, 1513.596256836690145, 223.2301996313669861 ) ) ;
#57980 = CARTESIAN_POINT ( 'NONE',  ( 19.60792669039999936, 1475.100271358290229, 204.3343059087790152 ) ) ;
#57981 = CIRCLE ( 'NONE', #90077, 1.000000000000001332 ) ;
#57982 = CARTESIAN_POINT ( 'NONE',  ( 19.18154864119999914, 1456.154625754229983, 224.9761355071979949 ) ) ;
#57983 = CARTESIAN_POINT ( 'NONE',  ( 7.743430599797714642, 1438.376054508304833, 153.8132518338354657 ) ) ;
#57984 = CARTESIAN_POINT ( 'NONE',  ( -5.064702160787156515, 1462.535433854306575, 200.7801777857700074 ) ) ;
#57985 = CARTESIAN_POINT ( 'NONE',  ( -16.06428792994629973, 1414.913060387329779, 209.3174441339999987 ) ) ;
#57986 = CARTESIAN_POINT ( 'NONE',  ( 4.219439013950669448, 1441.595895969210005, 182.7715284958480026 ) ) ;
#57987 = B_SPLINE_CURVE_WITH_KNOTS ( 'NONE', 5,
 ( #9891, #79319, #60882, #61988, #51911, #27250, #61431, #53582, #87729 ),
 .UNSPECIFIED., .F., .F.,
 ( 6, 3, 6 ),
 ( 0.000000000000000000, 0.4107976024515093694, 1.000000000000000000 ),
 .UNSPECIFIED. ) ;
#57988 = CARTESIAN_POINT ( 'NONE',  ( 27.07880669207580127, 1435.598858538910008, 136.1558489245400096 ) ) ;
#57989 = CARTESIAN_POINT ( 'NONE',  ( 39.23819738392720069, 1447.383198997459886, 136.5851928137900018 ) ) ;
#57990 = CARTESIAN_POINT ( 'NONE',  ( -21.46437004979999941, 1429.716328564329842, 220.0955847048980161 ) ) ;
#57991 = CARTESIAN_POINT ( 'NONE',  ( -10.80059289547383194, 1474.148535085230606, 269.6142578605208087 ) ) ;
#57992 = CARTESIAN_POINT ( 'NONE',  ( -105.2029017080000131, 1390.344333028660003, 302.0615195368590093 ) ) ;
#57993 = EDGE_CURVE ( 'NONE', #52122, #81601, #42962, .T. ) ;
#57994 = CARTESIAN_POINT ( 'NONE',  ( -17.00646468379999732, 1415.800410784929909, 226.5733319496979732 ) ) ;
#57995 = CARTESIAN_POINT ( 'NONE',  ( -107.1612063080000041, 1391.913060387289988, 300.7260049596590079 ) ) ;
#57996 = CARTESIAN_POINT ( 'NONE',  ( -13.57486036570845833, 1469.792362884156773, 269.3590160498212640 ) ) ;
#57997 = ORIENTED_EDGE ( 'NONE', *, *, #76878, .F. ) ;
#57998 = CARTESIAN_POINT ( 'NONE',  ( -8.542608682037007739, 1440.192411897979810, 205.6891261743860184 ) ) ;
#57999 = CARTESIAN_POINT ( 'NONE',  ( -32.46047264654747266, 1416.888327440118019, 269.3060940481729517 ) ) ;
#58000 = CARTESIAN_POINT ( 'NONE',  ( -4.802243959118389860, 1508.551704408389924, 213.5515878908929892 ) ) ;
#58001 = CARTESIAN_POINT ( 'NONE',  ( -4.360582346120001063, 1431.113060387329824, 227.9437648745980027 ) ) ;
#58002 = CARTESIAN_POINT ( 'NONE',  ( -15.31264328659269403, 1451.565714120024722, 222.7578395244654814 ) ) ;
#58003 = CARTESIAN_POINT ( 'NONE',  ( -13.27459202670609173, 1444.621175491612121, 186.6925910478026367 ) ) ;
#58004 = CARTESIAN_POINT ( 'NONE',  ( -8.838558338096110134, 1438.385153647559946, 208.8793219489340061 ) ) ;
#58005 = CARTESIAN_POINT ( 'NONE',  ( -2.958096254149490623, 1515.068899375750107, 213.4512612264969960 ) ) ;
#58006 = FACE_OUTER_BOUND ( 'NONE', #35818, .T. ) ;
#58008 = ADVANCED_FACE ( 'NONE', ( #64123 ), #54404, .T. ) ;
#58007 = CARTESIAN_POINT ( 'NONE',  ( -7.863053483428857682, 1451.394019542978185, 152.9855632054714931 ) ) ;
#58009 = CARTESIAN_POINT ( 'NONE',  ( -9.661041455239748998, 1460.496751011739889, 209.0910779832980211 ) ) ;
#58010 = CARTESIAN_POINT ( 'NONE',  ( -2.586254832189999853, 1431.686802707190054, 214.1917715140089911 ) ) ;
#58012 = ORIENTED_EDGE ( 'NONE', *, *, #3790, .T. ) ;
#58011 = CARTESIAN_POINT ( 'NONE',  ( -14.06591346399999942, 1410.775981576729919, 226.9656985104979867 ) ) ;
#58013 = CARTESIAN_POINT ( 'NONE',  ( 0.5081859945959991132, 1415.431750870129918, 191.3337547248510191 ) ) ;
#58014 = CARTESIAN_POINT ( 'NONE',  ( 21.07223471314816265, 1508.254227089592632, 226.1111686167440951 ) ) ;
#58015 = EDGE_CURVE ( 'NONE', #70504, #7001, #73957, .T. ) ;
#58016 = ORIENTED_EDGE ( 'NONE', *, *, #28969, .T. ) ;
#58017 = ORIENTED_EDGE ( 'NONE', *, *, #39405, .F. ) ;
#58018 = CARTESIAN_POINT ( 'NONE',  ( 16.38929703815969674, 1414.913060387399810, 210.1493163092779923 ) ) ;
#58019 = FACE_OUTER_BOUND ( 'NONE', #104728, .T. ) ;
#58021 = CARTESIAN_POINT ( 'NONE',  ( -3.776117134630000205, 1460.308496303429820, 216.2848420587179987 ) ) ;
#58020 = CARTESIAN_POINT ( 'NONE',  ( 2.419279911200000299, 1454.975743091090180, 218.2344084821389743 ) ) ;
#58022 = CARTESIAN_POINT ( 'NONE',  ( -20.49650080320000001, 1506.525074349130136, 189.7974850576979975 ) ) ;
#58023 = CARTESIAN_POINT ( 'NONE',  ( -10.99125927559999916, 1433.250798529490112, 151.7641638922980007 ) ) ;
#58024 = CARTESIAN_POINT ( 'NONE',  ( -15.09047375999176843, 1517.051704408389924, 202.6311677367078232 ) ) ;
#58025 = CARTESIAN_POINT ( 'NONE',  ( 16.19492434978379691, 1409.478599607480191, 224.1775087544979783 ) ) ;
#58026 = CARTESIAN_POINT ( 'NONE',  ( 6.826200034800000260, 1424.874072630889941, 213.4902541782590220 ) ) ;
#58027 = CARTESIAN_POINT ( 'NONE',  ( -24.25757607999999976, 1438.852108944180145, 211.3728147305379821 ) ) ;
#58028 = CARTESIAN_POINT ( 'NONE',  ( -3.516555726533699744, 1454.164898032659949, 199.2503824040580014 ) ) ;
#58029 = CARTESIAN_POINT ( 'NONE',  ( 2.480548060760000340, 1449.812485612440241, 182.9983066197980008 ) ) ;
#58030 = CARTESIAN_POINT ( 'NONE',  ( 8.716786869081156297, 1364.517005822695410, 210.6218459617142003 ) ) ;
#58031 = CARTESIAN_POINT ( 'NONE',  ( -24.38581948224031137, 1509.879308922522114, 226.6760032255506871 ) ) ;
#58033 = ORIENTED_EDGE ( 'NONE', *, *, #69999, .F. ) ;
#58032 = FACE_OUTER_BOUND ( 'NONE', #29093, .T. ) ;
#58034 = EDGE_LOOP ( 'NONE', ( #141, #4908, #7387, #104600 ) ) ;
#58035 = CARTESIAN_POINT ( 'NONE',  ( -11.81201955091739997, 1428.846405886920138, 148.7528568703669976 ) ) ;
#58036 = CARTESIAN_POINT ( 'NONE',  ( 13.97509019449999812, 1500.690698309590061, 227.7022812698990037 ) ) ;
#58037 = CARTESIAN_POINT ( 'NONE',  ( -4.903602370519999809, 1472.418623804529943, 270.3706473056980144 ) ) ;
#58038 = CARTESIAN_POINT ( 'NONE',  ( -110.0631611386010036, 1384.920974733809771, 296.9512360025400426 ) ) ;
#58040 = EDGE_CURVE ( 'NONE', #73515, #4626, #19181, .T. ) ;
#58039 = CARTESIAN_POINT ( 'NONE',  ( -113.4000000000000057, 1366.350733876289951, 315.0056284496589569 ) ) ;
#58041 = CARTESIAN_POINT ( 'NONE',  ( 41.19002696412830034, 1446.271008772989944, 136.2099985660260018 ) ) ;
#58042 = CARTESIAN_POINT ( 'NONE',  ( 19.60393592299999810, 1475.513060387329915, 201.4085066119280043 ) ) ;
#58043 = FACE_OUTER_BOUND ( 'NONE', #102638, .T. ) ;
#58044 = CARTESIAN_POINT ( 'NONE',  ( 10.01013843233299916, 1469.369181467840008, 209.9819040969830155 ) ) ;
#58045 = B_SPLINE_CURVE_WITH_KNOTS ( 'NONE', 5,
 ( #74297, #47432, #98914, #41225, #81555, #39573, #92176, #13242, #24404 ),
 .UNSPECIFIED., .F., .F.,
 ( 6, 3, 6 ),
 ( 0.7655572723410000169, 2.316155491850000026, 3.835724788409999420 ),
 .UNSPECIFIED. ) ;
#58046 = CYLINDRICAL_SURFACE ( 'NONE', #41503, 1.000000000000000888 ) ;
#58047 = CARTESIAN_POINT ( 'NONE',  ( 9.813910351400000565, 1364.017814053650000, 207.6218459616989946 ) ) ;
#58048 = CARTESIAN_POINT ( 'NONE',  ( -43.54088588253560488, 1430.059707464080248, 268.8270446202420203 ) ) ;
#58049 = ORIENTED_EDGE ( 'NONE', *, *, #22971, .F. ) ;
#58050 = CYLINDRICAL_SURFACE ( 'NONE', #9089, 2.000000000000003553 ) ;
#58051 = VECTOR ( 'NONE', #73381, 1000.000000000000000 ) ;
#58052 = EDGE_LOOP ( 'NONE', ( #1999, #13136, #50208, #27233, #53119 ) ) ;
#58053 = VERTEX_POINT ( 'NONE', #103191 ) ;
#58054 = CARTESIAN_POINT ( 'NONE',  ( 4.624736859184999993, 1516.994127245590107, 211.9896495963369887 ) ) ;
#58055 = CARTESIAN_POINT ( 'NONE',  ( -8.630493275741649484, 1448.198865873919885, 212.2264116289769902 ) ) ;
#58056 = CARTESIAN_POINT ( 'NONE',  ( 0.000000000000000000, 1420.119835273649869, 209.1218459616989946 ) ) ;
#58057 = AXIS2_PLACEMENT_3D ( 'NONE', #21844, #56594, #14011 ) ;
#58059 = CARTESIAN_POINT ( 'NONE',  ( -14.41619594183999986, 1509.538862653740125, 182.8126525573280219 ) ) ;
#58058 = CARTESIAN_POINT ( 'NONE',  ( 4.622842844184999578, 1516.901952101700090, 213.1523604828169880 ) ) ;
#58060 = CARTESIAN_POINT ( 'NONE',  ( -2.840701075410000165, 1470.463058086329966, 183.9230798073980111 ) ) ;
#58061 = CIRCLE ( 'NONE', #84801, 5.133097426430088817 ) ;
#58062 = CARTESIAN_POINT ( 'NONE',  ( -17.28556280980830095, 1479.740375246909935, 228.8535606757079961 ) ) ;
#58063 = B_SPLINE_SURFACE_WITH_KNOTS ( 'NONE', 2, 5, ( 
 ( #69858, #44088, #76569, #87185, #93908, #59243 ),
 ( #34012, #51934, #34566, #52494, #17733, #18301 ),
 ( #25041, #445, #86623, #78226, #85502, #103408 ) ),
 .UNSPECIFIED., .F., .F., .F.,
 ( 3, 3 ),
 ( 6, 6 ),
 ( 1.399803019419999961, 2.016961153140000018 ),
 ( 0.000000000000000000, 1.000000000000000000 ),
 .UNSPECIFIED. ) ;
#58064 = ORIENTED_EDGE ( 'NONE', *, *, #108035, .T. ) ;
#58065 = DIRECTION ( 'NONE',  ( 0.000000000000000000, -1.000000000000000000, 0.000000000000000000 ) ) ;
#58066 = CARTESIAN_POINT ( 'NONE',  ( 2.483322453895000059, 1517.139039350860003, 202.5585910412470128 ) ) ;
#58067 = B_SPLINE_SURFACE_WITH_KNOTS ( 'NONE', 5, 1, ( 
 ( #63581, #11501 ),
 ( #97151, #64677 ),
 ( #97698, #106640 ),
 ( #30488, #88758 ),
 ( #45677, #21513 ),
 ( #38877, #98243 ),
 ( #29931, #105564 ),
 ( #79815, #55173 ),
 ( #64122, #37249 ) ),
 .UNSPECIFIED., .F., .F., .F.,
 ( 6, 3, 6 ),
 ( 2, 2 ),
 ( 2.977480884639999825, 6.317148707589999468, 12.84608988247099859 ),
 ( -13.58503197309999955, -1.277641458209999969 ),
 .UNSPECIFIED. ) ;
#58068 = DIRECTION ( 'NONE',  ( -1.577721810442025012E-32, -1.000000000000000000, 6.123233995736769734E-17 ) ) ;
#58069 = CARTESIAN_POINT ( 'NONE',  ( -46.70525487443880053, 1384.605919513219760, 220.5286058093979875 ) ) ;
#58070 = CARTESIAN_POINT ( 'NONE',  ( -42.85029935319199978, 1436.020988110130020, 270.2009494392980287 ) ) ;
#58071 = CARTESIAN_POINT ( 'NONE',  ( -19.49652697766560294, 1485.947961896859852, 201.9289638760380114 ) ) ;
#58073 = ORIENTED_EDGE ( 'NONE', *, *, #40540, .F. ) ;
#58072 = LINE ( 'NONE', #25532, #38630 ) ;
#58074 = ORIENTED_EDGE ( 'NONE', *, *, #100969, .F. ) ;
#58075 = CARTESIAN_POINT ( 'NONE',  ( 18.79226589730000185, 1456.307606824690083, 213.7887498653890077 ) ) ;
#58076 = CARTESIAN_POINT ( 'NONE',  ( -28.44964981546823779, 1526.382868172864164, 219.8796466721389606 ) ) ;
#58077 = CARTESIAN_POINT ( 'NONE',  ( 2.588573091324529951, 1426.130607012579958, 191.2585785401599878 ) ) ;
#58078 = CARTESIAN_POINT ( 'NONE',  ( -12.84239665067440050, 1435.935719077439899, 150.8114796122480072 ) ) ;
#58079 = CARTESIAN_POINT ( 'NONE',  ( -24.28687749879999913, 1442.594715683929962, 211.8376410442379836 ) ) ;
#58080 = CARTESIAN_POINT ( 'NONE',  ( -6.933587693644999383, 1516.542957540330008, 210.8312046333570038 ) ) ;
#58081 = CARTESIAN_POINT ( 'NONE',  ( 4.689995948910178569, 1459.453669361078482, 200.6829600737077044 ) ) ;
#58082 = CARTESIAN_POINT ( 'NONE',  ( -2.234865362860189553, 1484.253666364170158, 183.1161028472960197 ) ) ;
#58083 = CARTESIAN_POINT ( 'NONE',  ( 9.130434922834639977, 1437.290822646750030, 212.9268152338410118 ) ) ;
#58084 = LINE ( 'NONE', #92217, #46792 ) ;
#58085 = VECTOR ( 'NONE', #2475, 1000.000000000000000 ) ;
#58086 = CARTESIAN_POINT ( 'NONE',  ( 4.026614479655000522, 1516.699825673279975, 207.4075116849170115 ) ) ;
#58087 = VERTEX_POINT ( 'NONE', #2994 ) ;
#58088 = CARTESIAN_POINT ( 'NONE',  ( -33.91369120209999721, 1451.728768194229815, 134.0999999980979851 ) ) ;
#58089 = CARTESIAN_POINT ( 'NONE',  ( -10.74194912529999968, 1471.560973568090049, 206.8675636587589963 ) ) ;
#58090 = AXIS2_PLACEMENT_3D ( 'NONE', #74074, #16323, #75721 ) ;
#58091 = CARTESIAN_POINT ( 'NONE',  ( -18.92604478490211406, 1457.990945249578544, 226.9998699462371405 ) ) ;
#58092 = ORIENTED_EDGE ( 'NONE', *, *, #85721, .F. ) ;
#58093 = CARTESIAN_POINT ( 'NONE',  ( -29.35073940689260752, 1526.211523310372058, 197.7230717947574306 ) ) ;
#58094 = CARTESIAN_POINT ( 'NONE',  ( 12.87368581495110043, 1434.742583859479964, 149.5707935314029839 ) ) ;
#58095 = CARTESIAN_POINT ( 'NONE',  ( 4.454121045402620105, 1468.999327738519924, 234.0578715337849758 ) ) ;
#58096 = B_SPLINE_CURVE_WITH_KNOTS ( 'NONE', 3,
 ( #4584, #38717, #89134, #61755, #12960, #87495 ),
 .UNSPECIFIED., .F., .F.,
 ( 4, 2, 4 ),
 ( 0.000000000000000000, 0.5000000000000000000, 1.000000000000000000 ),
 .UNSPECIFIED. ) ;
#58097 = CARTESIAN_POINT ( 'NONE',  ( 18.28985832975333636, 1522.051704408389924, 219.7143006364888436 ) ) ;
#58098 = CARTESIAN_POINT ( 'NONE',  ( 24.32432927030000158, 1452.063639817629792, 136.1371466596980042 ) ) ;
#58099 = CARTESIAN_POINT ( 'NONE',  ( 5.823572337359999906, 1487.975078907890065, 198.5964445195989754 ) ) ;
#58100 = CARTESIAN_POINT ( 'NONE',  ( 2.404122373123565914, 1426.711430350427463, 142.7750368341233695 ) ) ;
#58101 = CARTESIAN_POINT ( 'NONE',  ( 4.269138570313380399, 1441.141876082800081, 158.1427116847730190 ) ) ;
#58103 = CARTESIAN_POINT ( 'NONE',  ( -16.27770732761305794, 1446.651107274472906, 198.7459790681657807 ) ) ;
#58102 = CARTESIAN_POINT ( 'NONE',  ( -4.611879723454999969, 1516.858533673840157, 213.7437437946470027 ) ) ;
#58104 = CARTESIAN_POINT ( 'NONE',  ( -7.508706911753730395, 1508.884207225577029, 214.6352815288312570 ) ) ;
#58105 = CARTESIAN_POINT ( 'NONE',  ( -5.003220765204999587, 1516.983995446890049, 216.0685944891870065 ) ) ;
#58106 = EDGE_LOOP ( 'NONE', ( #91584, #57905, #31763, #29209, #71181 ) ) ;
#58107 = CARTESIAN_POINT ( 'NONE',  ( -17.97818486826909989, 1488.931524437730104, 229.1373185541280009 ) ) ;
#58108 = CARTESIAN_POINT ( 'NONE',  ( -16.76029352119999771, 1420.475925714450113, 203.3596836330289932 ) ) ;
#58109 = CARTESIAN_POINT ( 'NONE',  ( 2.191804311359999868, 1420.975114716630060, 184.3756173852979714 ) ) ;
#58110 = B_SPLINE_CURVE_WITH_KNOTS ( 'NONE', 5,
 ( #11713, #104113, #80021, #3342, #63254, #97362 ),
 .UNSPECIFIED., .F., .F.,
 ( 6, 6 ),
 ( -0.5000000000000000000, 0.000000000000000000 ),
 .UNSPECIFIED. ) ;
#58111 = CARTESIAN_POINT ( 'NONE',  ( -3.523962717220000318, 1476.511731497689880, 220.0526012939989755 ) ) ;
#58112 = CARTESIAN_POINT ( 'NONE',  ( 2.478617600774434049, 1524.659802833172535, 175.7713138579284475 ) ) ;
#58113 = CARTESIAN_POINT ( 'NONE',  ( -7.545139471115629881, 1384.910385469629773, 219.0876080393670122 ) ) ;
#58114 = CARTESIAN_POINT ( 'NONE',  ( -11.17593228934340033, 1471.359546453119947, 206.7956388744609910 ) ) ;
#58115 = CARTESIAN_POINT ( 'NONE',  ( -7.106047323496611945, 1508.384870682446717, 219.7310283353839111 ) ) ;
#58116 = CARTESIAN_POINT ( 'NONE',  ( 17.67081254923106926, 1423.277421049964914, 226.2500432428864485 ) ) ;
#58117 = CARTESIAN_POINT ( 'NONE',  ( -109.1672562883220081, 1384.984605947210184, 297.1332200933230183 ) ) ;
#58118 = DIRECTION ( 'NONE',  ( 0.02616798426500960631, 0.9993150019883682011, 0.02616798426500950570 ) ) ;
#58119 = CARTESIAN_POINT ( 'NONE',  ( 38.64164465084230216, 1440.913060378469936, 257.2879587844699927 ) ) ;
#58121 = CARTESIAN_POINT ( 'NONE',  ( 14.31472612081786799, 1507.539056556547848, 186.0170524603447859 ) ) ;
#58120 = CARTESIAN_POINT ( 'NONE',  ( -10.64861439574930024, 1470.416444257950161, 211.6181901305839972 ) ) ;
#58122 = LINE ( 'NONE', #107952, #99290 ) ;
#58123 = ORIENTED_EDGE ( 'NONE', *, *, #37818, .F. ) ;
#58124 = EDGE_LOOP ( 'NONE', ( #99315, #41082, #26727, #68899 ) ) ;
#58125 = CIRCLE ( 'NONE', #92082, 1.999999999999999556 ) ;
#58126 = CARTESIAN_POINT ( 'NONE',  ( -19.51279205535366046, 1485.520671005373060, 190.0467292662184491 ) ) ;
#58127 = CARTESIAN_POINT ( 'NONE',  ( 9.500116199115000271, 1517.051704408389924, 195.7139841003669858 ) ) ;
#58128 = CARTESIAN_POINT ( 'NONE',  ( 11.36216713388179933, 1503.110266152410077, 211.0233809544849919 ) ) ;
#58129 = CARTESIAN_POINT ( 'NONE',  ( 1.400808530693328446, 1507.374882240569832, 236.8304372390393837 ) ) ;
#58130 = VECTOR ( 'NONE', #108637, 1000.000000000000000 ) ;
#58131 = DIRECTION ( 'NONE',  ( 0.06436433998262545975, 0.7055452152162795532, 0.7057359145062795935 ) ) ;
#58132 = CARTESIAN_POINT ( 'NONE',  ( 1.657045479016600042, 1508.551704408389924, 219.7501937159020144 ) ) ;
#58133 = CARTESIAN_POINT ( 'NONE',  ( 19.67623451925446076, 1525.581535527372807, 181.0581612215006260 ) ) ;
#58134 = CARTESIAN_POINT ( 'NONE',  ( -39.76728728541259983, 1383.828512391789900, 241.3785448166720187 ) ) ;
#58135 = CARTESIAN_POINT ( 'NONE',  ( -4.820945246504999560, 1510.984078637139874, 201.4521197723069861 ) ) ;
#58136 = CARTESIAN_POINT ( 'NONE',  ( -13.18252224579999954, 1434.994542537020152, 194.3559101920980083 ) ) ;
#58137 = B_SPLINE_CURVE_WITH_KNOTS ( 'NONE', 3,
 ( #101999, #17427, #84655, #43772, #9060, #1230, #25285, #51078, #68442, #94157, #84108, #93596, #110418, #7952, #34260, #60596, #76823, #75728, #8494, #33152, #95279, #16873, #16330, #94717, #17993, #85205, #102545, #25838, #41573, #85762, #103102, #34812, #42667, #138, #60039, #51625, #77923, #43231, #24729, #35367, #50530, #77379, #681, #52188, #42121, #69554, #68999, #76269, #26403, #86318, #33697, #109873, #9602, #103674 ),
 .UNSPECIFIED., .F., .F.,
 ( 4, 2, 2, 2, 2, 2, 1, 2, 2, 2, 2, 1, 2, 2, 2, 1, 1, 2, 2, 2, 1, 1, 2, 2, 2, 2, 1, 1, 2, 2, 4 ),
 ( 0.000000000000000000, 0.03125000000116372884, 0.04687500000159226105, 0.05468750000166328062, 0.06250000000173429326, 0.09375000000235139686, 0.1093750000026626479, 0.1171875000029593689, 0.1250000000032560898, 0.1875000000045450310, 0.2187500000051895155, 0.2343750000053846372, 0.2421875000053570204, 0.2500000000053294036, 0.3125000000048098747, 0.3437500000045571324, 0.3593750000044307336, 0.3671875000043675619, 0.3750000000043043347, 0.4375000000043617887, 0.4687500000045123350, 0.4843750000045782822, 0.4921875000046112558, 0.5000000000046441739, 0.6250000000040655257, 0.6875000000037638781, 0.7187500000035280667, 0.7343750000034996450, 0.7421875000034117154, 0.7500000000033237857, 1.000000000000000000 ),
 .UNSPECIFIED. ) ;
#58138 = CARTESIAN_POINT ( 'NONE',  ( -8.589426147275000645, 1436.798469860880004, 209.9038450004319998 ) ) ;
#58139 = CARTESIAN_POINT ( 'NONE',  ( 10.93677888065239934, 1490.434389039140115, 209.9320082733399886 ) ) ;
#58141 = ORIENTED_EDGE ( 'NONE', *, *, #85108, .F. ) ;
#58140 = CARTESIAN_POINT ( 'NONE',  ( -3.084094934559999945, 1457.182013509390117, 218.2582506311690054 ) ) ;
#58142 = CARTESIAN_POINT ( 'NONE',  ( 33.28034951413137321, 1522.644714754858796, 217.4407153818774248 ) ) ;
#58143 = B_SPLINE_SURFACE_WITH_KNOTS ( 'NONE', 4, 5, ( 
 ( #99193, #107617, #4615, #64541, #13533, #65078 ),
 ( #72926, #107065, #47719, #31449, #83499, #32006 ),
 ( #81850, #6254, #5153, #22473, #6795, #66195 ),
 ( #109282, #39310, #32566, #56673, #89711, #12989 ),
 ( #85156, #58324, #33101, #85708, #7897, #33641 ) ),
 .UNSPECIFIED., .F., .F., .F.,
 ( 5, 5 ),
 ( 6, 6 ),
 ( 17.21936457409999832, 17.22979334940000129 ),
 ( 0.000000000000000000, 2.175007696500000254 ),
 .UNSPECIFIED. ) ;
#58144 = CARTESIAN_POINT ( 'NONE',  ( -48.18572634930000476, 1380.371872704240104, 227.8530853065590236 ) ) ;
#58145 = CARTESIAN_POINT ( 'NONE',  ( 19.85783298583229950, 1508.594920224220004, 229.4585935219059820 ) ) ;
#58146 = VERTEX_POINT ( 'NONE', #86411 ) ;
#58147 = ORIENTED_EDGE ( 'NONE', *, *, #28124, .T. ) ;
#58148 = CARTESIAN_POINT ( 'NONE',  ( -8.633823299111480054, 1386.054477820370039, 218.5393177817969956 ) ) ;
#58149 = CARTESIAN_POINT ( 'NONE',  ( -4.136749811987540326, 1515.492902828930028, 206.2237479538289904 ) ) ;
#58151 = CARTESIAN_POINT ( 'NONE',  ( -2.723255399910000207, 1468.839623697090019, 189.3038879039989979 ) ) ;
#58150 = CARTESIAN_POINT ( 'NONE',  ( 18.07041998555279960, 1523.313115944345554, 180.1545818505811667 ) ) ;
#58152 = CARTESIAN_POINT ( 'NONE',  ( 11.72068719049280006, 1479.848144395859890, 210.3626758944340054 ) ) ;
#58153 = CARTESIAN_POINT ( 'NONE',  ( -105.5320588160000028, 1381.208403848540001, 299.1971426474589748 ) ) ;
#58154 = DIRECTION ( 'NONE',  ( 0.7071067811870476172, 0.000000000000000000, -0.7071067811860475283 ) ) ;
#58155 = DIRECTION ( 'NONE',  ( -9.551066690030985733E-08, -1.946171181391529080E-07, 0.9999999999999764633 ) ) ;
#58156 = CARTESIAN_POINT ( 'NONE',  ( -8.519142658073340257, 1508.551704408389924, 218.7985387068179932 ) ) ;
#58157 = CARTESIAN_POINT ( 'NONE',  ( -113.4000000000000057, 1378.913060387289988, 304.2218459572590064 ) ) ;
#58158 = CARTESIAN_POINT ( 'NONE',  ( 18.52279787119999810, 1425.631473512029970, 225.3995475816979877 ) ) ;
#58159 = CARTESIAN_POINT ( 'NONE',  ( -108.8775172686859918, 1385.241885096709893, 297.1378884389180257 ) ) ;
#58160 = CARTESIAN_POINT ( 'NONE',  ( -1.636741614903409969, 1469.777368438049962, 219.0527109355280118 ) ) ;
#58161 = CARTESIAN_POINT ( 'NONE',  ( -4.220880940900710421, 1441.618787263769718, 168.7222756990960022 ) ) ;
#58162 = CARTESIAN_POINT ( 'NONE',  ( 0.000000000000000000, 1412.913060387329779, 209.1218459616979999 ) ) ;
#58163 = ORIENTED_EDGE ( 'NONE', *, *, #96530, .T. ) ;
#58164 = CIRCLE ( 'NONE', #15203, 2.000000000000001776 ) ;
#58165 = CARTESIAN_POINT ( 'NONE',  ( 18.02257621027596812, 1526.382868172863937, 235.3484976865586589 ) ) ;
#58166 = CARTESIAN_POINT ( 'NONE',  ( 19.27358882249560068, 1456.231984985270174, 227.7371637781419906 ) ) ;
#58167 = CARTESIAN_POINT ( 'NONE',  ( -19.27355791249999939, 1467.813399981289876, 204.3088842694490097 ) ) ;
#58168 = CARTESIAN_POINT ( 'NONE',  ( -8.278637686411969791E-09, 1472.684511341680036, 260.5494539826829623 ) ) ;
#58169 = CARTESIAN_POINT ( 'NONE',  ( 20.36084529355510142, 1436.440394646498589, 145.0484382341195726 ) ) ;
#58170 = CARTESIAN_POINT ( 'NONE',  ( 1.422097314359999976, 1477.081575188689840, 198.6901653669989969 ) ) ;
#58171 = CARTESIAN_POINT ( 'NONE',  ( -108.3896730050000059, 1388.605325449289921, 310.3517716152589969 ) ) ;
#58172 = AXIS2_PLACEMENT_3D ( 'NONE', #68385, #2293, #86811 ) ;
#58173 = CARTESIAN_POINT ( 'NONE',  ( -1.215107678660000134, 1486.521536555729881, 182.1360231587979968 ) ) ;
#58174 = CARTESIAN_POINT ( 'NONE',  ( -8.082564370840000123, 1362.241991287400197, 207.6218459616989946 ) ) ;
#58175 = CARTESIAN_POINT ( 'NONE',  ( 2.393091348901930093, 1429.053683011190060, 217.0555866711269744 ) ) ;
#58176 = CARTESIAN_POINT ( 'NONE',  ( -8.742754168010000271, 1424.489613839150024, 206.0336725849989818 ) ) ;
#58177 = ADVANCED_FACE ( 'NONE', ( #44429 ), #37392, .F. ) ;
#58178 = CARTESIAN_POINT ( 'NONE',  ( -7.724874651314999952, 1517.139320148880188, 208.3815253650730028 ) ) ;
#58179 = CARTESIAN_POINT ( 'NONE',  ( 17.66967187227356817, 1521.951704408389787, 223.1030594000600900 ) ) ;
#58180 = B_SPLINE_SURFACE_WITH_KNOTS ( 'NONE', 5, 5, ( 
 ( #38091, #54912, #97449, #105300, #36984, #80094 ),
 ( #70629, #28034, #47060, #88506, #19060, #3414 ),
 ( #11789, #81184, #62791, #96906, #53265, #89038 ),
 ( #4500, #95793, #53829, #105862, #37543, #70083 ),
 ( #71745, #87404, #29685, #27480, #3964, #12326 ),
 ( #10698, #29141, #63329, #61670, #71178, #54374 ) ),
 .UNSPECIFIED., .F., .F., .F.,
 ( 6, 6 ),
 ( 6, 6 ),
 ( 16.36816738399999949, 93.94674272650000546 ),
 ( -2.775557561569999727E-17, 1.000000000000000000 ),
 .UNSPECIFIED. ) ;
#58181 = CARTESIAN_POINT ( 'NONE',  ( -1.546867746862319981, 1416.839692133689823, 228.0214409764060122 ) ) ;
#58182 = CARTESIAN_POINT ( 'NONE',  ( 7.516502869536429543, 1425.414971123999749, 212.2146689648959921 ) ) ;
#58183 = VERTEX_POINT ( 'NONE', #99309 ) ;
#58184 = CARTESIAN_POINT ( 'NONE',  ( 11.18741891859999882, 1423.006079699629936, 217.1793481124879861 ) ) ;
#58186 = CARTESIAN_POINT ( 'NONE',  ( -15.15436964682470133, 1512.305164330070056, 221.9485801204349968 ) ) ;
#58185 = CARTESIAN_POINT ( 'NONE',  ( -1.502588279119999815, 1469.871880491130014, 182.3802797567980178 ) ) ;
#58187 = DIRECTION ( 'NONE',  ( -1.836970198721029688E-16, -1.000000000000000000, 0.000000000000000000 ) ) ;
#58188 = CARTESIAN_POINT ( 'NONE',  ( 3.156166260290000025, 1466.544008048530031, 236.1241471695980181 ) ) ;
#58189 = CARTESIAN_POINT ( 'NONE',  ( -29.75012120250000081, 1509.993914124430148, 208.5595671623779879 ) ) ;
#58190 = CARTESIAN_POINT ( 'NONE',  ( -13.86903295495070054, 1452.428743084420148, 148.6123537208110008 ) ) ;
#58191 = CARTESIAN_POINT ( 'NONE',  ( 15.05358515032119904, 1410.831827804430077, 191.5175411757069810 ) ) ;
#58192 = EDGE_LOOP ( 'NONE', ( #3277, #57963, #42779, #70608 ) ) ;
#58193 = CARTESIAN_POINT ( 'NONE',  ( -2.500000000000000000, 1421.745358796729988, 151.9633565684980283 ) ) ;
#58194 = CARTESIAN_POINT ( 'NONE',  ( -0.6164045617451590076, 1407.928388523590002, 270.2926945153609495 ) ) ;
#58195 = CARTESIAN_POINT ( 'NONE',  ( -0.05082476190679999922, 1508.992422786230009, 238.9842641244979973 ) ) ;
#58196 = CARTESIAN_POINT ( 'NONE',  ( 16.99532478070279851, 1414.913372219064513, 210.5807211179420619 ) ) ;
#58197 = ORIENTED_EDGE ( 'NONE', *, *, #37214, .F. ) ;
#58198 = ORIENTED_EDGE ( 'NONE', *, *, #60466, .T. ) ;
#58199 = CARTESIAN_POINT ( 'NONE',  ( -50.84956067560000292, 1384.888209502700192, 226.1736401165590280 ) ) ;
#58200 = CARTESIAN_POINT ( 'NONE',  ( -23.96638063676619979, 1410.422153605740050, 209.1360332124949934 ) ) ;
#58201 = ORIENTED_EDGE ( 'NONE', *, *, #48262, .F. ) ;
#58202 = CARTESIAN_POINT ( 'NONE',  ( 16.19492434978379691, 1409.478599607480191, 224.1775087544979783 ) ) ;
#58203 = CARTESIAN_POINT ( 'NONE',  ( -45.67177343128329881, 1440.913044206929953, 266.1885934837860077 ) ) ;
#58204 = CARTESIAN_POINT ( 'NONE',  ( -0.2366988889530000084, 1507.644349193429889, 237.3561800022980037 ) ) ;
#58205 = CARTESIAN_POINT ( 'NONE',  ( 4.554948888541289875, 1508.731372606449895, 211.6097697255310095 ) ) ;
#58206 = ORIENTED_EDGE ( 'NONE', *, *, #10589, .F. ) ;
#58207 = EDGE_CURVE ( 'NONE', #110792, #101763, #99313, .T. ) ;
#58208 = CARTESIAN_POINT ( 'NONE',  ( 41.99034683523260014, 1455.513645117400074, 268.3446858974320435 ) ) ;
#58209 = VECTOR ( 'NONE', #74408, 1000.000000000000000 ) ;
#58210 = ADVANCED_FACE ( 'NONE', ( #58444, #56788, #38860, #65746, #107732, #14211, #108832, #47831, #64655, #81964, #73038, #107177, #30469, #39425, #31017, #48397, #5836, #39976, #74152, #101511, #18069, #9676, #51145, #92572, #51697, #17500, #24797, #59549, #69625, #59002, #76339, #86388, #84723, #210, #109944, #102610, #93130, #50592, #7475, #41637, #33769, #84177, #85270, #25356, #77450, #8021, #75792, #35438, #25910, #33222 ), #42740, .F. ) ;
#58211 = CARTESIAN_POINT ( 'NONE',  ( -10.62594761801030074, 1391.913060387249971, 205.0845642080600157 ) ) ;
#58212 = CARTESIAN_POINT ( 'NONE',  ( 0.03978530575449999718, 1419.130000249829891, 184.6452573654979972 ) ) ;
#58213 = CARTESIAN_POINT ( 'NONE',  ( -0.01306004006829850073, 1516.939762005280045, 204.5032625402269844 ) ) ;
#58214 = EDGE_LOOP ( 'NONE', ( #34815, #46541, #28308, #88579, #18989, #45177 ) ) ;
#58216 = EDGE_CURVE ( 'NONE', #65907, #87972, #64394, .T. ) ;
#58215 = CARTESIAN_POINT ( 'NONE',  ( -21.63849897585056681, 1521.951704408389787, 215.5584779397909188 ) ) ;
#58217 = CARTESIAN_POINT ( 'NONE',  ( -0.9122102915526030253, 1444.513817941259958, 199.1093392106390070 ) ) ;
#58218 = CARTESIAN_POINT ( 'NONE',  ( 1.282760155569999894, 1429.107748742090052, 214.5111769290890038 ) ) ;
#58219 = ORIENTED_EDGE ( 'NONE', *, *, #6520, .F. ) ;
#58220 = CARTESIAN_POINT ( 'NONE',  ( -10.41578227499199905, 1479.949469769299867, 210.5455296413880149 ) ) ;
#58221 = ADVANCED_FACE ( 'NONE', ( #76901 ), #94225, .T. ) ;
#58222 = CARTESIAN_POINT ( 'NONE',  ( 27.02053382135309789, 1451.952557960830063, 135.1688879843840141 ) ) ;
#58223 = EDGE_CURVE ( 'NONE', #3165, #42483, #79320, .T. ) ;
#58224 = CARTESIAN_POINT ( 'NONE',  ( -12.72383577362860052, 1512.260118274579781, 194.0134362855580150 ) ) ;
#58225 = CARTESIAN_POINT ( 'NONE',  ( 10.74159879227639891, 1502.696702000269852, 215.9649088173380278 ) ) ;
#58226 = CARTESIAN_POINT ( 'NONE',  ( 8.209570662930000040, 1421.454114719120298, 196.1494337501989946 ) ) ;
#58227 = CARTESIAN_POINT ( 'NONE',  ( -0.6675760093930949157, 1432.097311422259963, 218.6006162758970106 ) ) ;
#58228 = CARTESIAN_POINT ( 'NONE',  ( -5.061893406920000338, 1495.006295643590192, 197.8849625455989951 ) ) ;
#58229 = CARTESIAN_POINT ( 'NONE',  ( 11.26174377530239923, 1409.306329145770178, 191.0634772139260065 ) ) ;
#58231 = CARTESIAN_POINT ( 'NONE',  ( -17.73406580063780069, 1423.343214054229975, 226.1884525926029994 ) ) ;
#58230 = CARTESIAN_POINT ( 'NONE',  ( -12.89608512423069975, 1434.724840024559853, 149.2206170422699927 ) ) ;
#58232 = CARTESIAN_POINT ( 'NONE',  ( 2.571344636303355635, 1440.211256060247251, 170.5281974707060044 ) ) ;
#58233 = CARTESIAN_POINT ( 'NONE',  ( -12.29033186280000045, 1380.572208205969901, 215.3566307603289829 ) ) ;
#58234 = CARTESIAN_POINT ( 'NONE',  ( 11.86716023049999968, 1432.353341358199941, 147.6509521729980179 ) ) ;
#58235 = ORIENTED_EDGE ( 'NONE', *, *, #69304, .T. ) ;
#58236 = CARTESIAN_POINT ( 'NONE',  ( 12.81185530964379815, 1416.835419214280137, 221.9980326694370092 ) ) ;
#58237 = DIRECTION ( 'NONE',  ( 0.000000000000000000, 0.000000000000000000, -1.000000000000000000 ) ) ;
#58238 = CARTESIAN_POINT ( 'NONE',  ( 17.01308443848121499, 1414.913060595379648, 210.6742099983445087 ) ) ;
#58239 = CARTESIAN_POINT ( 'NONE',  ( -12.14635843149999950, 1389.476265811170151, 203.8304572938190233 ) ) ;
#58240 = CARTESIAN_POINT ( 'NONE',  ( 11.41293808157470124, 1427.618755674339809, 209.6356236935340007 ) ) ;
#58241 = ADVANCED_FACE ( 'NONE', ( #9138 ), #46495, .F. ) ;
#58242 =( BOUNDED_SURFACE ( )  B_SPLINE_SURFACE ( 3, 2, ( 
 ( #101334, #31953, #92959 ),
 ( #16232, #93502, #14595 ),
 ( #50436, #67784, #48785 ),
 ( #100796, #76718, #76168 ) ),
 .UNSPECIFIED., .F., .F., .T. ) 
 B_SPLINE_SURFACE_WITH_KNOTS ( ( 4, 4 ),
 ( 3, 3 ),
 ( 0.000000000000000000, 0.0002960034161023854899 ),
 ( 0.000000000000000000, 1.000000000000000000 ),
 .UNSPECIFIED. ) 
 GEOMETRIC_REPRESENTATION_ITEM ( )  RATIONAL_B_SPLINE_SURFACE ( (
 ( 1.000000000000000000, 0.8072480644198084532, 1.000000000000000000),
 ( 1.000000000000000000, 0.8072480346917723093, 1.000000000000000000),
 ( 1.000000000000000000, 0.8071723757218308704, 1.000000000000000000),
 ( 1.000000000000000000, 0.8070209408749940971, 1.000000000000000000) ) ) 
 REPRESENTATION_ITEM ( '' )  SURFACE ( )  );
#58243 = CARTESIAN_POINT ( 'NONE',  ( 10.95522075352049995, 1424.091714785270142, 203.1699306280349901 ) ) ;
#58244 = CARTESIAN_POINT ( 'NONE',  ( -10.89732850212739912, 1462.760389868430138, 207.2746260999839762 ) ) ;
#58245 = CARTESIAN_POINT ( 'NONE',  ( -36.06124927020000115, 1445.049634742420039, 262.6648722463980334 ) ) ;
#58246 = CARTESIAN_POINT ( 'NONE',  ( -21.94594868458499093, 1509.533995021516603, 191.4017675758697123 ) ) ;
#58247 = FACE_OUTER_BOUND ( 'NONE', #40985, .T. ) ;
#58248 = CARTESIAN_POINT ( 'NONE',  ( 28.05448517229999794, 1461.575973716330054, 265.6112250856980381 ) ) ;
#58249 = CARTESIAN_POINT ( 'NONE',  ( -9.662959447710280259, 1460.558442627200066, 208.8701083130750078 ) ) ;
#58250 = EDGE_CURVE ( 'NONE', #40999, #74254, #109070, .T. ) ;
#58251 = CIRCLE ( 'NONE', #24251, 1.500000000000001332 ) ;
#58252 = CARTESIAN_POINT ( 'NONE',  ( -16.18976011259663750, 1409.478419268353264, 194.8164317614535150 ) ) ;
#58253 = CARTESIAN_POINT ( 'NONE',  ( -0.9796450454589999968, 1519.913060387329779, 232.6858900125980085 ) ) ;
#58254 = ADVANCED_FACE ( 'NONE', ( #43845 ), #77992, .T. ) ;
#58255 = CARTESIAN_POINT ( 'NONE',  ( 4.647650363794389783, 1467.200465736529850, 217.9234417945369842 ) ) ;
#58256 = CARTESIAN_POINT ( 'NONE',  ( -18.23438631919999864, 1486.008731762530033, 188.8346238057980031 ) ) ;
#58257 = CARTESIAN_POINT ( 'NONE',  ( 5.095760143028649658, 1474.009471786559970, 219.3429060835489963 ) ) ;
#58258 = CARTESIAN_POINT ( 'NONE',  ( -4.487249770485409961, 1509.038615931769982, 206.6339108289169815 ) ) ;
#58259 = CARTESIAN_POINT ( 'NONE',  ( 17.76091713730000166, 1410.905089306629861, 223.3054222800980142 ) ) ;
#58260 = CARTESIAN_POINT ( 'NONE',  ( -25.58458546029999781, 1449.894445106999910, 137.3532228530980035 ) ) ;
#58261 = CARTESIAN_POINT ( 'NONE',  ( -17.06940528265129942, 1409.674914835549998, 193.4350317209980119 ) ) ;
#58262 = CARTESIAN_POINT ( 'NONE',  ( 8.106578671807320281E-07, 1407.561928582239943, 196.0178922782889686 ) ) ;
#58263 = CARTESIAN_POINT ( 'NONE',  ( -4.992349863779999453, 1391.620913471789891, 203.8075142969990168 ) ) ;
#58264 = CARTESIAN_POINT ( 'NONE',  ( 5.140094623760980141, 1436.845495186209973, 228.7442485543419934 ) ) ;
#58265 = CARTESIAN_POINT ( 'NONE',  ( -3.747719220470000057, 1415.426091369430196, 226.7846717995979873 ) ) ;
#58266 = CARTESIAN_POINT ( 'NONE',  ( 0.1694144171801959808, 1480.673780128910039, 182.0654477247749696 ) ) ;
#58268 = ORIENTED_EDGE ( 'NONE', *, *, #43339, .F. ) ;
#58267 = CARTESIAN_POINT ( 'NONE',  ( -4.500000000000000000, 1423.874532569730036, 167.3087045231979744 ) ) ;
#58269 = CARTESIAN_POINT ( 'NONE',  ( 2.596261494520241353, 1525.907212628473644, 177.4701144822246874 ) ) ;
#58270 = CARTESIAN_POINT ( 'NONE',  ( 11.94104774480000053, 1433.615498876629999, 149.8850687855980084 ) ) ;
#58271 = CARTESIAN_POINT ( 'NONE',  ( -40.94560254916699193, 1440.384112706839915, 134.0999999980729740 ) ) ;
#58272 = CARTESIAN_POINT ( 'NONE',  ( -110.0633064609999963, 1384.901791039720138, 296.9512369705590231 ) ) ;
#58273 = ORIENTED_EDGE ( 'NONE', *, *, #77232, .F. ) ;
#58274 = CARTESIAN_POINT ( 'NONE',  ( -17.83486663330525346, 1523.678648413191695, 180.3677388339002334 ) ) ;
#58275 = LINE ( 'NONE', #22984, #4580 ) ;
#58276 = CARTESIAN_POINT ( 'NONE',  ( -104.6561145012381928, 1380.660749972640588, 307.8568443802569732 ) ) ;
#58277 = FACE_OUTER_BOUND ( 'NONE', #17633, .T. ) ;
#58278 = CARTESIAN_POINT ( 'NONE',  ( 19.52205534611780280, 1473.076231017440023, 204.3554433243390065 ) ) ;
#58279 = CARTESIAN_POINT ( 'NONE',  ( -109.0737800152069639, 1382.200485035640668, 310.8665753754681305 ) ) ;
#58280 = CARTESIAN_POINT ( 'NONE',  ( 22.15551762850000017, 1489.466917450329902, 210.2377471049379949 ) ) ;
#58281 = CARTESIAN_POINT ( 'NONE',  ( -12.30978043270000022, 1378.957296234380237, 210.0572917626269884 ) ) ;
#58282 = CARTESIAN_POINT ( 'NONE',  ( 3.829620113550000315, 1515.551704408389924, 210.9648081929590262 ) ) ;
#58283 = CARTESIAN_POINT ( 'NONE',  ( -53.45114155367870268, 1385.032075449320018, 231.0041225493250181 ) ) ;
#58284 = CARTESIAN_POINT ( 'NONE',  ( -10.70151013563189935, 1391.913060387289988, 213.1790326816040135 ) ) ;
#58285 = CARTESIAN_POINT ( 'NONE',  ( 10.64684366344270039, 1425.854810616539908, 207.2965554390950160 ) ) ;
#58286 = ORIENTED_EDGE ( 'NONE', *, *, #86710, .T. ) ;
#58287 = CARTESIAN_POINT ( 'NONE',  ( -29.81974100089999880, 1451.010966676529733, 136.2919626754980129 ) ) ;
#58288 = CARTESIAN_POINT ( 'NONE',  ( -17.02002156968800151, 1410.733189543489971, 226.2282921672789939 ) ) ;
#58289 = AXIS2_PLACEMENT_3D ( 'NONE', #14439, #97898, #48636 ) ;
#58291 = ORIENTED_EDGE ( 'NONE', *, *, #81136, .T. ) ;
#58290 = DIRECTION ( 'NONE',  ( 0.000000000000000000, -1.000000000000000000, 0.000000000000000000 ) ) ;
#58292 = CARTESIAN_POINT ( 'NONE',  ( -109.6575144030000075, 1384.919426084519955, 311.3230337842589961 ) ) ;
#58293 = B_SPLINE_CURVE_WITH_KNOTS ( 'NONE', 5,
 ( #69659, #43336, #109975, #784, #11926, #79148 ),
 .UNSPECIFIED., .F., .F.,
 ( 6, 6 ),
 ( 434.5419185690000177, 439.7519038140000021 ),
 .UNSPECIFIED. ) ;
#58294 = VECTOR ( 'NONE', #3917, 1000.000000000000000 ) ;
#58295 = CARTESIAN_POINT ( 'NONE',  ( -17.56882915975198856, 1410.890595540249024, 225.4874358264362399 ) ) ;
#58296 = CARTESIAN_POINT ( 'NONE',  ( -109.2942948309999878, 1384.591425206880103, 311.2507045772590004 ) ) ;
#58297 = CARTESIAN_POINT ( 'NONE',  ( -0.08394227893480489533, 1419.987834470179905, 183.9790430942110220 ) ) ;
#58298 = CARTESIAN_POINT ( 'NONE',  ( 35.24315337100163248, 1457.507325202675929, 269.5348779185313219 ) ) ;
#58299 = CARTESIAN_POINT ( 'NONE',  ( 9.862951377130659836, 1517.051704408389924, 189.8497022437369708 ) ) ;
#58300 = CARTESIAN_POINT ( 'NONE',  ( -16.14423341240000198, 1422.196820606129904, 227.3644137178979747 ) ) ;
#58301 = CARTESIAN_POINT ( 'NONE',  ( -3.059258307290346313, 1511.948750846285975, 201.2117255214971294 ) ) ;
#58302 = CARTESIAN_POINT ( 'NONE',  ( 10.34950180350000082, 1451.639534145589778, 207.2650128738690114 ) ) ;
#58303 = CARTESIAN_POINT ( 'NONE',  ( -107.1941519259530082, 1348.229899472569969, 304.2218459572590064 ) ) ;
#58304 = CARTESIAN_POINT ( 'NONE',  ( 3.294994957250000134, 1408.913060387329779, 226.6118641217979928 ) ) ;
#58305 = CARTESIAN_POINT ( 'NONE',  ( -0.0007469751400547060965, 1455.736088183790116, 198.5579702233989963 ) ) ;
#58306 = ADVANCED_FACE ( 'NONE', ( #104852 ), #90293, .T. ) ;
#58307 = CARTESIAN_POINT ( 'NONE',  ( -4.624099329465000352, 1516.962555622980062, 205.8665050058069994 ) ) ;
#58308 = CARTESIAN_POINT ( 'NONE',  ( 2.500000000000000000, 1448.191388957269965, 168.9995349768979906 ) ) ;
#58309 = VERTEX_POINT ( 'NONE', #66180 ) ;
#58310 = CARTESIAN_POINT ( 'NONE',  ( -109.1645132478509908, 1384.901512804259937, 297.1326343494729940 ) ) ;
#58311 = CARTESIAN_POINT ( 'NONE',  ( -4.231842431855520559, 1441.513933367780055, 164.4206257021209865 ) ) ;
#58313 = ORIENTED_EDGE ( 'NONE', *, *, #49553, .T. ) ;
#58312 = CARTESIAN_POINT ( 'NONE',  ( -68.55621501180290522, 1379.747479911359960, 280.1551959466660264 ) ) ;
#58314 = CARTESIAN_POINT ( 'NONE',  ( -17.53532366528470021, 1417.850058971930139, 206.8376673564200132 ) ) ;
#58315 = ORIENTED_EDGE ( 'NONE', *, *, #82542, .F. ) ;
#58316 = CARTESIAN_POINT ( 'NONE',  ( -16.06220695246549113, 1512.836811624631537, 220.2343054163481781 ) ) ;
#58317 = AXIS2_PLACEMENT_3D ( 'NONE', #63958, #71832, #20807 ) ;
#58318 = FACE_OUTER_BOUND ( 'NONE', #96747, .T. ) ;
#58320 = CARTESIAN_POINT ( 'NONE',  ( 16.36854146560279943, 1410.124658228839962, 191.8480414016150064 ) ) ;
#58319 = CARTESIAN_POINT ( 'NONE',  ( -11.63658677818990128, 1425.864905157940257, 144.1610764294569833 ) ) ;
#58321 = CARTESIAN_POINT ( 'NONE',  ( -4.608146819384999482, 1516.677239312369920, 211.4179708211670174 ) ) ;
#58322 = CARTESIAN_POINT ( 'NONE',  ( 34.91588500242689719, 1437.049151938289924, 136.5304996461299822 ) ) ;
#58323 = EDGE_CURVE ( 'NONE', #94600, #102101, #57303, .T. ) ;
#58324 = CARTESIAN_POINT ( 'NONE',  ( -11.73643181629999965, 1426.280401702830204, 144.1638243106980042 ) ) ;
#58325 = CARTESIAN_POINT ( 'NONE',  ( -0.0001187281342228439996, 1508.967929526819944, 179.3767679645770272 ) ) ;
#58326 = CARTESIAN_POINT ( 'NONE',  ( 17.10224595388506330, 1460.321307548461164, 228.6740676894672788 ) ) ;
#58327 = PRODUCT_CONTEXT ( 'NONE', #70655, 'mechanical' ) ;
#58328 = CARTESIAN_POINT ( 'NONE',  ( 38.20286890328719664, 1450.309401038089845, 134.0999999984079807 ) ) ;
#58329 = CARTESIAN_POINT ( 'NONE',  ( -40.27308906366239682, 1443.612067134240078, 137.1163379626329970 ) ) ;
#58330 = VERTEX_POINT ( 'NONE', #98639 ) ;
#58331 = CARTESIAN_POINT ( 'NONE',  ( -9.838224505759999516, 1462.268909614690074, 227.9668215275989667 ) ) ;
#58332 = DIRECTION ( 'NONE',  ( -0.09872117914509953573, 0.9946471739456684835, 0.03051439250741381365 ) ) ;
#58333 = ORIENTED_EDGE ( 'NONE', *, *, #11251, .F. ) ;
#58334 = ORIENTED_EDGE ( 'NONE', *, *, #78287, .T. ) ;
#58335 = CARTESIAN_POINT ( 'NONE',  ( -29.47787601289847714, 1509.952111658624290, 211.1326834024595200 ) ) ;
#58336 = CARTESIAN_POINT ( 'NONE',  ( -17.06941237829999736, 1409.674943312830010, 194.0661809782980072 ) ) ;
#58337 = B_SPLINE_CURVE_WITH_KNOTS ( 'NONE', 5,
 ( #99153, #92835, #67114, #34036, #34588, #102333 ),
 .UNSPECIFIED., .F., .F.,
 ( 6, 6 ),
 ( 0.000000000000000000, 1.000000000000000000 ),
 .UNSPECIFIED. ) ;
#58338 = CARTESIAN_POINT ( 'NONE',  ( -5.668982378084499452, 1507.922364110239869, 220.7207090108649936 ) ) ;
#58339 = CARTESIAN_POINT ( 'NONE',  ( -16.88207931438999765, 1507.985365216929949, 209.4467744516990138 ) ) ;
#58340 = CARTESIAN_POINT ( 'NONE',  ( 3.984081752360000284, 1515.551704408389924, 210.9648081929590262 ) ) ;
#58341 = CARTESIAN_POINT ( 'NONE',  ( -27.89972997509999786, 1508.077281474930032, 206.8466243103179920 ) ) ;
#58342 = CARTESIAN_POINT ( 'NONE',  ( 42.60628463920169651, 1443.705283414120004, 135.0591082134169767 ) ) ;
#58343 = CARTESIAN_POINT ( 'NONE',  ( 2.446740381308137646, 1516.554415856208834, 216.2144072986330343 ) ) ;
#58344 = EDGE_CURVE ( 'NONE', #45409, #77352, #20380, .T. ) ;
#58345 = CARTESIAN_POINT ( 'NONE',  ( 26.06817282160000104, 1439.608707811800059, 137.5105934946979858 ) ) ;
#58346 = FACE_OUTER_BOUND ( 'NONE', #21496, .T. ) ;
#58347 = CARTESIAN_POINT ( 'NONE',  ( -85.41229846784960955, 1384.819622699739966, 289.1167610944229978 ) ) ;
#58348 = ORIENTED_EDGE ( 'NONE', *, *, #95410, .T. ) ;
#58349 = CARTESIAN_POINT ( 'NONE',  ( -1.129386240404999908, 1516.613712827999962, 201.7984555248870038 ) ) ;
#58350 = CARTESIAN_POINT ( 'NONE',  ( 6.550870144104999682, 1516.727502608469877, 208.3674577492799926 ) ) ;
#58351 = ORIENTED_EDGE ( 'NONE', *, *, #11652, .T. ) ;
#58353 = ADVANCED_FACE ( 'NONE', ( #82407 ), #5703, .T. ) ;
#58352 = CARTESIAN_POINT ( 'NONE',  ( 11.82617426117190007, 1429.667056798789872, 149.2970047124300095 ) ) ;
#58354 = CARTESIAN_POINT ( 'NONE',  ( 4.433893130974031038, 1511.410080502447272, 217.4576852855098252 ) ) ;
#58355 = EDGE_LOOP ( 'NONE', ( #8682, #68757 ) ) ;
#58356 = CARTESIAN_POINT ( 'NONE',  ( -14.34198504589999956, 1416.067629296030191, 221.2727144154980010 ) ) ;
#58357 = CARTESIAN_POINT ( 'NONE',  ( -11.30564195107439929, 1432.342987153669810, 151.4629878985130063 ) ) ;
#58358 = DIRECTION ( 'NONE',  ( 0.9076061524720632212, 0.000000000000000000, -0.4198226673190215696 ) ) ;
#58359 = CARTESIAN_POINT ( 'NONE',  ( -10.37041358865520024, 1462.696929687640022, 206.9223858279979993 ) ) ;
#58360 = CARTESIAN_POINT ( 'NONE',  ( 21.99869784864110400, 1409.975627104619889, 206.2846292323520174 ) ) ;
#58361 = DIRECTION ( 'NONE',  ( -6.123233995736769734E-17, -1.000000000000000000, 7.888609052210119587E-33 ) ) ;
#58362 = CARTESIAN_POINT ( 'NONE',  ( -10.74194911459999879, 1471.560973731990089, 206.8675634873690115 ) ) ;
#58363 = CARTESIAN_POINT ( 'NONE',  ( -10.62228157299999864, 1490.415513672490079, 212.3812309668689977 ) ) ;
#58364 = CARTESIAN_POINT ( 'NONE',  ( -54.34609671659999464, 1379.710116771220100, 248.9718466677589959 ) ) ;
#58365 = CARTESIAN_POINT ( 'NONE',  ( 23.73948244347349856, 1437.917305470170049, 206.2095067639299941 ) ) ;
#58366 = ADVANCED_FACE ( 'NONE', ( #51556 ), #25774, .F. ) ;
#58368 = CARTESIAN_POINT ( 'NONE',  ( 1.925297170580940076, 1517.151704408390060, 230.6853930747409720 ) ) ;
#58367 = CARTESIAN_POINT ( 'NONE',  ( 13.85688183060000078, 1460.822580857430012, 232.2031414462979910 ) ) ;
#58369 = DIRECTION ( 'NONE',  ( -1.305148739725796033E-31, 1.000000000000000000, -1.836970198721029688E-16 ) ) ;
#58370 = CARTESIAN_POINT ( 'NONE',  ( 3.260378255074999565, 1516.582197289609894, 216.8321318079170226 ) ) ;
#58371 = ORIENTED_EDGE ( 'NONE', *, *, #11350, .F. ) ;
#58372 = ADVANCED_FACE ( 'NONE', ( #109806 ), #92138, .F. ) ;
#58373 = CARTESIAN_POINT ( 'NONE',  ( -4.378216884482949212, 1453.707746088449994, 199.6107954155660025 ) ) ;
#58374 = CARTESIAN_POINT ( 'NONE',  ( -0.2726138066919999714, 1487.235664587629799, 230.5521328613980074 ) ) ;
#58375 = CARTESIAN_POINT ( 'NONE',  ( -21.83550407203881960, 1523.678648413191695, 234.9693198511253911 ) ) ;
#58376 = CARTESIAN_POINT ( 'NONE',  ( -7.711550716115000093, 1516.630499592039996, 213.1573366827869904 ) ) ;
#58377 = CARTESIAN_POINT ( 'NONE',  ( 3.829164872245370166, 1515.551704201149960, 211.4518032850860152 ) ) ;
#58378 = CARTESIAN_POINT ( 'NONE',  ( -11.60004869885776024, 1425.683027346956351, 138.3963214575541940 ) ) ;
#58380 = ORIENTED_EDGE ( 'NONE', *, *, #98330, .T. ) ;
#58379 = CARTESIAN_POINT ( 'NONE',  ( -11.72416936767639939, 1501.387581424680093, 211.3308819256019717 ) ) ;
#58381 = CARTESIAN_POINT ( 'NONE',  ( -7.966233669470000223, 1384.910919823659924, 199.4893341005590059 ) ) ;
#58382 = CARTESIAN_POINT ( 'NONE',  ( -15.54603058869099996, 1507.439214557209880, 192.4074551458910207 ) ) ;
#58383 = CARTESIAN_POINT ( 'NONE',  ( -11.81867802130000022, 1429.211286938129888, 149.0416137968979911 ) ) ;
#58384 = CARTESIAN_POINT ( 'NONE',  ( 19.02876048740180082, 1456.918022623920024, 225.5897448336330058 ) ) ;
#58385 = CARTESIAN_POINT ( 'NONE',  ( -109.8241992154370053, 1383.739369478020080, 311.3440882120070228 ) ) ;
#58386 = DIRECTION ( 'NONE',  ( 0.5781790699150771706, 0.04201035868947775725, 0.8148276461159855710 ) ) ;
#58387 = CARTESIAN_POINT ( 'NONE',  ( -8.316672828268760753, 1425.055149638239982, 204.9623390585310005 ) ) ;
#58388 = EDGE_CURVE ( 'NONE', #86873, #71251, #42051, .T. ) ;
#58389 = CARTESIAN_POINT ( 'NONE',  ( -2.471608048749999842, 1438.194204504490017, 150.4833623973980252 ) ) ;
#58391 = CARTESIAN_POINT ( 'NONE',  ( -10.26804317657019894, 1481.277325295010087, 206.6051681627829737 ) ) ;
#58390 = CARTESIAN_POINT ( 'NONE',  ( -21.04359474530000185, 1482.728143256829981, 225.6449476673980143 ) ) ;
#58392 = CARTESIAN_POINT ( 'NONE',  ( -4.018690540569999747, 1470.826407316289988, 215.3451084216990239 ) ) ;
#58393 = VERTEX_POINT ( 'NONE', #1167 ) ;
#58394 = CARTESIAN_POINT ( 'NONE',  ( 4.028307740155000261, 1516.797038924770050, 205.8554964580370097 ) ) ;
#58395 = CARTESIAN_POINT ( 'NONE',  ( 3.767309702620000422, 1405.959571974130085, 267.2290117651980381 ) ) ;
#58396 = EDGE_CURVE ( 'NONE', #70982, #56035, #11096, .T. ) ;
#58397 = CARTESIAN_POINT ( 'NONE',  ( -0.001550886560859999954, 1408.913006230129895, 186.0211967747979998 ) ) ;
#58398 = CARTESIAN_POINT ( 'NONE',  ( 20.00430653580000140, 1449.729862604200207, 193.6333489802979955 ) ) ;
#58399 = CIRCLE ( 'NONE', #36948, 0.9999999999999326095 ) ;
#58400 = CARTESIAN_POINT ( 'NONE',  ( 7.527653235111040786, 1506.538134868789029, 229.8708666564015175 ) ) ;
#58401 = CARTESIAN_POINT ( 'NONE',  ( 2.395226819458120104, 1454.514303657540040, 218.2121819530340190 ) ) ;
#58402 = CARTESIAN_POINT ( 'NONE',  ( -0.5133638609672289688, 1410.311096993930050, 233.1717005261690190 ) ) ;
#58403 = CARTESIAN_POINT ( 'NONE',  ( -18.51604897466450694, 1457.427690017132363, 227.8249311439416829 ) ) ;
#58404 = CARTESIAN_POINT ( 'NONE',  ( -15.01368523340000216, 1416.900385880339854, 204.9748714204190208 ) ) ;
#58405 = CARTESIAN_POINT ( 'NONE',  ( -14.45727104390000051, 1444.967096565130078, 188.7843282767979929 ) ) ;
#58406 = CARTESIAN_POINT ( 'NONE',  ( -3.594043688008891291, 1496.396823991950669, 219.7606401984895967 ) ) ;
#58407 = CARTESIAN_POINT ( 'NONE',  ( -15.89250414441243464, 1419.836041960068769, 210.6346457996376955 ) ) ;
#58408 = CARTESIAN_POINT ( 'NONE',  ( 0.4918993947909917619, 1407.650947846033205, 270.1377426664976156 ) ) ;
#58409 = CIRCLE ( 'NONE', #78064, 1.999999999999998668 ) ;
#58410 = CARTESIAN_POINT ( 'NONE',  ( 1.463365724432849957, 1492.705009941090111, 181.7417394025019917 ) ) ;
#58411 = DIRECTION ( 'NONE',  ( 0.7071067811865490160, 0.000000000000000000, -0.7071067811865461294 ) ) ;
#58412 = CARTESIAN_POINT ( 'NONE',  ( -11.95661960621089825, 1507.899396442559919, 208.5587272349789885 ) ) ;
#58413 = CARTESIAN_POINT ( 'NONE',  ( 21.19077256501174844, 1525.394081235439444, 234.2786530305002657 ) ) ;
#58414 = CARTESIAN_POINT ( 'NONE',  ( -3.444139561100000080, 1476.012962394230044, 267.8489069608979776 ) ) ;
#58415 = CARTESIAN_POINT ( 'NONE',  ( -4.227395202513110739, 1446.270036243080085, 165.6810918684970204 ) ) ;
#58416 = CARTESIAN_POINT ( 'NONE',  ( -13.24074056834217217, 1513.560729025362889, 192.3374869004694574 ) ) ;
#58417 = CARTESIAN_POINT ( 'NONE',  ( -13.51891076255363089, 1486.505240369647936, 185.1172359407312342 ) ) ;
#58418 = CARTESIAN_POINT ( 'NONE',  ( -52.91565643769759930, 1384.726266332619844, 267.6878703111970026 ) ) ;
#58419 = CARTESIAN_POINT ( 'NONE',  ( 2.798741256952680168, 1509.010794585639815, 238.1786444310339732 ) ) ;
#58420 = CARTESIAN_POINT ( 'NONE',  ( -12.00000000000000000, 1443.913060387330006, 150.5878346084980137 ) ) ;
#58421 = CARTESIAN_POINT ( 'NONE',  ( -25.73740863305900106, 1482.722876254420044, 212.0196469772590149 ) ) ;
#58422 = CARTESIAN_POINT ( 'NONE',  ( 4.290508147089998836, 1515.379315998089851, 208.7552087591940051 ) ) ;
#58423 = DIRECTION ( 'NONE',  ( -8.832268201338159945E-47, 1.000000000000000000, -1.836970198721029688E-16 ) ) ;
#58424 = CARTESIAN_POINT ( 'NONE',  ( -19.24979467460000038, 1409.749958184729849, 197.9967212150980060 ) ) ;
#58425 = CARTESIAN_POINT ( 'NONE',  ( -10.50535462500723938, 1379.632225880806118, 202.6061242926490422 ) ) ;
#58426 = CARTESIAN_POINT ( 'NONE',  ( -0.4986843622567649348, 1508.982343520079894, 238.8510830230749775 ) ) ;
#58427 = CARTESIAN_POINT ( 'NONE',  ( -9.858902522070000174, 1408.321029724029813, 270.1194230524980071 ) ) ;
#58428 = ORIENTED_EDGE ( 'NONE', *, *, #37201, .F. ) ;
#58429 = CARTESIAN_POINT ( 'NONE',  ( -0.5133638609672289688, 1410.311096993930050, 233.1717005261690190 ) ) ;
#58430 = CARTESIAN_POINT ( 'NONE',  ( -19.86701999479999969, 1444.364638085089837, 213.3580800903289969 ) ) ;
#58431 = CARTESIAN_POINT ( 'NONE',  ( -7.461942747583736768, 1510.835436364141515, 215.2999418035631152 ) ) ;
#58432 = CARTESIAN_POINT ( 'NONE',  ( 14.17511108698380085, 1428.761363100300059, 195.0897028359609919 ) ) ;
#58434 = LINE ( 'NONE', #93118, #64749 ) ;
#58433 = FACE_OUTER_BOUND ( 'NONE', #50374, .T. ) ;
#58435 = FACE_OUTER_BOUND ( 'NONE', #6474, .T. ) ;
#58436 = CARTESIAN_POINT ( 'NONE',  ( -6.616507082082380364, 1517.051706634759967, 205.3940390167639976 ) ) ;
#58437 = CARTESIAN_POINT ( 'NONE',  ( 8.129906402815519684, 1449.255237000160150, 202.7301597656260128 ) ) ;
#58438 = CARTESIAN_POINT ( 'NONE',  ( 0.000000000000000000, 1511.187213306747708, 209.1218459616979999 ) ) ;
#58439 = EDGE_CURVE ( 'NONE', #46666, #55409, #94837, .T. ) ;
#58440 = CARTESIAN_POINT ( 'NONE',  ( -4.038637500854999729, 1516.734985836460055, 203.3481771172569950 ) ) ;
#58441 = CARTESIAN_POINT ( 'NONE',  ( -0.1955981719786639705, 1416.913060341709979, 193.0575580088199956 ) ) ;
#58442 = CARTESIAN_POINT ( 'NONE',  ( -12.49651378394149148, 1398.283529688983435, 205.2589461638358443 ) ) ;
#58443 = CARTESIAN_POINT ( 'NONE',  ( 15.38132086023500023, 1512.167884426309911, 196.2735975057670146 ) ) ;
#58444 = FACE_BOUND ( 'NONE', #19227, .T. ) ;
#58445 = CARTESIAN_POINT ( 'NONE',  ( -11.32057025491729974, 1380.342214975079969, 210.2587660409990349 ) ) ;
#58446 = CARTESIAN_POINT ( 'NONE',  ( 20.11526801819819710, 1508.362997783120136, 229.0140906582849993 ) ) ;
#58449 = ORIENTED_EDGE ( 'NONE', *, *, #93867, .F. ) ;
#58448 = CARTESIAN_POINT ( 'NONE',  ( -26.04300106147669780, 1379.718900503969962, 215.2617740064779923 ) ) ;
#58447 = AXIS2_PLACEMENT_3D ( 'NONE', #50441, #59949, #75640 ) ;
#58450 = ORIENTED_EDGE ( 'NONE', *, *, #104758, .F. ) ;
#58451 = CARTESIAN_POINT ( 'NONE',  ( 11.78634442959999973, 1433.876985662710013, 150.9130302334980058 ) ) ;
#58452 = CARTESIAN_POINT ( 'NONE',  ( -11.28524207019999892, 1396.366239101729889, 212.5318391717879933 ) ) ;
#58453 = ORIENTED_EDGE ( 'NONE', *, *, #19366, .F. ) ;
#58454 = CARTESIAN_POINT ( 'NONE',  ( -1.551161424019060098, 1463.265709907049995, 199.4650991780359846 ) ) ;
#58455 = DIRECTION ( 'NONE',  ( 2.048418183714850102E-08, 0.03085826933284185197, -0.9995237702094840193 ) ) ;
#58456 = CARTESIAN_POINT ( 'NONE',  ( 3.912776123226219926, 1515.493282983300105, 205.6567928634579800 ) ) ;
#58458 = CARTESIAN_POINT ( 'NONE',  ( -1.658081806242819971E-15, 1375.886883438980021, 209.1218459572589836 ) ) ;
#58457 = CARTESIAN_POINT ( 'NONE',  ( 1.236701001219999929, 1445.191800647990021, 199.4886538942189986 ) ) ;
#58459 = CARTESIAN_POINT ( 'NONE',  ( 16.69463186169999958, 1507.812162581230041, 231.3306424561980066 ) ) ;
#58460 = EDGE_CURVE ( 'NONE', #70320, #44418, #70589, .T. ) ;
#58461 = CARTESIAN_POINT ( 'NONE',  ( 5.538579248009999567, 1468.700840589029895, 183.8662599229979833 ) ) ;
#58462 = CARTESIAN_POINT ( 'NONE',  ( -12.26359197939999923, 1416.522662136229883, 194.6757565915980024 ) ) ;
#58463 = CARTESIAN_POINT ( 'NONE',  ( 22.03465957474570658, 1512.187213306747481, 235.4136513321629991 ) ) ;
#58464 =( NAMED_UNIT ( * ) PLANE_ANGLE_UNIT ( ) SI_UNIT ( $, .RADIAN. ) );
#58465 = CARTESIAN_POINT ( 'NONE',  ( 8.134874095680000750, 1436.133436978890131, 226.1977348306990336 ) ) ;
#58466 = CARTESIAN_POINT ( 'NONE',  ( 2.500000000000000000, 1419.437602159330027, 141.5609288386980040 ) ) ;
#58467 = CARTESIAN_POINT ( 'NONE',  ( 11.77006340779999860, 1432.381006235819996, 150.8117714391979973 ) ) ;
#58468 = CARTESIAN_POINT ( 'NONE',  ( 40.27308735900000158, 1443.611949368910018, 137.1163358467979947 ) ) ;
#58469 = VERTEX_POINT ( 'NONE', #53226 ) ;
#58470 = CARTESIAN_POINT ( 'NONE',  ( 13.03861301673589956, 1434.799502881549870, 149.2342568181190074 ) ) ;
#58471 = ADVANCED_FACE ( 'NONE', ( #104705 ), #100176, .T. ) ;
#58472 = ORIENTED_EDGE ( 'NONE', *, *, #78189, .F. ) ;
#58473 = ORIENTED_EDGE ( 'NONE', *, *, #47380, .F. ) ;
#58474 = CARTESIAN_POINT ( 'NONE',  ( 13.50347664955267213, 1444.084118611255917, 169.3539558340694384 ) ) ;
#58475 = CARTESIAN_POINT ( 'NONE',  ( -6.719960884899998987, 1465.583908313830079, 233.8333315335979989 ) ) ;
#58476 = CARTESIAN_POINT ( 'NONE',  ( -109.8754351979164738, 1385.888632332895668, 311.3751271473491329 ) ) ;
#58477 = AXIS2_PLACEMENT_3D ( 'NONE', #28751, #105461, #97066 ) ;
#58478 = CARTESIAN_POINT ( 'NONE',  ( -3.259101837015000225, 1517.102359858469754, 216.0714209178769920 ) ) ;
#58479 = CARTESIAN_POINT ( 'NONE',  ( -7.891777529692960869, 1512.314860027450095, 212.0638759934929851 ) ) ;
#58480 = EDGE_LOOP ( 'NONE', ( #43489, #5408, #108509, #76093, #13122 ) ) ;
#58481 = CARTESIAN_POINT ( 'NONE',  ( -11.60962210859999821, 1502.036214399190158, 208.5035594193370230 ) ) ;
#58482 = CARTESIAN_POINT ( 'NONE',  ( 2.500000000000000000, 1448.295510712299802, 164.4143809015409659 ) ) ;
#58483 = CARTESIAN_POINT ( 'NONE',  ( -11.47183536569999873, 1380.342188321910044, 208.5259290606079787 ) ) ;
#58484 = ORIENTED_EDGE ( 'NONE', *, *, #52321, .T. ) ;
#58485 = CARTESIAN_POINT ( 'NONE',  ( 2.478306819944999795, 1516.938330505699923, 205.6592251139969960 ) ) ;
#58486 = VERTEX_POINT ( 'NONE', #20678 ) ;
#58487 = CARTESIAN_POINT ( 'NONE',  ( 1.127928333405000094, 1516.989863902050047, 209.1117210464550169 ) ) ;
#58488 = CARTESIAN_POINT ( 'NONE',  ( -20.01040017649999925, 1508.355603652830041, 229.1813846036980067 ) ) ;
#58489 = EDGE_CURVE ( 'NONE', #87976, #108859, #52667, .T. ) ;
#58490 = CARTESIAN_POINT ( 'NONE',  ( -11.19668478630000052, 1409.304057235629898, 189.9697753155979854 ) ) ;
#58491 = CARTESIAN_POINT ( 'NONE',  ( 7.779264690585000253, 1514.199187793469946, 215.8377718132869916 ) ) ;
#58492 = EDGE_CURVE ( 'NONE', #60257, #50191, #12515, .T. ) ;
#58494 = ORIENTED_EDGE ( 'NONE', *, *, #94459, .F. ) ;
#58493 = CARTESIAN_POINT ( 'NONE',  ( -0.3166099825070000096, 1416.237488680629895, 227.4124177731980012 ) ) ;
#58495 = CARTESIAN_POINT ( 'NONE',  ( 22.48557446689999750, 1431.347824966569760, 217.2207584623980097 ) ) ;
#58496 = CARTESIAN_POINT ( 'NONE',  ( -16.03794089777630205, 1508.551704408389924, 210.3786724331339997 ) ) ;
#58497 = DIRECTION ( 'NONE',  ( 1.835183309750130004E-16, 1.000000000000000000, 1.599799320660000123E-19 ) ) ;
#58498 = CARTESIAN_POINT ( 'NONE',  ( 0.002041696164862339888, 1465.101599726780023, 237.0127939912499926 ) ) ;
#58499 = ADVANCED_FACE ( 'NONE', ( #20141 ), #8122, .F. ) ;
#58500 = CARTESIAN_POINT ( 'NONE',  ( 13.37958332529999872, 1410.033118652530220, 270.4094488018980087 ) ) ;
#58501 = CARTESIAN_POINT ( 'NONE',  ( 3.264778779384999829, 1516.727068157269969, 214.1190961241369735 ) ) ;
#58502 = ADVANCED_FACE ( 'NONE', ( #60822 ), #68008, .T. ) ;
#58503 = CARTESIAN_POINT ( 'NONE',  ( 24.13371414729999742, 1410.980460536530018, 209.3325957110889988 ) ) ;
#58504 = CARTESIAN_POINT ( 'NONE',  ( 24.08426297012860218, 1411.115209414830133, 209.6325633951909708 ) ) ;
#58505 = CARTESIAN_POINT ( 'NONE',  ( 12.32608557850170072, 1492.201684892610047, 209.6317255076330071 ) ) ;
#58506 = CARTESIAN_POINT ( 'NONE',  ( 21.82415348264087740, 1524.756004293092474, 184.6268171959276287 ) ) ;
#58507 = CARTESIAN_POINT ( 'NONE',  ( 2.881548424445000034, 1516.909589401870107, 211.4054166033970148 ) ) ;
#58508 = CARTESIAN_POINT ( 'NONE',  ( -2.936501545661585055, 1447.710472861017934, 154.8059207791675647 ) ) ;
#58509 = CARTESIAN_POINT ( 'NONE',  ( 17.43549125882616124, 1525.211477436245787, 181.0323534358458062 ) ) ;
#58510 = CARTESIAN_POINT ( 'NONE',  ( 0.000000000000000000, 1377.913060387289988, 209.1218459616989946 ) ) ;
#58512 = EDGE_LOOP ( 'NONE', ( #54611, #34102, #102032, #76818 ) ) ;
#58511 = CARTESIAN_POINT ( 'NONE',  ( -44.22662318030000250, 1388.378119737989891, 246.9464660031590029 ) ) ;
#58513 = CARTESIAN_POINT ( 'NONE',  ( -50.55048253121940149, 1385.118695880380074, 262.8599624479500108 ) ) ;
#58514 = CARTESIAN_POINT ( 'NONE',  ( 37.17593098820000108, 1458.776684284729981, 264.1765544691980381 ) ) ;
#58515 = CARTESIAN_POINT ( 'NONE',  ( -3.877733327704724342, 1370.349513340957628, 208.3133770646377059 ) ) ;
#58516 = CARTESIAN_POINT ( 'NONE',  ( 1.481577638361565530, 1494.010533848515024, 220.1478854846517947 ) ) ;
#58517 = EDGE_CURVE ( 'NONE', #102115, #104584, #80535, .T. ) ;
#58518 = CARTESIAN_POINT ( 'NONE',  ( -5.388302382240000021, 1432.653872217849994, 154.6144426912980236 ) ) ;
#58519 = CARTESIAN_POINT ( 'NONE',  ( -22.79362109059999852, 1450.012765720310199, 219.0613567770580232 ) ) ;
#58520 = CARTESIAN_POINT ( 'NONE',  ( 0.2227148572559347062, 1444.496034457048154, 218.0821367963589239 ) ) ;
#58521 = CIRCLE ( 'NONE', #10228, 7.999657266239995401 ) ;
#58522 =( REPRESENTATION_RELATIONSHIP ('NONE','NONE', #14372, #83713 ) REPRESENTATION_RELATIONSHIP_WITH_TRANSFORMATION ( #75682 )SHAPE_REPRESENTATION_RELATIONSHIP( ) );
#58524 = DIRECTION ( 'NONE',  ( -0.7071067811865475727, 2.497298964526426743E-16, 0.7071067811865475727 ) ) ;
#58523 = DIRECTION ( 'NONE',  ( -0.000000000000000000, -0.000000000000000000, 1.000000000000000000 ) ) ;
#58525 = CARTESIAN_POINT ( 'NONE',  ( 11.87563351815570023, 1433.006677199550040, 147.6591432317509884 ) ) ;
#58526 = CARTESIAN_POINT ( 'NONE',  ( 33.42844755917196409, 1522.382868172863937, 222.1271778627165929 ) ) ;
#58527 = ORIENTED_EDGE ( 'NONE', *, *, #17808, .F. ) ;
#58528 = CARTESIAN_POINT ( 'NONE',  ( 6.939219482805000005, 1516.783701990830195, 203.3409846960470020 ) ) ;
#58529 = EDGE_CURVE ( 'NONE', #6757, #101455, #40420, .T. ) ;
#58530 = CARTESIAN_POINT ( 'NONE',  ( -0.04744486741469999824, 1487.212584747929895, 230.3635807236979929 ) ) ;
#58531 = CIRCLE ( 'NONE', #28143, 26.43993992909998525 ) ;
#58532 = CARTESIAN_POINT ( 'NONE',  ( 20.89213389120000031, 1453.805113726430136, 224.2163675376980052 ) ) ;
#58533 = CARTESIAN_POINT ( 'NONE',  ( 10.95575241281549950, 1461.178150784580112, 209.3116150371660069 ) ) ;
#58534 = EDGE_CURVE ( 'NONE', #81290, #16271, #75108, .T. ) ;
#58535 = CARTESIAN_POINT ( 'NONE',  ( -7.557465101040457434, 1461.895601300565204, 203.0080691329112881 ) ) ;
#58536 = CARTESIAN_POINT ( 'NONE',  ( 4.440234083720000058, 1466.830466837689983, 218.1566789410989884 ) ) ;
#58537 = CARTESIAN_POINT ( 'NONE',  ( 14.29986306199981705, 1420.106603705138014, 228.3309057200090706 ) ) ;
#58538 = CARTESIAN_POINT ( 'NONE',  ( 26.81568938926840318, 1435.910991003079971, 136.5211442880660115 ) ) ;
#58539 = CARTESIAN_POINT ( 'NONE',  ( -105.5774816291841915, 1391.233265412462515, 302.6220820957303772 ) ) ;
#58540 = CARTESIAN_POINT ( 'NONE',  ( -20.86012771369999896, 1428.511789623030154, 221.0723165858979939 ) ) ;
#58541 = CARTESIAN_POINT ( 'NONE',  ( -45.28159994719300840, 1445.743959104784381, 268.9845966081527990 ) ) ;
#58542 = CARTESIAN_POINT ( 'NONE',  ( -109.5642235760000034, 1387.004236421979840, 297.2531471322589596 ) ) ;
#58543 = CARTESIAN_POINT ( 'NONE',  ( 12.57505856210000061, 1509.295204559930198, 183.4866265921980073 ) ) ;
#58544 = CARTESIAN_POINT ( 'NONE',  ( -20.68299495988535242, 1525.856064936169560, 184.2887581975230376 ) ) ;
#58545 = CARTESIAN_POINT ( 'NONE',  ( -29.35411896400288612, 1462.717522830221014, 269.4640705128969671 ) ) ;
#58546 = ORIENTED_EDGE ( 'NONE', *, *, #78200, .T. ) ;
#58547 = DIRECTION ( 'NONE',  ( 0.000000000000000000, 0.000000000000000000, 1.000000000000000000 ) ) ;
#58548 = CARTESIAN_POINT ( 'NONE',  ( -34.55887780631552886, 1418.580484962596984, 269.2604001755976242 ) ) ;
#58549 = CARTESIAN_POINT ( 'NONE',  ( 736.9598419237370308, 11220.04953453921007, 2047.362669009807405 ) ) ;
#58550 = CARTESIAN_POINT ( 'NONE',  ( -113.4000000000000057, 1305.913060387289988, 304.2218459572590064 ) ) ;
#58551 = CARTESIAN_POINT ( 'NONE',  ( -0.004559919551130000963, 1417.346727339029940, 235.5710182631979706 ) ) ;
#58552 = VECTOR ( 'NONE', #65151, 1000.000000000000000 ) ;
#58553 = CARTESIAN_POINT ( 'NONE',  ( 24.95756540081792707, 1451.613964887439806, 137.4741668746740686 ) ) ;
#58554 = CARTESIAN_POINT ( 'NONE',  ( -8.724201986094810124, 1437.633551000330044, 210.3037638580349835 ) ) ;
#58555 = CARTESIAN_POINT ( 'NONE',  ( -3.829222816047260114, 1515.551704203360032, 211.9228904752730216 ) ) ;
#58556 = CARTESIAN_POINT ( 'NONE',  ( -7.429475295173068261, 1416.924823922019868, 231.1912767165910907 ) ) ;
#58557 = CARTESIAN_POINT ( 'NONE',  ( -15.08216819395825148, 1451.149145817307499, 149.6691153907744081 ) ) ;
#58558 = CARTESIAN_POINT ( 'NONE',  ( 25.13854614859999970, 1436.603051257809966, 137.6783714398980010 ) ) ;
#58559 =( BOUNDED_SURFACE ( )  B_SPLINE_SURFACE ( 1, 2, ( 
 ( #2033, #39331, #72407 ),
 ( #29826, #70350, #98124 ) ),
 .UNSPECIFIED., .F., .F., .F. ) 
 B_SPLINE_SURFACE_WITH_KNOTS ( ( 2, 2 ),
 ( 3, 3 ),
 ( -10000.00000000000000, 10000.00000000000000 ),
 ( 5.178100005973779396, 6.283185307179590673 ),
 .UNSPECIFIED. ) 
 GEOMETRIC_REPRESENTATION_ITEM ( )  RATIONAL_B_SPLINE_SURFACE ( (
 ( 0.8778166915500580370, 0.7939440108100890292, 1.000000000000000000),
 ( 0.8778166915500580370, 0.7939440108100890292, 1.000000000000000000) ) ) 
 REPRESENTATION_ITEM ( '' )  SURFACE ( )  );
#58560 = CARTESIAN_POINT ( 'NONE',  ( -4.660393612750000081, 1436.848553822789881, 227.0391165213990234 ) ) ;
#58561 = CARTESIAN_POINT ( 'NONE',  ( 11.15120484727999894, 1517.051704408389924, 220.1441346914401720 ) ) ;
#58562 = CARTESIAN_POINT ( 'NONE',  ( -0.2223009154971570256, 1416.826860677879949, 191.0546700833079967 ) ) ;
#58563 = DIRECTION ( 'NONE',  ( -0.000000000000000000, -1.000000000000000000, -0.000000000000000000 ) ) ;
#58564 = VERTEX_POINT ( 'NONE', #94947 ) ;
#58565 = ORIENTED_EDGE ( 'NONE', *, *, #52321, .F. ) ;
#58566 = CARTESIAN_POINT ( 'NONE',  ( 16.09938272070030152, 1414.913060387399810, 209.3459460732159982 ) ) ;
#58567 = DIRECTION ( 'NONE',  ( 0.5877852522924673639, 0.000000000000000000, -0.8090169943749514481 ) ) ;
#58569 = CARTESIAN_POINT ( 'NONE',  ( -23.75987188199999878, 1449.114753669629863, 220.8695786834980197 ) ) ;
#58568 = CARTESIAN_POINT ( 'NONE',  ( 4.492546581380000958, 1453.878649273890005, 217.3453973181289882 ) ) ;
#58570 = CARTESIAN_POINT ( 'NONE',  ( -7.499365986679999985, 1445.290603318090007, 216.2717625584189989 ) ) ;
#58571 = B_SPLINE_CURVE_WITH_KNOTS ( 'NONE', 3,
 ( #105266, #38600, #4472, #37510, #105832, #97412, #72780 ),
 .UNSPECIFIED., .F., .F.,
 ( 4, 3, 4 ),
 ( -84.90067530945870544, -53.18660760086410022, -19.14976305580000826 ),
 .UNSPECIFIED. ) ;
#58572 = CARTESIAN_POINT ( 'NONE',  ( -11.87231497000000147, 1433.085999529410174, 150.1763001176979913 ) ) ;
#58573 = CARTESIAN_POINT ( 'NONE',  ( -12.29271509424149933, 1378.291405090629951, 210.0354033918439995 ) ) ;
#58574 = CIRCLE ( 'NONE', #103224, 11.73843354579999954 ) ;
#58575 = CYLINDRICAL_SURFACE ( 'NONE', #5375, 1.999999999999997335 ) ;
#58576 = CARTESIAN_POINT ( 'NONE',  ( 7.308867546920000180, 1424.255848919720165, 212.7423161441389823 ) ) ;
#58577 = CARTESIAN_POINT ( 'NONE',  ( -24.15153490410000359, 1438.063247892820073, 212.1983423404379892 ) ) ;
#58578 = CARTESIAN_POINT ( 'NONE',  ( -3.580429133039419565, 1454.131615231540081, 199.2738294499930021 ) ) ;
#58579 = CARTESIAN_POINT ( 'NONE',  ( 1.127298601310000148, 1450.859579147270097, 182.1360869505979849 ) ) ;
#58580 = CARTESIAN_POINT ( 'NONE',  ( 7.877099145829999038, 1362.118768394180051, 207.6218459616989946 ) ) ;
#58581 = CARTESIAN_POINT ( 'NONE',  ( -28.69781424069330455, 1510.026368465050155, 200.3394183414388863 ) ) ;
#58583 = VERTEX_POINT ( 'NONE', #86538 ) ;
#58582 = DIRECTION ( 'NONE',  ( -0.6736849260863841948, 0.000000000000000000, 0.7390186874254148774 ) ) ;
#58584 = ORIENTED_EDGE ( 'NONE', *, *, #86267, .F. ) ;
#58585 = CARTESIAN_POINT ( 'NONE',  ( -11.73951205012229870, 1426.693896884819878, 144.3445227941359974 ) ) ;
#58586 = CARTESIAN_POINT ( 'NONE',  ( 0.07276018598029700135, 1502.631145669490024, 233.2831920997990096 ) ) ;
#58587 = CARTESIAN_POINT ( 'NONE',  ( -7.954913669629999795, 1471.040533207630006, 269.6217432392980413 ) ) ;
#58588 = CARTESIAN_POINT ( 'NONE',  ( -2.261284126934287819, 1474.298250304425210, 219.1320758864328013 ) ) ;
#58589 = CARTESIAN_POINT ( 'NONE',  ( -98.31848842976613412, 1331.448250124729157, 312.4609132786720807 ) ) ;
#58590 = CARTESIAN_POINT ( 'NONE',  ( 1.439851189671822240, 1526.382868172864164, 239.5034140466408417 ) ) ;
#58591 = CARTESIAN_POINT ( 'NONE',  ( -7.973835201749999158, 1384.482862421380105, 199.5100561111489981 ) ) ;
#58592 = CARTESIAN_POINT ( 'NONE',  ( 9.944339257881379623, 1468.659659235959907, 207.9255319265940045 ) ) ;
#58593 = CARTESIAN_POINT ( 'NONE',  ( 38.61927353243170558, 1444.188088105049928, 137.1592452208769828 ) ) ;
#58594 = CARTESIAN_POINT ( 'NONE',  ( 9.813910351407720611, 1364.017814053649772, 210.6218459616991936 ) ) ;
#58595 = CARTESIAN_POINT ( 'NONE',  ( -9.880950594389059205, 1447.806469747649999, 210.0498174535929934 ) ) ;
#58596 = CARTESIAN_POINT ( 'NONE',  ( -24.00968221052989904, 1411.233756715259915, 269.0770596960790613 ) ) ;
#58597 = CARTESIAN_POINT ( 'NONE',  ( -13.68160004434409949, 1436.078871575160065, 150.3811401317549894 ) ) ;
#58598 = ORIENTED_EDGE ( 'NONE', *, *, #72638, .T. ) ;
#58599 = CARTESIAN_POINT ( 'NONE',  ( -13.77266209894789917, 1517.151704408390060, 217.0393652727940150 ) ) ;
#58600 = ORIENTED_EDGE ( 'NONE', *, *, #94710, .T. ) ;
#58601 = AXIS2_PLACEMENT_3D ( 'NONE', #29986, #22114, #15386 ) ;
#58602 = EDGE_LOOP ( 'NONE', ( #80090, #46517, #34910, #88885 ) ) ;
#58603 = CARTESIAN_POINT ( 'NONE',  ( 4.329791490734999471, 1515.051704408389924, 212.4519801359869859 ) ) ;
#58604 = DIRECTION ( 'NONE',  ( 0.001041802705676860138, 1.836969201840314816E-16, 0.9999994573234139983 ) ) ;
#58606 = CARTESIAN_POINT ( 'NONE',  ( 0.7564154366205578794, 1432.638783478930009, 200.7115661240650013 ) ) ;
#58605 = CARTESIAN_POINT ( 'NONE',  ( 3.267291605165000057, 1516.842852731759876, 212.5687880419470162 ) ) ;
#58607 = CARTESIAN_POINT ( 'NONE',  ( 5.110470188734999475, 1511.399604276809896, 217.3678244789069822 ) ) ;
#58608 = CIRCLE ( 'NONE', #105120, 1.000000000000000888 ) ;
#58609 = CARTESIAN_POINT ( 'NONE',  ( 4.925527104771288300, 1409.085063583942656, 223.4852962484615375 ) ) ;
#58610 = VERTEX_POINT ( 'NONE', #10949 ) ;
#58611 = CARTESIAN_POINT ( 'NONE',  ( -109.5441724480000119, 1378.507830972490183, 302.0293835567589440 ) ) ;
#58612 = CARTESIAN_POINT ( 'NONE',  ( 6.940473334145000450, 1516.833525648419936, 202.5658237375970145 ) ) ;
#58613 = EDGE_CURVE ( 'NONE', #19377, #39608, #97700, .T. ) ;
#58614 = EDGE_CURVE ( 'NONE', #74953, #85887, #80481, .T. ) ;
#58615 = LINE ( 'NONE', #9306, #90975 ) ;
#58616 = CARTESIAN_POINT ( 'NONE',  ( -36.69594268719530561, 1384.573250885219977, 210.0209466372170084 ) ) ;
#58617 = CARTESIAN_POINT ( 'NONE',  ( -14.48969036947769951, 1379.662410256569956, 208.2055791338830204 ) ) ;
#58618 = CARTESIAN_POINT ( 'NONE',  ( 8.578717400394859958E-16, 1374.913060387289988, 209.1218459616989946 ) ) ;
#58620 = ORIENTED_EDGE ( 'NONE', *, *, #18037, .F. ) ;
#58619 = DIRECTION ( 'NONE',  ( 1.755985294532469921E-16, -1.000000000000000000, 1.338183447452831989E-16 ) ) ;
#58621 = CARTESIAN_POINT ( 'NONE',  ( 12.67629937430701936, 1426.478869958664063, 202.7079000866955028 ) ) ;
#58622 = CARTESIAN_POINT ( 'NONE',  ( 26.91706399319999932, 1488.687396144229979, 211.9506526117480121 ) ) ;
#58623 = DIRECTION ( 'NONE',  ( 0.9455185755993178454, 0.000000000000000000, -0.3255681544571537578 ) ) ;
#58624 = CARTESIAN_POINT ( 'NONE',  ( -9.393822458599998981, 1383.815214525520105, 200.1452963205690025 ) ) ;
#58625 = CARTESIAN_POINT ( 'NONE',  ( -23.91862134480000179, 1435.332757494850057, 136.7253933288979795 ) ) ;
#58626 = CARTESIAN_POINT ( 'NONE',  ( -24.90258955090000015, 1442.651874318690034, 210.5047954567180000 ) ) ;
#58627 = CIRCLE ( 'NONE', #94400, 33.13701971169416538 ) ;
#58628 = CARTESIAN_POINT ( 'NONE',  ( 2.881222757585000238, 1516.891731298979948, 211.5992195760969707 ) ) ;
#58629 = CARTESIAN_POINT ( 'NONE',  ( -68.79001571249999358, 1379.747967232289966, 280.2970183437590208 ) ) ;
#58630 = CARTESIAN_POINT ( 'NONE',  ( -3.887263819049999736, 1491.372323727890034, 188.5673907495989852 ) ) ;
#58631 = DIRECTION ( 'NONE',  ( 0.000000000000000000, 1.000000000000000000, 0.000000000000000000 ) ) ;
#58632 = CARTESIAN_POINT ( 'NONE',  ( 20.92767404034498924, 1511.187213306747708, 182.8548762971663848 ) ) ;
#58633 = CARTESIAN_POINT ( 'NONE',  ( 6.546001350565000543, 1516.557392317769882, 207.4118413833070065 ) ) ;
#58634 = ORIENTED_EDGE ( 'NONE', *, *, #17238, .T. ) ;
#58635 = CARTESIAN_POINT ( 'NONE',  ( -2.435720948416219667, 1451.955458385490147, 184.6330791665090203 ) ) ;
#58636 = CARTESIAN_POINT ( 'NONE',  ( -8.834982911374369863, 1438.486838626130066, 208.6720045421899954 ) ) ;
#58637 = DIRECTION ( 'NONE',  ( -0.8090169943749507819, 0.000000000000000000, -0.5877852522924685852 ) ) ;
#58638 = VERTEX_POINT ( 'NONE', #106642 ) ;
#58639 = CARTESIAN_POINT ( 'NONE',  ( -3.316380893998936763, 1524.425415513988810, 241.9071459675778613 ) ) ;
#58640 = CARTESIAN_POINT ( 'NONE',  ( 12.68045462138680080, 1435.869917964839942, 150.8815144536550008 ) ) ;
#58641 = CARTESIAN_POINT ( 'NONE',  ( -4.072368715194547129, 1441.029081303531029, 184.8776654416552674 ) ) ;
#58642 = CARTESIAN_POINT ( 'NONE',  ( -6.998115108689999531, 1413.756493170500107, 208.1001205746590017 ) ) ;
#58643 = DIRECTION ( 'NONE',  ( -0.7044160264027579110, -0.08715574274766998975, 0.7044160264027579110 ) ) ;
#58644 = CARTESIAN_POINT ( 'NONE',  ( 4.403123731590000034, 1485.794562715689835, 199.2936768241389984 ) ) ;
#58645 = CARTESIAN_POINT ( 'NONE',  ( 2.149719450999330039, 1431.090543968449992, 218.3651844143140011 ) ) ;
#58646 = DIRECTION ( 'NONE',  ( -1.295211781927295682E-16, 1.000000000000000000, 0.000000000000000000 ) ) ;
#58647 = VECTOR ( 'NONE', #103986, 1000.000000000000000 ) ;
#58649 = CARTESIAN_POINT ( 'NONE',  ( 40.62990393029997449, 1439.681967586943756, 135.2802163397979314 ) ) ;
#58648 = CARTESIAN_POINT ( 'NONE',  ( -7.713117841115000317, 1516.690345681169902, 214.1262880092169780 ) ) ;
#58650 = CARTESIAN_POINT ( 'NONE',  ( -8.859802060015358194, 1385.025244372899806, 218.6830422513599785 ) ) ;
#58651 = CARTESIAN_POINT ( 'NONE',  ( -5.778372601744999670, 1516.932669162149978, 216.0673360190369863 ) ) ;
#58652 = ORIENTED_EDGE ( 'NONE', *, *, #70508, .F. ) ;
#58653 = CARTESIAN_POINT ( 'NONE',  ( -17.70115280944790115, 1479.586903222029832, 228.8488225417430328 ) ) ;
#58654 = ADVANCED_FACE ( 'NONE', ( #54627 ), #64124, .T. ) ;
#58655 = CARTESIAN_POINT ( 'NONE',  ( -17.28042313459999946, 1420.187471544980099, 203.7977315272489989 ) ) ;
#58656 = CARTESIAN_POINT ( 'NONE',  ( 1.661580760779999943, 1421.006482085029802, 183.6687324547980040 ) ) ;
#58657 = CARTESIAN_POINT ( 'NONE',  ( -2.568249187049999716, 1475.995101164990047, 219.8900349392989995 ) ) ;
#58658 = ADVANCED_FACE ( 'NONE', ( #81425 ), #29382, .F. ) ;
#58659 = CARTESIAN_POINT ( 'NONE',  ( 2.494575337237918689, 1524.201816949777367, 175.5410045932797516 ) ) ;
#58660 = CYLINDRICAL_SURFACE ( 'NONE', #98676, 1.000000000000003775 ) ;
#58661 = LINE ( 'NONE', #74918, #108594 ) ;
#58662 = CARTESIAN_POINT ( 'NONE',  ( -5.016006900679014002, 1508.231295651743494, 220.4176492183756579 ) ) ;
#58663 = CARTESIAN_POINT ( 'NONE',  ( 17.22755355015131684, 1422.440680106109312, 226.6931585904254973 ) ) ;
#58664 = CARTESIAN_POINT ( 'NONE',  ( 18.24797473426792394, 1425.311414221095447, 224.8433002223622168 ) ) ;
#58665 = CARTESIAN_POINT ( 'NONE',  ( -2.488082932330000219, 1441.600846913620217, 150.5962877614979902 ) ) ;
#58666 = CARTESIAN_POINT ( 'NONE',  ( 37.61101231473060125, 1440.913060385340032, 255.6516536714609629 ) ) ;
#58668 = CARTESIAN_POINT ( 'NONE',  ( 1.180034279919999873, 1492.152004741890096, 188.0782235167989995 ) ) ;
#58667 = CARTESIAN_POINT ( 'NONE',  ( -10.93690819593899910, 1470.800486576299818, 209.7884454878060012 ) ) ;
#58669 = CARTESIAN_POINT ( 'NONE',  ( 13.31007525419999915, 1426.030389151729878, 221.9162573719980003 ) ) ;
#58670 = ORIENTED_EDGE ( 'NONE', *, *, #85761, .T. ) ;
#58671 = EDGE_LOOP ( 'NONE', ( #95040, #60697, #107673, #97737, #100456, #93053, #34045, #96144 ) ) ;
#58672 = CARTESIAN_POINT ( 'NONE',  ( 9.225907677606098645, 1522.051704408389924, 198.5805875773771731 ) ) ;
#58673 = AXIS2_PLACEMENT_3D ( 'NONE', #20092, #29061, #38543 ) ;
#58674 = CARTESIAN_POINT ( 'NONE',  ( -5.062152673029999939, 1439.003726787289906, 206.7420654048690096 ) ) ;
#58675 = CARTESIAN_POINT ( 'NONE',  ( -28.73878198690000119, 1509.916640767629815, 211.4156715658480152 ) ) ;
#58676 = CARTESIAN_POINT ( 'NONE',  ( 7.891238773745893553, 1517.051704408389924, 189.5145166091198803 ) ) ;
#58677 = AXIS2_PLACEMENT_3D ( 'NONE', #52243, #17480, #42723 ) ;
#58678 = CARTESIAN_POINT ( 'NONE',  ( 1.519498793946838067, 1507.960421343096868, 236.9808823838983187 ) ) ;
#58679 = CARTESIAN_POINT ( 'NONE',  ( 9.357015822218050616, 1422.633417228330018, 212.8722094221120074 ) ) ;
#58680 = CONICAL_SURFACE ( 'NONE', #108788, 7.999999999999996447, 0.02617993877989872875 ) ;
#58681 = CARTESIAN_POINT ( 'NONE',  ( -1.517668881329999886, 1497.681034404829916, 231.6004894389980109 ) ) ;
#58682 = CARTESIAN_POINT ( 'NONE',  ( 19.07966196791809210, 1524.244163922423695, 179.2412984082194214 ) ) ;
#58683 = CARTESIAN_POINT ( 'NONE',  ( -63.80571065684490151, 1383.791867485110060, 286.7071051378580364 ) ) ;
#58684 = VECTOR ( 'NONE', #63431, 1000.000000000000114 ) ;
#58685 = CARTESIAN_POINT ( 'NONE',  ( 7.197032540600000416, 1452.516711882729851, 152.8386597052979994 ) ) ;
#58686 = CARTESIAN_POINT ( 'NONE',  ( -27.56721773654333774, 1509.458873407235387, 212.0988943604728263 ) ) ;
#58687 = CARTESIAN_POINT ( 'NONE',  ( 12.20128992515689959, 1492.563683748890071, 211.0969524153320265 ) ) ;
#58689 = EDGE_LOOP ( 'NONE', ( #40665, #82758, #26501, #25384 ) ) ;
#58688 = CARTESIAN_POINT ( 'NONE',  ( -3.286480964850000408, 1456.341185808290220, 218.0120306903490075 ) ) ;
#58690 = CARTESIAN_POINT ( 'NONE',  ( 31.47409394596150634, 1526.278758871497985, 218.5859237437351510 ) ) ;
#58691 = CARTESIAN_POINT ( 'NONE',  ( -70.73284055979999607, 1380.574797240599992, 273.6446839984589587 ) ) ;
#58692 = CARTESIAN_POINT ( 'NONE',  ( 19.79142244099470105, 1508.177231791150007, 229.3266476993300103 ) ) ;
#58693 = ORIENTED_EDGE ( 'NONE', *, *, #24331, .T. ) ;
#58694 = ORIENTED_EDGE ( 'NONE', *, *, #56372, .F. ) ;
#58695 =( BOUNDED_CURVE ( )  B_SPLINE_CURVE ( 3, ( #42403, #95570, #10460, #60896 ),
 .UNSPECIFIED., .F., .T. ) 
 B_SPLINE_CURVE_WITH_KNOTS ( ( 4, 4 ),
 ( 3.040788486948645009, 3.052744563067074868 ),
 .UNSPECIFIED. ) 
 CURVE ( )  GEOMETRIC_REPRESENTATION_ITEM ( )  RATIONAL_B_SPLINE_CURVE ( ( 1.000000000000000000, 0.9999880877224632814, 0.9999880877224632814, 1.000000000000000000 ) ) 
 REPRESENTATION_ITEM ( '' )  );
#58696 = CARTESIAN_POINT ( 'NONE',  ( -8.080339290932069929, 1386.284300861730117, 218.6800679842810098 ) ) ;
#58697 = CARTESIAN_POINT ( 'NONE',  ( 40.05235817349409899, 1441.916377590050161, 136.9240625044390072 ) ) ;
#58699 = CARTESIAN_POINT ( 'NONE',  ( -2.472529913803022783, 1523.678648413191695, 242.8674788698241400 ) ) ;
#58698 = CARTESIAN_POINT ( 'NONE',  ( -15.69795926856320101, 1517.051704408389924, 195.4758181589010064 ) ) ;
#58700 = CARTESIAN_POINT ( 'NONE',  ( -9.276944363820000206, 1461.680301575389876, 206.2489193930190083 ) ) ;
#58701 = CARTESIAN_POINT ( 'NONE',  ( -105.8961900970000016, 1378.203726956179935, 301.8257929996590292 ) ) ;
#58702 = CARTESIAN_POINT ( 'NONE',  ( -11.81894877114215348, 1435.231921587601164, 151.2719100762131177 ) ) ;
#58703 = CARTESIAN_POINT ( 'NONE',  ( -11.16643436200000039, 1471.372555910990059, 206.7508257863089796 ) ) ;
#58704 = AXIS2_PLACEMENT_3D ( 'NONE', #63811, #3362, #21195 ) ;
#58705 = CARTESIAN_POINT ( 'NONE',  ( -2.777756275229999794, 1456.209068913490000, 202.9659093387089968 ) ) ;
#58706 = CARTESIAN_POINT ( 'NONE',  ( 1.103557112500000104, 1409.457326867330039, 185.4212059947979867 ) ) ;
#58707 = CARTESIAN_POINT ( 'NONE',  ( 4.385995343010000269, 1424.610434865430079, 185.2880463713979964 ) ) ;
#58708 = CARTESIAN_POINT ( 'NONE',  ( 3.212856134899739757, 1433.121553999790194, 201.2044923049280101 ) ) ;
#58709 = CARTESIAN_POINT ( 'NONE',  ( -4.270405931533109545, 1441.143229069919926, 158.1181609420549989 ) ) ;
#58710 = CARTESIAN_POINT ( 'NONE',  ( 11.84030382862209940, 1430.235986815720025, 151.0624496527620124 ) ) ;
#58711 = ORIENTED_EDGE ( 'NONE', *, *, #80949, .F. ) ;
#58712 = CARTESIAN_POINT ( 'NONE',  ( -1.618115094650000030, 1427.197104430330000, 147.9439864917980287 ) ) ;
#58713 = CARTESIAN_POINT ( 'NONE',  ( 18.47806089193409562, 1457.403878534810019, 229.7720814934239968 ) ) ;
#58714 = CARTESIAN_POINT ( 'NONE',  ( 15.09717514449999953, 1449.518815468759840, 189.9127100080980028 ) ) ;
#58715 = CARTESIAN_POINT ( 'NONE',  ( -1.118730856090010083E-08, 1473.460517805439849, 262.2339000674530212 ) ) ;
#58716 = CARTESIAN_POINT ( 'NONE',  ( -12.86990655680000017, 1502.949917638090028, 208.7255105242149682 ) ) ;
#58717 = CARTESIAN_POINT ( 'NONE',  ( -0.7186627752419999515, 1416.547221146729953, 227.9060452208979939 ) ) ;
#58718 = CARTESIAN_POINT ( 'NONE',  ( -2.424815126019999934, 1477.020009817290202, 199.0133905605989924 ) ) ;
#58719 = CARTESIAN_POINT ( 'NONE',  ( -105.7870492409999912, 1391.295072527720095, 306.5714272217589951 ) ) ;
#58720 = CARTESIAN_POINT ( 'NONE',  ( -0.02015038597255117483, 1486.257254326256998, 181.8141459044200872 ) ) ;
#58721 = CARTESIAN_POINT ( 'NONE',  ( -8.512285033948522539, 1360.184861213356498, 209.6218459617033432 ) ) ;
#58722 = CARTESIAN_POINT ( 'NONE',  ( -45.72254065293900283, 1438.289221927810104, 268.7603399551510392 ) ) ;
#58723 = CARTESIAN_POINT ( 'NONE',  ( 0.7162863658319988946, 1429.709265593189912, 217.4063670190490143 ) ) ;
#58724 = CARTESIAN_POINT ( 'NONE',  ( -8.316701203199999171, 1425.055152618780085, 204.9623575238389890 ) ) ;
#58725 = CARTESIAN_POINT ( 'NONE',  ( -2.486220139904999904, 1516.939658295650133, 209.1350829839039989 ) ) ;
#58726 = CARTESIAN_POINT ( 'NONE',  ( -11.39903424189999903, 1388.037600957480208, 201.7885523045490004 ) ) ;
#58727 = CARTESIAN_POINT ( 'NONE',  ( 2.583688234164152497, 1424.460962572045901, 227.2704015761902667 ) ) ;
#58728 = CARTESIAN_POINT ( 'NONE',  ( 7.492432155504880065, 1426.008877190969770, 212.3388350879999962 ) ) ;
#58729 = CARTESIAN_POINT ( 'NONE',  ( -26.29521927434609907, 1450.751943985090065, 136.5719960223099747 ) ) ;
#58730 = ORIENTED_EDGE ( 'NONE', *, *, #59060, .T. ) ;
#58731 = CARTESIAN_POINT ( 'NONE',  ( 30.53571888249999944, 1440.913060393610067, 240.1260121784980015 ) ) ;
#58733 = CARTESIAN_POINT ( 'NONE',  ( -14.95092673998889943, 1512.169469372310004, 221.5792698019450029 ) ) ;
#58732 = CARTESIAN_POINT ( 'NONE',  ( -11.39217826018909996, 1491.610218127549842, 206.8972610507499894 ) ) ;
#58734 = CARTESIAN_POINT ( 'NONE',  ( -0.7950140742365245927, 1488.007107121973604, 219.9546037614996123 ) ) ;
#58735 = CARTESIAN_POINT ( 'NONE',  ( -24.40164415750000160, 1440.913060428330027, 211.9534758661580156 ) ) ;
#58736 = DIRECTION ( 'NONE',  ( -1.000000000000000000, 0.000000000000000000, 0.000000000000000000 ) ) ;
#58737 = CARTESIAN_POINT ( 'NONE',  ( -0.4151546846821903003, 1511.187213306747708, 175.3106345060153046 ) ) ;
#58738 = CARTESIAN_POINT ( 'NONE',  ( 4.932967056419999885, 1425.220831261190142, 209.6856336174119804 ) ) ;
#58739 = VERTEX_POINT ( 'NONE', #105566 ) ;
#58740 = DIRECTION ( 'NONE',  ( 0.000000000000000000, 0.000000000000000000, -1.000000000000000000 ) ) ;
#58741 = LINE ( 'NONE', #73897, #66884 ) ;
#58742 = CARTESIAN_POINT ( 'NONE',  ( 10.01433737459999840, 1462.389872936090114, 210.8954339908790132 ) ) ;
#58743 = ORIENTED_EDGE ( 'NONE', *, *, #89858, .T. ) ;
#58744 = ORIENTED_EDGE ( 'NONE', *, *, #30159, .F. ) ;
#58745 = CARTESIAN_POINT ( 'NONE',  ( -23.95553366050739896, 1410.857329053969806, 209.8766206678370168 ) ) ;
#58746 = CARTESIAN_POINT ( 'NONE',  ( -3.721277981550000113, 1424.084032539730060, 184.7565605802979860 ) ) ;
#58747 = CARTESIAN_POINT ( 'NONE',  ( -6.647330431358690284, 1522.051704408389924, 184.4413780136169976 ) ) ;
#58748 = CARTESIAN_POINT ( 'NONE',  ( -45.41132133646503632, 1437.168779479949762, 266.1959130671517073 ) ) ;
#58749 = CIRCLE ( 'NONE', #64132, 3.000000000000002665 ) ;
#58750 = CIRCLE ( 'NONE', #64137, 8.800000000000000711 ) ;
#58751 = CARTESIAN_POINT ( 'NONE',  ( -2.295501929209999847, 1507.640548290029983, 236.9905098398980101 ) ) ;
#58752 = CARTESIAN_POINT ( 'NONE',  ( 3.137390382537029954, 1508.729448375579977, 213.6787528850110220 ) ) ;
#58753 = ADVANCED_FACE ( 'NONE', ( #71991 ), #4202, .F. ) ;
#58754 = AXIS2_PLACEMENT_3D ( 'NONE', #80656, #29689, #85591 ) ;
#58755 = CARTESIAN_POINT ( 'NONE',  ( 41.00042505258200265, 1456.753174803509864, 266.5635232765240517 ) ) ;
#58756 = CARTESIAN_POINT ( 'NONE',  ( -10.50394959559160135, 1391.913060387279984, 204.8107535540119954 ) ) ;
#58757 = CARTESIAN_POINT ( 'NONE',  ( -3.707800473929999896, 1428.659817224090148, 200.9450977274489674 ) ) ;
#58758 = CARTESIAN_POINT ( 'NONE',  ( -4.041472511874999896, 1516.858649670339901, 205.0922732913970208 ) ) ;
#58759 = ORIENTED_EDGE ( 'NONE', *, *, #8925, .T. ) ;
#58760 = CARTESIAN_POINT ( 'NONE',  ( 18.51267396087533967, 1458.739381326464354, 227.6064210715596232 ) ) ;
#58761 = B_SPLINE_CURVE_WITH_KNOTS ( 'NONE', 3,
 ( #87946, #81166, #89570, #4481 ),
 .UNSPECIFIED., .F., .F.,
 ( 4, 4 ),
 ( 0.000000000000000000, 1.000000000000000000 ),
 .UNSPECIFIED. ) ;
#58762 = CARTESIAN_POINT ( 'NONE',  ( 1.365811584579660121, 1445.431647728280041, 199.1348593500399886 ) ) ;
#58763 = FACE_OUTER_BOUND ( 'NONE', #55106, .T. ) ;
#58764 = VERTEX_POINT ( 'NONE', #3675 ) ;
#58766 = B_SPLINE_CURVE_WITH_KNOTS ( 'NONE', 3,
 ( #35657, #10459, #88277, #103965, #27262, #53035, #87171, #44633, #70403, #104522, #53595, #105641, #63117, #98317, #37325, #4280, #3746, #97768, #56333, #89376, #63653, #28926, #97217, #90465, #38410, #98869, #5367, #13742, #82062, #71521, #38952, #46847, #80976, #20489, #54699, #47926, #107273, #73131, #21596, #106714, #88825, #3198, #106177, #37878, #79885, #30568 ),
 .UNSPECIFIED., .F., .F.,
 ( 4, 2, 2, 2, 2, 2, 1, 1, 2, 2, 2, 2, 2, 1, 1, 1, 2, 2, 2, 2, 1, 1, 1, 1, 1, 2, 2, 4 ),
 ( 0.000000000000000000, 0.06250000000046999904, 0.09375000000066381622, 0.1250000000008576473, 0.1875000000012422285, 0.2187500000014324097, 0.2343750000015297486, 0.2421875000015806800, 0.2460937500015798474, 0.2500000000015789592, 0.3750000000012674306, 0.4375000000011254886, 0.4687500000010677015, 0.4843750000010489387, 0.4921875000010395573, 0.4960937500010235146, 0.4980468750010155210, 0.5000000000010075274, 0.6250000000004316547, 0.6875000000001338929, 0.7187499999999865663, 0.7343749999999142908, 0.7421874999998850919, 0.7460937499998719913, 0.7480468749998668843, 0.7490234374998724354, 0.7499999999998779865, 1.000000000000000000 ),
 .UNSPECIFIED. ) ;
#58765 = CARTESIAN_POINT ( 'NONE',  ( -11.76331255911069995, 1481.397599341149999, 210.5790801447900265 ) ) ;
#58768 = EDGE_CURVE ( 'NONE', #36309, #65298, #87652, .T. ) ;
#58767 = CARTESIAN_POINT ( 'NONE',  ( 27.03107214705890016, 1451.493449271870077, 136.0706941817539928 ) ) ;
#58769 = DIRECTION ( 'NONE',  ( 9.056288633775531119E-47, -1.000000000000000000, 1.836970198721029688E-16 ) ) ;
#58770 = CARTESIAN_POINT ( 'NONE',  ( 4.226195811716859652, 1452.765478377580166, 152.2144321770960005 ) ) ;
#58771 = CARTESIAN_POINT ( 'NONE',  ( 8.299847678909999971, 1421.312374491559922, 196.1635037195989923 ) ) ;
#58772 = CARTESIAN_POINT ( 'NONE',  ( 0.5913408061856150200, 1431.617811701200026, 218.5945621063530098 ) ) ;
#58773 = LINE ( 'NONE', #32469, #84133 ) ;
#58774 = CARTESIAN_POINT ( 'NONE',  ( 6.924940705133599828, 1409.154884645419997, 188.7083484210960194 ) ) ;
#58776 = DIRECTION ( 'NONE',  ( 0.000000000000000000, 1.000000000000000000, 0.000000000000000000 ) ) ;
#58775 = CARTESIAN_POINT ( 'NONE',  ( 1.837350884659999961, 1417.558700500429950, 234.5777813587980063 ) ) ;
#58777 = B_SPLINE_CURVE_WITH_KNOTS ( 'NONE', 3,
 ( #38957, #73136, #107831, #28931 ),
 .UNSPECIFIED., .F., .F.,
 ( 4, 4 ),
 ( 0.000000000000000000, 0.0002220129587134776663 ),
 .UNSPECIFIED. ) ;
#58778 = DIRECTION ( 'NONE',  ( 1.836970198721029688E-16, 1.000000000000000000, 0.000000000000000000 ) ) ;
#58779 = CARTESIAN_POINT ( 'NONE',  ( -11.76384282640000123, 1377.860255930400172, 212.8274665997790009 ) ) ;
#58780 = CARTESIAN_POINT ( 'NONE',  ( -19.66678637224480397, 1522.051704408389924, 215.8936635741279986 ) ) ;
#58781 = ORIENTED_EDGE ( 'NONE', *, *, #33990, .F. ) ;
#58782 = CARTESIAN_POINT ( 'NONE',  ( -32.38114538885258753, 1523.604703353109699, 202.1233279672532888 ) ) ;
#58783 = CARTESIAN_POINT ( 'NONE',  ( -19.63722818156799832, 1517.151704408390060, 200.0074286628000095 ) ) ;
#58784 = DIRECTION ( 'NONE',  ( -1.000000000000000000, 0.000000000000000000, 0.000000000000000000 ) ) ;
#58785 = CARTESIAN_POINT ( 'NONE',  ( -12.31074584409999950, 1391.522609710569895, 206.9351367010589797 ) ) ;
#58786 = CARTESIAN_POINT ( 'NONE',  ( 8.663868365875391220, 1423.279983291419967, 211.7948421327720041 ) ) ;
#58787 = CARTESIAN_POINT ( 'NONE',  ( 12.41549622805439945, 1426.345760381200080, 202.7472225575059781 ) ) ;
#58788 = CARTESIAN_POINT ( 'NONE',  ( -17.17241001986523941, 1518.913060387330006, 179.6185504016045797 ) ) ;
#58789 = CARTESIAN_POINT ( 'NONE',  ( -34.84383440970000123, 1453.969943383929831, 265.6112250856980381 ) ) ;
#58790 = CARTESIAN_POINT ( 'NONE',  ( -22.39540327093973104, 1509.695125100958421, 191.0396457048211403 ) ) ;
#58791 = CARTESIAN_POINT ( 'NONE',  ( 11.08805915299999967, 1433.401164229489950, 151.6926779325980021 ) ) ;
#58792 = CARTESIAN_POINT ( 'NONE',  ( 8.881784197000000993E-16, 1470.874276671130019, 268.3665355202980436 ) ) ;
#58793 = B_SPLINE_CURVE_WITH_KNOTS ( 'NONE', 5,
 ( #13305, #72174, #29575, #65414, #99520, #90028, #107940, #30682, #23375, #65968, #63761, #5482, #64869, #46962, #57566, #31781, #22805, #91139, #22251, #48609, #98977, #39643, #55356, #39068, #3864, #55910, #74368 ),
 .UNSPECIFIED., .F., .F.,
 ( 6, 3, 3, 3, 3, 3, 3, 3, 6 ),
 ( 0.000000000000000000, 0.03529557405075641613, 0.06179070172895334556, 0.08828582939876877811, 0.1412760847467809111, 0.2826085572933068613, 0.5644389168522545575, 0.8435653545061785330, 1.000000000000000000 ),
 .UNSPECIFIED. ) ;
#58794 = CARTESIAN_POINT ( 'NONE',  ( 11.41805403401209951, 1414.913057862230062, 197.3911482182210193 ) ) ;
#58795 = CARTESIAN_POINT ( 'NONE',  ( -29.00779973304138437, 1526.382868172864164, 200.9494832830839073 ) ) ;
#58796 = CARTESIAN_POINT ( 'NONE',  ( 12.14135103133349958, 1420.978590117220165, 201.7400648282489897 ) ) ;
#58797 = CARTESIAN_POINT ( 'NONE',  ( 6.072417058032599790, 1467.015289949989892, 217.0523006129610053 ) ) ;
#58798 = CARTESIAN_POINT ( 'NONE',  ( -18.92783145980000370, 1486.091458575729803, 189.3401239504979969 ) ) ;
#58799 = CARTESIAN_POINT ( 'NONE',  ( 30.31052258194597115, 1523.604703353109699, 222.4930856806589929 ) ) ;
#58800 = CARTESIAN_POINT ( 'NONE',  ( 17.33645362950000290, 1414.996442546130083, 210.3925741896480304 ) ) ;
#58801 = B_SPLINE_CURVE_WITH_KNOTS ( 'NONE', 3,
 ( #10771, #45498, #78524, #44942, #88585, #27559, #61204, #11326, #54449, #71258, #26442, #94761, #70708, #86357, #36514, #105380, #28668, #103714, #19132, #69596, #1835, #53907, #104270, #79089, #52775, #86913, #11867, #61742, #44380, #62873, #9640, #77416, #95865, #53335, #18036, #87483, #95319, #62299, #2397, #96985, #96426, #104821, #20248 ),
 .UNSPECIFIED., .F., .F.,
 ( 4, 3, 3, 3, 3, 3, 3, 3, 3, 3, 3, 3, 3, 3, 4 ),
 ( -1.999999029881750046, -1.991354409435089901, -1.843127450874009865, -1.686255871866269906, -1.534783949317029883, -1.379712255795449982, -1.225304414952149923, -1.070191527292039924, -0.9147394646296638232, -0.7593381984712410659, -0.6048407093868408690, -0.4514088248038210516, -0.2993314472943329196, -0.1488170141350799724, -5.152078763615008938E-11 ),
 .UNSPECIFIED. ) ;
#58802 = CARTESIAN_POINT ( 'NONE',  ( 19.39159332000000191, 1430.347784931329898, 222.5897557541980234 ) ) ;
#58803 = CARTESIAN_POINT ( 'NONE',  ( -15.36549428884569934, 1420.414141511310163, 227.0219848988409979 ) ) ;
#58804 = CARTESIAN_POINT ( 'NONE',  ( -1.569161292555000031, 1517.051704408389924, 216.8444262845069943 ) ) ;
#58805 = CARTESIAN_POINT ( 'NONE',  ( -1.842963808589999974, 1515.492058141890084, 204.9833025469089876 ) ) ;
#58806 = CARTESIAN_POINT ( 'NONE',  ( -5.215016241880452874, 1391.913060387290443, 203.8075142969990168 ) ) ;
#58807 = CARTESIAN_POINT ( 'NONE',  ( -19.34949478396210054, 1446.106506027710111, 200.0047807539029918 ) ) ;
#58808 = CARTESIAN_POINT ( 'NONE',  ( -16.56680993899979981, 1420.259233108609806, 206.2549788483950124 ) ) ;
#58809 = CARTESIAN_POINT ( 'NONE',  ( 0.1811898575556089852, 1473.797889089420096, 182.3607679443829852 ) ) ;
#58811 = ORIENTED_EDGE ( 'NONE', *, *, #105656, .F. ) ;
#58810 = CARTESIAN_POINT ( 'NONE',  ( -5.816635555072360297, 1408.583828391070028, 221.8830431125730058 ) ) ;
#58812 = CARTESIAN_POINT ( 'NONE',  ( -17.22592482065197927, 1444.324653571828776, 162.9227486220069920 ) ) ;
#58813 = B_SPLINE_CURVE_WITH_KNOTS ( 'NONE', 5,
 ( #27981, #86227, #43686, #62166, #54318, #61071, #1147, #103014, #96857, #96292, #20126, #52646, #17899, #19571, #103580, #26882, #95188, #18447, #86783, #87343, #10072, #44247, #27422, #61605, #19002, #91191, #55406, #81670, #38041, #107987, #4976, #97929, #89538, #4448, #71693, #46464, #88984, #99026, #105812, #3911, #72220, #82240, #106342, #81131, #106881, #12272, #90076, #72752 ),
 .UNSPECIFIED., .F., .F.,
 ( 6, 3, 3, 3, 3, 3, 3, 3, 3, 3, 3, 3, 3, 3, 3, 6 ),
 ( 0.000000000000000000, 0.1188772993508104975, 0.2620754547158732350, 0.4767847777604456994, 0.6196881868957598849, 0.7909627338043010436, 0.8908775806277737797, 0.9289413061621332179, 0.9543180330005532896, 0.9712371219245071741, 0.9825186400522594177, 0.9900448187280238566, 0.9950985928942978065, 0.9968304128275284892, 0.9985622327607588389, 1.000000000000000000 ),
 .UNSPECIFIED. ) ;
#58814 = DIRECTION ( 'NONE',  ( 0.9510565162951566398, 0.000000000000000000, -0.3090169943749382919 ) ) ;
#58815 = CARTESIAN_POINT ( 'NONE',  ( -16.36456115631863284, 1522.051704408389924, 220.0929384032941698 ) ) ;
#58816 = CARTESIAN_POINT ( 'NONE',  ( -40.76227011288860069, 1440.007145189510084, 134.0999999980880091 ) ) ;
#58817 = CARTESIAN_POINT ( 'NONE',  ( -109.3494421689999996, 1384.898366538659957, 297.1385770996590168 ) ) ;
#58818 = ORIENTED_EDGE ( 'NONE', *, *, #33520, .F. ) ;
#58819 = B_SPLINE_SURFACE_WITH_KNOTS ( 'NONE', 5, 1, ( 
 ( #472, #24521 ),
 ( #34043, #58710 ),
 ( #92843, #68233 ),
 ( #25626, #93391 ),
 ( #16120, #93937 ),
 ( #50324, #16656 ) ),
 .UNSPECIFIED., .F., .F., .F.,
 ( 6, 6 ),
 ( 2, 2 ),
 ( 0.000000000000000000, 11.48860277639830052 ),
 ( -1.500000000000000000, 1.500000000000000000 ),
 .UNSPECIFIED. ) ;
#58820 = CARTESIAN_POINT ( 'NONE',  ( -16.57695357294941019, 1524.524650307242837, 180.6873389552785625 ) ) ;
#58821 = DIRECTION ( 'NONE',  ( 0.9900965937346507539, -0.1403878024439509931, 3.790652827686679061E-16 ) ) ;
#58822 = CARTESIAN_POINT ( 'NONE',  ( -105.2354452277541554, 1381.066582002241830, 308.6640088333896870 ) ) ;
#58823 = DIRECTION ( 'NONE',  ( 0.9786619618251632957, -0.000000000000000000, 0.2054769195713296581 ) ) ;
#58824 = CARTESIAN_POINT ( 'NONE',  ( 18.18716276245509889, 1472.405785144279889, 200.2358052267980213 ) ) ;
#58825 = CARTESIAN_POINT ( 'NONE',  ( 0.4863421998530879642, 1418.702335047680208, 184.7127968358159933 ) ) ;
#58826 = CIRCLE ( 'NONE', #44391, 1.999999999999999556 ) ;
#58827 = CARTESIAN_POINT ( 'NONE',  ( 22.11623627239999834, 1489.468502498730004, 210.6419393784279919 ) ) ;
#58828 = CARTESIAN_POINT ( 'NONE',  ( -14.08142779579999981, 1379.709124900479765, 211.5303545317289888 ) ) ;
#58829 = CARTESIAN_POINT ( 'NONE',  ( 3.917311521000000685, 1436.965663665770080, 184.8061579696979777 ) ) ;
#58830 = B_SPLINE_SURFACE_WITH_KNOTS ( 'NONE', 5, 4, ( 
 ( #10511, #53083, #36262, #62619, #54201 ),
 ( #95069, #70451, #86659, #36819, #11072 ),
 ( #104571, #63166, #27866, #71009, #3247 ),
 ( #9954, #44126, #62046, #53646, #45242 ),
 ( #11621, #78261, #105130, #96736, #37373 ),
 ( #20007, #45798, #1574, #79931, #71574 ),
 ( #9406, #35707, #105695, #43568, #69897 ),
 ( #77718, #39003, #12162, #90517, #14350 ),
 ( #22187, #48541, #106765, #65349, #21642 ) ),
 .UNSPECIFIED., .F., .F., .F.,
 ( 6, 3, 6 ),
 ( 5, 5 ),
 ( 0.000000000000000000, 5.782490304330000441, 11.25975508159999983 ),
 ( 25.78146411700000229, 39.23969207129999859 ),
 .UNSPECIFIED. ) ;
#58831 = CARTESIAN_POINT ( 'NONE',  ( -79.38120359113469249, 1385.155067698849962, 282.2779454254330176 ) ) ;
#58832 = CARTESIAN_POINT ( 'NONE',  ( -18.19590854887641740, 1522.644714754858796, 238.2026672068733433 ) ) ;
#58833 = CARTESIAN_POINT ( 'NONE',  ( 12.02790215590800038, 1427.361711468500062, 208.2118097891859918 ) ) ;
#58834 = ORIENTED_EDGE ( 'NONE', *, *, #76663, .T. ) ;
#58835 = AXIS2_PLACEMENT_3D ( 'NONE', #66510, #49144, #93319 ) ;
#58836 = CARTESIAN_POINT ( 'NONE',  ( 11.93818824289999903, 1433.480083226980014, 149.8972169559980046 ) ) ;
#58837 = CARTESIAN_POINT ( 'NONE',  ( 12.53517974735357576, 1442.773887286369700, 169.5044317858253464 ) ) ;
#58839 = VERTEX_POINT ( 'NONE', #45121 ) ;
#58838 = CARTESIAN_POINT ( 'NONE',  ( 2.280774907361240000, 1437.403108797190043, 227.5229878108619914 ) ) ;
#58840 = CARTESIAN_POINT ( 'NONE',  ( 3.962210237229999432, 1474.305345705389982, 219.8526279916989949 ) ) ;
#58841 = AXIS2_PLACEMENT_3D ( 'NONE', #96668, #43508, #77653 ) ;
#58842 = ADVANCED_FACE ( 'NONE', ( #21515 ), #32236, .F. ) ;
#58843 = CARTESIAN_POINT ( 'NONE',  ( -19.20111751579667114, 1410.945218301533487, 222.5811953199733466 ) ) ;
#58844 = CARTESIAN_POINT ( 'NONE',  ( -6.393428210657781108, 1363.466147642558553, 208.3718459617061285 ) ) ;
#58845 = CARTESIAN_POINT ( 'NONE',  ( -10.99857202889999996, 1492.065341454889904, 207.0970296734990086 ) ) ;
#58846 = EDGE_CURVE ( 'NONE', #104880, #16730, #105888, .T. ) ;
#58847 = CARTESIAN_POINT ( 'NONE',  ( 39.91348005095139939, 1450.504013711060225, 269.6087561242041488 ) ) ;
#58848 = CARTESIAN_POINT ( 'NONE',  ( 15.00522596485355287, 1511.839858410422266, 197.1933472413483912 ) ) ;
#58849 = EDGE_CURVE ( 'NONE', #43125, #49156, #14723, .T. ) ;
#58850 = CARTESIAN_POINT ( 'NONE',  ( 15.03154484612626263, 1430.682371875214812, 220.0467435185384204 ) ) ;
#58851 = CARTESIAN_POINT ( 'NONE',  ( 2.572398481029999573, 1417.848201471729908, 233.8656960024980265 ) ) ;
#58852 = CARTESIAN_POINT ( 'NONE',  ( 9.146237109299999446, 1449.998848175489911, 208.1168068839089926 ) ) ;
#58853 = CARTESIAN_POINT ( 'NONE',  ( 40.27308693906149273, 1443.611999474700042, 137.1163322506119755 ) ) ;
#58854 = CARTESIAN_POINT ( 'NONE',  ( 1.910126501409999789E-10, 1431.113060387329824, 227.8291532366980050 ) ) ;
#58855 = CARTESIAN_POINT ( 'NONE',  ( -29.37542415142184993, 1526.382868172864164, 217.2587022579325833 ) ) ;
#58856 = CARTESIAN_POINT ( 'NONE',  ( -1.715704529104999931, 1516.757508073510053, 205.8704515699670026 ) ) ;
#58857 = AXIS2_PLACEMENT_3D ( 'NONE', #56965, #58068, #4884 ) ;
#58858 = CARTESIAN_POINT ( 'NONE',  ( 2.704954423850000289, 1447.065239520190062, 170.5387359128979767 ) ) ;
#58859 = ORIENTED_EDGE ( 'NONE', *, *, #33002, .F. ) ;
#58860 = CARTESIAN_POINT ( 'NONE',  ( -16.87207556298167077, 1516.551188142742376, 195.8275909262277708 ) ) ;
#58861 = CARTESIAN_POINT ( 'NONE',  ( 14.35469249349999998, 1416.832348283729971, 196.6649917540980255 ) ) ;
#58863 = ORIENTED_EDGE ( 'NONE', *, *, #52153, .T. ) ;
#58862 = CARTESIAN_POINT ( 'NONE',  ( -68.43062188917149058, 1379.747186918749776, 280.0365307058419830 ) ) ;
#58864 = CARTESIAN_POINT ( 'NONE',  ( -15.06280282045160135, 1422.388303761650150, 229.4662100962750060 ) ) ;
#58865 = ORIENTED_EDGE ( 'NONE', *, *, #3599, .T. ) ;
#58866 = DIRECTION ( 'NONE',  ( -0.8672669759446699489, 0.000000000000000000, -0.4978433412588613716 ) ) ;
#58867 = CARTESIAN_POINT ( 'NONE',  ( -20.29535751400000265, 1430.346966375530201, 196.9847315563980032 ) ) ;
#58869 = CARTESIAN_POINT ( 'NONE',  ( 15.87404176176099924, 1409.467377696719950, 192.9779251718159969 ) ) ;
#58868 = CARTESIAN_POINT ( 'NONE',  ( -11.18248557239999919, 1426.884307463830055, 103.8973682686980169 ) ) ;
#58870 = CARTESIAN_POINT ( 'NONE',  ( -1.701027861004999808, 1516.937508036699910, 211.6166039682370013 ) ) ;
#58871 = CARTESIAN_POINT ( 'NONE',  ( 36.22678859348660296, 1436.464133680080067, 136.2561648524459770 ) ) ;
#58872 = FACE_OUTER_BOUND ( 'NONE', #89901, .T. ) ;
#58873 = CARTESIAN_POINT ( 'NONE',  ( -35.25148663959999595, 1420.828143575929971, 264.2529700431979904 ) ) ;
#58874 = CARTESIAN_POINT ( 'NONE',  ( -0.7704842542331529209, 1509.002383188599879, 179.3520445167110040 ) ) ;
#58875 = CARTESIAN_POINT ( 'NONE',  ( 17.06106173523173553, 1460.356808348517234, 228.7022572861417586 ) ) ;
#58876 = CONTEXT_DEPENDENT_SHAPE_REPRESENTATION ( #51309, #83156 ) ;
#58877 = CARTESIAN_POINT ( 'NONE',  ( -109.1655177890000061, 1384.872414444939977, 297.1329087538589420 ) ) ;
#58878 = FACE_BOUND ( 'NONE', #32114, .T. ) ;
#58879 = ORIENTED_EDGE ( 'NONE', *, *, #25456, .T. ) ;
#58880 = CARTESIAN_POINT ( 'NONE',  ( -17.66967187341156986, 1519.551704408389924, 195.1406325240351123 ) ) ;
#58881 = CARTESIAN_POINT ( 'NONE',  ( -18.76125227649999871, 1457.009933317229979, 229.1040481900979842 ) ) ;
#58882 = ORIENTED_EDGE ( 'NONE', *, *, #28303, .F. ) ;
#58883 = ORIENTED_EDGE ( 'NONE', *, *, #50103, .T. ) ;
#58884 = CARTESIAN_POINT ( 'NONE',  ( -1.482599699759999945, 1431.767369128790051, 203.5535557080689841 ) ) ;
#58885 = CARTESIAN_POINT ( 'NONE',  ( 13.76740486215110160, 1464.191801214029738, 225.0510466410910055 ) ) ;
#58886 = CARTESIAN_POINT ( 'NONE',  ( -4.244621079450020318, 1507.604642859460000, 221.2803215189360060 ) ) ;
#58887 = CARTESIAN_POINT ( 'NONE',  ( -15.31725463369030038, 1507.984504716529955, 209.4225156325090040 ) ) ;
#58888 = CARTESIAN_POINT ( 'NONE',  ( 4.217997304759999899, 1515.470303964289997, 209.8638434859140034 ) ) ;
#58889 = CIRCLE ( 'NONE', #108921, 1.999999999999998668 ) ;
#58890 = CARTESIAN_POINT ( 'NONE',  ( -5.331678975189100278, 1454.863890310829902, 201.3635607548650057 ) ) ;
#58891 = CARTESIAN_POINT ( 'NONE',  ( 36.37832876739999932, 1451.642701153929920, 134.0999999898979809 ) ) ;
#58892 = CARTESIAN_POINT ( 'NONE',  ( 1.781283018236084148, 1516.548117337700205, 216.4089363120791347 ) ) ;
#58893 = B_SPLINE_SURFACE_WITH_KNOTS ( 'NONE', 5, 5, ( 
 ( #82420, #90805, #6248, #66736, #14646, #57784 ),
 ( #31446, #67285, #48832, #65629, #49918, #99189 ),
 ( #82955, #83494, #14086, #23034, #23595, #74575 ),
 ( #33096, #15179, #39859, #56113, #40951, #100839 ),
 ( #91902, #107610, #66190, #7351, #108711, #74022 ),
 ( #90246, #41514, #58319, #6790, #49366, #75128 ),
 ( #75673, #109817, #108156, #109277, #92441, #13528 ),
 ( #47715, #81845, #5149, #39304, #30894, #43716 ),
 ( #67829, #35307, #1177, #68387, #43170, #8998 ),
 ( #26341, #77867, #18480, #69494, #86813, #35872 ),
 ( #52677, #623, #76213, #51569, #85702, #52128 ),
 ( #86256, #103043, #25784, #51016, #1733, #70056 ),
 ( #17930, #16816, #77324, #110358, #84600, #10105 ),
 ( #24669, #103616, #26914, #61102, #60537, #94659 ),
 ( #68942, #76763, #101940, #78422, #9546, #59982 ),
 ( #44278, #93543, #42062, #95219, #85151, #33635 ),
 ( #58868, #7891, #34203, #92998, #25228, #16274 ),
 ( #50476, #59431, #8437, #42610, #72, #34754 ),
 ( #102494, #94100, #17371, #36406, #97955, #53802 ),
 ( #20689, #95767, #71150, #97419, #79531, #37516 ),
 ( #54346, #89011, #44837, #55434, #21225, #19034 ),
 ( #62195, #10671, #54886, #96322, #78992, #104167 ),
 ( #87377, #2833, #71719, #2295, #47036, #89565 ),
 ( #12855, #19600, #81161, #3939, #3388, #105837 ),
 ( #80066, #11761, #70598, #4476, #87939, #11230 ),
 ( #53235, #105273, #12300, #36954, #29115, #28565 ) ),
 .UNSPECIFIED., .F., .F., .F.,
 ( 6, 5, 3, 3, 3, 3, 3, 6 ),
 ( 6, 6 ),
 ( 14.16850226231500010, 14.91778146530000093, 25.40568016630000159, 46.35833806440000160, 67.31099596259998918, 78.57834886320000578, 84.21202531349999276, 89.84570176380000817 ),
 ( 0.000000000000000000, 2.061429890987789726 ),
 .UNSPECIFIED. ) ;
#58894 = CARTESIAN_POINT ( 'NONE',  ( 27.69925880659999962, 1441.434395406610065, 137.3015763229979882 ) ) ;
#58895 = DIRECTION ( 'NONE',  ( 0.9824080081115887930, -2.243614313870717968E-31, 0.1867471702549210744 ) ) ;
#58896 = CARTESIAN_POINT ( 'NONE',  ( -93.46913709372920209, 1384.851876627109959, 294.3416048512119687 ) ) ;
#58897 = ORIENTED_EDGE ( 'NONE', *, *, #47446, .F. ) ;
#58898 =( BOUNDED_CURVE ( )  B_SPLINE_CURVE ( 3, ( #23780, #22659, #33287, #83157 ),
 .UNSPECIFIED., .F., .T. ) 
 B_SPLINE_CURVE_WITH_KNOTS ( ( 4, 4 ),
 ( 2.890157840421000213, 3.288561460421139948 ),
 .UNSPECIFIED. ) 
 CURVE ( )  GEOMETRIC_REPRESENTATION_ITEM ( )  RATIONAL_B_SPLINE_CURVE ( ( 1.000000000000000000, 0.9868165609958530204, 0.9868165609958530204, 1.000000000000000000 ) ) 
 REPRESENTATION_ITEM ( '' )  );
#58899 = CARTESIAN_POINT ( 'NONE',  ( 2.871580388595000422, 1517.129577905929864, 202.1716309988170224 ) ) ;
#58900 = CARTESIAN_POINT ( 'NONE',  ( 6.949703334655000120, 1517.130100026000036, 209.8609679372960102 ) ) ;
#58901 = ORIENTED_EDGE ( 'NONE', *, *, #2147, .F. ) ;
#58902 = CARTESIAN_POINT ( 'NONE',  ( 18.95766226850000180, 1454.628370232990164, 205.4382105502989759 ) ) ;
#58903 = TOROIDAL_SURFACE ( 'NONE', #16021, 6.646318662569999702, 0.5000000000000000000 ) ;
#58904 = CARTESIAN_POINT ( 'NONE',  ( 20.28635835149999878, 1497.705735184930063, 227.7388624672979915 ) ) ;
#58905 = ORIENTED_EDGE ( 'NONE', *, *, #44015, .T. ) ;
#58906 = CARTESIAN_POINT ( 'NONE',  ( -13.56558276610000036, 1415.128105759529944, 220.7749916984980132 ) ) ;
#58907 = EDGE_CURVE ( 'NONE', #102101, #51188, #35062, .T. ) ;
#58908 = CARTESIAN_POINT ( 'NONE',  ( -11.40717366248250109, 1432.341607270339864, 151.3374056301740040 ) ) ;
#58909 = CARTESIAN_POINT ( 'NONE',  ( -2.330134127310790060, 1515.064792882719985, 213.4512947379739956 ) ) ;
#58910 = CARTESIAN_POINT ( 'NONE',  ( -2.031407857746849732, 1468.162645372460020, 219.6586981276110180 ) ) ;
#58911 = CARTESIAN_POINT ( 'NONE',  ( 21.63738260543960124, 1409.760734550770167, 206.3395242849809961 ) ) ;
#58912 = CARTESIAN_POINT ( 'NONE',  ( 10.20064331328789997, 1469.553217653640104, 207.2979568099669905 ) ) ;
#58913 = CARTESIAN_POINT ( 'NONE',  ( -0.1318727118059999925, 1507.624523832230125, 180.8831098946980092 ) ) ;
#58914 = CARTESIAN_POINT ( 'NONE',  ( -11.28649141220000018, 1489.673453124989919, 212.4368142099590102 ) ) ;
#58915 = CARTESIAN_POINT ( 'NONE',  ( -56.85802524500000033, 1379.713981567250130, 254.2456484369590157 ) ) ;
#58916 = CARTESIAN_POINT ( 'NONE',  ( 23.49278042014210044, 1432.394255265819993, 206.2073926321550061 ) ) ;
#58918 = CARTESIAN_POINT ( 'NONE',  ( -10.70847609427080016, 1506.854789404229905, 189.5201119528840081 ) ) ;
#58917 = CARTESIAN_POINT ( 'NONE',  ( -20.74020547129999770, 1505.489868768189808, 209.1669152150809907 ) ) ;
#58919 = CARTESIAN_POINT ( 'NONE',  ( 0.000000000000000000, 1378.013060387289897, 209.1218459616989946 ) ) ;
#58920 = CARTESIAN_POINT ( 'NONE',  ( -3.454172653555000139, 1517.122088787240045, 216.8462693643270143 ) ) ;
#58921 = VERTEX_POINT ( 'NONE', #14790 ) ;
#58922 = VECTOR ( 'NONE', #60615, 1000.000000000000227 ) ;
#58923 = CARTESIAN_POINT ( 'NONE',  ( -8.301987938657498844, 1512.913060387330006, 186.6498241004079262 ) ) ;
#58924 = CARTESIAN_POINT ( 'NONE',  ( -21.75647715750836753, 1524.201816949742124, 234.8230427201935697 ) ) ;
#58925 = CARTESIAN_POINT ( 'NONE',  ( -2.480187054844999572, 1517.025470194390209, 213.7472054950769973 ) ) ;
#58926 = CARTESIAN_POINT ( 'NONE',  ( 5.517786218439999502, 1505.096896727989815, 220.1774552607989790 ) ) ;
#58927 = CARTESIAN_POINT ( 'NONE',  ( -11.41895509221428284, 1425.728710957366502, 138.9295753978231573 ) ) ;
#58929 = ORIENTED_EDGE ( 'NONE', *, *, #89132, .F. ) ;
#58928 = CARTESIAN_POINT ( 'NONE',  ( -11.47725681950860022, 1501.043658996279873, 211.1773061387589792 ) ) ;
#58930 = CARTESIAN_POINT ( 'NONE',  ( -9.095184790679999409, 1384.908537446980063, 199.9427583283290062 ) ) ;
#58931 = CARTESIAN_POINT ( 'NONE',  ( 0.7858030238929989419, 1508.037196299090056, 220.8608535643990081 ) ) ;
#58932 = CARTESIAN_POINT ( 'NONE',  ( -10.87453050220000073, 1426.191206384630050, 148.6425034869979811 ) ) ;
#58933 = CARTESIAN_POINT ( 'NONE',  ( 19.11490450420339826, 1456.932054066890032, 225.0864823901050045 ) ) ;
#58934 = CARTESIAN_POINT ( 'NONE',  ( -10.98475441868929892, 1462.126042464299871, 210.0219236981780000 ) ) ;
#58935 = CARTESIAN_POINT ( 'NONE',  ( -18.49530585604750144, 1445.106360394780040, 205.2817505082109903 ) ) ;
#58936 = CARTESIAN_POINT ( 'NONE',  ( -6.708171328076900863, 1426.565319743190003, 202.6435997773789950 ) ) ;
#58937 = CARTESIAN_POINT ( 'NONE',  ( 11.10897332659999925, 1410.396565740230244, 229.3766474285979768 ) ) ;
#58938 = ADVANCED_FACE ( 'NONE', ( #49523 ), #91213, .F. ) ;
#58940 = CARTESIAN_POINT ( 'NONE',  ( -19.25698220359180368, 1504.759393713030022, 209.4658869119480187 ) ) ;
#58939 = CARTESIAN_POINT ( 'NONE',  ( -21.05893290610000079, 1495.370945771229799, 226.6524662259979834 ) ) ;
#58941 = DIRECTION ( 'NONE',  ( 0.0009897943187279698019, -0.9990041106109668334, -0.04460725601959834169 ) ) ;
#58942 = AXIS2_PLACEMENT_3D ( 'NONE', #92500, #109331, #35222 ) ;
#58943 = EDGE_LOOP ( 'NONE', ( #79389, #28368, #82848, #66064, #87474 ) ) ;
#58944 = CARTESIAN_POINT ( 'NONE',  ( 2.478306819944999795, 1516.938330505699923, 205.6592251139969960 ) ) ;
#58945 = CARTESIAN_POINT ( 'NONE',  ( 27.10552972939999705, 1412.304471280730013, 267.5397075098980508 ) ) ;
#58946 = CARTESIAN_POINT ( 'NONE',  ( -0.2565576784669999499, 1409.415731107930014, 185.2539421329980200 ) ) ;
#58947 = CARTESIAN_POINT ( 'NONE',  ( 19.60616233339999681, 1449.731300271829923, 192.9561808612979803 ) ) ;
#58948 = CARTESIAN_POINT ( 'NONE',  ( -0.04703443907195579976, 1508.971642086719839, 238.8756872305209811 ) ) ;
#58949 = CARTESIAN_POINT ( 'NONE',  ( 2.200196402067729817, 1454.568881740520055, 218.2638029879659882 ) ) ;
#58950 = CARTESIAN_POINT ( 'NONE',  ( -1.524714358750000054, 1451.605638646529997, 183.9700909300979959 ) ) ;
#58951 = CARTESIAN_POINT ( 'NONE',  ( -16.65376728669999906, 1508.454796204690183, 213.7212179624189901 ) ) ;
#58952 = CARTESIAN_POINT ( 'NONE',  ( -14.34171585720000053, 1416.291316961129951, 203.4717140614689868 ) ) ;
#58953 = CIRCLE ( 'NONE', #10676, 1.999999954377544853 ) ;
#58954 = CARTESIAN_POINT ( 'NONE',  ( -13.41257183429999955, 1444.508158409760199, 187.3828037918979703 ) ) ;
#58955 = CARTESIAN_POINT ( 'NONE',  ( -18.91838588339999916, 1497.713060387329961, 221.0203545984980167 ) ) ;
#58956 = DIRECTION ( 'NONE',  ( 5.980589973904019347E-17, -1.000000000000000000, 1.736889445713099699E-16 ) ) ;
#58957 = CARTESIAN_POINT ( 'NONE',  ( 36.48439548460181214, 1420.562375130034297, 269.8440692943977410 ) ) ;
#58958 = CARTESIAN_POINT ( 'NONE',  ( 1.459360875619579945, 1496.550641856539869, 181.5740326910060105 ) ) ;
#58959 = CARTESIAN_POINT ( 'NONE',  ( -19.02913997090000109, 1436.609546585079897, 214.3676144204279694 ) ) ;
#58960 = CARTESIAN_POINT ( 'NONE',  ( -11.25663888305209959, 1508.421392267890042, 207.6010232658840096 ) ) ;
#58961 = CARTESIAN_POINT ( 'NONE',  ( -12.14288099779810715, 1377.667352148589998, 211.1463812155207052 ) ) ;
#58962 = CARTESIAN_POINT ( 'NONE',  ( -18.38476637639999822, 1473.248652006430120, 267.3950365521980075 ) ) ;
#58963 = CARTESIAN_POINT ( 'NONE',  ( -18.82774374539999940, 1444.049758829389930, 210.0174085047549966 ) ) ;
#58964 = CARTESIAN_POINT ( 'NONE',  ( -21.24473942629999712, 1509.721192233729880, 188.1671532087979699 ) ) ;
#58965 = CARTESIAN_POINT ( 'NONE',  ( -24.26250232874330237, 1444.584236750404443, 211.3627685846172710 ) ) ;
#58966 = CARTESIAN_POINT ( 'NONE',  ( -53.95864250903900228, 1384.721469025669876, 269.7706786227579983 ) ) ;
#58967 = CARTESIAN_POINT ( 'NONE',  ( -106.9811535215749956, 1391.913060387289988, 301.7491911334220163 ) ) ;
#58968 = CARTESIAN_POINT ( 'NONE',  ( 12.17244369425279871, 1416.196255298699953, 223.4846811968139946 ) ) ;
#58969 = B_SPLINE_SURFACE_WITH_KNOTS ( 'NONE', 5, 5, ( 
 ( #49860, #39800, #100253, #83994, #65010, #21855 ),
 ( #73960, #75620, #82894, #57724, #90742, #40888 ),
 ( #108650, #64475, #81781, #15120, #73411, #75070 ),
 ( #109218, #14022, #32504, #24069, #13463, #47653 ),
 ( #5083, #108090, #65566, #30283, #98590, #90180 ),
 ( #39234, #107547, #48213, #99677, #22968, #95164 ),
 ( #77270, #568, #68332, #26285, #68885, #101320 ),
 ( #1121, #102986, #42548, #12, #51504, #34147 ),
 ( #17310, #18421, #103551, #58805, #102439, #8937 ) ),
 .UNSPECIFIED., .F., .F., .F.,
 ( 6, 3, 6 ),
 ( 6, 6 ),
 ( 2.324858856900000159, 4.970096098089999970, 7.657659708029999734 ),
 ( 0.000000000000000000, 0.5000000000000000000 ),
 .UNSPECIFIED. ) ;
#58970 = CARTESIAN_POINT ( 'NONE',  ( -108.2039567000000062, 1378.913060387289988, 299.7295690323589952 ) ) ;
#58971 = DIRECTION ( 'NONE',  ( 0.3090169943749515036, -0.000000000000000000, 0.9510565162951521989 ) ) ;
#58972 = CARTESIAN_POINT ( 'NONE',  ( 12.17073519972539941, 1499.730396604210000, 205.6506567772970016 ) ) ;
#58973 = ADVANCED_FACE ( 'NONE', ( #93686 ), #68071, .T. ) ;
#58974 = CARTESIAN_POINT ( 'NONE',  ( -22.02805665500000032, 1409.682297076129998, 206.3742546035879855 ) ) ;
#58975 = EDGE_CURVE ( 'NONE', #40624, #105727, #82886, .T. ) ;
#58976 = ADVANCED_FACE ( 'NONE', ( #97036 ), #33146, .T. ) ;
#58977 = CARTESIAN_POINT ( 'NONE',  ( -10.17189341190630358, 1380.026521348481310, 202.0760537856158976 ) ) ;
#58978 = CARTESIAN_POINT ( 'NONE',  ( 3.445653300429999621, 1486.078848993990050, 219.3336973419989988 ) ) ;
#58979 = TOROIDAL_SURFACE ( 'NONE', #80403, 2.000000000000000000, 1.000000000000000000 ) ;
#58980 = CARTESIAN_POINT ( 'NONE',  ( -16.59207410940000216, 1408.838686485329845, 269.5630249687979472 ) ) ;
#58981 = ADVANCED_FACE ( 'NONE', ( #63457 ), #104397, .T. ) ;
#58982 = B_SPLINE_SURFACE_WITH_KNOTS ( 'NONE', 5, 5, ( 
 ( #32903, #21729, #99000, #48076, #99552, #22837 ),
 ( #81647, #31261, #58136, #73271, #83865, #49737 ),
 ( #39095, #57042, #107411, #66553, #7168, #5513 ),
 ( #30707, #31813, #32372, #74396, #41326, #91168 ),
 ( #82209, #47526, #6062, #75496, #64893, #39669 ),
 ( #14446, #48640, #100120, #22277, #92269, #73837 ) ),
 .UNSPECIFIED., .F., .F., .F.,
 ( 6, 6 ),
 ( 6, 6 ),
 ( 29.50720980489999690, 158.0245753780000086 ),
 ( 0.000000000000000000, 1.000000000000000000 ),
 .UNSPECIFIED. ) ;
#58983 = CARTESIAN_POINT ( 'NONE',  ( -6.076016477482709455, 1450.645068205029929, 208.7037722137420133 ) ) ;
#58984 = EDGE_CURVE ( 'NONE', #40567, #66989, #75786, .T. ) ;
#58985 = CARTESIAN_POINT ( 'NONE',  ( -19.86464702156969864, 1441.435616204289772, 212.6459227002919761 ) ) ;
#58986 = CARTESIAN_POINT ( 'NONE',  ( -6.140127969266069741, 1508.880864730590019, 216.6292689825000082 ) ) ;
#58987 = CARTESIAN_POINT ( 'NONE',  ( 13.52268460241299941, 1497.923627544540068, 227.8730058996700052 ) ) ;
#58989 = CARTESIAN_POINT ( 'NONE',  ( -2.487934962309999776, 1508.551704408389924, 204.1347675205190058 ) ) ;
#58988 = FACE_OUTER_BOUND ( 'NONE', #78596, .T. ) ;
#58990 = CARTESIAN_POINT ( 'NONE',  ( 11.73681854383099932, 1426.696124960400084, 144.1550751902559853 ) ) ;
#58991 = CARTESIAN_POINT ( 'NONE',  ( 17.59770716511923894, 1524.659802833172989, 237.5598880769025243 ) ) ;
#58992 = CIRCLE ( 'NONE', #7102, 2.000000000000001776 ) ;
#58993 = LINE ( 'NONE', #93655, #11533 ) ;
#58994 = CARTESIAN_POINT ( 'NONE',  ( 8.181958942834999249, 1517.051704408389924, 212.1568108385370124 ) ) ;
#58995 = EDGE_CURVE ( 'NONE', #67802, #73303, #74039, .T. ) ;
#58996 = B_SPLINE_CURVE_WITH_KNOTS ( 'NONE', 3,
 ( #50803, #58114, #66529, #92247, #25021, #109068, #59224, #101178, #33993, #41302, #32350, #68186, #32882, #100633, #23919, #15517, #49714, #51347, #83846, #6040, #40192, #76547, #7145, #16606, #75475, #16068, #109608, #67073, #25574, #24473, #8226, #40742, #59768, #102291, #50271, #31786, #42392 ),
 .UNSPECIFIED., .F., .F.,
 ( 4, 3, 3, 3, 3, 3, 3, 3, 3, 3, 3, 3, 4 ),
 ( -7.474718202020000035, -7.256328811620320174, -6.989423022925070228, -6.695085830317820452, -6.368123258945879606, -5.921286250405219498, -5.573260391803679603, -5.269658889521529943, -5.196602558778829817, -4.761443928031699357, -4.253228966541860778, -3.623072494495270579, -3.064599166389999851 ),
 .UNSPECIFIED. ) ;
#58997 = CARTESIAN_POINT ( 'NONE',  ( -0.2148496144000409946, 1419.222389015129920, 184.6498064978729872 ) ) ;
#58998 = CARTESIAN_POINT ( 'NONE',  ( -6.945490086935000029, 1516.932669162149978, 203.3434733684869968 ) ) ;
#58999 = DIRECTION ( 'NONE',  ( -1.755985294532469921E-16, 1.000000000000000000, -1.338183447452831989E-16 ) ) ;
#59000 = CARTESIAN_POINT ( 'NONE',  ( -13.35004134540000109, 1415.296882282229944, 221.1257189973979962 ) ) ;
#59001 = CARTESIAN_POINT ( 'NONE',  ( 16.46592301883499943, 1512.456207068040158, 197.3724380419670297 ) ) ;
#59002 = FACE_BOUND ( 'NONE', #67145, .T. ) ;
#59003 = CARTESIAN_POINT ( 'NONE',  ( -33.96591335708179571, 1378.821001449670121, 222.2770748186169953 ) ) ;
#59004 = CIRCLE ( 'NONE', #85840, 1.999999999999998668 ) ;
#59005 = CARTESIAN_POINT ( 'NONE',  ( 21.17557709188830017, 1509.351061401330071, 228.3384711562210043 ) ) ;
#59007 = ORIENTED_EDGE ( 'NONE', *, *, #26837, .F. ) ;
#59006 = CARTESIAN_POINT ( 'NONE',  ( -21.72241338915559794, 1379.603549772170254, 213.5570291714129780 ) ) ;
#59008 = ORIENTED_EDGE ( 'NONE', *, *, #23852, .F. ) ;
#59009 = CARTESIAN_POINT ( 'NONE',  ( 11.53651591631439999, 1434.720663866509994, 151.3975021344279810 ) ) ;
#59010 = CARTESIAN_POINT ( 'NONE',  ( -6.779985536469999907, 1396.149822699429933, 218.3141025366080044 ) ) ;
#59011 = VERTEX_POINT ( 'NONE', #105430 ) ;
#59012 = CARTESIAN_POINT ( 'NONE',  ( -0.0002532898294781912862, 1396.497903775337136, 221.5346559189089817 ) ) ;
#59013 = FACE_OUTER_BOUND ( 'NONE', #94959, .T. ) ;
#59014 = DIRECTION ( 'NONE',  ( 0.000000000000000000, -1.000000000000000000, 0.000000000000000000 ) ) ;
#59016 = CARTESIAN_POINT ( 'NONE',  ( -13.71800425710380011, 1507.970762863469872, 184.2200768164369720 ) ) ;
#59015 = CARTESIAN_POINT ( 'NONE',  ( 3.329657646939999438, 1445.620183030290036, 200.6158394109289986 ) ) ;
#59017 = CARTESIAN_POINT ( 'NONE',  ( 19.29102239047420042, 1488.415415665300088, 228.6203174551539803 ) ) ;
#59018 = EDGE_CURVE ( 'NONE', #76827, #17927, #18304, .T. ) ;
#59019 = CARTESIAN_POINT ( 'NONE',  ( 1.309051754279999980, 1468.707717750329948, 182.7499832783979912 ) ) ;
#59020 = CARTESIAN_POINT ( 'NONE',  ( 2.864776410889999791, 1467.969787444489839, 218.6984507715789903 ) ) ;
#59021 = CARTESIAN_POINT ( 'NONE',  ( 44.43457369424350389, 1440.913053162589904, 270.0922382296420210 ) ) ;
#59022 = SURFACE_SIDE_STYLE ('',( #16417 ) ) ;
#59024 = EDGE_CURVE ( 'NONE', #47969, #101819, #36452, .T. ) ;
#59023 = CARTESIAN_POINT ( 'NONE',  ( 6.531167973260561865, 1522.051704408389924, 201.5366623270788295 ) ) ;
#59025 = CARTESIAN_POINT ( 'NONE',  ( 14.45145579027819949, 1416.702560754929891, 196.8582874468680188 ) ) ;
#59026 = CARTESIAN_POINT ( 'NONE',  ( 11.85618979400000050, 1431.606717022440080, 150.3527028125979825 ) ) ;
#59027 = CARTESIAN_POINT ( 'NONE',  ( 6.055196916395000351, 1514.134513140259969, 201.4763673648269844 ) ) ;
#59028 = ORIENTED_EDGE ( 'NONE', *, *, #74320, .T. ) ;
#59029 = CARTESIAN_POINT ( 'NONE',  ( 12.95217011737299906, 1434.756318633420051, 149.1861961083450012 ) ) ;
#59030 = ORIENTED_EDGE ( 'NONE', *, *, #67325, .T. ) ;
#59031 = ADVANCED_FACE ( 'NONE', ( #36565 ), #21888, .T. ) ;
#59032 = ORIENTED_EDGE ( 'NONE', *, *, #12505, .T. ) ;
#59033 = CARTESIAN_POINT ( 'NONE',  ( 13.44657628210572575, 1444.308568810446104, 169.3633758692288040 ) ) ;
#59034 = CARTESIAN_POINT ( 'NONE',  ( -6.868311248510000411, 1463.903099144130010, 235.5040378045979992 ) ) ;
#59035 = AXIS2_PLACEMENT_3D ( 'NONE', #87187, #45207, #12128 ) ;
#59036 = CARTESIAN_POINT ( 'NONE',  ( -10.07154918488590134, 1473.228065907060000, 207.4129428866500007 ) ) ;
#59037 = CARTESIAN_POINT ( 'NONE',  ( 1.708720984574999768, 1516.531533746980131, 216.4430152012269843 ) ) ;
#59038 = CARTESIAN_POINT ( 'NONE',  ( -8.609273301071175055, 1511.418042823250744, 214.3800210669276112 ) ) ;
#59039 = EDGE_CURVE ( 'NONE', #58469, #9890, #17584, .T. ) ;
#59040 = CARTESIAN_POINT ( 'NONE',  ( -11.43590621159999898, 1501.508488288289982, 208.4755739533859753 ) ) ;
#59041 = CARTESIAN_POINT ( 'NONE',  ( 2.500000000000000000, 1448.349745776700047, 163.1876515373769791 ) ) ;
#59042 = CARTESIAN_POINT ( 'NONE',  ( 5.105014162403789241E-14, 1376.342264060500156, 206.9293834673690071 ) ) ;
#59043 = ORIENTED_EDGE ( 'NONE', *, *, #30159, .T. ) ;
#59044 = CARTESIAN_POINT ( 'NONE',  ( 0.7353365397730019515, 1516.995911393979895, 206.2425275143270085 ) ) ;
#59045 = VERTEX_POINT ( 'NONE', #28719 ) ;
#59046 = CARTESIAN_POINT ( 'NONE',  ( 21.73410520339709961, 1440.913060387330006, 226.0964448684460137 ) ) ;
#59047 = AXIS2_PLACEMENT_3D ( 'NONE', #46775, #80907, #20422 ) ;
#59048 = CARTESIAN_POINT ( 'NONE',  ( -19.34325532379999757, 1509.569025808630158, 231.1400346091979827 ) ) ;
#59049 = CARTESIAN_POINT ( 'NONE',  ( -11.71720101390000046, 1409.322234063030010, 190.6809772676980117 ) ) ;
#59050 = CARTESIAN_POINT ( 'NONE',  ( 7.643022747455000321, 1513.886778334019937, 216.1363302133069908 ) ) ;
#59052 = ORIENTED_EDGE ( 'NONE', *, *, #56997, .T. ) ;
#59051 = CARTESIAN_POINT ( 'NONE',  ( 4.163336342339999869E-15, 1416.177402202029953, 209.1218459616989946 ) ) ;
#59053 = CARTESIAN_POINT ( 'NONE',  ( 20.62552256830000275, 1428.450544870129988, 221.6279733991980265 ) ) ;
#59054 = DIRECTION ( 'NONE',  ( 1.755985294532464991E-16, -1.000000000000000000, 1.338183447452830017E-16 ) ) ;
#59055 = CARTESIAN_POINT ( 'NONE',  ( -102.7434157679999913, 1384.036053956720025, 311.1373841372590050 ) ) ;
#59056 = DIRECTION ( 'NONE',  ( 1.040834085586083310E-14, 0.000000000000000000, 1.000000000000000000 ) ) ;
#59057 = CARTESIAN_POINT ( 'NONE',  ( 21.92916355573829890, 1523.390106123591067, 183.0654104491179908 ) ) ;
#59058 = CARTESIAN_POINT ( 'NONE',  ( 2.489617538345000103, 1516.665179208830068, 214.1178407578070164 ) ) ;
#59059 = CARTESIAN_POINT ( 'NONE',  ( 4.637787270109999582, 1462.124489585889933, 228.1829287868989979 ) ) ;
#59060 = EDGE_CURVE ( 'NONE', #100304, #34471, #52539, .T. ) ;
#59061 = CARTESIAN_POINT ( 'NONE',  ( 23.89892935376693828, 1410.398181730384294, 209.5833290241005500 ) ) ;
#59062 = CARTESIAN_POINT ( 'NONE',  ( -11.20854089327220038, 1414.996442620800053, 195.7122650692939771 ) ) ;
#59063 = CARTESIAN_POINT ( 'NONE',  ( 7.725990161824999980, 1517.181921232829836, 211.6070516194370157 ) ) ;
#59065 = ADVANCED_FACE ( 'NONE', ( #88640 ), #100849, .F. ) ;
#59064 = CARTESIAN_POINT ( 'NONE',  ( 20.14739811709999984, 1412.328483943929996, 271.1218459616979999 ) ) ;
#59066 = CARTESIAN_POINT ( 'NONE',  ( -11.86685402762820019, 1482.064906951660078, 208.4268465260890082 ) ) ;
#59067 = CARTESIAN_POINT ( 'NONE',  ( -10.59445717635187023, 1486.014368868439760, 184.0782091622903636 ) ) ;
#59069 = ORIENTED_EDGE ( 'NONE', *, *, #66582, .T. ) ;
#59068 = CARTESIAN_POINT ( 'NONE',  ( -52.50755113500000704, 1388.282985474849966, 231.2999456731590158 ) ) ;
#59070 = CARTESIAN_POINT ( 'NONE',  ( -53.77332582030280150, 1385.099635535869993, 269.3953241406759957 ) ) ;
#59071 = VECTOR ( 'NONE', #78009, 1000.000000000000000 ) ;
#59072 = B_SPLINE_SURFACE_WITH_KNOTS ( 'NONE', 5, 5, ( 
 ( #30480, #64668, #47842, #5283, #39439, #31028 ),
 ( #99322, #77462, #51155, #9689, #67423, #92584 ),
 ( #85851, #42201, #68523, #76352, #69081, #764 ),
 ( #24275, #93674, #110501, #58456, #109415, #33781 ),
 ( #67978, #50603, #34893, #60680, #9150, #102085 ),
 ( #25368, #93141, #100980, #94806, #101522, #32691 ) ),
 .UNSPECIFIED., .F., .F., .F.,
 ( 6, 6 ),
 ( 6, 6 ),
 ( 5.893388375706040350, 9.819929736133959253 ),
 ( 0.000000000000000000, 0.5002947206939659663 ),
 .UNSPECIFIED. ) ;
#59073 = CARTESIAN_POINT ( 'NONE',  ( 29.43658765730000226, 1455.581846386829966, 250.1802633525980184 ) ) ;
#59074 = LINE ( 'NONE', #41148, #2058 ) ;
#59075 = B_SPLINE_CURVE_WITH_KNOTS ( 'NONE', 5,
 ( #3448, #37578, #71780, #35372, #103680, #26980 ),
 .UNSPECIFIED., .F., .F.,
 ( 6, 6 ),
 ( 297.9944221590000097, 302.8993106099999864 ),
 .UNSPECIFIED. ) ;
#59076 = CARTESIAN_POINT ( 'NONE',  ( -0.8945946638535250406, 1417.298095655010002, 235.8147265033050246 ) ) ;
#59077 = AXIS2_PLACEMENT_3D ( 'NONE', #35745, #110234, #59858 ) ;
#59078 = CARTESIAN_POINT ( 'NONE',  ( -19.18813880309999931, 1465.797355387890093, 204.3301597990889888 ) ) ;
#59079 = CARTESIAN_POINT ( 'NONE',  ( 0.9900606234040129072, 1452.889512402500031, 183.3744259742010172 ) ) ;
#59080 = EDGE_CURVE ( 'NONE', #79053, #101350, #91247, .T. ) ;
#59082 = DIRECTION ( 'NONE',  ( 0.000000000000000000, 0.000000000000000000, -1.000000000000000000 ) ) ;
#59081 = CARTESIAN_POINT ( 'NONE',  ( -1.126138146715000010, 1517.208444099459939, 216.8485306577670144 ) ) ;
#59083 = CARTESIAN_POINT ( 'NONE',  ( 2.956070248525000110, 1512.851027015570025, 217.0276636870669904 ) ) ;
#59084 = CARTESIAN_POINT ( 'NONE',  ( -108.7920667164509894, 1381.754968429450173, 310.6777004439369989 ) ) ;
#59085 = VERTEX_POINT ( 'NONE', #65636 ) ;
#59086 = CARTESIAN_POINT ( 'NONE',  ( -3.261635970955000019, 1516.613881697390070, 202.1867125516770045 ) ) ;
#59087 = CARTESIAN_POINT ( 'NONE',  ( -27.01382282590000017, 1451.969727051930022, 134.9184453750980026 ) ) ;
#59088 = CARTESIAN_POINT ( 'NONE',  ( 12.97050746999999937, 1422.770599689629762, 223.1036895935980056 ) ) ;
#59089 = CARTESIAN_POINT ( 'NONE',  ( -31.95643112690575549, 1526.329757971585195, 216.6807372299043095 ) ) ;
#59090 = CARTESIAN_POINT ( 'NONE',  ( -2.500000000000000000, 1423.874532570859856, 167.3087045243360080 ) ) ;
#59091 = CARTESIAN_POINT ( 'NONE',  ( -1.194268154760000034, 1444.571194286590071, 218.0071140876989944 ) ) ;
#59092 = DIRECTION ( 'NONE',  ( 0.9983395709201744461, -0.05760296116452706672, 0.000000000000000000 ) ) ;
#59093 = CARTESIAN_POINT ( 'NONE',  ( 29.70034918587519712, 1435.534590375950074, 135.6337138702669733 ) ) ;
#59094 = ADVANCED_FACE ( 'NONE', ( #74585 ), #77550, .T. ) ;
#59095 = CARTESIAN_POINT ( 'NONE',  ( 37.77054191136320327, 1449.013782357440050, 136.3553928163400144 ) ) ;
#59096 = CARTESIAN_POINT ( 'NONE',  ( -3.793562082119010803, 1450.899618466582069, 184.9307169054388282 ) ) ;
#59097 = CARTESIAN_POINT ( 'NONE',  ( -108.5296511849999916, 1386.299881632349980, 297.3615022879590128 ) ) ;
#59098 = CARTESIAN_POINT ( 'NONE',  ( 12.44163360890000014, 1509.176498968829947, 183.7399934378979935 ) ) ;
#59099 = CARTESIAN_POINT ( 'NONE',  ( 3.927179831460580139, 1507.318492355100034, 220.1472266827140061 ) ) ;
#59100 = CARTESIAN_POINT ( 'NONE',  ( -1.073559340110749938, 1444.993510080170154, 218.0402162255370229 ) ) ;
#59101 = VERTEX_POINT ( 'NONE', #75138 ) ;
#59103 = ADVANCED_FACE ( 'NONE', ( #107070 ), #91913, .T. ) ;
#59102 = DIRECTION ( 'NONE',  ( -1.755985294532469921E-16, 1.000000000000000000, -1.338183447452831989E-16 ) ) ;
#59104 = CARTESIAN_POINT ( 'NONE',  ( -42.89947813909407159, 1429.237451840416952, 269.0512739436722995 ) ) ;
#59105 = CARTESIAN_POINT ( 'NONE',  ( -3.958644675774470212, 1508.551704408389924, 214.1089269091330038 ) ) ;
#59106 = CARTESIAN_POINT ( 'NONE',  ( 14.62884502624119953, 1434.834865051830093, 190.3726805430140132 ) ) ;
#59107 = CONICAL_SURFACE ( 'NONE', #73402, 6.911399307709998219, 0.04363323129990067523 ) ;
#59108 = CARTESIAN_POINT ( 'NONE',  ( -0.3094189819459999824, 1415.413778627430020, 233.4271496902980232 ) ) ;
#59109 = CARTESIAN_POINT ( 'NONE',  ( -11.43185072513739797, 1443.913060387330006, 147.9056598087979921 ) ) ;
#59110 = CARTESIAN_POINT ( 'NONE',  ( -28.30491477860000060, 1508.660124211329958, 209.1318398264210145 ) ) ;
#59111 = B_SPLINE_SURFACE_WITH_KNOTS ( 'NONE', 5, 4, ( 
 ( #101825, #52011, #33515, #32975, #84493 ),
 ( #43058, #17256, #16703, #77216, #86151 ),
 ( #50903, #9444, #92888, #51448, #43608 ),
 ( #93434, #94536, #24008, #16164, #85034 ),
 ( #59322, #66623, #67715, #24561, #41947 ),
 ( #34644, #85579, #8326, #92331, #68828 ) ),
 .UNSPECIFIED., .F., .F., .F.,
 ( 6, 6 ),
 ( 5, 5 ),
 ( 0.000000000000000000, 52.98902693510000006 ),
 ( 40.20365518519999881, 50.26548245740000453 ),
 .UNSPECIFIED. ) ;
#59112 = DIRECTION ( 'NONE',  ( -0.4999999999998399058, 0.7071067811867739472, -0.4999999999998399058 ) ) ;
#59113 = CARTESIAN_POINT ( 'NONE',  ( -4.020406191785280470, 1515.375307391110027, 212.6641346454879908 ) ) ;
#59114 = CARTESIAN_POINT ( 'NONE',  ( 44.93136303398450337, 1440.913046276439900, 269.6838066906610152 ) ) ;
#59115 = CARTESIAN_POINT ( 'NONE',  ( -17.35680393429759860, 1451.072033954267226, 148.0582205165680705 ) ) ;
#59116 = CARTESIAN_POINT ( 'NONE',  ( -22.86388144358860330, 1435.295931049460023, 134.1000000049170069 ) ) ;
#59117 = CARTESIAN_POINT ( 'NONE',  ( 25.71088399069999753, 1436.647695531819863, 137.0958841102980159 ) ) ;
#59118 = EDGE_CURVE ( 'NONE', #84300, #45857, #56121, .T. ) ;
#59119 = CARTESIAN_POINT ( 'NONE',  ( -13.02011975896744111, 1442.961602265839474, 169.4183208322911582 ) ) ;
#59120 = ORIENTED_EDGE ( 'NONE', *, *, #83912, .T. ) ;
#59121 = CIRCLE ( 'NONE', #82359, 30.10786454236638576 ) ;
#59122 = CARTESIAN_POINT ( 'NONE',  ( -0.3551244063711440080, 1416.218047878440075, 191.1510195321629908 ) ) ;
#59123 = ADVANCED_FACE ( 'NONE', ( #74033 ), #49379, .F. ) ;
#59124 = CARTESIAN_POINT ( 'NONE',  ( 21.38848997940215924, 1509.000357915978839, 226.3836373717206527 ) ) ;
#59125 = VERTEX_POINT ( 'NONE', #83505 ) ;
#59126 = ORIENTED_EDGE ( 'NONE', *, *, #68000, .F. ) ;
#59127 = CARTESIAN_POINT ( 'NONE',  ( -0.6255756489468429216, 1435.976707381580127, 227.5909497020410015 ) ) ;
#59128 = CARTESIAN_POINT ( 'NONE',  ( -14.93598579144041416, 1416.108359274850045, 205.2289421662831330 ) ) ;
#59130 = CARTESIAN_POINT ( 'NONE',  ( -3.627898411379999910, 1459.479586690430096, 211.7966661443780083 ) ) ;
#59129 = CARTESIAN_POINT ( 'NONE',  ( 1.326715741870000187, 1454.806610190989886, 218.4390638076189930 ) ) ;
#59131 = CARTESIAN_POINT ( 'NONE',  ( -1.591562321820000125, 1443.444047077889991, 218.6175910282489951 ) ) ;
#59132 = CARTESIAN_POINT ( 'NONE',  ( 4.243141308438709736, 1425.234291684319942, 185.3368633770080010 ) ) ;
#59133 = EDGE_CURVE ( 'NONE', #106936, #50244, #41869, .T. ) ;
#59134 = CARTESIAN_POINT ( 'NONE',  ( -12.30596913808479975, 1378.368950717130019, 209.8692018423830064 ) ) ;
#59135 = CARTESIAN_POINT ( 'NONE',  ( -2.586211294052060072, 1420.639117752620450, 185.6985776663195509 ) ) ;
#59136 = CARTESIAN_POINT ( 'NONE',  ( 7.566081195099999768, 1424.291034983149984, 212.3491042945289848 ) ) ;
#59137 = CARTESIAN_POINT ( 'NONE',  ( -24.66478414839999900, 1440.651724578850235, 210.6803367953379791 ) ) ;
#59138 = CARTESIAN_POINT ( 'NONE',  ( -4.251240061320140207, 1453.776278923900236, 199.5516788180739809 ) ) ;
#59139 = CARTESIAN_POINT ( 'NONE',  ( 2.054351737509999776, 1450.909068314819933, 183.2085949937979876 ) ) ;
#59140 = CARTESIAN_POINT ( 'NONE',  ( 9.622136349646140729, 1363.684386430199993, 210.6218459616987957 ) ) ;
#59141 = ADVANCED_FACE ( 'NONE', ( #21928 ), #40409, .T. ) ;
#59142 = CARTESIAN_POINT ( 'NONE',  ( -27.88347671565054497, 1509.998607907042697, 220.2191159836331735 ) ) ;
#59143 = EDGE_CURVE ( 'NONE', #13894, #75732, #66201, .T. ) ;
#59145 = ORIENTED_EDGE ( 'NONE', *, *, #86680, .F. ) ;
#59144 = CARTESIAN_POINT ( 'NONE',  ( -2.787097905305880323E-09, 1415.115138440810142, 244.0122842078770020 ) ) ;
#59146 = ORIENTED_EDGE ( 'NONE', *, *, #89094, .F. ) ;
#59147 = CARTESIAN_POINT ( 'NONE',  ( -2.140641997699999965, 1508.551704408389924, 220.0635241299990241 ) ) ;
#59148 = CARTESIAN_POINT ( 'NONE',  ( -2.760778634279479782, 1409.009468901610035, 188.0459411385839985 ) ) ;
#59149 = CARTESIAN_POINT ( 'NONE',  ( -6.198205771480000514, 1471.106402530630021, 269.3395160832980082 ) ) ;
#59150 = DIRECTION ( 'NONE',  ( -0.9412234725396940727, 0.02592281343750019867, -0.3367883348392645138 ) ) ;
#59151 = CARTESIAN_POINT ( 'NONE',  ( -106.3317231422732476, 1368.558218059090223, 316.1375217595586946 ) ) ;
#59152 = AXIS2_PLACEMENT_3D ( 'NONE', #63885, #64978, #105317 ) ;
#59153 = CARTESIAN_POINT ( 'NONE',  ( -13.58268883541719951, 1416.851343898680170, 221.9096085506480165 ) ) ;
#59154 = CARTESIAN_POINT ( 'NONE',  ( -0.4328695768656839471, 1475.687559908960111, 197.6741279352499987 ) ) ;
#59155 = CARTESIAN_POINT ( 'NONE',  ( -113.4000000000000057, 1305.714868215269917, 304.2218459572590064 ) ) ;
#59156 = CARTESIAN_POINT ( 'NONE',  ( 9.231361398829999843, 1366.659448741839924, 207.6218459616989946 ) ) ;
#59157 = DIRECTION ( 'NONE',  ( -7.436362843295819681E-17, 1.000000000000000000, -1.457576885956999882E-16 ) ) ;
#59158 = CARTESIAN_POINT ( 'NONE',  ( -18.82370638324319856, 1408.747051114209853, 268.3329375438490274 ) ) ;
#59159 = CARTESIAN_POINT ( 'NONE',  ( -13.60407173860000007, 1435.200345218290067, 149.7125188640980014 ) ) ;
#59160 = ORIENTED_EDGE ( 'NONE', *, *, #99298, .T. ) ;
#59161 = CARTESIAN_POINT ( 'NONE',  ( -4.327511837212590251, 1515.138761592190122, 209.7121513359620337 ) ) ;
#59162 = EDGE_CURVE ( 'NONE', #55526, #22209, #31102, .T. ) ;
#59163 = CARTESIAN_POINT ( 'NONE',  ( 13.49221535360000068, 1444.360430239190009, 188.3140289464980128 ) ) ;
#59164 = ORIENTED_EDGE ( 'NONE', *, *, #15213, .F. ) ;
#59165 = ORIENTED_EDGE ( 'NONE', *, *, #74475, .F. ) ;
#59166 = CARTESIAN_POINT ( 'NONE',  ( -22.04844205606989149, 1506.512156832672417, 209.1936639346002949 ) ) ;
#59167 = CARTESIAN_POINT ( 'NONE',  ( 7.982669098950510467, 1424.960829083689987, 194.4768953556059898 ) ) ;
#59168 = ADVANCED_FACE ( 'NONE', ( #58878, #16283 ), #84610, .F. ) ;
#59169 = CARTESIAN_POINT ( 'NONE',  ( -5.774609660074999873, 1516.777260590120022, 213.7418541773069762 ) ) ;
#59170 = CARTESIAN_POINT ( 'NONE',  ( -13.12714717100000072, 1470.463974201930114, 186.8692217856980164 ) ) ;
#59171 = AXIS2_PLACEMENT_3D ( 'NONE', #46526, #64428, #21261 ) ;
#59172 = CARTESIAN_POINT ( 'NONE',  ( -9.702212350455228673, 1471.555838493580040, 212.0786635793400023 ) ) ;
#59173 = VERTEX_POINT ( 'NONE', #42620 ) ;
#59174 = DIRECTION ( 'NONE',  ( 0.03173147633638118831, -0.9969860201949398704, 0.07079540200725417676 ) ) ;
#59175 = CARTESIAN_POINT ( 'NONE',  ( 7.715625202974999652, 1516.786099423779888, 202.5670817708370066 ) ) ;
#59176 = CARTESIAN_POINT ( 'NONE',  ( -27.42461697039999891, 1509.627276150529951, 202.3633461635780009 ) ) ;
#59177 = CARTESIAN_POINT ( 'NONE',  ( 1.418617516391186495, 1507.072688282607032, 236.8007530455898006 ) ) ;
#59178 = CARTESIAN_POINT ( 'NONE',  ( -46.34909325035440020, 1384.604549084440123, 220.0612681586810311 ) ) ;
#59179 = CARTESIAN_POINT ( 'NONE',  ( -2.658297512749999925, 1408.468078491630195, 195.7434692079979754 ) ) ;
#59180 = AXIS2_PLACEMENT_3D ( 'NONE', #99546, #32896, #50291 ) ;
#59181 = CARTESIAN_POINT ( 'NONE',  ( -10.14857146045310010, 1472.086425147420186, 209.7191475320900054 ) ) ;
#59183 = VERTEX_POINT ( 'NONE', #76772 ) ;
#59182 = CARTESIAN_POINT ( 'NONE',  ( 15.56983241408575580, 1506.527232289068252, 193.4924744589925183 ) ) ;
#59184 = CARTESIAN_POINT ( 'NONE',  ( -24.99664572855169808, 1430.498658011320231, 209.0631888998489956 ) ) ;
#59185 = CARTESIAN_POINT ( 'NONE',  ( 26.66951752199999959, 1488.685949850129873, 212.9498159561979946 ) ) ;
#59186 = CARTESIAN_POINT ( 'NONE',  ( -53.46082045212465772, 1379.704646932813830, 252.6341302468160848 ) ) ;
#59187 = CARTESIAN_POINT ( 'NONE',  ( -8.922475182707978902, 1440.999127764592004, 204.4963557433056565 ) ) ;
#59188 = CARTESIAN_POINT ( 'NONE',  ( -15.20279581456499862, 1516.814170398969964, 193.2119433744669834 ) ) ;
#59189 = AXIS2_PLACEMENT_3D ( 'NONE', #73989, #30863, #55546 ) ;
#59190 = CARTESIAN_POINT ( 'NONE',  ( 0.01323701367210150005, 1516.939658295650133, 211.6080660720070341 ) ) ;
#59191 = CARTESIAN_POINT ( 'NONE',  ( -68.57934351740000523, 1379.747889361729904, 279.7331283945590030 ) ) ;
#59192 = AXIS2_PLACEMENT_3D ( 'NONE', #101768, #100673, #76589 ) ;
#59193 = DIRECTION ( 'NONE',  ( 1.000000000000000000, 0.000000000000000000, 0.000000000000000000 ) ) ;
#59194 = CARTESIAN_POINT ( 'NONE',  ( 4.492546581380000958, 1453.878649273890005, 217.3453973181289882 ) ) ;
#59195 = CARTESIAN_POINT ( 'NONE',  ( 3.447128460625000113, 1516.778853242349896, 207.9866608880570027 ) ) ;
#59196 = EDGE_LOOP ( 'NONE', ( #95966, #48724, #77152, #19061, #47855 ) ) ;
#59197 = LINE ( 'NONE', #109041, #88490 ) ;
#59198 = CARTESIAN_POINT ( 'NONE',  ( -10.13245368019999937, 1472.295917692089915, 207.1576018941290158 ) ) ;
#59199 = CARTESIAN_POINT ( 'NONE',  ( -5.958828918610000080, 1384.900097640590047, 218.5255276338789940 ) ) ;
#59200 = ORIENTED_EDGE ( 'NONE', *, *, #31011, .T. ) ;
#59202 = AXIS2_PLACEMENT_3D ( 'NONE', #69026, #9628, #69583 ) ;
#59201 = CARTESIAN_POINT ( 'NONE',  ( 10.95098205620359977, 1471.837422849929908, 212.3987392730099657 ) ) ;
#59203 = CARTESIAN_POINT ( 'NONE',  ( -23.97468780672586774, 1509.756983508501435, 226.3117272632610479 ) ) ;
#59204 = CARTESIAN_POINT ( 'NONE',  ( -4.087001431972547394, 1440.394582734599453, 185.3240461973863660 ) ) ;
#59205 = CARTESIAN_POINT ( 'NONE',  ( -12.35910314799999909, 1415.406472713659923, 208.4697927874989887 ) ) ;
#59206 = CARTESIAN_POINT ( 'NONE',  ( -11.41042431937685819, 1425.708686112080841, 138.9044708858078820 ) ) ;
#59207 = CARTESIAN_POINT ( 'NONE',  ( 3.889852026509999838, 1485.593720051389937, 199.0907241709990103 ) ) ;
#59208 = CARTESIAN_POINT ( 'NONE',  ( 3.610745725306120146, 1430.587129522550185, 217.8985349120129911 ) ) ;
#59209 = DIRECTION ( 'NONE',  ( 0.000000000000000000, 0.000000000000000000, 1.000000000000000000 ) ) ;
#59211 = LINE ( 'NONE', #14411, #94210 ) ;
#59210 = CARTESIAN_POINT ( 'NONE',  ( -5.774609660074999873, 1516.777260590120022, 213.7418541773069762 ) ) ;
#59212 = CARTESIAN_POINT ( 'NONE',  ( 20.06869819519999965, 1507.849569125829930, 189.2236336047979819 ) ) ;
#59213 = CARTESIAN_POINT ( 'NONE',  ( 6.554764161265000055, 1516.786099423779888, 216.8374711732070068 ) ) ;
#59214 = ORIENTED_EDGE ( 'NONE', *, *, #8571, .T. ) ;
#59215 = CARTESIAN_POINT ( 'NONE',  ( -12.45702696549999899, 1416.837177087930058, 194.7670149573980041 ) ) ;
#59216 = CARTESIAN_POINT ( 'NONE',  ( -16.90511930290000109, 1420.406826955899987, 203.3373784124190138 ) ) ;
#59217 = ORIENTED_EDGE ( 'NONE', *, *, #55721, .T. ) ;
#59218 = CARTESIAN_POINT ( 'NONE',  ( 1.148639102450000005, 1420.599583713030142, 184.1279056854980070 ) ) ;
#59219 =( BOUNDED_CURVE ( )  B_SPLINE_CURVE ( 3, ( #37218, #71961, #29351, #63551 ),
 .UNSPECIFIED., .F., .F. ) 
 B_SPLINE_CURVE_WITH_KNOTS ( ( 4, 4 ),
 ( 2.890157810870130017, 3.288561387820169823 ),
 .UNSPECIFIED. ) 
 CURVE ( )  GEOMETRIC_REPRESENTATION_ITEM ( )  RATIONAL_B_SPLINE_CURVE ( ( 1.000000000000000000, 0.9868165638355377300, 0.9868165638355377300, 1.000000000000000000 ) ) 
 REPRESENTATION_ITEM ( '' )  );
#59220 = CARTESIAN_POINT ( 'NONE',  ( -21.51339057090000040, 1505.551704408389924, 209.1218459616989946 ) ) ;
#59221 = CARTESIAN_POINT ( 'NONE',  ( 3.302346719094112260, 1524.524650307243519, 176.3741577287142661 ) ) ;
#59222 = UNCERTAINTY_MEASURE_WITH_UNIT (LENGTH_MEASURE( 1.000000000000000082E-05 ), #43444, 'distance_accuracy_value', 'NONE');
#59223 = FACE_OUTER_BOUND ( 'NONE', #91076, .T. ) ;
#59224 = CARTESIAN_POINT ( 'NONE',  ( -11.22547157564759956, 1471.287375098959956, 207.0499038567439811 ) ) ;
#59225 = CARTESIAN_POINT ( 'NONE',  ( -6.064879440841631997, 1508.311297157248646, 220.0963463610631834 ) ) ;
#59226 = CARTESIAN_POINT ( 'NONE',  ( 17.02668221408760019, 1422.112876149069962, 226.8213126862850118 ) ) ;
#59227 = CARTESIAN_POINT ( 'NONE',  ( 18.02574679518840028, 1424.482682570480165, 224.6196048480980210 ) ) ;
#59228 = CARTESIAN_POINT ( 'NONE',  ( 17.84054674790834127, 1523.580204110584191, 180.3625987835367539 ) ) ;
#59229 = CARTESIAN_POINT ( 'NONE',  ( -7.362632729190000447, 1435.943783413959864, 149.6281905168980302 ) ) ;
#59230 = CARTESIAN_POINT ( 'NONE',  ( 40.29567722275079689, 1440.913060362669967, 259.7007748391999939 ) ) ;
#59232 = CARTESIAN_POINT ( 'NONE',  ( 5.172586535390000684, 1492.767659076290101, 188.8148697515989909 ) ) ;
#59231 = CARTESIAN_POINT ( 'NONE',  ( -14.75797601881649967, 1418.752372393509859, 201.0755002445320088 ) ) ;
#59233 = CARTESIAN_POINT ( 'NONE',  ( 17.17241001986506888, 1512.187213306747481, 238.6251415217915337 ) ) ;
#59234 = ORIENTED_EDGE ( 'NONE', *, *, #47348, .T. ) ;
#59235 = VERTEX_POINT ( 'NONE', #88 ) ;
#59236 = CARTESIAN_POINT ( 'NONE',  ( 1.547965266439779830, 1416.384967866679972, 190.2939387135980098 ) ) ;
#59237 = CARTESIAN_POINT ( 'NONE',  ( -8.899876699774402766, 1506.575639936663492, 229.3526251636746167 ) ) ;
#59238 = CARTESIAN_POINT ( 'NONE',  ( -27.70374316190000030, 1507.991978473030031, 210.5564529905680047 ) ) ;
#59239 = DIRECTION ( 'NONE',  ( -0.6736849260863841948, 0.000000000000000000, 0.7390186874254148774 ) ) ;
#59240 = CARTESIAN_POINT ( 'NONE',  ( -12.61172662586290016, 1379.083473090599909, 208.5076072890859962 ) ) ;
#59241 = CARTESIAN_POINT ( 'NONE',  ( 27.55277507892554212, 1509.987269819408084, 220.9896407951380581 ) ) ;
#59242 = CARTESIAN_POINT ( 'NONE',  ( -4.636100717163651019, 1378.002096502181075, 203.9687531828620877 ) ) ;
#59243 = CARTESIAN_POINT ( 'NONE',  ( 13.15726447020000123, 1414.996442546130083, 197.7616625855980033 ) ) ;
#59244 = CARTESIAN_POINT ( 'NONE',  ( -60.45726899866969717, 1383.796084930870165, 281.3943264362069954 ) ) ;
#59245 = CARTESIAN_POINT ( 'NONE',  ( -0.04349597063549999476, 1452.084370640529869, 153.9873413333980068 ) ) ;
#59246 = CARTESIAN_POINT ( 'NONE',  ( -5.292247061280000331, 1391.913060387289988, 214.4361776263990009 ) ) ;
#59248 = VECTOR ( 'NONE', #67035, 1000.000000000000114 ) ;
#59247 = CARTESIAN_POINT ( 'NONE',  ( 11.86864872463300102, 1492.042928286840151, 209.5967942225589979 ) ) ;
#59250 = VERTEX_POINT ( 'NONE', #2842 ) ;
#59249 = CARTESIAN_POINT ( 'NONE',  ( -3.060197065649999715, 1457.550370828590076, 218.5492502934789911 ) ) ;
#59251 = CARTESIAN_POINT ( 'NONE',  ( -1.228956895969999907, 1451.852644323129880, 183.6261370569979761 ) ) ;
#59252 = CARTESIAN_POINT ( 'NONE',  ( -68.70547844060000386, 1384.729371863979850, 263.4329467144589785 ) ) ;
#59253 = ADVANCED_FACE ( 'NONE', ( #1743 ), #79001, .T. ) ;
#59254 = CARTESIAN_POINT ( 'NONE',  ( 4.984765438547570149, 1508.551704408389924, 206.5097441823970144 ) ) ;
#59255 = VERTEX_POINT ( 'NONE', #78431 ) ;
#59256 = ORIENTED_EDGE ( 'NONE', *, *, #14562, .T. ) ;
#59257 = CARTESIAN_POINT ( 'NONE',  ( 19.75505552754349736, 1509.267941800199878, 230.0092462747840045 ) ) ;
#59258 = CARTESIAN_POINT ( 'NONE',  ( -8.235011779212388916, 1386.670742518729867, 218.5434337873010122 ) ) ;
#59259 = CARTESIAN_POINT ( 'NONE',  ( 0.000000000000000000, 1512.187213306747481, 174.3106345060153046 ) ) ;
#59261 = CARTESIAN_POINT ( 'NONE',  ( -2.372478608332516892, 1522.382868172863937, 243.3440112565233449 ) ) ;
#59260 = DIRECTION ( 'NONE',  ( -0.1306151939486110136, 0.9872726063158969723, 0.09073297045717730602 ) ) ;
#59262 = CARTESIAN_POINT ( 'NONE',  ( -10.61999428370000054, 1462.990852395989805, 206.0510139005290000 ) ) ;
#59263 = CARTESIAN_POINT ( 'NONE',  ( -109.2936197549999946, 1383.544291963839896, 297.2875327422589748 ) ) ;
#59264 = CARTESIAN_POINT ( 'NONE',  ( 0.1713342119950009845, 1442.917349970689884, 202.9113549887590011 ) ) ;
#59265 = VECTOR ( 'NONE', #4695, 1000.000000000000000 ) ;
#59266 = DIRECTION ( 'NONE',  ( 0.000000000000000000, 1.000000000000000000, 0.000000000000000000 ) ) ;
#59267 = CARTESIAN_POINT ( 'NONE',  ( -11.63919359464260062, 1508.551704408389924, 217.4554316303789960 ) ) ;
#59268 = CARTESIAN_POINT ( 'NONE',  ( 4.099770245750000264, 1409.056227519030017, 187.5794659243979936 ) ) ;
#59269 = CARTESIAN_POINT ( 'NONE',  ( 1.604608372890350187, 1486.554689331300096, 197.3067947285690309 ) ) ;
#59270 = CARTESIAN_POINT ( 'NONE',  ( 4.699465565660820410, 1432.335544942790193, 201.1496391276479869 ) ) ;
#59271 = CARTESIAN_POINT ( 'NONE',  ( -2.704712804207050070, 1440.782885268830114, 168.7248546753820051 ) ) ;
#59272 = EDGE_CURVE ( 'NONE', #104782, #90951, #57894, .T. ) ;
#59273 = CARTESIAN_POINT ( 'NONE',  ( -21.74667324010000158, 1452.010995276330050, 142.8652655935979965 ) ) ;
#59274 = CARTESIAN_POINT ( 'NONE',  ( 0.3090117147110000295, 1467.131542599430077, 235.6271451561979973 ) ) ;
#59275 = VERTEX_POINT ( 'NONE', #36415 ) ;
#59276 = CARTESIAN_POINT ( 'NONE',  ( 10.75504506440890040, 1478.312245267059780, 229.8871532797240036 ) ) ;
#59277 = CARTESIAN_POINT ( 'NONE',  ( 2.632631803615880450, 1417.642869435429930, 234.7516633181379859 ) ) ;
#59278 = DIRECTION ( 'NONE',  ( 0.000000000000000000, 1.000000000000000000, -1.836970198721029688E-16 ) ) ;
#59279 = CARTESIAN_POINT ( 'NONE',  ( -21.12212911287051043, 1511.187213306747708, 182.4210318429776976 ) ) ;
#59280 = CARTESIAN_POINT ( 'NONE',  ( 17.29256643469999943, 1488.208383692229972, 189.1286988683980042 ) ) ;
#59281 = AXIS2_PLACEMENT_3D ( 'NONE', #90704, #100746, #22374 ) ;
#59282 = CARTESIAN_POINT ( 'NONE',  ( -1.943334382303870373E-12, 1470.170431109869924, 254.4737176916079875 ) ) ;
#59283 = DIRECTION ( 'NONE',  ( -1.224646799147350002E-16, 1.836970198721029688E-16, 1.000000000000000000 ) ) ;
#59284 = CARTESIAN_POINT ( 'NONE',  ( -1.163296394699999903, 1415.996778985530000, 227.8825576561980313 ) ) ;
#59285 = CARTESIAN_POINT ( 'NONE',  ( -23.67893809570000130, 1435.763822560270000, 211.7787295027080177 ) ) ;
#59286 = CARTESIAN_POINT ( 'NONE',  ( -3.046861489599999917, 1475.471994209789955, 198.8673666174990160 ) ) ;
#59287 = CARTESIAN_POINT ( 'NONE',  ( -107.0296446230000100, 1389.965289768990033, 308.9939284075589399 ) ) ;
#59288 = CIRCLE ( 'NONE', #19927, 2.000000000000003553 ) ;
#59289 = CARTESIAN_POINT ( 'NONE',  ( -0.2553961933194452971, 1485.936309581204569, 181.8381039734772742 ) ) ;
#59290 = CARTESIAN_POINT ( 'NONE',  ( -2.380813228428187767, 1360.502616939895915, 210.6218459616991936 ) ) ;
#59291 = CARTESIAN_POINT ( 'NONE',  ( -45.56241648270140132, 1438.493849736420088, 266.1915599396410244 ) ) ;
#59292 = CARTESIAN_POINT ( 'NONE',  ( 2.566509579899709959, 1428.984001205079949, 217.0000999674069817 ) ) ;
#59293 = CARTESIAN_POINT ( 'NONE',  ( -8.412371419999999489, 1424.256181506120129, 208.0131652990489783 ) ) ;
#59294 = ORIENTED_EDGE ( 'NONE', *, *, #19121, .T. ) ;
#59295 = CARTESIAN_POINT ( 'NONE',  ( -2.873919040654999701, 1516.940252185109784, 209.1351185066319829 ) ) ;
#59296 = CARTESIAN_POINT ( 'NONE',  ( -9.094129269030000629, 1384.954944735329946, 199.9429221374590213 ) ) ;
#59298 = EDGE_CURVE ( 'NONE', #110603, #68835, #8276, .T. ) ;
#59297 = EDGE_CURVE ( 'NONE', #51052, #10764, #99016, .T. ) ;
#59299 = CARTESIAN_POINT ( 'NONE',  ( -6.707757304198008086, 1470.964955385042231, 216.6951309197101239 ) ) ;
#59300 = CARTESIAN_POINT ( 'NONE',  ( 7.244778264954490510, 1426.495820955630052, 212.9096779512760236 ) ) ;
#59301 = CIRCLE ( 'NONE', #93237, 1.000000000028000047 ) ;
#59302 = CARTESIAN_POINT ( 'NONE',  ( -26.60536840204009934, 1451.234345923490082, 136.3028184666089828 ) ) ;
#59303 = ORIENTED_EDGE ( 'NONE', *, *, #91812, .T. ) ;
#59304 = CARTESIAN_POINT ( 'NONE',  ( 29.87497007650000214, 1440.913060390719920, 238.0574376938980095 ) ) ;
#59306 = CARTESIAN_POINT ( 'NONE',  ( -15.13723823385460143, 1513.497693043359959, 223.5461030115109793 ) ) ;
#59305 = CARTESIAN_POINT ( 'NONE',  ( -11.25957898075910002, 1491.777264728850014, 206.9688726115570034 ) ) ;
#59307 = ADVANCED_FACE ( 'NONE', ( #38073 ), #49234, .T. ) ;
#59308 = CARTESIAN_POINT ( 'NONE',  ( -2.309563177363039621, 1419.513509509170035, 186.0127616851229959 ) ) ;
#59309 = CARTESIAN_POINT ( 'NONE',  ( 15.81201445386249915, 1506.433683730510211, 224.3933755863170063 ) ) ;
#59310 = CARTESIAN_POINT ( 'NONE',  ( -4.438186827019999854E-16, 1395.913060387330006, 217.1218459616979999 ) ) ;
#59311 = LINE ( 'NONE', #92876, #24855 ) ;
#59312 = CARTESIAN_POINT ( 'NONE',  ( -18.95816156469999925, 1416.822692809329965, 207.7797354902180018 ) ) ;
#59313 = ORIENTED_EDGE ( 'NONE', *, *, #77539, .T. ) ;
#59314 = CARTESIAN_POINT ( 'NONE',  ( -4.184099373191500604, 1410.387155536230011, 269.6167533213169349 ) ) ;
#59315 = CARTESIAN_POINT ( 'NONE',  ( 12.29573117529999848, 1419.871834229630167, 229.5356804718979902 ) ) ;
#59316 = CARTESIAN_POINT ( 'NONE',  ( 8.316853310700460966, 1435.402407723380065, 206.5373084086480162 ) ) ;
#59317 = ORIENTED_EDGE ( 'NONE', *, *, #16496, .F. ) ;
#59318 = ORIENTED_EDGE ( 'NONE', *, *, #54357, .T. ) ;
#59319 = CARTESIAN_POINT ( 'NONE',  ( -23.67543694167489932, 1410.417538101999980, 210.0557992214939986 ) ) ;
#59320 = CARTESIAN_POINT ( 'NONE',  ( -0.9956478785452340663, 1409.114994574759976, 186.0079330497359820 ) ) ;
#59321 = DIRECTION ( 'NONE',  ( -0.7071067811865475727, 0.000000000000000000, 0.7071067811865475727 ) ) ;
#59322 = CARTESIAN_POINT ( 'NONE',  ( -2.244413413239999766, 1428.081157166129969, 101.8807690336980016 ) ) ;
#59323 = AXIS2_PLACEMENT_3D ( 'NONE', #6798, #21925, #30903 ) ;
#59324 = CARTESIAN_POINT ( 'NONE',  ( -20.64441152918609745, 1495.412616601870241, 192.5697118770649752 ) ) ;
#59325 = CARTESIAN_POINT ( 'NONE',  ( -22.54740219580000016, 1410.868171134329941, 211.9285665470380025 ) ) ;
#59326 = CARTESIAN_POINT ( 'NONE',  ( 32.78481868098219820, 1465.118709357260059, 269.1179671746619988 ) ) ;
#59327 = CARTESIAN_POINT ( 'NONE',  ( -1.378966749891139987, 1424.159261042490016, 228.3819189927079947 ) ) ;
#59328 = B_SPLINE_CURVE_WITH_KNOTS ( 'NONE', 3,
 ( #9508, #93501, #61057, #77285, #16773, #17885 ),
 .UNSPECIFIED., .F., .F.,
 ( 4, 2, 4 ),
 ( 1.348463003743570024E-05, 0.01516384436121859941, 0.03032162875772679775 ),
 .UNSPECIFIED. ) ;
#59329 = CARTESIAN_POINT ( 'NONE',  ( -6.561686461364999445, 1517.069378699710114, 205.6695567495270041 ) ) ;
#59330 = ORIENTED_EDGE ( 'NONE', *, *, #61302, .F. ) ;
#59331 = CARTESIAN_POINT ( 'NONE',  ( 18.69185951995306993, 1458.324745879651800, 227.3668699999246883 ) ) ;
#59333 = B_SPLINE_CURVE_WITH_KNOTS ( 'NONE', 3,
 ( #62063, #97285, #11093, #20557, #80500, #37946, #72127, #29528, #12734, #45260 ),
 .UNSPECIFIED., .F., .F.,
 ( 4, 2, 2, 2, 4 ),
 ( 0.000000000000000000, 0.2500000000000000000, 0.5000000000000000000, 0.7500000000000000000, 1.000000000000000000 ),
 .UNSPECIFIED. ) ;
#59332 = CARTESIAN_POINT ( 'NONE',  ( 14.86025862469639947, 1514.013728164689837, 194.2524291478609939 ) ) ;
#59334 = DIRECTION ( 'NONE',  ( 0.0001373912891020987869, 0.01108474315567990406, -0.9999385529085306201 ) ) ;
#59335 = ORIENTED_EDGE ( 'NONE', *, *, #28798, .F. ) ;
#59336 = CARTESIAN_POINT ( 'NONE',  ( -10.45120302590630068, 1480.043455506409828, 210.3065010141500011 ) ) ;
#59337 = CARTESIAN_POINT ( 'NONE',  ( 4.081077166763362740, 1433.956112075854662, 201.6265345710585279 ) ) ;
#59338 = CARTESIAN_POINT ( 'NONE',  ( -3.466266129564929965, 1508.551704408389924, 213.9108720011500111 ) ) ;
#59339 = CARTESIAN_POINT ( 'NONE',  ( -3.078458355400000013, 1386.601749568020068, 199.6726121090490267 ) ) ;
#59340 = CARTESIAN_POINT ( 'NONE',  ( 7.399151400400000078, 1422.280175886809957, 195.6034776983989900 ) ) ;
#59341 = CARTESIAN_POINT ( 'NONE',  ( 22.40106396050000015, 1409.695322778229865, 210.5405262121579995 ) ) ;
#59342 = B_SPLINE_CURVE_WITH_KNOTS ( 'NONE', 3,
 ( #68746, #93904, #17171, #26142, #36226, #103403, #70411, #87180, #17728, #60334, #51363, #69296, #94450, #104530, #110719, #51930 ),
 .UNSPECIFIED., .F., .F.,
 ( 4, 3, 3, 3, 3, 4 ),
 ( -7.627871908653229838, -7.157619290633450149, -6.147716997384709892, -5.141165131806689992, -4.136155949588020242, -3.133321433589999927 ),
 .UNSPECIFIED. ) ;
#59343 = CARTESIAN_POINT ( 'NONE',  ( -4.366144226260000316, 1495.418471743290183, 198.0199394070990024 ) ) ;
#59344 = CARTESIAN_POINT ( 'NONE',  ( 2.053713886625649909, 1408.984777656559800, 186.9425993992589952 ) ) ;
#59346 = CARTESIAN_POINT ( 'NONE',  ( 1.702416261868870073, 1493.957958506549858, 220.1113518634800243 ) ) ;
#59345 = CARTESIAN_POINT ( 'NONE',  ( 1.461041045310000008, 1417.190561156129888, 233.6733459660979975 ) ) ;
#59347 = CARTESIAN_POINT ( 'NONE',  ( -16.51112239071575516, 1525.159177407155767, 181.0518290279077576 ) ) ;
#59348 = AXIS2_PLACEMENT_3D ( 'NONE', #24515, #15557, #103868 ) ;
#59349 = CARTESIAN_POINT ( 'NONE',  ( -11.35047539859999866, 1380.036999151499913, 215.0867406839389844 ) ) ;
#59350 = CARTESIAN_POINT ( 'NONE',  ( 11.84704892624298012, 1420.366920634892949, 231.7806654029725735 ) ) ;
#59351 = ORIENTED_EDGE ( 'NONE', *, *, #65082, .F. ) ;
#59352 = CARTESIAN_POINT ( 'NONE',  ( 13.01305160761890001, 1416.520646088589956, 221.6242373452080017 ) ) ;
#59353 = CARTESIAN_POINT ( 'NONE',  ( 0.000000000000000000, 1405.413060387330006, 209.1218459616979999 ) ) ;
#59354 = CARTESIAN_POINT ( 'NONE',  ( -108.7828337545389985, 1384.925007157400159, 311.2643083153219550 ) ) ;
#59355 = CARTESIAN_POINT ( 'NONE',  ( -13.55796854679999974, 1390.272843676579896, 206.9364406775789860 ) ) ;
#59356 = CARTESIAN_POINT ( 'NONE',  ( 8.742631905043140250, 1426.622762530149885, 210.8844128420550135 ) ) ;
#59357 = CARTESIAN_POINT ( 'NONE',  ( -35.61939005354069820, 1450.149788447230094, 136.2352736447359973 ) ) ;
#59358 = CARTESIAN_POINT ( 'NONE',  ( 13.40566205669149902, 1429.098591087019940, 222.0107402452829888 ) ) ;
#59359 = TOROIDAL_SURFACE ( 'NONE', #82606, 1.000000000000000000, 1.000000000000000000 ) ;
#59360 = CARTESIAN_POINT ( 'NONE',  ( 1.021405182659999929E-14, 1469.463552837929910, 265.6112251771979800 ) ) ;
#59361 = CARTESIAN_POINT ( 'NONE',  ( -21.03615331023111068, 1508.023275259974525, 192.1677045215957662 ) ) ;
#59362 = CARTESIAN_POINT ( 'NONE',  ( 11.11327778789999954, 1433.557389433600065, 151.6749141554979872 ) ) ;
#59363 = CARTESIAN_POINT ( 'NONE',  ( 2.886579864029999753E-15, 1458.952956299430070, 234.3916895801979763 ) ) ;
#59364 = CARTESIAN_POINT ( 'NONE',  ( 11.87146819884729965, 1414.971390223329990, 197.3742744802259779 ) ) ;
#59365 = CARTESIAN_POINT ( 'NONE',  ( -16.78271819211574112, 1420.478864045909404, 203.1931770898623597 ) ) ;
#59366 = CARTESIAN_POINT ( 'NONE',  ( -1.842962215208689303, 1515.492058412107781, 213.2603893544997504 ) ) ;
#59367 = CARTESIAN_POINT ( 'NONE',  ( 8.885863169899998582, 1465.108758012390126, 213.4968473838789862 ) ) ;
#59368 = CARTESIAN_POINT ( 'NONE',  ( -19.45240832520000041, 1485.997265531630092, 190.0281968953979970 ) ) ;
#59369 = LINE ( 'NONE', #109748, #50315 ) ;
#59370 = CARTESIAN_POINT ( 'NONE',  ( -7.546382087207799572, 1509.216843681829914, 238.8694033275340018 ) ) ;
#59371 = AXIS2_PLACEMENT_3D ( 'NONE', #96089, #10433, #77642 ) ;
#59372 = CARTESIAN_POINT ( 'NONE',  ( 21.12097961079999919, 1430.346877874630081, 219.8772875276980017 ) ) ;
#59373 = CARTESIAN_POINT ( 'NONE',  ( -0.7263599678500212153, 1477.494758098099737, 198.7454087897867225 ) ) ;
#59374 = CARTESIAN_POINT ( 'NONE',  ( -3.469833849039999683E-16, 1426.566393376330097, 144.1938086916980239 ) ) ;
#59375 = CARTESIAN_POINT ( 'NONE',  ( 9.146237114798470458, 1449.998848199699978, 208.1168068718100130 ) ) ;
#59376 = CARTESIAN_POINT ( 'NONE',  ( -2.372478608334043670, 1522.644714754858114, 174.8996806668799024 ) ) ;
#59377 = CARTESIAN_POINT ( 'NONE',  ( -13.05162046615980032, 1467.538720443550119, 191.8992815197879906 ) ) ;
#59378 = CARTESIAN_POINT ( 'NONE',  ( -2.479246885834999858, 1516.983612918759945, 213.1658362778269691 ) ) ;
#59380 = AXIS2_PLACEMENT_3D ( 'NONE', #80768, #29802, #80216 ) ;
#59379 = CARTESIAN_POINT ( 'NONE',  ( -12.63495890147190082, 1422.290833888599991, 205.4229267067590285 ) ) ;
#59381 = CARTESIAN_POINT ( 'NONE',  ( 0.1698047298984949882, 1480.444372444690089, 182.0753023306870091 ) ) ;
#59383 = ORIENTED_EDGE ( 'NONE', *, *, #72276, .T. ) ;
#59382 = CARTESIAN_POINT ( 'NONE',  ( -2.881142919476630038, 1408.476254411279797, 222.6699509515860029 ) ) ;
#59384 = CARTESIAN_POINT ( 'NONE',  ( 9.722207004026980570, 1428.114070666289763, 212.2005352792010058 ) ) ;
#59385 = CARTESIAN_POINT ( 'NONE',  ( 22.03465957474570658, 1501.977400791986611, 235.4136513321629991 ) ) ;
#59386 = CARTESIAN_POINT ( 'NONE',  ( 12.40400603319999817, 1434.420125459849942, 149.7889667278979857 ) ) ;
#59387 = CARTESIAN_POINT ( 'NONE',  ( -41.53765979145569531, 1445.128430570340015, 134.0999999984609872 ) ) ;
#59388 = DIRECTION ( 'NONE',  ( -0.7414773880254650340, 0.000000000000000000, 0.6709778558543747495 ) ) ;
#59389 = ORIENTED_EDGE ( 'NONE', *, *, #83893, .T. ) ;
#59390 = CARTESIAN_POINT ( 'NONE',  ( -5.930127944598649670, 1391.913057044489960, 203.1301316852850221 ) ) ;
#59391 = CARTESIAN_POINT ( 'NONE',  ( 9.186645411349999790, 1479.540829827790049, 203.8650577567789810 ) ) ;
#59392 = CARTESIAN_POINT ( 'NONE',  ( -15.32781675520000064, 1414.971279908829956, 216.4146992301180035 ) ) ;
#59393 = CARTESIAN_POINT ( 'NONE',  ( -16.73628186595857059, 1526.382868172863937, 184.0591879540917546 ) ) ;
#59394 = CARTESIAN_POINT ( 'NONE',  ( -5.543844742518439617, 1434.311283813799946, 216.1702177519260033 ) ) ;
#59395 = CARTESIAN_POINT ( 'NONE',  ( -108.5877928923653570, 1381.490933517691019, 310.5017133838013592 ) ) ;
#59396 = CARTESIAN_POINT ( 'NONE',  ( -15.22200272170000090, 1417.314676559359896, 211.7966809115490037 ) ) ;
#59397 = DIRECTION ( 'NONE',  ( -0.000000000000000000, -1.000000000000000000, -0.000000000000000000 ) ) ;
#59398 = CARTESIAN_POINT ( 'NONE',  ( -11.73107767829999837, 1391.121393030069839, 205.1223722441990276 ) ) ;
#59399 = CARTESIAN_POINT ( 'NONE',  ( -79.01945392300798687, 1385.153591211519824, 281.7696847378040275 ) ) ;
#59400 = CARTESIAN_POINT ( 'NONE',  ( -17.61183580542321536, 1523.982201850120191, 237.6741279912556593 ) ) ;
#59401 = CARTESIAN_POINT ( 'NONE',  ( 10.40611076564779935, 1423.173680896260066, 208.2592473985839945 ) ) ;
#59402 = ORIENTED_EDGE ( 'NONE', *, *, #9707, .F. ) ;
#59403 = CARTESIAN_POINT ( 'NONE',  ( -28.53738135360000072, 1451.916516915729972, 134.8736009463979997 ) ) ;
#59404 = CARTESIAN_POINT ( 'NONE',  ( 13.51812398686129590, 1443.501467202829645, 169.4008117781763190 ) ) ;
#59405 = EDGE_CURVE ( 'NONE', #12190, #22497, #2522, .T. ) ;
#59407 = ORIENTED_EDGE ( 'NONE', *, *, #75470, .T. ) ;
#59406 = DIRECTION ( 'NONE',  ( 0.5032920991128559951, -0.8641163480519131745, 0.000000000000000000 ) ) ;
#59408 = CARTESIAN_POINT ( 'NONE',  ( 5.346297422500000174, 1473.360741859489963, 218.2967445439789742 ) ) ;
#59409 = CARTESIAN_POINT ( 'NONE',  ( 5.983287317399999417, 1451.235340618889950, 210.0682002075799915 ) ) ;
#59410 = CARTESIAN_POINT ( 'NONE',  ( -8.014696367955107092, 1363.426607574581794, 207.6218459616988241 ) ) ;
#59411 = CARTESIAN_POINT ( 'NONE',  ( -10.49113256600000099, 1492.581845576989963, 203.3991013598590030 ) ) ;
#59412 = EDGE_CURVE ( 'NONE', #101169, #575, #106942, .T. ) ;
#59413 = DIRECTION ( 'NONE',  ( -0.2054769195713296304, 0.000000000000000000, 0.9786619618251631847 ) ) ;
#59414 = DIRECTION ( 'NONE',  ( -1.000000000000000000, 0.000000000000000000, 0.000000000000000000 ) ) ;
#59415 = CARTESIAN_POINT ( 'NONE',  ( 16.00594386000976499, 1431.827458374873913, 218.6954846823096830 ) ) ;
#59416 = CARTESIAN_POINT ( 'NONE',  ( 1.467367638679999864, 1417.074472501330092, 233.2101326662979659 ) ) ;
#59417 = CARTESIAN_POINT ( 'NONE',  ( -3.052975934615000053, 1516.551704408390151, 201.1191225673069880 ) ) ;
#59418 = CARTESIAN_POINT ( 'NONE',  ( -20.58241815119903961, 1507.840888067528340, 228.3121511827991696 ) ) ;
#59419 = CARTESIAN_POINT ( 'NONE',  ( 4.255689356150000435, 1519.913060387329779, 231.5674970370980077 ) ) ;
#59420 = CARTESIAN_POINT ( 'NONE',  ( -0.5336398385289990998, 1457.451400674990055, 199.5863132090090062 ) ) ;
#59421 = CARTESIAN_POINT ( 'NONE',  ( -2.493073867885000183, 1516.826109302209943, 206.2575198447970024 ) ) ;
#59422 = CARTESIAN_POINT ( 'NONE',  ( 4.220206612560000181, 1446.210882134419990, 168.9980572354979813 ) ) ;
#59423 = CARTESIAN_POINT ( 'NONE',  ( -2.500000000000000000, 1437.234369398040144, 157.6522023233980008 ) ) ;
#59424 = CARTESIAN_POINT ( 'NONE',  ( -3.467940627379999974, 1495.562067971789929, 197.2905559059990139 ) ) ;
#59426 = VERTEX_POINT ( 'NONE', #49246 ) ;
#59425 = CARTESIAN_POINT ( 'NONE',  ( -68.58629774669110191, 1379.747539349169983, 280.1877734521850130 ) ) ;
#59427 = CARTESIAN_POINT ( 'NONE',  ( -6.232532191338900240, 1398.098440470949981, 197.7132727547819968 ) ) ;
#59428 = EDGE_LOOP ( 'NONE', ( #38282, #54085 ) ) ;
#59429 = CARTESIAN_POINT ( 'NONE',  ( -16.66011982862587715, 1513.969110094344160, 223.0773383146762114 ) ) ;
#59430 = CARTESIAN_POINT ( 'NONE',  ( -24.85895335939999740, 1430.362482304829882, 208.4345430527690155 ) ) ;
#59432 = CARTESIAN_POINT ( 'NONE',  ( 16.84651400299079782, 1409.747734344990022, 192.6928343578630063 ) ) ;
#59431 = CARTESIAN_POINT ( 'NONE',  ( -11.15980475191650001, 1426.466872868450082, 102.3027272071919924 ) ) ;
#59433 = CARTESIAN_POINT ( 'NONE',  ( 6.950833530105000158, 1517.156142772249950, 211.6057959108269984 ) ) ;
#59434 = ADVANCED_FACE ( 'NONE', ( #23464 ), #65306, .F. ) ;
#59435 = CARTESIAN_POINT ( 'NONE',  ( 21.09276969954263947, 1509.766718187257993, 187.7199361994491937 ) ) ;
#59436 = CIRCLE ( 'NONE', #11157, 1.999999999999999556 ) ;
#59437 = CARTESIAN_POINT ( 'NONE',  ( 22.04658257820665668, 1524.075000532257263, 233.7649905024729549 ) ) ;
#59438 = PRESENTATION_STYLE_ASSIGNMENT (( #42069 ) ) ;
#59439 = CARTESIAN_POINT ( 'NONE',  ( 15.16658111565280009, 1509.443839351920133, 234.3011174550109956 ) ) ;
#59440 = CARTESIAN_POINT ( 'NONE',  ( 12.68801083313210043, 1500.413651417279880, 208.6561539661539939 ) ) ;
#59441 = FACE_OUTER_BOUND ( 'NONE', #82546, .T. ) ;
#59442 = CARTESIAN_POINT ( 'NONE',  ( -38.82359025196139868, 1439.487870305959859, 136.6807876477819832 ) ) ;
#59443 = VERTEX_POINT ( 'NONE', #58191 ) ;
#59444 = CARTESIAN_POINT ( 'NONE',  ( 9.441477048479999468, 1396.242764029729869, 201.4775236043080042 ) ) ;
#59445 = LINE ( 'NONE', #8450, #79466 ) ;
#59446 = CARTESIAN_POINT ( 'NONE',  ( -18.37698674530000176, 1457.555359684630048, 228.2935531249980272 ) ) ;
#59447 = ORIENTED_EDGE ( 'NONE', *, *, #22789, .T. ) ;
#59448 = ORIENTED_EDGE ( 'NONE', *, *, #98682, .F. ) ;
#59449 = CARTESIAN_POINT ( 'NONE',  ( -29.43467078477432253, 1509.947524417930026, 211.2629717639432840 ) ) ;
#59450 = CARTESIAN_POINT ( 'NONE',  ( 10.21346743305219995, 1453.430616332530008, 212.0093735090799782 ) ) ;
#59451 = CARTESIAN_POINT ( 'NONE',  ( -14.23346546853939998, 1380.249845882129875, 210.5096821227170096 ) ) ;
#59452 = CARTESIAN_POINT ( 'NONE',  ( -14.17032501240000109, 1507.703614819789891, 209.3618925486269973 ) ) ;
#59454 = CARTESIAN_POINT ( 'NONE',  ( 4.038582019099999698, 1515.598601288489817, 209.1218459617159908 ) ) ;
#59453 = AXIS2_PLACEMENT_3D ( 'NONE', #16590, #68172, #60872 ) ;
#59455 = CARTESIAN_POINT ( 'NONE',  ( -6.508912761185129625, 1454.032954269330048, 202.3712805252700093 ) ) ;
#59456 = CARTESIAN_POINT ( 'NONE',  ( -14.28760104070000025, 1461.186940285030005, 229.6152737784979934 ) ) ;
#59457 = CARTESIAN_POINT ( 'NONE',  ( 21.97938480441199971, 1506.433683733499947, 208.7396655020440051 ) ) ;
#59458 = CARTESIAN_POINT ( 'NONE',  ( 9.409271459137828586, 1451.760564006479854, 209.6856075121530125 ) ) ;
#59459 = CARTESIAN_POINT ( 'NONE',  ( 17.22592475669953416, 1443.501467202839649, 162.9227486557969655 ) ) ;
#59460 = CARTESIAN_POINT ( 'NONE',  ( -97.29693749981930750, 1384.865312593040244, 295.6567534606039658 ) ) ;
#59461 = ORIENTED_EDGE ( 'NONE', *, *, #61791, .T. ) ;
#59462 = CARTESIAN_POINT ( 'NONE',  ( 2.483949940595000516, 1517.156142772249950, 202.1710124019969896 ) ) ;
#59463 = CARTESIAN_POINT ( 'NONE',  ( 3.460866170685000132, 1517.020847257979995, 209.8575449048190080 ) ) ;
#59464 = VERTEX_POINT ( 'NONE', #85567 ) ;
#59465 = CARTESIAN_POINT ( 'NONE',  ( 11.06583617892839833, 1414.913527292460003, 222.2283161299670269 ) ) ;
#59466 = CARTESIAN_POINT ( 'NONE',  ( 4.726342638545708574, 1511.395336166597417, 217.5537869467808605 ) ) ;
#59467 = EDGE_LOOP ( 'NONE', ( #108311, #51598, #5438 ) ) ;
#59468 = CARTESIAN_POINT ( 'NONE',  ( -14.15450645269999974, 1415.628674276829770, 221.0805609275980146 ) ) ;
#59469 = CARTESIAN_POINT ( 'NONE',  ( -11.45640830748399885, 1432.340941395319987, 151.2730090707190129 ) ) ;
#59470 = CARTESIAN_POINT ( 'NONE',  ( -17.33881979142094920, 1508.455908737108757, 212.8389046703344434 ) ) ;
#59471 = CARTESIAN_POINT ( 'NONE',  ( -7.130431368400969916, 1489.820748338716157, 217.4188096387678399 ) ) ;
#59472 = CARTESIAN_POINT ( 'NONE',  ( -4.533058655030000494, 1424.018048896529990, 185.2641154658980156 ) ) ;
#59473 = CARTESIAN_POINT ( 'NONE',  ( 14.59277107062129986, 1436.244837967300100, 149.8707660814949918 ) ) ;
#59474 = CARTESIAN_POINT ( 'NONE',  ( -7.941319541319999509, 1469.154588994090091, 217.1846401660390029 ) ) ;
#59475 = CARTESIAN_POINT ( 'NONE',  ( -2.923521517025829741, 1410.394928878200062, 186.6127595807840009 ) ) ;
#59476 = CARTESIAN_POINT ( 'NONE',  ( -57.93277555979999960, 1379.748264674359916, 257.2455319417590545 ) ) ;
#59477 = CARTESIAN_POINT ( 'NONE',  ( -16.28504566760000216, 1496.371285614329963, 224.3646236400980172 ) ) ;
#59479 = CARTESIAN_POINT ( 'NONE',  ( 7.159096167851838999, 1467.721109967099892, 200.5586486524099996 ) ) ;
#59478 = CARTESIAN_POINT ( 'NONE',  ( 17.33021867909999969, 1458.353808689130119, 229.6040141600979894 ) ) ;
#59480 = CARTESIAN_POINT ( 'NONE',  ( -4.989978619240677205, 1423.182856176245650, 184.7654884127948094 ) ) ;
#59481 = CARTESIAN_POINT ( 'NONE',  ( -2.499952938216249976, 1420.029941299070060, 100.9689851914940135 ) ) ;
#59482 = EDGE_LOOP ( 'NONE', ( #61704, #24381, #3145, #27619 ) ) ;
#59483 = CARTESIAN_POINT ( 'NONE',  ( -6.531167973260561865, 1517.051704408389924, 216.7070295963201829 ) ) ;
#59484 = CARTESIAN_POINT ( 'NONE',  ( -21.30905559963850493, 1524.964230758882877, 233.9180796557699864 ) ) ;
#59485 = B_SPLINE_CURVE_WITH_KNOTS ( 'NONE', 3,
 ( #75154, #40424, #101404, #33120, #67308, #85177, #68414, #57806, #15739, #24696, #25808, #49940, #42089, #58343, #84623, #17398, #58892, #84078, #34228, #93025, #7919, #76238 ),
 .UNSPECIFIED., .F., .F.,
 ( 4, 2, 2, 2, 2, 2, 2, 2, 2, 2, 4 ),
 ( 0.000000000000000000, 0.2500000000000107137, 0.3750000000000233147, 0.4375000000000259237, 0.4687500000000261458, 0.5000000000000263123, 0.6250000000000224265, 0.6875000000000186517, 0.7500000000000148770, 0.8750000000000075495, 1.000000000000000000 ),
 .UNSPECIFIED. ) ;
#59486 = FACE_OUTER_BOUND ( 'NONE', #21542, .T. ) ;
#59487 = CARTESIAN_POINT ( 'NONE',  ( -14.40762303440000025, 1415.739699861750069, 214.0597611563689782 ) ) ;
#59489 = VERTEX_POINT ( 'NONE', #102379 ) ;
#59488 = CARTESIAN_POINT ( 'NONE',  ( -11.27716492698469963, 1500.448551123189873, 210.9498347538589940 ) ) ;
#59490 = CARTESIAN_POINT ( 'NONE',  ( 1.336626035159999892, 1434.994518313450044, 189.3609647309980062 ) ) ;
#59491 = FACE_OUTER_BOUND ( 'NONE', #51152, .T. ) ;
#59492 = CARTESIAN_POINT ( 'NONE',  ( -11.50995325589999929, 1427.639127959429970, 149.3376616764980156 ) ) ;
#59493 = CARTESIAN_POINT ( 'NONE',  ( -10.91327520126305117, 1428.362630744280750, 150.6705834258702907 ) ) ;
#59494 = CARTESIAN_POINT ( 'NONE',  ( -5.772970091560000405, 1439.947079492359990, 185.7689619320979943 ) ) ;
#59495 = FACE_OUTER_BOUND ( 'NONE', #78140, .T. ) ;
#59496 = DIRECTION ( 'NONE',  ( -1.836970198721029688E-16, -1.000000000000000000, 0.000000000000000000 ) ) ;
#59498 = CARTESIAN_POINT ( 'NONE',  ( -9.350033435369999424, 1478.007838331189760, 213.9435157906089842 ) ) ;
#59497 = CARTESIAN_POINT ( 'NONE',  ( -24.52682765429999634, 1495.363418884229986, 219.7720737364980153 ) ) ;
#59499 = CARTESIAN_POINT ( 'NONE',  ( -16.78746488157599970, 1460.262648982494056, 228.3352623233340069 ) ) ;
#59500 = ORIENTED_EDGE ( 'NONE', *, *, #27571, .F. ) ;
#59501 = CARTESIAN_POINT ( 'NONE',  ( 5.771797426184999580, 1516.647618671360078, 206.2459958378869942 ) ) ;
#59502 = CARTESIAN_POINT ( 'NONE',  ( 18.39953948240000159, 1408.534890842129926, 267.7101522853979532 ) ) ;
#59503 = DIRECTION ( 'NONE',  ( -1.000000000000000000, 0.000000000000000000, 0.000000000000000000 ) ) ;
#59505 = B_SPLINE_CURVE_WITH_KNOTS ( 'NONE', 5,
 ( #101200, #92819, #16090, #50297, #84425, #7711 ),
 .UNSPECIFIED., .F., .F.,
 ( 6, 6 ),
 ( -2.000000000000000000, 0.000000000000000000 ),
 .UNSPECIFIED. ) ;
#59504 = CARTESIAN_POINT ( 'NONE',  ( 20.03780167889999930, 1430.300308916730046, 195.4616010020980070 ) ) ;
#59506 = CARTESIAN_POINT ( 'NONE',  ( 0.06174575640759859957, 1508.562174490289863, 237.9142381842480063 ) ) ;
#59507 = CARTESIAN_POINT ( 'NONE',  ( -8.363594539798167915, 1387.928394511323859, 218.3056381099177941 ) ) ;
#59508 = DIRECTION ( 'NONE',  ( 0.000000000000000000, 0.000000000000000000, 1.000000000000000000 ) ) ;
#59509 = CARTESIAN_POINT ( 'NONE',  ( 12.32422840039999912, 1461.784851115730135, 233.7517049971980043 ) ) ;
#59510 = CARTESIAN_POINT ( 'NONE',  ( -8.372769162319999126, 1460.069700419990113, 216.1743697456390123 ) ) ;
#59511 = CARTESIAN_POINT ( 'NONE',  ( -13.45215185470000030, 1444.587159410089953, 187.5992218171979857 ) ) ;
#59512 = CARTESIAN_POINT ( 'NONE',  ( -19.47227132649999959, 1453.313060387329870, 212.8011186786780229 ) ) ;
#59513 = CARTESIAN_POINT ( 'NONE',  ( -16.62627913534196367, 1419.615195795464842, 209.0779031733366082 ) ) ;
#59514 = CARTESIAN_POINT ( 'NONE',  ( -3.607509927959999807, 1496.493923052690207, 219.8931759207989955 ) ) ;
#59515 = ORIENTED_EDGE ( 'NONE', *, *, #102671, .F. ) ;
#59516 = CARTESIAN_POINT ( 'NONE',  ( 1.454477355351579959, 1501.339712585870075, 181.3651619459799917 ) ) ;
#59517 = CARTESIAN_POINT ( 'NONE',  ( -10.85260544259019966, 1409.292041720379984, 198.8351549789040007 ) ) ;
#59518 = CARTESIAN_POINT ( 'NONE',  ( 10.56678653000900070, 1481.373476838040006, 208.8185995517700064 ) ) ;
#59519 = DIRECTION ( 'NONE',  ( -1.755985294532469921E-16, 1.000000000000000000, -1.338183447452831989E-16 ) ) ;
#59520 = CARTESIAN_POINT ( 'NONE',  ( -18.35025482799999708, 1473.149480673029984, 267.0969222196980013 ) ) ;
#59521 = CARTESIAN_POINT ( 'NONE',  ( -3.448830483803564828, 1512.187213306747481, 175.1594891075192209 ) ) ;
#59522 = CARTESIAN_POINT ( 'NONE',  ( -20.99310762600000047, 1509.712614273529880, 187.9175820947980071 ) ) ;
#59523 = CARTESIAN_POINT ( 'NONE',  ( -24.08371411292216280, 1444.410970683369897, 211.9273017543515039 ) ) ;
#59524 = CARTESIAN_POINT ( 'NONE',  ( -60.96793211269689294, 1384.692043816230125, 282.5782060957649833 ) ) ;
#59525 = CARTESIAN_POINT ( 'NONE',  ( -18.51341249058109995, 1384.948111255019967, 201.2951208967390073 ) ) ;
#59526 = CARTESIAN_POINT ( 'NONE',  ( -3.663735981259999979E-15, 1440.444625599219989, 155.6821044880979912 ) ) ;
#59527 = CARTESIAN_POINT ( 'NONE',  ( -107.1138176589999915, 1379.788324461719867, 299.4659512524589786 ) ) ;
#59528 = CARTESIAN_POINT ( 'NONE',  ( -15.64577902933677400, 1415.699214057148765, 209.5376509458647831 ) ) ;
#59529 = CARTESIAN_POINT ( 'NONE',  ( 1.842963721827329815, 1515.551704300040001, 212.9514659606769840 ) ) ;
#59530 = CARTESIAN_POINT ( 'NONE',  ( -23.04389186530000089, 1409.882248337629790, 206.7352832536480207 ) ) ;
#59531 = DIRECTION ( 'NONE',  ( 0.000000000000000000, 1.000000000000000000, 0.000000000000000000 ) ) ;
#59532 = CARTESIAN_POINT ( 'NONE',  ( 4.194095649580000362, 1484.606106053989834, 219.7768138602989723 ) ) ;
#59533 = CARTESIAN_POINT ( 'NONE',  ( 10.67085484400129936, 1479.345408069779978, 206.7791535906509921 ) ) ;
#59534 = DIRECTION ( 'NONE',  ( -0.6736849260863839728, 0.000000000000000000, 0.7390186874254150995 ) ) ;
#59535 = CARTESIAN_POINT ( 'NONE',  ( -19.86607082145389924, 1443.193049015349970, 213.0732219199160227 ) ) ;
#59536 = CARTESIAN_POINT ( 'NONE',  ( 17.22627300067414069, 1525.856064936170469, 181.7773026866640862 ) ) ;
#59537 = CARTESIAN_POINT ( 'NONE',  ( -21.59687425035849984, 1507.523446669369832, 209.4572656896989997 ) ) ;
#59539 = CARTESIAN_POINT ( 'NONE',  ( -8.435900379319999587, 1384.078873582379856, 199.8582732524889991 ) ) ;
#59538 = CARTESIAN_POINT ( 'NONE',  ( -21.20067971809999818, 1409.653404436829760, 211.3910486286680168 ) ) ;
#59540 = CARTESIAN_POINT ( 'NONE',  ( 11.73426358108639889, 1426.697716059430149, 143.9718653054989943 ) ) ;
#59541 = CARTESIAN_POINT ( 'NONE',  ( 2.880836473691240407, 1368.383867273139913, 210.4211859087380105 ) ) ;
#59542 = CARTESIAN_POINT ( 'NONE',  ( -113.4000000000000057, 1305.714868215269917, 304.2218459572590064 ) ) ;
#59543 = B_SPLINE_CURVE_WITH_KNOTS ( 'NONE', 5,
 ( #6180, #24606, #15116, #32497, #14017, #100773, #48207, #66670, #58800 ),
 .UNSPECIFIED., .F., .F.,
 ( 6, 3, 6 ),
 ( 0.000000000000000000, 0.5050532947624984947, 1.000000000000000000 ),
 .UNSPECIFIED. ) ;
#59544 = CARTESIAN_POINT ( 'NONE',  ( 4.144219985687159991, 1446.806893490560014, 199.8398090959030071 ) ) ;
#59545 = CARTESIAN_POINT ( 'NONE',  ( -17.22174736099490033, 1507.619498584509984, 224.3333391233730083 ) ) ;
#59546 = CARTESIAN_POINT ( 'NONE',  ( -7.331812124104999384, 1516.906641539930206, 202.5676945058570197 ) ) ;
#59547 = CARTESIAN_POINT ( 'NONE',  ( -11.72661338454730640, 1398.260517928511490, 214.9127125651629058 ) ) ;
#59548 = DIRECTION ( 'NONE',  ( 2.182550389754619197E-05, -9.529833270879996287E-07, -0.9999999997613695513 ) ) ;
#59549 = FACE_BOUND ( 'NONE', #107901, .T. ) ;
#59550 = CARTESIAN_POINT ( 'NONE',  ( 1.441485945039999939, 1507.073353643630071, 236.7786021845980144 ) ) ;
#59551 = CARTESIAN_POINT ( 'NONE',  ( 2.621457251729789384, 1519.551704408389924, 190.1820379210428200 ) ) ;
#59553 = ORIENTED_EDGE ( 'NONE', *, *, #73495, .T. ) ;
#59552 = CARTESIAN_POINT ( 'NONE',  ( -56.94149478592599678, 1379.719693845439906, 259.4788933646619853 ) ) ;
#59554 = EDGE_LOOP ( 'NONE', ( #14289, #80497, #4429, #17096 ) ) ;
#59555 = CARTESIAN_POINT ( 'NONE',  ( 11.55278678904199907, 1434.349239717640103, 151.3337279177310108 ) ) ;
#59556 = CARTESIAN_POINT ( 'NONE',  ( -13.31309558959999961, 1398.000656151930116, 207.3565362264480143 ) ) ;
#59557 = EDGE_LOOP ( 'NONE', ( #88210, #75887, #67236, #88075 ) ) ;
#59558 = CARTESIAN_POINT ( 'NONE',  ( -19.18813880309999931, 1465.797355387890093, 204.3301597990889888 ) ) ;
#59559 = CARTESIAN_POINT ( 'NONE',  ( -109.1310718750000177, 1384.930040066290076, 311.2646600702590263 ) ) ;
#59560 = CARTESIAN_POINT ( 'NONE',  ( -110.7672523143304488, 1306.913060387289988, 305.6601225730707370 ) ) ;
#59562 = CARTESIAN_POINT ( 'NONE',  ( -13.89790203009249936, 1508.842249044219898, 183.8389499564130176 ) ) ;
#59561 = CARTESIAN_POINT ( 'NONE',  ( -0.8695030706469989434, 1444.523560491489889, 199.0910625714990090 ) ) ;
#59563 = CARTESIAN_POINT ( 'NONE',  ( 2.854897837073400169, 1498.106740913580097, 235.5480816206879808 ) ) ;
#59564 =( BOUNDED_CURVE ( )  B_SPLINE_CURVE ( 3, ( #59923, #52067, #75618, #94042 ),
 .UNSPECIFIED., .F., .T. ) 
 B_SPLINE_CURVE_WITH_KNOTS ( ( 4, 4 ),
 ( 4.177898707858459737, 5.246900984146320113 ),
 .UNSPECIFIED. ) 
 CURVE ( )  GEOMETRIC_REPRESENTATION_ITEM ( )  RATIONAL_B_SPLINE_CURVE ( ( 1.000000000000000000, 0.9070152416445715904, 0.9070152416445715904, 1.000000000000000000 ) ) 
 REPRESENTATION_ITEM ( '' )  );
#59565 = CARTESIAN_POINT ( 'NONE',  ( 1.520031180769999990, 1468.707239051229863, 182.7929238198979931 ) ) ;
#59566 = CARTESIAN_POINT ( 'NONE',  ( 1.902221077130000104, 1466.933671594890029, 220.0347825763990102 ) ) ;
#59567 = CARTESIAN_POINT ( 'NONE',  ( 15.48869622149999969, 1409.453937571630149, 226.0647739019979952 ) ) ;
#59568 = SHAPE_REPRESENTATION_RELATIONSHIP ( 'NONE' , 'NONE' ,  #22211, #17149 ) ;
#59569 = CARTESIAN_POINT ( 'NONE',  ( 2.753170620192659790, 1396.009203223909935, 198.4539142632749815 ) ) ;
#59570 = CARTESIAN_POINT ( 'NONE',  ( 33.91369120210129751, 1435.681798817170147, 134.0999999980979851 ) ) ;
#59571 = CARTESIAN_POINT ( 'NONE',  ( 11.86160965589999883, 1432.010073915890189, 150.3887981409980057 ) ) ;
#59572 = CARTESIAN_POINT ( 'NONE',  ( 6.964055579694999665, 1512.881909847360021, 201.9408257871969852 ) ) ;
#59573 = ORIENTED_EDGE ( 'NONE', *, *, #22111, .F. ) ;
#59574 = CARTESIAN_POINT ( 'NONE',  ( 13.68681530539999969, 1435.283985230760209, 149.7729792379979870 ) ) ;
#59575 = VERTEX_POINT ( 'NONE', #16693 ) ;
#59576 = ORIENTED_EDGE ( 'NONE', *, *, #2384, .T. ) ;
#59577 = EDGE_CURVE ( 'NONE', #34885, #81601, #94524, .T. ) ;
#59578 = CARTESIAN_POINT ( 'NONE',  ( 13.51596914371239500, 1443.950082444225018, 169.3503480695792121 ) ) ;
#59579 = CARTESIAN_POINT ( 'NONE',  ( -4.248356950199999815, 1464.543264781329981, 236.4384044122979844 ) ) ;
#59580 = CARTESIAN_POINT ( 'NONE',  ( -13.29011429918680065, 1407.447342471949923, 210.5442722391819927 ) ) ;
#59581 = CARTESIAN_POINT ( 'NONE',  ( -1.710012758625000018, 1517.232977404109988, 216.8491730849570160 ) ) ;
#59582 = CARTESIAN_POINT ( 'NONE',  ( -8.392728068336928970, 1511.399179795969530, 213.7293764352533287 ) ) ;
#59583 = CARTESIAN_POINT ( 'NONE',  ( 11.20822254254120054, 1422.140100304710131, 210.4218750758840031 ) ) ;
#59584 = CARTESIAN_POINT ( 'NONE',  ( 2.500000000000000000, 1448.283969051469967, 164.7257521935120224 ) ) ;
#59585 = CARTESIAN_POINT ( 'NONE',  ( -18.96272001720000233, 1375.296266888390164, 209.6316668867899864 ) ) ;
#59586 = ORIENTED_EDGE ( 'NONE', *, *, #62735, .T. ) ;
#59587 = CARTESIAN_POINT ( 'NONE',  ( -5.787477032644999575, 1517.070197312179971, 206.2521524731670013 ) ) ;
#59588 = ORIENTED_EDGE ( 'NONE', *, *, #60401, .T. ) ;
#59589 = CARTESIAN_POINT ( 'NONE',  ( 22.20198509923669761, 1440.913060387330006, 228.2955218435759832 ) ) ;
#59590 = B_SPLINE_CURVE_WITH_KNOTS ( 'NONE', 3,
 ( #67149, #15044, #101247, #24546, #58734, #92872, #95092, #95642, #77201, #27889, #96198, #44709, #59849, #60966, #503, #27329, #53673, #10535, #35179, #26213, #18910, #71031, #104595, #68812, #26779 ),
 .UNSPECIFIED., .F., .F.,
 ( 4, 2, 1, 1, 1, 2, 2, 2, 2, 2, 1, 1, 2, 2, 4 ),
 ( 0.000000000000000000, 0.1249999999994817756, 0.1874999999992220667, 0.2187499999990761834, 0.2343749999990034638, 0.2421874999989827582, 0.2499999999989620525, 0.3749999999991381894, 0.4999999999993144373, 0.6249999999994905187, 0.6874999999995785593, 0.7187499999996226352, 0.7343749999996446176, 0.7499999999996664890, 1.000000000000000000 ),
 .UNSPECIFIED. ) ;
#59591 = CARTESIAN_POINT ( 'NONE',  ( -19.27289889490000263, 1509.486203086629985, 230.8709054965979988 ) ) ;
#59592 = CARTESIAN_POINT ( 'NONE',  ( -10.55778742260000058, 1409.281746448229796, 190.1804069070979892 ) ) ;
#59593 = CARTESIAN_POINT ( 'NONE',  ( 8.027449271465000535, 1514.605246816809768, 215.6121524902470128 ) ) ;
#59595 = ORIENTED_EDGE ( 'NONE', *, *, #43284, .F. ) ;
#59594 = CARTESIAN_POINT ( 'NONE',  ( -1.457047359353270011, 1414.913057819779851, 226.2719804722950130 ) ) ;
#59596 = CARTESIAN_POINT ( 'NONE',  ( 23.06896861730000126, 1432.937351989309946, 217.3496264744780149 ) ) ;
#59597 = CARTESIAN_POINT ( 'NONE',  ( -17.99551211388680017, 1508.551704408389924, 210.4093460685060109 ) ) ;
#59598 = CARTESIAN_POINT ( 'NONE',  ( 1.145290945507940084, 1458.110487998910003, 199.6352770989870180 ) ) ;
#59599 = DIRECTION ( 'NONE',  ( 0.02616798426500965835, 0.9993150019883683122, -0.02616798426500980754 ) ) ;
#59600 = CARTESIAN_POINT ( 'NONE',  ( 19.90023153800465749, 1526.278758871497303, 182.9652379492366094 ) ) ;
#59601 = CARTESIAN_POINT ( 'NONE',  ( -4.612507312034999529, 1516.886345593249871, 214.1313240375470173 ) ) ;
#59602 = CARTESIAN_POINT ( 'NONE',  ( 22.99941532620000118, 1409.742488423629993, 209.3674398474389875 ) ) ;
#59603 = CARTESIAN_POINT ( 'NONE',  ( -21.20923297919999584, 1509.358812534630033, 189.9045910904980019 ) ) ;
#59605 = ADVANCED_FACE ( 'NONE', ( #100715 ), #26217, .T. ) ;
#59604 = CARTESIAN_POINT ( 'NONE',  ( 7.266080978071760121, 1509.032013615249980, 215.8915072422500145 ) ) ;
#59606 = CARTESIAN_POINT ( 'NONE',  ( -1.118104767724999782, 1516.965971551240045, 211.4215139361070044 ) ) ;
#59607 = EDGE_CURVE ( 'NONE', #23415, #42647, #91832, .T. ) ;
#59608 = CARTESIAN_POINT ( 'NONE',  ( 43.50000000000000000, 1435.965051957929973, 271.1218459616979999 ) ) ;
#59609 = CARTESIAN_POINT ( 'NONE',  ( 14.06591726819999977, 1410.775981654029920, 191.2779949321979984 ) ) ;
#59610 = CARTESIAN_POINT ( 'NONE',  ( 30.64453888532167269, 1525.163527997505753, 221.6135595047366849 ) ) ;
#59611 = EDGE_CURVE ( 'NONE', #83466, #23328, #93424, .T. ) ;
#59613 = ORIENTED_EDGE ( 'NONE', *, *, #60704, .F. ) ;
#59612 = CARTESIAN_POINT ( 'NONE',  ( -62.13760418270000230, 1386.639474965800218, 284.7250346138590089 ) ) ;
#59614 = CARTESIAN_POINT ( 'NONE',  ( -67.42891481536051401, 1385.033601920959882, 291.9986235379319623 ) ) ;
#59615 = CARTESIAN_POINT ( 'NONE',  ( 32.79493994319999928, 1447.324624206830094, 248.1152222146980080 ) ) ;
#59616 = EDGE_CURVE ( 'NONE', #59275, #43874, #75554, .T. ) ;
#59617 = CARTESIAN_POINT ( 'NONE',  ( -29.16731927555590076, 1436.844791263991738, 136.7085273712292519 ) ) ;
#59618 = CARTESIAN_POINT ( 'NONE',  ( -7.559673342214999536, 1510.830536680500245, 212.2954481221070182 ) ) ;
#59619 = EDGE_CURVE ( 'NONE', #66206, #84614, #29710, .T. ) ;
#59620 = CARTESIAN_POINT ( 'NONE',  ( -8.313288157249999699, 1507.316777883029999, 235.1567909999980088 ) ) ;
#59621 = CARTESIAN_POINT ( 'NONE',  ( -23.95707600360000100, 1445.781625871360120, 214.3999464195180167 ) ) ;
#59622 = LINE ( 'NONE', #110014, #36179 ) ;
#59623 = B_SPLINE_CURVE_WITH_KNOTS ( 'NONE', 3,
 ( #35530, #52363, #27143, #76430, #78086, #77545, #849, #68059, #102707, #59100 ),
 .UNSPECIFIED., .F., .F.,
 ( 4, 2, 2, 2, 4 ),
 ( 0.000000000000000000, 0.2500000000000000555, 0.5000000000000001110, 0.7500000000000002220, 1.000000000000000000 ),
 .UNSPECIFIED. ) ;
#59625 = CARTESIAN_POINT ( 'NONE',  ( 17.57055179088690267, 1409.820984684919949, 222.6405620070939904 ) ) ;
#59624 = CARTESIAN_POINT ( 'NONE',  ( 20.54534055259999903, 1497.714303034489831, 214.2326470396490095 ) ) ;
#59626 = CARTESIAN_POINT ( 'NONE',  ( -3.909710721586109550, 1522.051704408389924, 197.7672215555029993 ) ) ;
#59627 = CARTESIAN_POINT ( 'NONE',  ( -107.6137522180000019, 1380.536624878880275, 309.5969479812590066 ) ) ;
#59628 = ORIENTED_EDGE ( 'NONE', *, *, #35181, .T. ) ;
#59629 = CARTESIAN_POINT ( 'NONE',  ( -1.130002532395000037, 1516.621991115350056, 202.1860446705670142 ) ) ;
#59630 = CARTESIAN_POINT ( 'NONE',  ( -9.534866870576710340, 1508.435327360539986, 218.9526267747990005 ) ) ;
#59631 = CARTESIAN_POINT ( 'NONE',  ( 27.87492299980000254, 1509.195406835429822, 207.4799702676380093 ) ) ;
#59632 = CARTESIAN_POINT ( 'NONE',  ( 12.78776258910000152, 1416.851343903229917, 222.7045348341980002 ) ) ;
#59633 = CARTESIAN_POINT ( 'NONE',  ( 38.41729418578510291, 1444.641748167779951, 137.0880170108979996 ) ) ;
#59634 = CARTESIAN_POINT ( 'NONE',  ( -7.000556739138234619, 1462.063838201012686, 202.3209658103452568 ) ) ;
#59635 = EDGE_CURVE ( 'NONE', #95178, #7253, #76092, .T. ) ;
#59636 = CARTESIAN_POINT ( 'NONE',  ( -0.8181503024550010883, 1443.528514123589957, 218.3809319504590007 ) ) ;
#59637 = CARTESIAN_POINT ( 'NONE',  ( 1.836834587526461560, 1468.808813678543174, 218.9756236043036779 ) ) ;
#59638 = CARTESIAN_POINT ( 'NONE',  ( 29.17442666288910047, 1435.515888873780113, 135.6503853385080163 ) ) ;
#59639 = CARTESIAN_POINT ( 'NONE',  ( 40.06992063472939947, 1445.460187879419891, 136.8880302072950030 ) ) ;
#59640 = CARTESIAN_POINT ( 'NONE',  ( -44.02689737971761730, 1450.201568725966808, 269.0198393128794692 ) ) ;
#59641 = CARTESIAN_POINT ( 'NONE',  ( -2.435720382860000033, 1429.409294826790074, 200.4602887765989863 ) ) ;
#59642 = CARTESIAN_POINT ( 'NONE',  ( 14.53903903039999790, 1509.420774818030168, 184.2780880536979851 ) ) ;
#59643 = CARTESIAN_POINT ( 'NONE',  ( -20.20959865099510111, 1512.187213306747481, 182.0120230947222524 ) ) ;
#59644 = CARTESIAN_POINT ( 'NONE',  ( 4.748711208231009451, 1507.009513748249901, 219.8044609659320088 ) ) ;
#59645 = ADVANCED_FACE ( 'NONE', ( #9432 ), #31092, .T. ) ;
#59646 = CARTESIAN_POINT ( 'NONE',  ( 0.000000000000000000, 1522.051704408389924, 209.1218459616979999 ) ) ;
#59647 = EDGE_LOOP ( 'NONE', ( #77493, #73189, #97137, #57052, #27194 ) ) ;
#59648 = CARTESIAN_POINT ( 'NONE',  ( -7.848979634317430509, 1517.051704408389924, 202.2988320601959913 ) ) ;
#59649 = CARTESIAN_POINT ( 'NONE',  ( 1.875671004969999833, 1456.514200624189925, 219.5762891113990065 ) ) ;
#59650 = EDGE_CURVE ( 'NONE', #30342, #51456, #68816, .T. ) ;
#59651 = AXIS2_PLACEMENT_3D ( 'NONE', #3623, #97108, #63000 ) ;
#59652 = CARTESIAN_POINT ( 'NONE',  ( -4.426499592775540393, 1508.728286212990042, 213.2816877793200092 ) ) ;
#59653 = CARTESIAN_POINT ( 'NONE',  ( 1.399926847669999974, 1507.072115598929940, 236.8180522793980174 ) ) ;
#59654 = CARTESIAN_POINT ( 'NONE',  ( -0.4026299538800000022, 1417.288473575429862, 234.8326129995979841 ) ) ;
#59656 = CARTESIAN_POINT ( 'NONE',  ( 13.15726447020000123, 1414.996442546130083, 197.7616625855980033 ) ) ;
#59655 = CARTESIAN_POINT ( 'NONE',  ( 11.36216709560000027, 1503.110266136990049, 211.0233811791089806 ) ) ;
#59657 = CARTESIAN_POINT ( 'NONE',  ( -28.48686853690000120, 1509.161777456430173, 209.2972665594169825 ) ) ;
#59658 = CARTESIAN_POINT ( 'NONE',  ( 0.000000000000000000, 1523.382868172864164, 209.1218459616979999 ) ) ;
#59659 = CARTESIAN_POINT ( 'NONE',  ( 2.135969990866780410, 1495.504088156479838, 220.8536837690359960 ) ) ;
#59660 = CARTESIAN_POINT ( 'NONE',  ( -7.910716753646842569, 1417.101719454672320, 230.9803857119551935 ) ) ;
#59661 = CARTESIAN_POINT ( 'NONE',  ( -32.30068554584621410, 1526.382868172863937, 198.0073124585818789 ) ) ;
#59662 = CARTESIAN_POINT ( 'NONE',  ( -17.06443472855709942, 1415.088506334920112, 208.8111692386390246 ) ) ;
#59663 = CARTESIAN_POINT ( 'NONE',  ( 25.76105412372420034, 1435.403606809190023, 135.5887298860220085 ) ) ;
#59664 = CARTESIAN_POINT ( 'NONE',  ( -5.799069655498709785, 1396.115568362039767, 199.7279999695500123 ) ) ;
#59665 = EDGE_LOOP ( 'NONE', ( #73226, #72648, #107337, #84428, #102826 ) ) ;
#59666 = CARTESIAN_POINT ( 'NONE',  ( 3.968827103902559550, 1517.151704408390060, 188.7040005461919918 ) ) ;
#59667 = CARTESIAN_POINT ( 'NONE',  ( 21.30850089961481331, 1508.868632108111569, 226.3165434354574188 ) ) ;
#59668 = ORIENTED_EDGE ( 'NONE', *, *, #24780, .F. ) ;
#59669 = VERTEX_POINT ( 'NONE', #41389 ) ;
#59670 = CARTESIAN_POINT ( 'NONE',  ( 3.434724471535389956, 1435.107767863380104, 227.2409729610280067 ) ) ;
#59671 = CARTESIAN_POINT ( 'NONE',  ( -15.42684126378997078, 1416.006794007834969, 207.1724738609944723 ) ) ;
#59673 = CARTESIAN_POINT ( 'NONE',  ( -23.79657349140000022, 1452.984769824329987, 231.7466849528980219 ) ) ;
#59672 = CARTESIAN_POINT ( 'NONE',  ( 4.500000000000000000, 1423.874532569730036, 167.3087045231979744 ) ) ;
#59674 = CARTESIAN_POINT ( 'NONE',  ( -1.466948456919999977, 1443.753574957790079, 218.3055264745389934 ) ) ;
#59675 = CARTESIAN_POINT ( 'NONE',  ( -0.02433770998772320088, 1507.114569794609906, 237.3519378586950097 ) ) ;
#59676 = CARTESIAN_POINT ( 'NONE',  ( -21.44030951619999925, 1380.278426299410057, 211.4934892549489973 ) ) ;
#59677 = CARTESIAN_POINT ( 'NONE',  ( -2.810123179937576765, 1419.851975481765294, 186.1424120031869052 ) ) ;
#59678 = CARTESIAN_POINT ( 'NONE',  ( 7.418387368310000340, 1424.469332702489965, 212.4790143585790076 ) ) ;
#59679 = CARTESIAN_POINT ( 'NONE',  ( -24.71657962519999785, 1438.057265587329994, 210.4902010153179788 ) ) ;
#59680 = FACE_BOUND ( 'NONE', #46232, .T. ) ;
#59681 = CARTESIAN_POINT ( 'NONE',  ( 3.674243458920000371, 1449.362436213359842, 184.1757723556980011 ) ) ;
#59682 = CARTESIAN_POINT ( 'NONE',  ( 9.258247136799999666, 1363.198586359130104, 207.6218459616989946 ) ) ;
#59683 = CARTESIAN_POINT ( 'NONE',  ( -29.78845675224144429, 1510.063610128411483, 205.2021543053915877 ) ) ;
#59685 = VERTEX_POINT ( 'NONE', #15590 ) ;
#59684 = CARTESIAN_POINT ( 'NONE',  ( -31.92108011125358757, 1511.187213306747708, 197.2845127572065849 ) ) ;
#59686 = ORIENTED_EDGE ( 'NONE', *, *, #95552, .T. ) ;
#59687 = CARTESIAN_POINT ( 'NONE',  ( -11.77066367041570061, 1427.133876426280040, 146.4681802475080019 ) ) ;
#59688 = B_SPLINE_CURVE_WITH_KNOTS ( 'NONE', 3,
 ( #43736, #1196, #101396, #35328, #94121, #75692, #100857, #24690, #17392, #24148, #58338, #92462, #15733, #109835, #33115, #58886, #45947, #37534, #44861, #62782, #53821, #79551 ),
 .UNSPECIFIED., .F., .F.,
 ( 4, 3, 3, 3, 3, 3, 3, 4 ),
 ( -22.88731671675060042, -22.46512262839840091, -21.08674352509629912, -19.70521628440419803, -18.32242547603609850, -16.93931000582749746, -15.55731100368929987, -14.17748175460000049 ),
 .UNSPECIFIED. ) ;
#59689 = CARTESIAN_POINT ( 'NONE',  ( 7.541469341541871430, 1510.554407339950330, 203.3603459154996358 ) ) ;
#59690 = CARTESIAN_POINT ( 'NONE',  ( -2.278119754840000066, 1472.579670685429846, 270.3712227850979843 ) ) ;
#59691 = CARTESIAN_POINT ( 'NONE',  ( 12.55314581241474770, 1434.481572427596348, 147.2585247707476981 ) ) ;
#59692 = CARTESIAN_POINT ( 'NONE',  ( -124.0634771229000393, 1314.643966242389752, 314.8853230801590257 ) ) ;
#59693 = CARTESIAN_POINT ( 'NONE',  ( 1.338895077072648876, 1526.382868172864164, 239.5739613961636110 ) ) ;
#59694 = CARTESIAN_POINT ( 'NONE',  ( 14.25730472222872258, 1435.139833118672186, 149.2707372188924921 ) ) ;
#59695 = CARTESIAN_POINT ( 'NONE',  ( -14.69722372230000040, 1408.913060387329779, 199.0844487958979983 ) ) ;
#59696 = CARTESIAN_POINT ( 'NONE',  ( 5.528921214552624974, 1369.939580316713773, 210.6218459617030021 ) ) ;
#59697 = CARTESIAN_POINT ( 'NONE',  ( -9.827940810840798846, 1446.801051858660003, 212.2330799875740013 ) ) ;
#59698 = CARTESIAN_POINT ( 'NONE',  ( -15.46198845756829954, 1407.981833872850075, 266.8669550737199643 ) ) ;
#59699 = B_SPLINE_CURVE_WITH_KNOTS ( 'NONE', 3,
 ( #93069, #33164, #76282, #110430, #75740, #15781, #42132 ),
 .UNSPECIFIED., .F., .F.,
 ( 4, 3, 4 ),
 ( -157.7301682620000065, -100.4765180537589941, -30.40177460609999116 ),
 .UNSPECIFIED. ) ;
#59700 = CARTESIAN_POINT ( 'NONE',  ( -13.80960823982659846, 1434.980805496569701, 148.6628371575099834 ) ) ;
#59701 = ORIENTED_EDGE ( 'NONE', *, *, #5309, .T. ) ;
#59702 = CARTESIAN_POINT ( 'NONE',  ( -11.97267500829999953, 1391.195698933469885, 205.7774971565190185 ) ) ;
#59703 = CARTESIAN_POINT ( 'NONE',  ( 13.11558759679999930, 1445.024186261000068, 187.9997115717980023 ) ) ;
#59704 = ORIENTED_EDGE ( 'NONE', *, *, #55436, .F. ) ;
#59705 = ORIENTED_EDGE ( 'NONE', *, *, #80351, .T. ) ;
#59706 = ADVANCED_FACE ( 'NONE', ( #77747 ), #53348, .F. ) ;
#59707 = FACE_BOUND ( 'NONE', #69075, .T. ) ;
#59708 = CARTESIAN_POINT ( 'NONE',  ( 6.204876009399109549, 1424.478647642289843, 193.6606188949869818 ) ) ;
#59709 = EDGE_CURVE ( 'NONE', #20461, #63893, #79391, .T. ) ;
#59710 = CARTESIAN_POINT ( 'NONE',  ( 6.947377783174999877, 1517.009964551830080, 213.7374907746170152 ) ) ;
#59711 = CARTESIAN_POINT ( 'NONE',  ( -16.44414657789999978, 1470.468951170730179, 188.6467452786979777 ) ) ;
#59712 = CARTESIAN_POINT ( 'NONE',  ( -17.14890260233960362, 1507.633363089370050, 229.9813627781319951 ) ) ;
#59713 = ORIENTED_EDGE ( 'NONE', *, *, #92251, .F. ) ;
#59714 = FACE_OUTER_BOUND ( 'NONE', #22590, .T. ) ;
#59715 = CARTESIAN_POINT ( 'NONE',  ( -0.7560907659159991079, 1516.770163853809890, 204.1215159365669933 ) ) ;
#59716 = ADVANCED_FACE ( 'NONE', ( #102917 ), #75177, .T. ) ;
#59717 = CARTESIAN_POINT ( 'NONE',  ( -28.34573470619999824, 1509.902915575630004, 201.4105953259380044 ) ) ;
#59718 = CARTESIAN_POINT ( 'NONE',  ( -1.116639747240000036, 1477.815261412129985, 230.7657239923979944 ) ) ;
#59719 = CARTESIAN_POINT ( 'NONE',  ( -41.28896974651279805, 1384.586842369110173, 214.1824021301610230 ) ) ;
#59720 = CARTESIAN_POINT ( 'NONE',  ( -5.082272206379999879, 1407.428259763930100, 197.0859678235980255 ) ) ;
#59721 = CARTESIAN_POINT ( 'NONE',  ( -8.502906657153658898, 1438.177461398969172, 207.2017738345354871 ) ) ;
#59723 = ORIENTED_EDGE ( 'NONE', *, *, #101680, .F. ) ;
#59722 = CARTESIAN_POINT ( 'NONE',  ( -37.77042217320030204, 1442.790213540069999, 137.1073832721159818 ) ) ;
#59724 = CARTESIAN_POINT ( 'NONE',  ( -24.98277631911100016, 1430.498769793900010, 209.4735117548389951 ) ) ;
#59725 = CARTESIAN_POINT ( 'NONE',  ( 26.12765557829999707, 1469.244184476429837, 211.6578734458780104 ) ) ;
#59726 = VECTOR ( 'NONE', #57792, 1000.000000000000000 ) ;
#59727 = CARTESIAN_POINT ( 'NONE',  ( -47.88884525074264076, 1379.684776574018997, 241.7622029387366922 ) ) ;
#59728 = CARTESIAN_POINT ( 'NONE',  ( -5.303285988883490454, 1442.879254652209966, 200.5943008362860098 ) ) ;
#59729 = CARTESIAN_POINT ( 'NONE',  ( -23.61230847530000077, 1435.322064771759869, 137.2857865107980047 ) ) ;
#59730 = CARTESIAN_POINT ( 'NONE',  ( 5.013274961385000061, 1517.068517094990057, 211.4089302402969963 ) ) ;
#59731 = CARTESIAN_POINT ( 'NONE',  ( -68.69916525130000196, 1379.747766825639928, 279.9854416248589928 ) ) ;
#59732 = AXIS2_PLACEMENT_3D ( 'NONE', #73519, #57820, #41557 ) ;
#59733 = CARTESIAN_POINT ( 'NONE',  ( -14.22059293429999904, 1415.601144549029868, 227.1159107520979887 ) ) ;
#59734 = FACE_OUTER_BOUND ( 'NONE', #33629, .T. ) ;
#59735 = EDGE_CURVE ( 'NONE', #237, #59464, #102605, .T. ) ;
#59736 = CARTESIAN_POINT ( 'NONE',  ( -2.299668004004999933, 1516.965971551240045, 208.0037412025070012 ) ) ;
#59737 = EDGE_LOOP ( 'NONE', ( #105577, #9363, #44538, #27599, #18641 ) ) ;
#59738 = DIRECTION ( 'NONE',  ( 0.000000000000000000, 0.000000000000000000, 1.000000000000000000 ) ) ;
#59739 = CARTESIAN_POINT ( 'NONE',  ( -1.034085896929999970, 1410.308950511429885, 233.0477810549980120 ) ) ;
#59740 = CARTESIAN_POINT ( 'NONE',  ( -19.88336784562452664, 1456.648868693877375, 225.3973042494007757 ) ) ;
#59741 = ORIENTED_EDGE ( 'NONE', *, *, #39759, .T. ) ;
#59742 = CARTESIAN_POINT ( 'NONE',  ( 21.54116136312531893, 1523.382868172863937, 234.3126182787002278 ) ) ;
#59743 = CARTESIAN_POINT ( 'NONE',  ( -3.812371268600000196, 1428.459941784990178, 200.5740418463989840 ) ) ;
#59744 = CARTESIAN_POINT ( 'NONE',  ( 12.69471164485930004, 1434.997246021789806, 150.4091530359009994 ) ) ;
#59745 = B_SPLINE_SURFACE_WITH_KNOTS ( 'NONE', 5, 5, ( 
 ( #38874, #97691, #89839, #73053, #55168, #54620, #98238, #82558, #106097, #65213, #14226, #13655, #30483, #89293, #64672, #97146, #46217, #4195, #38328, #105558, #80350, #98789, #22051, #5850, #20414, #106636, #12588 ),
 ( #46768, #73618, #13112, #28845, #56248, #29375, #71442, #22599, #29925, #80898, #81978, #63576, #5286, #3668, #107747, #99325, #56802, #88752, #37796, #72507, #76357, #75809, #109960, #74716, #67428, #6935, #84194 ),
 ( #41653, #24279, #50065, #25373, #39991, #100984, #101527, #32694, #110506, #8037, #31583, #65761, #85286, #41092, #33787, #14783, #93146, #84739, #109418, #108298, #99877, #91503, #83640, #75271, #74168, #48968, #33239 ),
 ( #66874, #40541, #67982, #108847, #93678, #66330, #42206, #58461, #23176, #92588, #32143, #57377, #102091, #15860, #49515, #24814, #100447, #7491, #83102, #59565, #59019, #16414, #50607, #16958, #51159, #6394, #23730 ),
 ( #57917, #92050, #15322, #86956, #8586, #10248, #103766, #18630, #104867, #42757, #69643, #70209, #1314, #44986, #87527, #226, #34352, #53950, #9694, #79134, #94242, #61792, #53380, #78008, #76918, #68527, #94810 ),
 ( #102626, #28156, #43862, #35454, #86406, #17517, #60125, #43321, #25927, #51718, #18086, #85855, #9156, #2442, #69085, #27068, #61252, #103186, #95367, #77467, #768, #10816, #34897, #52827, #95914, #26489, #44424 ) ),
 .UNSPECIFIED., .F., .F., .F.,
 ( 6, 6 ),
 ( 6, 3, 3, 3, 3, 3, 3, 3, 6 ),
 ( 1.603980125900000164, 99.04053975169999546 ),
 ( 27.66747965320000091, 34.17287967890000289, 36.60297779519999750, 37.81802685339999925, 38.42555138250000368, 39.03307591160000101, 39.44437685990000375, 39.85567780810000471, 40.67827970449999953 ),
 .UNSPECIFIED. ) ;
#59746 = CARTESIAN_POINT ( 'NONE',  ( -4.085655924655085869, 1440.415659510594423, 185.3144063599575304 ) ) ;
#59747 = CARTESIAN_POINT ( 'NONE',  ( -6.793605660180000783, 1414.360700121709897, 207.1411138948689938 ) ) ;
#59748 = CARTESIAN_POINT ( 'NONE',  ( -15.94347048536829803, 1409.469818645040050, 192.9752432267480060 ) ) ;
#59749 = B_SPLINE_CURVE_WITH_KNOTS ( 'NONE', 5,
 ( #77678, #105089, #79342, #52492, #35116, #88288 ),
 .UNSPECIFIED., .F., .F.,
 ( 6, 6 ),
 ( 0.000000000000000000, 1.000000000000000000 ),
 .UNSPECIFIED. ) ;
#59750 = CARTESIAN_POINT ( 'NONE',  ( 28.15443155984639745, 1509.896245780209938, 217.4026704617729990 ) ) ;
#59751 = DIRECTION ( 'NONE',  ( 0.000000000000000000, 0.000000000000000000, -1.000000000000000000 ) ) ;
#59752 = CARTESIAN_POINT ( 'NONE',  ( 4.222470952326010440, 1441.596861596299959, 167.7009558891260212 ) ) ;
#59753 = ADVANCED_FACE ( 'NONE', ( #2171 ), #57290, .T. ) ;
#59755 = CARTESIAN_POINT ( 'NONE',  ( -3.998460401129999564, 1421.841081959129951, 184.4445580210980324 ) ) ;
#59754 = CARTESIAN_POINT ( 'NONE',  ( -4.031142389804999837, 1516.929569650079884, 214.1322689334670031 ) ) ;
#59756 = CARTESIAN_POINT ( 'NONE',  ( 20.67635560069999912, 1509.397142797630067, 188.6960315703979916 ) ) ;
#59757 = CARTESIAN_POINT ( 'NONE',  ( -4.406834599037237510, 1421.289441775209980, 144.1372251532988003 ) ) ;
#59758 = ORIENTED_EDGE ( 'NONE', *, *, #23305, .F. ) ;
#59759 = FACE_OUTER_BOUND ( 'NONE', #36385, .T. ) ;
#59760 = CONICAL_SURFACE ( 'NONE', #31124, 6.911399307709998219, 0.04363323129990067523 ) ;
#59761 = FACE_OUTER_BOUND ( 'NONE', #80342, .T. ) ;
#59762 = VERTEX_POINT ( 'NONE', #105154 ) ;
#59763 = CARTESIAN_POINT ( 'NONE',  ( 1.780863054839999959, 1419.796581447929839, 184.9705365426980279 ) ) ;
#59764 = EDGE_CURVE ( 'NONE', #36772, #75744, #55135, .T. ) ;
#59765 = CARTESIAN_POINT ( 'NONE',  ( 5.316196956075327051, 1519.551704408389924, 187.2259631713411636 ) ) ;
#59766 = PLANE ( 'NONE',  #28799 ) ;
#59767 = CARTESIAN_POINT ( 'NONE',  ( -7.545141261034559399, 1384.919253706480049, 219.0875759670219907 ) ) ;
#59768 = CARTESIAN_POINT ( 'NONE',  ( -11.40596013332580050, 1470.784863085199959, 209.0332487307530300 ) ) ;
#59769 = CARTESIAN_POINT ( 'NONE',  ( -7.713101326021401860, 1508.427059880648358, 219.5098945182681121 ) ) ;
#59770 = FACE_OUTER_BOUND ( 'NONE', #56144, .T. ) ;
#59771 = DIRECTION ( 'NONE',  ( 0.000000000000000000, 0.000000000000000000, 1.000000000000000000 ) ) ;
#59772 = CARTESIAN_POINT ( 'NONE',  ( -7.884560102309425389, 1458.514255516424100, 214.6067317821517406 ) ) ;
#59773 = CARTESIAN_POINT ( 'NONE',  ( -9.690208402899999740, 1434.541746329560056, 148.7586030823979968 ) ) ;
#59774 = CARTESIAN_POINT ( 'NONE',  ( 40.48639141129520169, 1440.913060360999907, 259.9639464203100374 ) ) ;
#59776 = CARTESIAN_POINT ( 'NONE',  ( 4.327012684985810154, 1515.157823446690145, 208.9938042305240060 ) ) ;
#59775 = CARTESIAN_POINT ( 'NONE',  ( -4.394042746799730281, 1420.918297765330180, 194.0393747012239771 ) ) ;
#59777 = CARTESIAN_POINT ( 'NONE',  ( -3.448830483803573710, 1523.382868172864164, 243.0842028158767505 ) ) ;
#59778 = VERTEX_POINT ( 'NONE', #90541 ) ;
#59779 = ORIENTED_EDGE ( 'NONE', *, *, #108896, .F. ) ;
#59780 = EDGE_CURVE ( 'NONE', #66581, #9033, #74327, .T. ) ;
#59781 = DIRECTION ( 'NONE',  ( 0.000000000000000000, 0.000000000000000000, 1.000000000000000000 ) ) ;
#59782 = CARTESIAN_POINT ( 'NONE',  ( -24.41216396249999931, 1440.964695643669984, 212.0310679874179982 ) ) ;
#59783 = CARTESIAN_POINT ( 'NONE',  ( 6.688171886676422595, 1447.885435886052392, 185.1357882069593472 ) ) ;
#59784 = CARTESIAN_POINT ( 'NONE',  ( -3.006969711954706526, 1425.989600909259252, 185.4751844751110923 ) ) ;
#59785 = EDGE_CURVE ( 'NONE', #77321, #42035, #71205, .T. ) ;
#59786 = B_SPLINE_SURFACE_WITH_KNOTS ( 'NONE', 4, 5, ( 
 ( #48100, #55954, #98484, #57067, #13359, #31284 ),
 ( #5541, #39120, #39692, #21752, #47550, #63276 ),
 ( #14473, #30730, #48665, #97387, #64915, #20658 ),
 ( #54860, #50323, #66578, #23966, #83891, #40237 ),
 ( #57623, #67671, #74420, #83340, #40791, #25068 ) ),
 .UNSPECIFIED., .F., .F., .F.,
 ( 5, 5 ),
 ( 6, 6 ),
 ( 7.148411859579999472, 7.252819523530000367 ),
 ( 0.000000000000000000, 2.228199834939999846 ),
 .UNSPECIFIED. ) ;
#59787 = CARTESIAN_POINT ( 'NONE',  ( 1.804213551060599885, 1410.351307734219972, 232.1928989352460064 ) ) ;
#59788 = CARTESIAN_POINT ( 'NONE',  ( -4.638785869710670084, 1378.122666164550310, 203.7745336881851586 ) ) ;
#59789 = CARTESIAN_POINT ( 'NONE',  ( -4.324092179420000015, 1515.269353058490196, 209.1218459618469865 ) ) ;
#59790 = CARTESIAN_POINT ( 'NONE',  ( -53.74473075458050175, 1383.805872317579997, 268.9597808447719558 ) ) ;
#59791 = CARTESIAN_POINT ( 'NONE',  ( -10.76610300729999992, 1461.751116409589940, 211.3389343560589850 ) ) ;
#59792 = CARTESIAN_POINT ( 'NONE',  ( -28.17098632135910918, 1509.816547239969623, 212.1705146586627109 ) ) ;
#59793 = CARTESIAN_POINT ( 'NONE',  ( -23.42685059075717646, 1410.407670574614940, 210.3305991070054972 ) ) ;
#59795 = VERTEX_POINT ( 'NONE', #40145 ) ;
#59794 = CARTESIAN_POINT ( 'NONE',  ( 10.56687430813880013, 1452.631846242170013, 209.6720685516360163 ) ) ;
#59796 = CARTESIAN_POINT ( 'NONE',  ( -1.270728227810000055, 1414.996442546230128, 226.4582995913979744 ) ) ;
#59797 = CARTESIAN_POINT ( 'NONE',  ( -40.27282834620000074, 1380.934810191280121, 238.2933727449590151 ) ) ;
#59798 = CARTESIAN_POINT ( 'NONE',  ( 19.77866596905520069, 1507.914512822359939, 229.2835366231990122 ) ) ;
#59799 = ORIENTED_EDGE ( 'NONE', *, *, #19692, .F. ) ;
#59800 = ORIENTED_EDGE ( 'NONE', *, *, #42680, .T. ) ;
#59801 = CARTESIAN_POINT ( 'NONE',  ( 17.32428483191130297, 1508.223220029260119, 230.9736489382000002 ) ) ;
#59802 = DIRECTION ( 'NONE',  ( -0.4763271851929161138, 0.000000000000000000, 0.8792681119238848764 ) ) ;
#59803 = CARTESIAN_POINT ( 'NONE',  ( 38.88009490570040327, 1439.559590605640096, 136.6872614661130001 ) ) ;
#59805 = SPHERICAL_SURFACE ( 'NONE', #44900, 2.000000000000000000 ) ;
#59804 = CARTESIAN_POINT ( 'NONE',  ( 21.49889961270000072, 1488.801231228130064, 209.3947183657330129 ) ) ;
#59806 = CIRCLE ( 'NONE', #13253, 26.50000000000001421 ) ;
#59807 = CARTESIAN_POINT ( 'NONE',  ( 11.76251392144250119, 1479.675718945300105, 209.8000875804440284 ) ) ;
#59808 = CARTESIAN_POINT ( 'NONE',  ( -108.7999967259999892, 1381.610864533399990, 297.7780583747590413 ) ) ;
#59809 = DIRECTION ( 'NONE',  ( 0.2766542314861598628, 0.3717636679784723786, 0.8861457054976875636 ) ) ;
#59810 = CARTESIAN_POINT ( 'NONE',  ( 0.000000000000000000, 1378.013060387289897, 209.1218459616989946 ) ) ;
#59811 = DIRECTION ( 'NONE',  ( -0.9455185755993178454, 0.000000000000000000, 0.3255681544571537578 ) ) ;
#59812 = CARTESIAN_POINT ( 'NONE',  ( 3.268551751039999953, 1410.404426152929773, 185.7978215306979735 ) ) ;
#59813 = CARTESIAN_POINT ( 'NONE',  ( -0.01713803560704209999, 1486.114444591910114, 197.2146938469659858 ) ) ;
#59814 = CARTESIAN_POINT ( 'NONE',  ( 10.52925756285159942, 1470.684013483499939, 209.6681956286249999 ) ) ;
#59815 = CARTESIAN_POINT ( 'NONE',  ( 6.800214974479639629, 1435.261544033620112, 203.8159018546080290 ) ) ;
#59816 = CARTESIAN_POINT ( 'NONE',  ( -4.263072128268690086, 1441.226134037160136, 159.2129237521010054 ) ) ;
#59817 = AXIS2_PLACEMENT_3D ( 'NONE', #12970, #5132, #47153 ) ;
#59818 = CARTESIAN_POINT ( 'NONE',  ( -2.743100966568880139, 1450.921041808649989, 184.6046904293359887 ) ) ;
#59819 = CARTESIAN_POINT ( 'NONE',  ( 0.6879682657500000298, 1464.995962445229907, 237.3245376353980021 ) ) ;
#59820 = ORIENTED_EDGE ( 'NONE', *, *, #54775, .T. ) ;
#59821 = CARTESIAN_POINT ( 'NONE',  ( 4.722103809230000060, 1472.365862868290151, 187.6427232028989920 ) ) ;
#59822 = CARTESIAN_POINT ( 'NONE',  ( -42.42054896300000166, 1443.932089742500011, 270.0676470778980161 ) ) ;
#59823 = CARTESIAN_POINT ( 'NONE',  ( -23.69928159108154375, 1436.231577400298420, 212.2790965043357403 ) ) ;
#59824 = DIRECTION ( 'NONE',  ( -1.836970198721029688E-16, -1.000000000000000000, 0.000000000000000000 ) ) ;
#59825 = CARTESIAN_POINT ( 'NONE',  ( 15.05055690159999848, 1410.738883364130061, 191.5204107739980088 ) ) ;
#59826 = DIRECTION ( 'NONE',  ( -0.4035202328300226404, 0.000000000000000000, 0.9149707217702675033 ) ) ;
#59827 = CARTESIAN_POINT ( 'NONE',  ( 22.41589833909626606, 1436.510086781942846, 142.7382537882818099 ) ) ;
#59828 = CARTESIAN_POINT ( 'NONE',  ( -12.91325991898034786, 1507.673968545811704, 209.2392918446375063 ) ) ;
#59829 = CARTESIAN_POINT ( 'NONE',  ( -8.202992217649999418, 1418.657529326630083, 231.5784025581979790 ) ) ;
#59830 = CARTESIAN_POINT ( 'NONE',  ( 1.329456730940000053, 1477.528821806389942, 198.7863296140990030 ) ) ;
#59831 = CARTESIAN_POINT ( 'NONE',  ( -105.8118099419999965, 1391.581618872429999, 306.6506172913590262 ) ) ;
#59832 = CARTESIAN_POINT ( 'NONE',  ( -7.683752594814639458, 1511.083508941950186, 214.8842481327019982 ) ) ;
#59833 = CARTESIAN_POINT ( 'NONE',  ( 3.586287380388563317, 1359.668001507771805, 207.6218459616987673 ) ) ;
#59834 = CARTESIAN_POINT ( 'NONE',  ( -45.54444238527090505, 1438.304335038940053, 266.1920658830019875 ) ) ;
#59835 = CARTESIAN_POINT ( 'NONE',  ( 14.09058600726540078, 1509.404319979430056, 234.7755637671129989 ) ) ;
#59836 = CARTESIAN_POINT ( 'NONE',  ( -1.430539248151910137, 1444.328264662749916, 199.1703804428329931 ) ) ;
#59837 = EDGE_LOOP ( 'NONE', ( #89171, #9703, #78560, #106384 ) ) ;
#59838 = CARTESIAN_POINT ( 'NONE',  ( -1.709766532154999963, 1516.959716008189844, 209.1345041580460133 ) ) ;
#59839 = EDGE_CURVE ( 'NONE', #29176, #17951, #4350, .T. ) ;
#59840 = CARTESIAN_POINT ( 'NONE',  ( -5.387558624149999531, 1432.551536822860044, 154.6121729928979960 ) ) ;
#59841 = CARTESIAN_POINT ( 'NONE',  ( 19.38028738881421731, 1456.807072245457448, 224.5317582173058213 ) ) ;
#59842 = CARTESIAN_POINT ( 'NONE',  ( 7.205920432443370771, 1426.539681308049921, 212.9869048957809810 ) ) ;
#59843 = CARTESIAN_POINT ( 'NONE',  ( -26.75400904328050089, 1451.059527259639935, 136.3674970195820038 ) ) ;
#59844 = ORIENTED_EDGE ( 'NONE', *, *, #82253, .T. ) ;
#59845 = CARTESIAN_POINT ( 'NONE',  ( 24.48136660710000001, 1435.989032281489926, 217.2949255070680010 ) ) ;
#59847 = CARTESIAN_POINT ( 'NONE',  ( 14.27633599229999994, 1452.807100928330101, 195.2240231267980164 ) ) ;
#59846 = CARTESIAN_POINT ( 'NONE',  ( -3.237130272123891928, 1524.843178112495480, 176.5219626358610583 ) ) ;
#59848 = AXIS2_PLACEMENT_3D ( 'NONE', #23080, #30394, #72967 ) ;
#59849 = CARTESIAN_POINT ( 'NONE',  ( 0.5238056268335857801, 1487.609062966209649, 219.9549396858940895 ) ) ;
#59850 = FACE_OUTER_BOUND ( 'NONE', #23701, .T. ) ;
#59851 = DIRECTION ( 'NONE',  ( 9.230617842401318720E-47, -1.000000000000000000, 1.836970198721029688E-16 ) ) ;
#59852 = EDGE_CURVE ( 'NONE', #2574, #39868, #54392, .T. ) ;
#59853 = CARTESIAN_POINT ( 'NONE',  ( 4.333931798808769997, 1467.827050109060110, 218.1149461721859950 ) ) ;
#59854 = CARTESIAN_POINT ( 'NONE',  ( 16.36456115949343015, 1517.151704408390060, 198.1507535207238391 ) ) ;
#59855 = ORIENTED_EDGE ( 'NONE', *, *, #20564, .T. ) ;
#59856 = CARTESIAN_POINT ( 'NONE',  ( -6.588284554585150055, 1410.390471986989951, 269.8687522186629622 ) ) ;
#59857 = CARTESIAN_POINT ( 'NONE',  ( 4.143780836689379576, 1416.454745150250119, 231.7095439720729928 ) ) ;
#59858 = DIRECTION ( 'NONE',  ( -0.9455185755993178454, 0.000000000000000000, 0.3255681544571537578 ) ) ;
#59860 = VERTEX_POINT ( 'NONE', #2863 ) ;
#59859 = CARTESIAN_POINT ( 'NONE',  ( 20.50000000000000000, 1445.052233488290085, 169.0968414572980123 ) ) ;
#59861 = VERTEX_POINT ( 'NONE', #12881 ) ;
#59862 = CARTESIAN_POINT ( 'NONE',  ( -110.0482597500069915, 1385.373319905469771, 296.9711118272649628 ) ) ;
#59863 = CARTESIAN_POINT ( 'NONE',  ( 0.004479545552087010364, 1409.421457559500141, 185.2262415390000001 ) ) ;
#59864 = CARTESIAN_POINT ( 'NONE',  ( -109.9850845680699933, 1384.907642987549934, 311.4561493310270066 ) ) ;
#59865 = CARTESIAN_POINT ( 'NONE',  ( -45.65247486738287108, 1439.849382516791593, 266.1891217565876673 ) ) ;
#59866 = CARTESIAN_POINT ( 'NONE',  ( -18.35772982613910287, 1422.336849757289883, 194.8914311005219986 ) ) ;
#59867 = CARTESIAN_POINT ( 'NONE',  ( -18.17931802150000209, 1415.859000051729936, 224.8780086886979745 ) ) ;
#59868 = CARTESIAN_POINT ( 'NONE',  ( 30.13944988253700075, 1467.656954244930148, 267.4649828126950410 ) ) ;
#59869 = CARTESIAN_POINT ( 'NONE',  ( -11.09483971705885885, 1464.088240666073261, 231.7174097975078553 ) ) ;
#59870 = CARTESIAN_POINT ( 'NONE',  ( -17.30312348755748530, 1422.521282115817712, 226.6250572771207317 ) ) ;
#59871 =( BOUNDED_CURVE ( )  B_SPLINE_CURVE ( 3, ( #11622, #71575, #3248, #46353 ),
 .UNSPECIFIED., .F., .F. ) 
 B_SPLINE_CURVE_WITH_KNOTS ( ( 4, 4 ),
 ( 5.361618747459259815, 6.000063634424889436 ),
 .UNSPECIFIED. ) 
 CURVE ( )  GEOMETRIC_REPRESENTATION_ITEM ( )  RATIONAL_B_SPLINE_CURVE ( ( 1.000000000000000000, 0.9663198162573465311, 0.9663198162573465311, 1.000000000000000000 ) ) 
 REPRESENTATION_ITEM ( '' )  );
#59872 = CARTESIAN_POINT ( 'NONE',  ( -5.011678876155000850, 1516.989560013210166, 205.8658785457569991 ) ) ;
#59873 = EDGE_LOOP ( 'NONE', ( #1195, #14245, #108169, #11740 ) ) ;
#59874 = CARTESIAN_POINT ( 'NONE',  ( 18.50667789485245507, 1458.752429087900964, 227.6133156040012011 ) ) ;
#59875 = CARTESIAN_POINT ( 'NONE',  ( 1.771184440399770077, 1445.612359891010101, 199.1903901163940134 ) ) ;
#59876 = DIRECTION ( 'NONE',  ( 0.000000000000000000, 1.000000000000000000, 0.000000000000000000 ) ) ;
#59877 = ORIENTED_EDGE ( 'NONE', *, *, #45967, .F. ) ;
#59878 = CARTESIAN_POINT ( 'NONE',  ( 2.487923159525660122, 1508.611354624159958, 204.4437017682370197 ) ) ;
#59879 = ADVANCED_FACE ( 'NONE', ( #44870 ), #58180, .T. ) ;
#59880 = CARTESIAN_POINT ( 'NONE',  ( 26.92948524801489896, 1451.211802498159841, 136.2741858638970029 ) ) ;
#59881 = CARTESIAN_POINT ( 'NONE',  ( -4.001327954982739854, 1508.551704408389924, 213.5978375056940024 ) ) ;
#59882 = CARTESIAN_POINT ( 'NONE',  ( 12.41491102362930121, 1501.318694629519996, 211.8840886488729893 ) ) ;
#59883 = ADVANCED_FACE ( 'NONE', ( #28590 ), #15229, .F. ) ;
#59884 = CARTESIAN_POINT ( 'NONE',  ( 7.311826422820000282, 1422.546741514869836, 195.5507102769989842 ) ) ;
#59886 = B_SPLINE_SURFACE_WITH_KNOTS ( 'NONE', 5, 5, ( 
 ( #13610, #100397, #30985, #23123, #90891, #65160 ),
 ( #99832, #74114, #14176, #82502, #91454, #5803 ),
 ( #47798, #39944, #108245, #6340, #83047, #31535 ),
 ( #65710, #34841, #100924, #84139, #43260, #51110 ),
 ( #713, #24759, #77407, #16904, #75757, #69032 ),
 ( #25870, #75216, #102031, #67922, #24222, #42151 ),
 ( #67373, #18029, #25317, #170, #50560, #52221 ),
 ( #7439, #7984, #84686, #109903, #6883, #85234 ),
 ( #41037, #15801, #59514, #26433, #103133, #16361 ) ),
 .UNSPECIFIED., .F., .F., .F.,
 ( 6, 3, 6 ),
 ( 6, 6 ),
 ( 14.73068219289999981, 30.91096027220000053, 36.02199544990000390 ),
 ( 0.000000000000000000, 2.000000000000000000 ),
 .UNSPECIFIED. ) ;
#59885 = CARTESIAN_POINT ( 'NONE',  ( -4.128104903896989697, 1425.965123590259509, 186.1105249954287331 ) ) ;
#59887 = FACE_OUTER_BOUND ( 'NONE', #83124, .T. ) ;
#59888 = AXIS2_PLACEMENT_3D ( 'NONE', #33416, #25014, #110692 ) ;
#59889 = CARTESIAN_POINT ( 'NONE',  ( 0.5844443723097010324, 1408.933469634509947, 186.5656055688390040 ) ) ;
#59891 = CARTESIAN_POINT ( 'NONE',  ( 3.829620113550000315, 1515.551704408389924, 210.9648081929590262 ) ) ;
#59890 = CARTESIAN_POINT ( 'NONE',  ( 30.64459234690374956, 1525.163457223743762, 196.6300966631588381 ) ) ;
#59892 = CARTESIAN_POINT ( 'NONE',  ( -113.4000000000000057, 1390.939237335599955, 304.2218459572590064 ) ) ;
#59893 = EDGE_CURVE ( 'NONE', #34577, #97374, #43581, .T. ) ;
#59894 = CARTESIAN_POINT ( 'NONE',  ( -13.41289550449999979, 1379.525782299150023, 211.7978701437990026 ) ) ;
#59895 = CIRCLE ( 'NONE', #106312, 1.000000000000000888 ) ;
#59896 = CARTESIAN_POINT ( 'NONE',  ( 11.31580077666816742, 1420.115919293237539, 232.0087015463770115 ) ) ;
#59897 = ORIENTED_EDGE ( 'NONE', *, *, #6266, .F. ) ;
#59898 = CARTESIAN_POINT ( 'NONE',  ( 11.46011354709300001, 1414.971717244350202, 221.6095414742599985 ) ) ;
#59899 = AXIS2_PLACEMENT_3D ( 'NONE', #65027, #99145, #22423 ) ;
#59900 = DIRECTION ( 'NONE',  ( 0.4794255386042030054, 0.000000000000000000, 0.8775825618903727587 ) ) ;
#59901 = DIRECTION ( 'NONE',  ( -9.138167445698339565E-47, 1.000000000000000000, -1.836970198721029688E-16 ) ) ;
#59902 = ADVANCED_FACE ( 'NONE', ( #47601 ), #101994, .T. ) ;
#59903 = B_SPLINE_SURFACE_WITH_KNOTS ( 'NONE', 5, 5, ( 
 ( #23006, #57209, #91333, #14618, #48805, #6220 ),
 ( #40372, #74551, #31976, #16791, #27429, #43146 ),
 ( #10647, #44814, #1707, #103021, #8974, #78968 ),
 ( #35285, #2273, #68365, #35847, #52653, #95195 ),
 ( #17345, #76738, #26317, #49, #19009, #103590 ),
 ( #36387, #52104, #50995, #9525, #70032, #43693 ) ),
 .UNSPECIFIED., .F., .F., .F.,
 ( 6, 6 ),
 ( 6, 6 ),
 ( 43.60693323619999973, 57.21764454529999711 ),
 ( 0.000000000000000000, 2.000000000000000000 ),
 .UNSPECIFIED. ) ;
#59904 = CARTESIAN_POINT ( 'NONE',  ( -12.36594955309999833, 1391.700202007920097, 209.7454160267469945 ) ) ;
#59905 = CARTESIAN_POINT ( 'NONE',  ( 9.911722878192179564, 1428.067636776900144, 211.9710459987479965 ) ) ;
#59906 = CARTESIAN_POINT ( 'NONE',  ( 0.4038046531345523271, 1421.163526409605765, 193.7214141364934221 ) ) ;
#59907 = CARTESIAN_POINT ( 'NONE',  ( -10.93147186535690096, 1462.715198542749931, 207.4958911510919961 ) ) ;
#59908 = FACE_OUTER_BOUND ( 'NONE', #80962, .T. ) ;
#59909 = CARTESIAN_POINT ( 'NONE',  ( -21.60872112289791147, 1509.279327801856198, 191.6769273891482612 ) ) ;
#59910 = CARTESIAN_POINT ( 'NONE',  ( 11.83363686220000055, 1433.395016513080009, 150.5889480672979914 ) ) ;
#59911 = CARTESIAN_POINT ( 'NONE',  ( -1.247529711191919932E-05, 1474.073207343779814, 267.9039250723909618 ) ) ;
#59912 = B_SPLINE_SURFACE_WITH_KNOTS ( 'NONE', 5, 5, ( 
 ( #87781, #17758, #28410, #27299, #61480, #68779 ),
 ( #93935, #9396, #43559, #77709, #26742, #95608 ),
 ( #69328, #53637, #18875, #53073, #87211, #10502 ),
 ( #103436, #70442, #44674, #104562, #43009, #27856 ),
 ( #62037, #96160, #77167, #19438, #36809, #11061 ),
 ( #2685, #71000, #17201, #88866, #98904, #38991 ),
 ( #30043, #72100, #105683, #72622, #97255, #106216 ),
 ( #3235, #81544, #29498, #28966, #73169, #107313 ),
 ( #12703, #79922, #56373, #107859, #71563, #63156 ) ),
 .UNSPECIFIED., .F., .F., .F.,
 ( 6, 3, 6 ),
 ( 6, 6 ),
 ( 6.014757022580000445, 12.35992153179999953, 20.20875793540000132 ),
 ( -4.440892098509999801E-16, 10.00000000000000000 ),
 .UNSPECIFIED. ) ;
#59913 = CARTESIAN_POINT ( 'NONE',  ( 12.50318290584439929, 1415.427621830080170, 196.7915438783630009 ) ) ;
#59914 = CARTESIAN_POINT ( 'NONE',  ( 18.34445210801149884, 1428.946210474640111, 201.3092770736820114 ) ) ;
#59915 = B_SPLINE_CURVE_WITH_KNOTS ( 'NONE', 5,
 ( #97546, #20817, #48814, #106495, #38726, #21900, #23016, #107041, #6227, #67268, #32544, #109260 ),
 .UNSPECIFIED., .F., .F.,
 ( 6, 3, 3, 6 ),
 ( 0.000000000000000000, 0.4545476142708403944, 0.7388436783044410872, 1.000000000000000000 ),
 .UNSPECIFIED. ) ;
#59916 = CARTESIAN_POINT ( 'NONE',  ( 9.425093484676720479, 1420.682064370679882, 196.8057936142159861 ) ) ;
#59917 = CARTESIAN_POINT ( 'NONE',  ( 10.15219587857820116, 1462.852240055779930, 213.4500398469340041 ) ) ;
#59918 = CARTESIAN_POINT ( 'NONE',  ( -18.38973187710000090, 1486.345248910030023, 188.6648160310980131 ) ) ;
#59919 = CARTESIAN_POINT ( 'NONE',  ( 11.72654505936638003, 1398.260515437505774, 203.3308392036481678 ) ) ;
#59920 = CARTESIAN_POINT ( 'NONE',  ( -3.200208338885655479, 1370.366479271463049, 211.5769014320682970 ) ) ;
#59921 = ADVANCED_FACE ( 'NONE', ( #41407 ), #92895, .T. ) ;
#59922 = CARTESIAN_POINT ( 'NONE',  ( -8.084570023343367495, 1425.034990034922430, 209.7848060853768573 ) ) ;
#59923 = CARTESIAN_POINT ( 'NONE',  ( 12.78690713350000152, 1416.828040475229955, 222.7042044314979989 ) ) ;
#59924 = FACE_OUTER_BOUND ( 'NONE', #6241, .T. ) ;
#59925 = CARTESIAN_POINT ( 'NONE',  ( 9.923042118358591068, 1451.489751077119990, 207.3834753951100254 ) ) ;
#59926 = CARTESIAN_POINT ( 'NONE',  ( 18.82191891289999930, 1431.113060387329824, 213.4824283078179974 ) ) ;
#59927 = CIRCLE ( 'NONE', #67043, 26.00000000000000711 ) ;
#59928 = CARTESIAN_POINT ( 'NONE',  ( 24.04367182619530041, 1494.655699650459837, 207.1743774084869756 ) ) ;
#59929 = EDGE_CURVE ( 'NONE', #30213, #911, #102673, .T. ) ;
#59930 = CARTESIAN_POINT ( 'NONE',  ( -3.448206916814999801, 1516.904492006980036, 213.1642637479369853 ) ) ;
#59931 = CARTESIAN_POINT ( 'NONE',  ( -17.84399408628319961, 1419.477046998499873, 208.9994865744390040 ) ) ;
#59932 = CARTESIAN_POINT ( 'NONE',  ( 0.1890019494398779976, 1469.284980727640004, 182.5545442408230201 ) ) ;
#59934 = ORIENTED_EDGE ( 'NONE', *, *, #70316, .T. ) ;
#59933 = CARTESIAN_POINT ( 'NONE',  ( 18.29188182340000068, 1431.768652859389704, 209.1218459616989946 ) ) ;
#59935 = DIRECTION ( 'NONE',  ( -0.9942586961433756976, -0.000000000000000000, -0.1070030146457317671 ) ) ;
#59936 = DIRECTION ( 'NONE',  ( -0.000000000000000000, -1.000000000000000000, -0.000000000000000000 ) ) ;
#59937 = CARTESIAN_POINT ( 'NONE',  ( 13.19841768679999916, 1434.900414241469889, 149.7891824259980069 ) ) ;
#59938 = CARTESIAN_POINT ( 'NONE',  ( -41.25063694456439833, 1441.159963068149864, 134.0999999980680002 ) ) ;
#59939 = CARTESIAN_POINT ( 'NONE',  ( -7.559730510238970247, 1508.551704408389924, 219.0490070243000105 ) ) ;
#59940 = VERTEX_POINT ( 'NONE', #77223 ) ;
#59941 = CARTESIAN_POINT ( 'NONE',  ( -10.28013529000000048, 1471.607561406590094, 209.6293381294269977 ) ) ;
#59942 = AXIS2_PLACEMENT_3D ( 'NONE', #104165, #95217, #88475 ) ;
#59943 = DIRECTION ( 'NONE',  ( 8.727810504445229884E-47, -1.000000000000000000, 1.836970198721029688E-16 ) ) ;
#59944 = CARTESIAN_POINT ( 'NONE',  ( 3.601839739459999912, 1444.840594719589944, 200.9001243581789993 ) ) ;
#59945 = CARTESIAN_POINT ( 'NONE',  ( -15.57808073540140015, 1420.358152465259991, 210.5578313205389804 ) ) ;
#59946 = CARTESIAN_POINT ( 'NONE',  ( 0.6715583085099990912, 1506.489872953789927, 221.9351472385990007 ) ) ;
#59947 = CARTESIAN_POINT ( 'NONE',  ( -108.3047457728057452, 1381.116487792409089, 310.2605079287397416 ) ) ;
#59948 = B_SPLINE_CURVE_WITH_KNOTS ( 'NONE', 3,
 ( #86400, #52822, #9688, #42200, #86952, #24809 ),
 .UNSPECIFIED., .F., .F.,
 ( 4, 2, 4 ),
 ( 0.000000000000000000, 0.5000000000000000000, 1.000000000000000000 ),
 .UNSPECIFIED. ) ;
#59949 = DIRECTION ( 'NONE',  ( 0.000000000000000000, -1.000000000000000000, 0.000000000000000000 ) ) ;
#59950 = DIRECTION ( 'NONE',  ( 0.000000000000000000, 0.000000000000000000, -1.000000000000000000 ) ) ;
#59951 = FACE_OUTER_BOUND ( 'NONE', #16969, .T. ) ;
#59952 = CARTESIAN_POINT ( 'NONE',  ( -81.15982276781578264, 1385.162085608370035, 284.5929643925970254 ) ) ;
#59953 = CARTESIAN_POINT ( 'NONE',  ( -11.03830765538920033, 1391.913060387289988, 212.4289022242699900 ) ) ;
#59954 = CARTESIAN_POINT ( 'NONE',  ( 11.82045713465280024, 1421.864468249930269, 207.3034728234389945 ) ) ;
#59955 = ORIENTED_EDGE ( 'NONE', *, *, #53839, .F. ) ;
#59956 = CARTESIAN_POINT ( 'NONE',  ( -33.30820988179999631, 1451.750048702429922, 135.1664504609980213 ) ) ;
#59957 = CARTESIAN_POINT ( 'NONE',  ( -15.81585810399169922, 1410.113222428570225, 226.5225277695919885 ) ) ;
#59959 = ORIENTED_EDGE ( 'NONE', *, *, #104861, .F. ) ;
#59958 = DIRECTION ( 'NONE',  ( -1.000000000000000000, 0.000000000000000000, 0.000000000000000000 ) ) ;
#59960 = CARTESIAN_POINT ( 'NONE',  ( -20.20959865099451847, 1522.382868172863937, 236.2316688286741453 ) ) ;
#59961 = CARTESIAN_POINT ( 'NONE',  ( -18.27210413946250256, 1441.296816368030022, 213.1559958055480024 ) ) ;
#59962 = CARTESIAN_POINT ( 'NONE',  ( -8.251318938499840883, 1363.612701139454202, 207.6218459616988241 ) ) ;
#59963 = CARTESIAN_POINT ( 'NONE',  ( -9.980038972539999165, 1493.754093306789855, 204.0458854781789739 ) ) ;
#59964 = CARTESIAN_POINT ( 'NONE',  ( 36.70160066626374373, 1455.767766055568927, 269.5559760384784909 ) ) ;
#59965 = CARTESIAN_POINT ( 'NONE',  ( -16.68463225901000158, 1442.773887286389936, 162.0935120915889911 ) ) ;
#59966 = CARTESIAN_POINT ( 'NONE',  ( 19.41828847086908283, 1440.403404493772996, 212.4137351852459403 ) ) ;
#59967 = CARTESIAN_POINT ( 'NONE',  ( -9079.130222195200986, 5181.793945261120825, -1567.248257619579817 ) ) ;
#59968 = CARTESIAN_POINT ( 'NONE',  ( 6.185074461130000145, 1447.943819131290184, 200.8573415407390144 ) ) ;
#59969 = CARTESIAN_POINT ( 'NONE',  ( 10.85845406881951192, 1424.793774302243946, 138.1921923613813590 ) ) ;
#59970 = CARTESIAN_POINT ( 'NONE',  ( -9.934214826642712381, 1367.375828905819617, 207.6218459616987673 ) ) ;
#59971 = CARTESIAN_POINT ( 'NONE',  ( -2.817242487250000149, 1454.702949441090141, 199.4062663517090073 ) ) ;
#59972 = CARTESIAN_POINT ( 'NONE',  ( 3.446329775655000205, 1516.812046502680005, 206.2422037788969931 ) ) ;
#59973 = CARTESIAN_POINT ( 'NONE',  ( 2.713767649309999808, 1447.666028319260022, 156.1533243690980157 ) ) ;
#59974 = CARTESIAN_POINT ( 'NONE',  ( 11.86100642208650058, 1492.894948804929982, 212.5846969273300147 ) ) ;
#59975 = CARTESIAN_POINT ( 'NONE',  ( 13.58256592070000046, 1416.843576337130116, 196.3343231799980231 ) ) ;
#59977 = ORIENTED_EDGE ( 'NONE', *, *, #85252, .F. ) ;
#59976 = CARTESIAN_POINT ( 'NONE',  ( 1.792291835849999959, 1494.398898525389995, 220.1169104681989950 ) ) ;
#59978 = DIRECTION ( 'NONE',  ( 0.000000000000000000, 0.000000000000000000, 1.000000000000000000 ) ) ;
#59979 = ORIENTED_EDGE ( 'NONE', *, *, #64430, .T. ) ;
#59980 = CARTESIAN_POINT ( 'NONE',  ( -16.52212295123237240, 1514.209381233995373, 223.4393621722829266 ) ) ;
#59981 = CARTESIAN_POINT ( 'NONE',  ( -23.92333147340000110, 1430.353917317029982, 204.8973678502680116 ) ) ;
#59984 = CARTESIAN_POINT ( 'NONE',  ( 16.96951548583769664, 1409.878878304549971, 192.5990281342199921 ) ) ;
#59983 = VECTOR ( 'NONE', #68087, 1000.000000000000000 ) ;
#59982 = CARTESIAN_POINT ( 'NONE',  ( -10.30849406833070070, 1425.144832954889807, 113.0135162854730027 ) ) ;
#59985 = CARTESIAN_POINT ( 'NONE',  ( 1.717084711415000076, 1516.819260244609950, 211.5980165671369946 ) ) ;
#59986 = CARTESIAN_POINT ( 'NONE',  ( -17.84338787571960339, 1523.481610426287716, 180.3600277896300383 ) ) ;
#59987 = CARTESIAN_POINT ( 'NONE',  ( 21.75649307329755899, 1524.201670966335314, 234.8230823334607749 ) ) ;
#59988 = CARTESIAN_POINT ( 'NONE',  ( -42.47346771400000875, 1432.913526188520109, 263.9447054790979905 ) ) ;
#59989 = CARTESIAN_POINT ( 'NONE',  ( -12.57793359742250061, 1378.943374723730130, 208.9206934522059953 ) ) ;
#59990 = CARTESIAN_POINT ( 'NONE',  ( 18.51436573157379328, 1511.187213306747708, 237.1421867457405881 ) ) ;
#59991 = CARTESIAN_POINT ( 'NONE',  ( 2.612101779301709836, 1508.551704408389924, 214.1066114002470044 ) ) ;
#59992 = CARTESIAN_POINT ( 'NONE',  ( -36.20244804693129481, 1437.512936826869918, 136.5399734142819739 ) ) ;
#59993 = ORIENTED_EDGE ( 'NONE', *, *, #47980, .T. ) ;
#59994 = CARTESIAN_POINT ( 'NONE',  ( 11.89590846401610058, 1396.328474664730038, 207.2763644758680073 ) ) ;
#59995 = CARTESIAN_POINT ( 'NONE',  ( -19.42433358639999952, 1464.716960038490242, 212.6616036344889835 ) ) ;
#59996 = CARTESIAN_POINT ( 'NONE',  ( -16.91389461470000199, 1458.999332487730271, 228.9792524216979928 ) ) ;
#59997 = ORIENTED_EDGE ( 'NONE', *, *, #69995, .F. ) ;
#59998 = ORIENTED_EDGE ( 'NONE', *, *, #89493, .T. ) ;
#59999 = CARTESIAN_POINT ( 'NONE',  ( -2.249657671790000091, 1425.043706724730100, 191.2451905349990113 ) ) ;
#60000 = CARTESIAN_POINT ( 'NONE',  ( -11.78818154252719985, 1426.417843477500128, 148.5075632149639944 ) ) ;
#60001 = CARTESIAN_POINT ( 'NONE',  ( -15.84449006176500241, 1515.383078152259941, 195.2224200989670067 ) ) ;
#60002 = DIRECTION ( 'NONE',  ( 0.000000000000000000, 0.000000000000000000, -1.000000000000000000 ) ) ;
#60003 = DIRECTION ( 'NONE',  ( 0.000000000000000000, 0.000000000000000000, -1.000000000000000000 ) ) ;
#60004 = CARTESIAN_POINT ( 'NONE',  ( 10.70848634212536865, 1506.855035729306792, 228.7236287190453936 ) ) ;
#60005 = CARTESIAN_POINT ( 'NONE',  ( -0.8934505306369999733, 1461.198707732230105, 235.2527420635979638 ) ) ;
#60006 = CARTESIAN_POINT ( 'NONE',  ( 2.322564298810700034, 1421.242547636910103, 183.2407391359299993 ) ) ;
#60007 = AXIS2_PLACEMENT_3D ( 'NONE', #25031, #75483, #14429 ) ;
#60008 = CARTESIAN_POINT ( 'NONE',  ( 10.04570719981230020, 1451.816709674880030, 208.0790574034220128 ) ) ;
#60009 = CARTESIAN_POINT ( 'NONE',  ( -90.07606196291349931, 1384.838993735919985, 292.6108296685719665 ) ) ;
#60010 = VERTEX_POINT ( 'NONE', #524 ) ;
#60011 = CARTESIAN_POINT ( 'NONE',  ( 2.482067860225000366, 1517.099836525840146, 203.3337487049469985 ) ) ;
#60012 = CARTESIAN_POINT ( 'NONE',  ( 0.7533003524100010395, 1516.992029636990083, 209.8620668306199946 ) ) ;
#60013 = ORIENTED_EDGE ( 'NONE', *, *, #4980, .F. ) ;
#60014 = CARTESIAN_POINT ( 'NONE',  ( 11.74616747385230120, 1426.722822852569834, 144.8102584898179828 ) ) ;
#60015 = CARTESIAN_POINT ( 'NONE',  ( 19.45725490719999939, 1497.694397923730094, 228.9812751475980122 ) ) ;
#60016 = EDGE_LOOP ( 'NONE', ( #74275, #94546, #96762, #66025 ) ) ;
#60017 = FACE_OUTER_BOUND ( 'NONE', #52767, .T. ) ;
#60018 = EDGE_CURVE ( 'NONE', #59173, #77352, #104476, .T. ) ;
#60019 = CARTESIAN_POINT ( 'NONE',  ( 7.214567273695688954, 1429.106908498430130, 215.2766334858309847 ) ) ;
#60020 = CARTESIAN_POINT ( 'NONE',  ( 5.089041851490000212, 1509.032960110130034, 237.0857944526979679 ) ) ;
#60021 = AXIS2_PLACEMENT_3D ( 'NONE', #88501, #29136, #81180 ) ;
#60022 =( BOUNDED_CURVE ( )  B_SPLINE_CURVE ( 3, ( #92862, #86128, #84471, #110219 ),
 .UNSPECIFIED., .F., .F. ) 
 B_SPLINE_CURVE_WITH_KNOTS ( ( 4, 4 ),
 ( 2.436781329611987790, 3.141592653589793116 ),
 .UNSPECIFIED. ) 
 CURVE ( )  GEOMETRIC_REPRESENTATION_ITEM ( )  RATIONAL_B_SPLINE_CURVE ( ( 1.000000000000000000, 0.9590300661663092585, 0.9590300661663092585, 1.000000000000000000 ) ) 
 REPRESENTATION_ITEM ( '' )  );
#60023 = CARTESIAN_POINT ( 'NONE',  ( -2.337589116788117760, 1488.423472059833557, 219.7633494153144511 ) ) ;
#60024 = CARTESIAN_POINT ( 'NONE',  ( -4.999592162339999923, 1422.499950720829929, 185.1272544950980148 ) ) ;
#60025 = CARTESIAN_POINT ( 'NONE',  ( -4.291175242752039765, 1446.971469842819943, 154.7965863647420122 ) ) ;
#60026 = CARTESIAN_POINT ( 'NONE',  ( -3.950648164493409720, 1468.310338075048548, 219.6289969960776887 ) ) ;
#60027 = CARTESIAN_POINT ( 'NONE',  ( -4.230274983775188069, 1410.439435280939961, 186.8053085259470549 ) ) ;
#60028 = CARTESIAN_POINT ( 'NONE',  ( -21.14027738949999957, 1379.625625016810091, 209.6601806591559978 ) ) ;
#60029 = CARTESIAN_POINT ( 'NONE',  ( 25.39780210992439891, 1475.101801264620235, 206.2221860197550143 ) ) ;
#60031 = CARTESIAN_POINT ( 'NONE',  ( 7.371950962006430075, 1467.810002177039905, 200.7277130371840030 ) ) ;
#60030 = CARTESIAN_POINT ( 'NONE',  ( 17.69068447980000158, 1457.992677922929943, 229.6631064895979932 ) ) ;
#60032 = CARTESIAN_POINT ( 'NONE',  ( 15.28377178641770051, 1507.620489299410110, 226.2805935727439817 ) ) ;
#60033 = B_SPLINE_SURFACE_WITH_KNOTS ( 'NONE', 5, 5, ( 
 ( #55823, #72087, #106201, #87767, #63679, #13218, #104548, #36796, #37350 ),
 ( #71549, #47408, #105670, #19423, #81530, #4832, #27844, #96145, #2671 ),
 ( #58018, #23826, #91602, #7045, #49070, #83205, #6494, #40646, #14329 ),
 ( #65869, #5393, #107301, #74817, #92696, #108963, #31687, #99989, #41204 ),
 ( #58566, #31137, #32250, #66430, #100546, #48518, #82092, #83750, #107848 ),
 ( #108405, #15425, #40094, #92153, #15972, #49617, #50174, #84301, #38979 ) ),
 .UNSPECIFIED., .F., .F., .F.,
 ( 6, 6 ),
 ( 6, 3, 6 ),
 ( 0.4666582264940000169, 2.797885342366120298 ),
 ( -1.082960611691029974E-05, 1.000000000000000000, 2.000000000000000000 ),
 .UNSPECIFIED. ) ;
#60034 = CARTESIAN_POINT ( 'NONE',  ( -5.655232455200980723, 1423.184742756340029, 101.0239091077149993 ) ) ;
#60035 = VERTEX_POINT ( 'NONE', #10001 ) ;
#60036 = DIRECTION ( 'NONE',  ( 0.4978433412588676998, 0.000000000000000000, -0.8672669759446663962 ) ) ;
#60037 = EDGE_CURVE ( 'NONE', #63956, #14535, #68686, .T. ) ;
#60038 = CARTESIAN_POINT ( 'NONE',  ( 1.114056763157479590, 1516.634548230098289, 216.8335026655383899 ) ) ;
#60039 = CARTESIAN_POINT ( 'NONE',  ( -2.933872690221072776, 1485.132197629912071, 183.0775065428524329 ) ) ;
#60040 = DIRECTION ( 'NONE',  ( -1.065814103640150437E-14, 0.000000000000000000, 1.000000000000000000 ) ) ;
#60042 = VERTEX_POINT ( 'NONE', #71052 ) ;
#60041 = CARTESIAN_POINT ( 'NONE',  ( 1.384206944075679901, 1515.080800108599988, 204.7928163502200221 ) ) ;
#60043 = CARTESIAN_POINT ( 'NONE',  ( 0.7353240777269999251, 1489.474306033429912, 187.1311076040980197 ) ) ;
#60044 = CARTESIAN_POINT ( 'NONE',  ( -0.9490323356140020206, 1507.925252277690106, 221.0232043775990007 ) ) ;
#60045 = EDGE_CURVE ( 'NONE', #97701, #88321, #19496, .T. ) ;
#60046 = CARTESIAN_POINT ( 'NONE',  ( -11.82947776570000009, 1429.869038498530244, 149.4074658875980219 ) ) ;
#60047 = CARTESIAN_POINT ( 'NONE',  ( -10.81518761075750135, 1424.921099531289883, 144.1705495212430037 ) ) ;
#60048 = CARTESIAN_POINT ( 'NONE',  ( -11.03313129935749792, 1462.309928051650104, 209.2979651268820191 ) ) ;
#60049 = CARTESIAN_POINT ( 'NONE',  ( 16.82545552545150258, 1509.500615784180127, 233.4982582598109957 ) ) ;
#60050 = CARTESIAN_POINT ( 'NONE',  ( -3.812371247207599900, 1428.459941768050157, 200.5740418269730014 ) ) ;
#60051 = CARTESIAN_POINT ( 'NONE',  ( -15.19327425026499867, 1512.300546902530186, 221.9778556009669899 ) ) ;
#60052 = CARTESIAN_POINT ( 'NONE',  ( 4.257623127619999615, 1479.092245966489827, 202.6254196850889855 ) ) ;
#60054 = CARTESIAN_POINT ( 'NONE',  ( -10.44175186412380008, 1480.437295940329932, 207.7252335065300031 ) ) ;
#60053 = CARTESIAN_POINT ( 'NONE',  ( -21.63817346260000107, 1508.012227572530037, 226.7581651977980073 ) ) ;
#60055 = CARTESIAN_POINT ( 'NONE',  ( -16.16654775127000221, 1459.157660042964153, 229.6201166687930026 ) ) ;
#60056 = EDGE_LOOP ( 'NONE', ( #62740, #46500, #4507, #74648 ) ) ;
#60057 = CARTESIAN_POINT ( 'NONE',  ( -4.043990345725000601, 1516.983612918759945, 206.6425990843970055 ) ) ;
#60058 = CARTESIAN_POINT ( 'NONE',  ( 27.07453441790000070, 1412.356090134630222, 267.2274653296979636 ) ) ;
#60059 = CARTESIAN_POINT ( 'NONE',  ( 24.54015759500000016, 1436.582034297039854, 138.9799141002980036 ) ) ;
#60060 = B_SPLINE_CURVE_WITH_KNOTS ( 'NONE', 3,
 ( #56389, #83231, #82684, #23311 ),
 .UNSPECIFIED., .F., .F.,
 ( 4, 4 ),
 ( 0.000000000000000000, 0.0002960034161023854899 ),
 .UNSPECIFIED. ) ;
#60061 = CARTESIAN_POINT ( 'NONE',  ( 23.23294983419999937, 1430.294683446630188, 204.9340936284079930 ) ) ;
#60062 = CARTESIAN_POINT ( 'NONE',  ( -0.1035247606053459890, 1508.569086740290004, 237.9121964778769893 ) ) ;
#60063 = AXIS2_PLACEMENT_3D ( 'NONE', #4910, #29560, #107371 ) ;
#60064 = CARTESIAN_POINT ( 'NONE',  ( 9.814762245626701187, 1424.216260739349764, 144.1582897308169890 ) ) ;
#60065 = CARTESIAN_POINT ( 'NONE',  ( -41.52520403286720807, 1442.071982413179967, 135.9507581816680215 ) ) ;
#60066 = ADVANCED_FACE ( 'NONE', ( #53698 ), #39354, .F. ) ;
#60067 = DIRECTION ( 'NONE',  ( 0.03489949670250328678, -0.9993908270190956511, 0.000000000000000000 ) ) ;
#60068 = CARTESIAN_POINT ( 'NONE',  ( -14.38020684849999853, 1416.780301525639970, 203.5793783887689870 ) ) ;
#60069 = CARTESIAN_POINT ( 'NONE',  ( -13.68074494839999922, 1444.567011418389939, 188.0766381524979920 ) ) ;
#60070 = CARTESIAN_POINT ( 'NONE',  ( -6.025152189795589308, 1484.743689720570046, 198.8560543189699956 ) ) ;
#60071 = B_SPLINE_SURFACE_WITH_KNOTS ( 'NONE', 5, 1, ( 
 ( #78115, #78676 ),
 ( #87074, #93791 ),
 ( #18743, #61357 ),
 ( #103295, #337 ),
 ( #42874, #9268 ),
 ( #95476, #104980 ),
 ( #103872, #94924 ),
 ( #10359, #27172 ),
 ( #1419, #70312 ),
 ( #1993, #70867 ),
 ( #69189, #52937 ),
 ( #26602, #26036 ),
 ( #85968, #44531 ),
 ( #36128, #104425 ),
 ( #17626, #77031 ),
 ( #85396, #35559 ),
 ( #34464, #68640 ),
 ( #35008, #27718 ),
 ( #52394, #102740 ),
 ( #60229, #94348 ),
 ( #60799, #61905 ),
 ( #96023, #69754 ),
 ( #36674, #8693 ),
 ( #19294, #10925 ),
 ( #885, #51263 ),
 ( #51831, #43976 ),
 ( #45101, #79241 ),
 ( #86517, #2549 ),
 ( #43428, #17066 ),
 ( #77577, #28269 ),
 ( #18197, #80883 ),
 ( #107175, #3652 ),
 ( #37781, #81402 ),
 ( #4714, #46752 ),
 ( #97676, #21490 ),
 ( #55702, #37229 ),
 ( #80335, #55154 ),
 ( #22034, #106620 ),
 ( #54060, #4179 ),
 ( #71970, #73600 ),
 ( #63026, #73036 ),
 ( #45655, #38858 ),
 ( #89823, #38312 ),
 ( #47829, #13639 ),
 ( #30467, #90361 ),
 ( #64653, #106082 ),
 ( #97131, #81962 ),
 ( #20400, #98772 ),
 ( #11479, #56231 ),
 ( #107730, #5268 ),
 ( #54605, #88737 ) ),
 .UNSPECIFIED., .F., .F., .F.,
 ( 6, 3, 3, 3, 3, 3, 3, 3, 3, 3, 3, 3, 3, 3, 3, 3, 6 ),
 ( 2, 2 ),
 ( 0.000000000000000000, 28.69702819429999963, 61.04778752440000034, 93.62768910810000023, 123.7336603250000024, 156.1762685979999787, 187.3272846180000215, 220.4669312460000015, 237.3878297990000021, 254.2938300590000154, 289.2398204710000300, 325.3030936050000150, 360.8626869010000178, 395.8828220460000011, 432.6128460950000090, 468.8934854820000169, 502.1482307969999965 ),
 ( -1.776356839400000001E-15, 2.001700839520000219 ),
 .UNSPECIFIED. ) ;
#60072 = CARTESIAN_POINT ( 'NONE',  ( -16.25590069084343270, 1419.722612204563575, 209.8386441428618809 ) ) ;
#60073 = CARTESIAN_POINT ( 'NONE',  ( 44.93136303390000563, 1440.913033067569813, 269.6838066906980202 ) ) ;
#60074 = ORIENTED_EDGE ( 'NONE', *, *, #27629, .T. ) ;
#60075 = CARTESIAN_POINT ( 'NONE',  ( 1.460943697043280087, 1495.022397442580086, 181.6406806417639928 ) ) ;
#60076 = CARTESIAN_POINT ( 'NONE',  ( -12.13599495486779922, 1409.336858669690173, 200.3964593173120079 ) ) ;
#60077 = CARTESIAN_POINT ( 'NONE',  ( -11.40049322445420010, 1508.551708765010062, 208.9769759148800006 ) ) ;
#60078 = CARTESIAN_POINT ( 'NONE',  ( -12.16766253904543582, 1377.701433628964878, 210.9975495011200053 ) ) ;
#60079 = CARTESIAN_POINT ( 'NONE',  ( -9.853196041699998631, 1474.808872623229945, 269.2594982597980220 ) ) ;
#60080 = CARTESIAN_POINT ( 'NONE',  ( -18.83642247210000065, 1444.248298674089938, 209.1218459616989946 ) ) ;
#60081 = CARTESIAN_POINT ( 'NONE',  ( -12.24389445090430328, 1513.118416466450981, 192.4462725802613932 ) ) ;
#60082 = CARTESIAN_POINT ( 'NONE',  ( -24.14770755569024985, 1444.491430425563976, 211.6499922375425058 ) ) ;
#60083 = CARTESIAN_POINT ( 'NONE',  ( -81.23110265244889661, 1384.636034499739935, 304.6366948209559951 ) ) ;
#60084 = CARTESIAN_POINT ( 'NONE',  ( 13.58235846979999906, 1416.828040475229955, 196.3349388281980055 ) ) ;
#60085 = CARTESIAN_POINT ( 'NONE',  ( 11.78977346136659854, 1415.441076448360036, 223.1097579672979805 ) ) ;
#60086 = DIRECTION ( 'NONE',  ( -0.6736849260863841948, 0.000000000000000000, 0.7390186874254148774 ) ) ;
#60087 = DIRECTION ( 'NONE',  ( 1.755985294532464991E-16, -1.000000000000000000, 1.338183447452830017E-16 ) ) ;
#60088 = CARTESIAN_POINT ( 'NONE',  ( -1.438891081339280120, 1452.191228260170192, 183.8587004481619829 ) ) ;
#60089 = AXIS2_PLACEMENT_3D ( 'NONE', #95877, #19141, #104833 ) ;
#60090 = CARTESIAN_POINT ( 'NONE',  ( -23.20723499460000028, 1410.644907069029841, 205.4415377791680157 ) ) ;
#60091 = CARTESIAN_POINT ( 'NONE',  ( 13.49734317350000090, 1415.088275290029969, 197.3807697222979982 ) ) ;
#60092 = CARTESIAN_POINT ( 'NONE',  ( 3.584507579370000308, 1486.500509928790052, 219.3043344553989868 ) ) ;
#60093 = CARTESIAN_POINT ( 'NONE',  ( 10.52840799775919933, 1481.199580776819857, 208.2609754401459838 ) ) ;
#60094 = CARTESIAN_POINT ( 'NONE',  ( -5.086186302109790169, 1453.993515012390162, 204.7329997213950037 ) ) ;
#60095 = CARTESIAN_POINT ( 'NONE',  ( -8.029654524079999689, 1440.425766428789757, 228.7538251570989871 ) ) ;
#60096 = CARTESIAN_POINT ( 'NONE',  ( 17.53714238134822168, 1524.871836253779975, 180.8013275667260871 ) ) ;
#60097 = CARTESIAN_POINT ( 'NONE',  ( -3.540693220810990471, 1508.270056219510025, 180.7688429917959922 ) ) ;
#60099 = CARTESIAN_POINT ( 'NONE',  ( -8.920215095379999681, 1384.216085512750169, 199.9962620032089831 ) ) ;
#60098 = CARTESIAN_POINT ( 'NONE',  ( 13.92686551478569967, 1517.051704405520013, 192.0624604828410043 ) ) ;
#60100 = CARTESIAN_POINT ( 'NONE',  ( 11.73499481921169973, 1426.697258569849964, 144.0242909167239986 ) ) ;
#60101 = CARTESIAN_POINT ( 'NONE',  ( 0.3722769099684289928, 1457.826255237599980, 228.9731060096619899 ) ) ;
#60102 = CARTESIAN_POINT ( 'NONE',  ( -10.90735812309999986, 1491.858081601189951, 210.7852297805490025 ) ) ;
#60103 = CARTESIAN_POINT ( 'NONE',  ( 8.291572064590001290, 1449.377284184440214, 202.9263957419950088 ) ) ;
#60104 = CARTESIAN_POINT ( 'NONE',  ( -0.06979898363973670306, 1408.910622953150096, 223.8076866964610190 ) ) ;
#60105 = CARTESIAN_POINT ( 'NONE',  ( 6.550389432124999800, 1516.755758396839838, 204.1155163507169732 ) ) ;
#60106 = CARTESIAN_POINT ( 'NONE',  ( -6.899998715920828474, 1398.118124432348850, 220.1627551181343563 ) ) ;
#60107 = CARTESIAN_POINT ( 'NONE',  ( 14.96231789283499936, 1514.242353506929931, 193.9066102308669883 ) ) ;
#60108 = CARTESIAN_POINT ( 'NONE',  ( 5.830794567472060486, 1434.584590126570220, 226.6688182991929921 ) ) ;
#60109 = CARTESIAN_POINT ( 'NONE',  ( -19.05511642929999994, 1449.657101504390084, 193.8129821119980249 ) ) ;
#60110 = CARTESIAN_POINT ( 'NONE',  ( 9.463244449160031380, 1503.982580522659873, 216.1976177253470155 ) ) ;
#60111 = CARTESIAN_POINT ( 'NONE',  ( 41.61763030636900140, 1445.085476029980100, 135.5083515819240176 ) ) ;
#60113 = ORIENTED_EDGE ( 'NONE', *, *, #74024, .T. ) ;
#60112 = CARTESIAN_POINT ( 'NONE',  ( -64.37783753600000125, 1379.747207013510206, 273.6112401810589745 ) ) ;
#60114 = ORIENTED_EDGE ( 'NONE', *, *, #40518, .F. ) ;
#60115 = CARTESIAN_POINT ( 'NONE',  ( 11.94595818812160104, 1433.509642704729913, 149.8900677580190006 ) ) ;
#60116 = CARTESIAN_POINT ( 'NONE',  ( 21.08095450301371088, 1525.506916460680713, 184.0391914173981149 ) ) ;
#60117 = VERTEX_POINT ( 'NONE', #98957 ) ;
#60118 = CARTESIAN_POINT ( 'NONE',  ( -107.1765804579999894, 1378.913059918550061, 307.8836185913590384 ) ) ;
#60119 = CARTESIAN_POINT ( 'NONE',  ( -10.35066018003379895, 1448.307506586269938, 208.4121118022800090 ) ) ;
#60120 = CARTESIAN_POINT ( 'NONE',  ( -8.606575390850000673, 1385.345214380770130, 218.6410135246489972 ) ) ;
#60122 = LINE ( 'NONE', #96467, #48671 ) ;
#60121 = CARTESIAN_POINT ( 'NONE',  ( 16.06157012919580040, 1423.788481394339897, 191.1175312021059938 ) ) ;
#60123 = CARTESIAN_POINT ( 'NONE',  ( 8.271109682960839038, 1498.104299293129998, 234.5502916224329795 ) ) ;
#60124 = B_SPLINE_CURVE_WITH_KNOTS ( 'NONE', 5,
 ( #8191, #42357, #93848, #110116, #76511, #94397 ),
 .UNSPECIFIED., .F., .F.,
 ( 6, 6 ),
 ( -2.000000000000000000, -2.672797316805031187E-08 ),
 .UNSPECIFIED. ) ;
#60125 = CARTESIAN_POINT ( 'NONE',  ( 6.753106024830000109, 1507.635313380530079, 182.4733158664980124 ) ) ;
#60126 = CARTESIAN_POINT ( 'NONE',  ( 3.135856758649999687, 1466.984112829190053, 218.9566971792889944 ) ) ;
#60127 = CARTESIAN_POINT ( 'NONE',  ( -24.56899124258660194, 1444.772254235220089, 210.9323875608310175 ) ) ;
#60128 = CARTESIAN_POINT ( 'NONE',  ( 1.717084711415000076, 1516.819260244609950, 211.5980165671369946 ) ) ;
#60129 = CARTESIAN_POINT ( 'NONE',  ( 0.2669485111002459776, 1395.922382434750034, 198.1227973212599807 ) ) ;
#60130 = CARTESIAN_POINT ( 'NONE',  ( 11.57170172580000056, 1431.970351487809921, 151.1874232329979861 ) ) ;
#60131 = CARTESIAN_POINT ( 'NONE',  ( 7.532473168254999685, 1513.265135866630089, 201.8177576823970014 ) ) ;
#60132 = ORIENTED_EDGE ( 'NONE', *, *, #82845, .F. ) ;
#60133 = CARTESIAN_POINT ( 'NONE',  ( 13.76019309406060032, 1436.072204996710070, 150.3335515433649903 ) ) ;
#60134 = ORIENTED_EDGE ( 'NONE', *, *, #55101, .F. ) ;
#60135 = ORIENTED_EDGE ( 'NONE', *, *, #38481, .T. ) ;
#60136 = CARTESIAN_POINT ( 'NONE',  ( 13.02399213288301105, 1444.859346537102965, 169.4177112119271271 ) ) ;
#60137 = CARTESIAN_POINT ( 'NONE',  ( -1.466394352250000255, 1466.280833669130061, 235.4455910585979836 ) ) ;
#60138 = CARTESIAN_POINT ( 'NONE',  ( 3.415238410854999795, 1511.801704408389924, 204.7069501962670017 ) ) ;
#60139 = CARTESIAN_POINT ( 'NONE',  ( 2.291676273424999799, 1516.534976163889951, 216.4430396779769978 ) ) ;
#60140 = CARTESIAN_POINT ( 'NONE',  ( -8.184208294724300004, 1511.478961034980102, 213.0871669047343175 ) ) ;
#60141 = CARTESIAN_POINT ( 'NONE',  ( -19.07569465070004711, 1442.225521153744921, 210.5149903700299205 ) ) ;
#60142 = CARTESIAN_POINT ( 'NONE',  ( -35.68475374490700602, 1379.642202425360210, 218.6381764093407867 ) ) ;
#60143 = CARTESIAN_POINT ( 'NONE',  ( -25.65041448810000091, 1380.250345454750004, 213.2122020707489867 ) ) ;
#60144 = ORIENTED_EDGE ( 'NONE', *, *, #45240, .T. ) ;
#60145 = CARTESIAN_POINT ( 'NONE',  ( 7.709681268295000223, 1516.559109716219837, 206.2491454149069909 ) ) ;
#60146 = ORIENTED_EDGE ( 'NONE', *, *, #70639, .T. ) ;
#60147 = CARTESIAN_POINT ( 'NONE',  ( 22.55659962669360041, 1440.913060387330006, 229.8770814074250097 ) ) ;
#60148 = CARTESIAN_POINT ( 'NONE',  ( -18.87980335319999625, 1507.654596516530091, 229.6982590054979880 ) ) ;
#60149 = ORIENTED_EDGE ( 'NONE', *, *, #17901, .T. ) ;
#60150 = CARTESIAN_POINT ( 'NONE',  ( -5.656834581150000041, 1409.110601402830071, 188.1059135931980109 ) ) ;
#60151 = CARTESIAN_POINT ( 'NONE',  ( 7.891962413025000345, 1514.771170611759999, 215.1394100340270086 ) ) ;
#60153 = ORIENTED_EDGE ( 'NONE', *, *, #97397, .T. ) ;
#60152 = CARTESIAN_POINT ( 'NONE',  ( -3.392699880776999688, 1433.356438688929984, 218.0666730085999916 ) ) ;
#60154 = CARTESIAN_POINT ( 'NONE',  ( 23.72977224379999583, 1434.259526396529964, 214.5256004728379935 ) ) ;
#60155 = CARTESIAN_POINT ( 'NONE',  ( -17.32634609470520104, 1508.551704408389924, 210.3986788274449680 ) ) ;
#60156 = CARTESIAN_POINT ( 'NONE',  ( -4.019837105682418255, 1515.589591810382899, 208.5006405197344179 ) ) ;
#60157 = LINE ( 'NONE', #75846, #64264 ) ;
#60158 = CARTESIAN_POINT ( 'NONE',  ( 21.19880661589004589, 1524.382868172863937, 184.6948938244647991 ) ) ;
#60159 = B_SPLINE_CURVE_WITH_KNOTS ( 'NONE', 3,
 ( #93922, #87198, #69315, #44101, #84969, #96146, #78239, #95048 ),
 .UNSPECIFIED., .F., .F.,
 ( 4, 2, 2, 4 ),
 ( 0.000000000000000000, 0.001073044933456263018, 0.001609567400184377722, 0.002146089866912492643 ),
 .UNSPECIFIED. ) ;
#60160 = CARTESIAN_POINT ( 'NONE',  ( 5.781490544344999982, 1516.807958722750072, 215.6734893570070142 ) ) ;
#60161 = CARTESIAN_POINT ( 'NONE',  ( -3.101981640767989656, 1428.864138099600041, 200.2836557281250123 ) ) ;
#60162 = STYLED_ITEM ( 'NONE', ( #969 ), #7937 ) ;
#60163 = CARTESIAN_POINT ( 'NONE',  ( 6.089577284407799773, 1511.778877376279979, 217.5949564134380125 ) ) ;
#60164 = AXIS2_PLACEMENT_3D ( 'NONE', #3355, #87902, #26872 ) ;
#60165 = ADVANCED_FACE ( 'NONE', ( #107367 ), #48326, .T. ) ;
#60166 = CARTESIAN_POINT ( 'NONE',  ( 22.04555908422425148, 1524.082740465118832, 184.4798216974346872 ) ) ;
#60167 = CARTESIAN_POINT ( 'NONE',  ( -0.7350232362959980836, 1516.970035769810011, 211.4194755912870107 ) ) ;
#60168 = CARTESIAN_POINT ( 'NONE',  ( -11.85859649436589969, 1482.110477596389956, 208.2678370658890117 ) ) ;
#60169 = CARTESIAN_POINT ( 'NONE',  ( -17.45339170113992822, 1486.143972108528942, 188.0383730386266450 ) ) ;
#60170 = B_SPLINE_CURVE_WITH_KNOTS ( 'NONE', 5,
 ( #2425, #105406, #63435, #44970, #11897, #82257, #108561, #82804, #11357, #6098, #108001, #5558, #53365, #39707, #19734, #57083, #28698, #80203, #88616, #74435, #70740, #28139, #48681, #31851, #55022, #53935, #37645 ),
 .UNSPECIFIED., .F., .F.,
 ( 6, 3, 3, 3, 3, 3, 3, 3, 6 ),
 ( 0.000000000000000000, 0.06058382609222391635, 0.1069330941294720783, 0.1211676521844478327, 0.1797127176077684407, 0.2382577830310894373, 0.3553479138777306812, 0.6482918569636776374, 1.000000000000000000 ),
 .UNSPECIFIED. ) ;
#60172 = EDGE_LOOP ( 'NONE', ( #79248, #62152, #82111, #15883 ) ) ;
#60171 = CARTESIAN_POINT ( 'NONE',  ( -98.86683315710000386, 1385.218296336320009, 296.2584199137589849 ) ) ;
#60173 = CARTESIAN_POINT ( 'NONE',  ( -57.94198640639650222, 1385.076618372680059, 277.3417116979370007 ) ) ;
#60174 = CARTESIAN_POINT ( 'NONE',  ( 16.98089203389999824, 1467.669754651430139, 255.1565212655980019 ) ) ;
#60175 = EDGE_CURVE ( 'NONE', #27879, #101391, #55156, .T. ) ;
#60176 = CARTESIAN_POINT ( 'NONE',  ( 2.108362890389359645, 1452.419099747896553, 183.6319488572359262 ) ) ;
#60177 = CARTESIAN_POINT ( 'NONE',  ( -7.548872338225000256, 1510.418062979269962, 214.3032561208869993 ) ) ;
#60178 = CARTESIAN_POINT ( 'NONE',  ( -7.828230685879998596, 1507.298741238030061, 235.3518363426980216 ) ) ;
#60179 = CARTESIAN_POINT ( 'NONE',  ( -23.94933866970000125, 1445.534750183129972, 212.9709028766179983 ) ) ;
#60180 = B_SPLINE_CURVE_WITH_KNOTS ( 'NONE', 3,
 ( #32772, #48499, #50684, #57459, #31668, #65849, #82639, #15408, #49597, #83730, #75889, #49051, #91586, #41182, #109495 ),
 .UNSPECIFIED., .F., .F.,
 ( 4, 2, 2, 1, 1, 1, 2, 2, 4 ),
 ( 0.000000000000000000, 0.2500000000000353051, 0.3750000000000530687, 0.4375000000000631162, 0.4687500000000695000, 0.4843750000000723865, 0.4921875000000711098, 0.5000000000000698330, 1.000000000000000000 ),
 .UNSPECIFIED. ) ;
#60182 = CARTESIAN_POINT ( 'NONE',  ( 17.89017687474920137, 1410.330682765429856, 222.8911238419379970 ) ) ;
#60181 = PLANE ( 'NONE',  #1810 ) ;
#60183 = DIRECTION ( 'NONE',  ( 0.000000000000000000, 0.000000000000000000, -1.000000000000000000 ) ) ;
#60184 = CARTESIAN_POINT ( 'NONE',  ( -108.7025099737439859, 1381.872732176050022, 310.6179191028680293 ) ) ;
#60185 = ORIENTED_EDGE ( 'NONE', *, *, #83387, .F. ) ;
#60186 = CARTESIAN_POINT ( 'NONE',  ( 2.867803626105000170, 1516.994127245590107, 204.4971090729170271 ) ) ;
#60187 = CARTESIAN_POINT ( 'NONE',  ( 0.3396692986610000409, 1405.750286565129954, 267.5371225631980110 ) ) ;
#60188 = CARTESIAN_POINT ( 'NONE',  ( 24.51495038730000076, 1443.562157032569758, 213.8565503907379934 ) ) ;
#60189 = DIRECTION ( 'NONE',  ( -0.1652739736738010612, 0.3722510636888851088, 0.9132982312522922586 ) ) ;
#60190 = CARTESIAN_POINT ( 'NONE',  ( 3.712013955199999771, 1466.291930614589774, 219.5294839965989979 ) ) ;
#60191 = CARTESIAN_POINT ( 'NONE',  ( 2.144000416237634266, 1468.703099310448806, 218.9077027719663704 ) ) ;
#60192 = CARTESIAN_POINT ( 'NONE',  ( 27.60464170112659943, 1435.621481315979963, 136.1400934894720081 ) ) ;
#60193 = DIRECTION ( 'NONE',  ( 1.755985294532469921E-16, -1.000000000000000000, 1.338183447452831989E-16 ) ) ;
#60194 = CARTESIAN_POINT ( 'NONE',  ( 3.286444981498850021E-15, 1458.388061309670093, 231.5054671141039933 ) ) ;
#60195 = CARTESIAN_POINT ( 'NONE',  ( -1.766639101469999806, 1429.583277275290129, 199.8949488872989946 ) ) ;
#60196 = CARTESIAN_POINT ( 'NONE',  ( 11.60840177515349936, 1480.119960163069891, 211.2000821351769844 ) ) ;
#60197 = B_SPLINE_CURVE_WITH_KNOTS ( 'NONE', 5,
 ( #7003, #49579, #108919, #102556, #72311, #79607, #61714, #87448, #38130, #28635, #53876, #19671, #71222, #29725, #105906, #2911, #63376, #54958 ),
 .UNSPECIFIED., .F., .F.,
 ( 6, 3, 3, 3, 3, 6 ),
 ( 0.000000000000000000, 0.04383986791751091211, 0.1036123950753678191, 0.2231574493812304161, 0.6694723481587087077, 1.000000000000000000 ),
 .UNSPECIFIED. ) ;
#60198 = CARTESIAN_POINT ( 'NONE',  ( 18.66420869458043441, 1526.382868172864164, 185.4599087859680537 ) ) ;
#60199 = DIRECTION ( 'NONE',  ( 0.9455185755993178454, 0.000000000000000000, -0.3255681544571539243 ) ) ;
#60200 = VERTEX_POINT ( 'NONE', #3654 ) ;
#60201 = CARTESIAN_POINT ( 'NONE',  ( 0.8041763403130000043, 1426.566393376330097, 144.1938086916980239 ) ) ;
#60202 = CARTESIAN_POINT ( 'NONE',  ( 12.91344045910000027, 1434.774313861569908, 146.5970547348979949 ) ) ;
#60203 = CARTESIAN_POINT ( 'NONE',  ( -4.429773136856780091, 1508.551704408389924, 213.9240780803189921 ) ) ;
#60204 = CARTESIAN_POINT ( 'NONE',  ( 15.64943080881179682, 1466.933481671390155, 189.3680284421589874 ) ) ;
#60205 = CARTESIAN_POINT ( 'NONE',  ( -0.2950133488750000255, 1415.766390753429960, 233.4435486769980059 ) ) ;
#60207 = CARTESIAN_POINT ( 'NONE',  ( -11.20330708994425883, 1469.676918551309882, 192.3606680380646878 ) ) ;
#60206 = CARTESIAN_POINT ( 'NONE',  ( 11.49286327549999953, 1502.439553125990187, 208.8615115388970196 ) ) ;
#60208 = CARTESIAN_POINT ( 'NONE',  ( -28.78960605939999695, 1509.588732895030262, 209.8024020300809980 ) ) ;
#60209 = CARTESIAN_POINT ( 'NONE',  ( 8.617375305610000424, 1422.946414101140135, 212.6945960971789873 ) ) ;
#60210 = CARTESIAN_POINT ( 'NONE',  ( -10.00342135130719967, 1384.890128760720017, 218.7594294872120031 ) ) ;
#60211 = AXIS2_PLACEMENT_3D ( 'NONE', #2805, #104682, #78954 ) ;
#60212 = CARTESIAN_POINT ( 'NONE',  ( -8.506922781476685458, 1417.327140144819396, 230.7140993806030735 ) ) ;
#60213 = CARTESIAN_POINT ( 'NONE',  ( -15.06028995570763840, 1451.149887921017580, 149.6833329127408092 ) ) ;
#60214 = CARTESIAN_POINT ( 'NONE',  ( -6.858322662029999961, 1484.305021930289968, 199.8403620220989865 ) ) ;
#60215 = CARTESIAN_POINT ( 'NONE',  ( 25.21992779760000047, 1436.607954016930080, 137.5621431200979998 ) ) ;
#60216 = CARTESIAN_POINT ( 'NONE',  ( -9.843170653638850354, 1396.256791483090183, 204.0667884097820206 ) ) ;
#60217 = EDGE_LOOP ( 'NONE', ( #102823, #43582, #15442, #87411 ) ) ;
#60218 = FACE_OUTER_BOUND ( 'NONE', #22219, .T. ) ;
#60219 = CARTESIAN_POINT ( 'NONE',  ( 4.915203104360000630, 1434.541746329560056, 150.1320020560979742 ) ) ;
#60220 = ORIENTED_EDGE ( 'NONE', *, *, #106249, .F. ) ;
#60221 = ORIENTED_EDGE ( 'NONE', *, *, #45529, .F. ) ;
#60222 = CARTESIAN_POINT ( 'NONE',  ( 2.262995014779219716, 1435.360232108469972, 227.4353352697579851 ) ) ;
#60223 = CARTESIAN_POINT ( 'NONE',  ( 7.170479361814977359, 1516.544351102706287, 206.9184616573184314 ) ) ;
#60225 = CARTESIAN_POINT ( 'NONE',  ( -0.1159644321946630141, 1457.025002160060012, 219.7504842676799797 ) ) ;
#60224 = CARTESIAN_POINT ( 'NONE',  ( 10.40857034289999916, 1425.394460820129780, 96.53362461269790629 ) ) ;
#60226 = CARTESIAN_POINT ( 'NONE',  ( -11.62902870529999966, 1433.064885913230000, 151.0294648830980009 ) ) ;
#60227 = CARTESIAN_POINT ( 'NONE',  ( -2.863573784786321408, 1419.688340288614654, 186.1810135818298875 ) ) ;
#60228 = CARTESIAN_POINT ( 'NONE',  ( 7.314450557279999821, 1425.029284243300026, 212.6285264488790006 ) ) ;
#60229 = CARTESIAN_POINT ( 'NONE',  ( 18.68390456929999743, 1457.534965338390066, 220.6831945507989872 ) ) ;
#60230 = CARTESIAN_POINT ( 'NONE',  ( 8.149343875210002253, 1509.018734359930249, 181.8702896482980123 ) ) ;
#60231 = CARTESIAN_POINT ( 'NONE',  ( 3.933035305499999801, 1449.187059537480081, 184.2601159103979853 ) ) ;
#60232 = CARTESIAN_POINT ( 'NONE',  ( 7.999617675857605192, 1364.906918534513807, 209.6218459617148824 ) ) ;
#60234 = ORIENTED_EDGE ( 'NONE', *, *, #21920, .F. ) ;
#60233 = CARTESIAN_POINT ( 'NONE',  ( 31.92108011125342770, 1511.187213306747708, 197.2845127572061301 ) ) ;
#60235 = EDGE_LOOP ( 'NONE', ( #4483, #29386, #49065, #46799 ) ) ;
#60236 = CARTESIAN_POINT ( 'NONE',  ( -41.65674268029999894, 1443.992461967939789, 135.6790812281979868 ) ) ;
#60237 = ADVANCED_FACE ( 'NONE', ( #19296 ), #63563, .T. ) ;
#60238 = DIRECTION ( 'NONE',  ( 0.000000000000000000, 0.000000000000000000, 1.000000000000000000 ) ) ;
#60239 = CARTESIAN_POINT ( 'NONE',  ( -2.002811041570000088E-09, 1473.589435999130046, 270.3925729408980487 ) ) ;
#60240 = DIRECTION ( 'NONE',  ( 0.000000000000000000, 0.000000000000000000, 1.000000000000000000 ) ) ;
#60241 = FACE_OUTER_BOUND ( 'NONE', #74571, .T. ) ;
#60243 = EDGE_CURVE ( 'NONE', #87891, #81034, #98222, .T. ) ;
#60242 = LINE ( 'NONE', #70327, #28619 ) ;
#60244 = CARTESIAN_POINT ( 'NONE',  ( 1.035878012497590150, 1476.011601096869981, 197.6942168356959826 ) ) ;
#60245 = CARTESIAN_POINT ( 'NONE',  ( -33.91368077465119768, 1451.728768558339880, 134.7155154936840233 ) ) ;
#60246 = EDGE_CURVE ( 'NONE', #104782, #105791, #34856, .T. ) ;
#60247 =( NAMED_UNIT ( * ) SI_UNIT ( $, .STERADIAN. ) SOLID_ANGLE_UNIT ( ) );
#60248 = CARTESIAN_POINT ( 'NONE',  ( -22.62861454470000311, 1507.212883763329955, 208.5231287359179930 ) ) ;
#60249 = CARTESIAN_POINT ( 'NONE',  ( 9.231361398833680454, 1366.659448741839924, 210.6218459616991936 ) ) ;
#60250 = CARTESIAN_POINT ( 'NONE',  ( 9.688704068493601440, 1409.071838889859919, 198.0917906310850185 ) ) ;
#60251 = CARTESIAN_POINT ( 'NONE',  ( -10.60628234125749891, 1406.913721737060087, 266.9166020718200230 ) ) ;
#60252 = CARTESIAN_POINT ( 'NONE',  ( -13.71031927006879947, 1434.974885213249991, 148.6196309992409965 ) ) ;
#60253 = ORIENTED_EDGE ( 'NONE', *, *, #37884, .T. ) ;
#60254 = CARTESIAN_POINT ( 'NONE',  ( 3.500614145640000174, 1441.116913297490100, 218.4019928104889914 ) ) ;
#60255 = CARTESIAN_POINT ( 'NONE',  ( 13.66368654969999952, 1443.423569391949968, 188.9472448265979949 ) ) ;
#60256 = VERTEX_POINT ( 'NONE', #10927 ) ;
#60257 = VERTEX_POINT ( 'NONE', #70869 ) ;
#60258 = CARTESIAN_POINT ( 'NONE',  ( -22.12758967992428794, 1506.606278687006125, 209.0267225037276830 ) ) ;
#60259 = CARTESIAN_POINT ( 'NONE',  ( -21.19077256501192608, 1525.394081235439444, 183.9650388928959615 ) ) ;
#60260 = CARTESIAN_POINT ( 'NONE',  ( 5.008848199894999631, 1516.858456333729919, 214.1219297979669989 ) ) ;
#60261 = CARTESIAN_POINT ( 'NONE',  ( -14.43173846279999850, 1485.481767227229966, 186.7711707502979834 ) ) ;
#60262 = B_SPLINE_CURVE_WITH_KNOTS ( 'NONE', 3,
 ( #98852, #23787, #82044, #99945 ),
 .UNSPECIFIED., .F., .F.,
 ( 4, 4 ),
 ( 0.000000000000000000, 0.0002220129587134776663 ),
 .UNSPECIFIED. ) ;
#60263 = B_SPLINE_CURVE_WITH_KNOTS ( 'NONE', 3,
 ( #12316, #30774, #55451, #55996, #37531, #56547, #90675, #39167, #20164, #47050 ),
 .UNSPECIFIED., .F., .F.,
 ( 4, 2, 2, 2, 4 ),
 ( 0.000000000000000000, 0.0007438262484377516567, 0.001487652496875503313, 0.002231478745313254970, 0.002975304993751006627 ),
 .UNSPECIFIED. ) ;
#60264 = ORIENTED_EDGE ( 'NONE', *, *, #97074, .F. ) ;
#60265 = CARTESIAN_POINT ( 'NONE',  ( -11.07527106836971775, 1414.913060387329779, 197.4018683738858044 ) ) ;
#60266 = CARTESIAN_POINT ( 'NONE',  ( -4.660393612750000081, 1436.848553822789881, 227.0391165213990234 ) ) ;
#60267 = CARTESIAN_POINT ( 'NONE',  ( -6.559168674874999105, 1516.960844870249957, 204.1192525727769862 ) ) ;
#60268 = CARTESIAN_POINT ( 'NONE',  ( -28.99333967900000175, 1509.929026104229933, 203.7293937816380094 ) ) ;
#60269 = DIRECTION ( 'NONE',  ( 0.000000000000000000, 1.000000000000000000, 0.000000000000000000 ) ) ;
#60270 = CARTESIAN_POINT ( 'NONE',  ( -64.53706522309998661, 1385.084217465399888, 254.0329369609589776 ) ) ;
#60271 = EDGE_CURVE ( 'NONE', #45857, #29539, #20373, .T. ) ;
#60272 = CARTESIAN_POINT ( 'NONE',  ( -39.24126402133479985, 1384.580542155480089, 212.2021475517339866 ) ) ;
#60273 = CARTESIAN_POINT ( 'NONE',  ( -6.972733185100000064, 1409.156553595530113, 196.2309095868979796 ) ) ;
#60274 = CARTESIAN_POINT ( 'NONE',  ( -107.6642996119999935, 1387.006294017490063, 310.6297471052590140 ) ) ;
#60276 = EDGE_LOOP ( 'NONE', ( #47182, #13646, #56681, #66447, #74952 ) ) ;
#60275 = CARTESIAN_POINT ( 'NONE',  ( -9.302446781629999606, 1445.510056962059934, 184.3653119834979748 ) ) ;
#60277 = FACE_OUTER_BOUND ( 'NONE', #31822, .T. ) ;
#60278 = CARTESIAN_POINT ( 'NONE',  ( 21.04266091710000097, 1508.126368074930269, 226.0751098261980019 ) ) ;
#60279 = CARTESIAN_POINT ( 'NONE',  ( 20.39580838967040322, 1487.450036232110051, 225.4216937902110089 ) ) ;
#60280 = CARTESIAN_POINT ( 'NONE',  ( -25.14723534630000046, 1435.562924969450251, 136.5603555134980240 ) ) ;
#60281 = CARTESIAN_POINT ( 'NONE',  ( -1.118903308544999975, 1517.003078582959688, 212.0031713441969998 ) ) ;
#60282 = CARTESIAN_POINT ( 'NONE',  ( -68.73472092510000664, 1379.747979032470084, 280.1061875640590415 ) ) ;
#60283 = AXIS2_PLACEMENT_3D ( 'NONE', #84015, #75090, #101339 ) ;
#60284 = CARTESIAN_POINT ( 'NONE',  ( -14.85284859380000100, 1420.429529095230009, 227.0635863076980172 ) ) ;
#60285 = CARTESIAN_POINT ( 'NONE',  ( 7.105427357599999217E-15, 1405.913060387330006, 146.1721969590979882 ) ) ;
#60286 = CARTESIAN_POINT ( 'NONE',  ( -2.491655763544999846, 1516.977504706749869, 208.3867361609839861 ) ) ;
#60287 = ORIENTED_EDGE ( 'NONE', *, *, #18490, .T. ) ;
#60288 = DIRECTION ( 'NONE',  ( 0.03204755514876567873, 0.01239821417688169794, 0.9994094448694244015 ) ) ;
#60289 = CARTESIAN_POINT ( 'NONE',  ( -2.824333841560000113, 1412.839907593029920, 232.6864343732979989 ) ) ;
#60291 = B_SPLINE_CURVE_WITH_KNOTS ( 'NONE', 3,
 ( #85538, #102349, #65610, #91345, #48256, #23015, #65055, #110203, #42447, #25632, #50860 ),
 .UNSPECIFIED., .F., .F.,
 ( 4, 2, 1, 2, 2, 4 ),
 ( 0.000000000000000000, 0.2500000000001129097, 0.3750000000001033618, 0.4375000000000550671, 0.5000000000000067724, 1.000000000000000000 ),
 .UNSPECIFIED. ) ;
#60290 = CARTESIAN_POINT ( 'NONE',  ( -59.23371022229999738, 1384.698177673139980, 279.9261678725590059 ) ) ;
#60292 = EDGE_LOOP ( 'NONE', ( #7157, #72719, #88541, #67274 ) ) ;
#60293 = CARTESIAN_POINT ( 'NONE',  ( -13.61444516352630174, 1385.299542045740054, 219.1554977703900136 ) ) ;
#60294 = CARTESIAN_POINT ( 'NONE',  ( -3.699859460309999903, 1428.525139549190044, 200.5225814697290048 ) ) ;
#60295 = CARTESIAN_POINT ( 'NONE',  ( 12.38050916831940107, 1435.706281718790024, 151.0122276686279861 ) ) ;
#60296 = EDGE_CURVE ( 'NONE', #90411, #100324, #44840, .T. ) ;
#60297 = CARTESIAN_POINT ( 'NONE',  ( 16.47627392169409788, 1459.305803831369985, 229.0165498365500127 ) ) ;
#60298 = CARTESIAN_POINT ( 'NONE',  ( -21.52252890938149932, 1508.917042082100124, 227.3600265264449831 ) ) ;
#60299 = CARTESIAN_POINT ( 'NONE',  ( 3.451257193719999616, 1486.991677164690145, 198.1002659811989872 ) ) ;
#60300 = CARTESIAN_POINT ( 'NONE',  ( -22.03465957474591619, 1501.977400791986611, 182.8300405912331144 ) ) ;
#60301 = CARTESIAN_POINT ( 'NONE',  ( -32.86802468386297704, 1501.977400791986611, 201.0396662540046577 ) ) ;
#60303 = CARTESIAN_POINT ( 'NONE',  ( 21.41971086555102133, 1511.187213306747708, 233.0798096144380906 ) ) ;
#60302 = CARTESIAN_POINT ( 'NONE',  ( -7.712490991114999694, 1516.666407245520077, 213.7387074786470009 ) ) ;
#60304 = CARTESIAN_POINT ( 'NONE',  ( -8.880888756510550763, 1385.269894070959708, 218.6655104340140099 ) ) ;
#60305 = CARTESIAN_POINT ( 'NONE',  ( -3.453453303525895635, 1420.336231801281883, 144.1190299178094563 ) ) ;
#60306 = VECTOR ( 'NONE', #84094, 1000.000000000000114 ) ;
#60307 = ORIENTED_EDGE ( 'NONE', *, *, #11355, .F. ) ;
#60308 = CARTESIAN_POINT ( 'NONE',  ( 7.718949774015209542, 1516.913059669559971, 209.0472627469650035 ) ) ;
#60309 = CARTESIAN_POINT ( 'NONE',  ( -11.60004869885203682, 1425.894669202444675, 137.5118601406020673 ) ) ;
#60310 = ORIENTED_EDGE ( 'NONE', *, *, #26824, .T. ) ;
#60311 = CARTESIAN_POINT ( 'NONE',  ( 3.126635617060000261, 1420.873695464229968, 185.0718492959979926 ) ) ;
#60312 = CARTESIAN_POINT ( 'NONE',  ( -21.54121752360000031, 1506.208929616789874, 209.2336487591589957 ) ) ;
#60313 = CARTESIAN_POINT ( 'NONE',  ( -105.4624709189999834, 1391.255327103129957, 304.2078109453590287 ) ) ;
#60314 = PRODUCT_DEFINITION_CONTEXT ( 'detailed design', #72126, 'design' ) ;
#60315 = CARTESIAN_POINT ( 'NONE',  ( 1.352857657636009847, 1423.805410520770010, 191.2289116454009843 ) ) ;
#60316 = DIRECTION ( 'NONE',  ( -0.9942586961433764747, -2.969930264099993005E-15, -0.1070030146457249115 ) ) ;
#60317 = CARTESIAN_POINT ( 'NONE',  ( -3.601377948332706413, 1508.124270563087748, 220.7476335447334748 ) ) ;
#60318 = CARTESIAN_POINT ( 'NONE',  ( 17.85311748929999709, 1415.140114704729967, 210.5770968554979845 ) ) ;
#60319 = CARTESIAN_POINT ( 'NONE',  ( -19.63722818156799832, 1519.551704408389924, 200.0074286628000095 ) ) ;
#60320 = CARTESIAN_POINT ( 'NONE',  ( -5.385523200472070116, 1511.435001055929888, 200.4690698413500058 ) ) ;
#60321 = LINE ( 'NONE', #43522, #36039 ) ;
#60322 = CARTESIAN_POINT ( 'NONE',  ( 45.19888506029440123, 1440.913060374670067, 265.6850257504329988 ) ) ;
#60324 = CARTESIAN_POINT ( 'NONE',  ( -2.967510011182339813, 1486.005022665990055, 182.1268798534620146 ) ) ;
#60323 = CARTESIAN_POINT ( 'NONE',  ( -14.38245154268600068, 1418.040796936970082, 202.3365336577070082 ) ) ;
#60325 = CARTESIAN_POINT ( 'NONE',  ( 10.85263098157019890, 1425.442989095870871, 147.0760006456408746 ) ) ;
#60326 = ORIENTED_EDGE ( 'NONE', *, *, #53884, .F. ) ;
#60327 = CARTESIAN_POINT ( 'NONE',  ( -7.694565099120000085, 1508.539300327990077, 219.2224448576989744 ) ) ;
#60328 = CARTESIAN_POINT ( 'NONE',  ( -4.487249066482500659, 1509.038643261319976, 211.6097700942569872 ) ) ;
#60329 = EDGE_CURVE ( 'NONE', #76242, #74855, #36130, .T. ) ;
#60330 = CIRCLE ( 'NONE', #83483, 7.999657266239995401 ) ;
#60331 = CARTESIAN_POINT ( 'NONE',  ( -28.70471842169999732, 1509.915451241629853, 211.4532599174380039 ) ) ;
#60332 = CARTESIAN_POINT ( 'NONE',  ( 5.503649956843871927, 1410.480191370396142, 186.5618691807696052 ) ) ;
#60333 = EDGE_CURVE ( 'NONE', #51540, #100609, #13167, .T. ) ;
#60334 = CARTESIAN_POINT ( 'NONE',  ( -10.50525416227409892, 1479.903349258469916, 209.3106010834520134 ) ) ;
#60335 = CARTESIAN_POINT ( 'NONE',  ( 9.833393186232889605, 1517.051704408389924, 205.7359371553449989 ) ) ;
#60336 = CARTESIAN_POINT ( 'NONE',  ( -11.15048904225209903, 1470.285759522020044, 211.3960241579200101 ) ) ;
#60337 = CARTESIAN_POINT ( 'NONE',  ( 33.42844755917187882, 1501.977400791986611, 196.1165140606791226 ) ) ;
#60338 = CARTESIAN_POINT ( 'NONE',  ( 4.677543868301159868, 1434.888993089650057, 228.7640141638709963 ) ) ;
#60339 = CARTESIAN_POINT ( 'NONE',  ( -71.42280142184640113, 1383.783904420230101, 296.3576773952639769 ) ) ;
#60340 = CARTESIAN_POINT ( 'NONE',  ( 3.538898781339999911, 1452.789479317830001, 152.9844706352979813 ) ) ;
#60341 = CARTESIAN_POINT ( 'NONE',  ( -27.23667361500285367, 1509.093168187175024, 212.0595736267784162 ) ) ;
#60342 = CARTESIAN_POINT ( 'NONE',  ( -1.695768267810110030, 1516.547466091170008, 201.4124695628590018 ) ) ;
#60344 = ORIENTED_EDGE ( 'NONE', *, *, #57002, .T. ) ;
#60343 = CARTESIAN_POINT ( 'NONE',  ( 25.40371319049999954, 1509.800185459130034, 194.3524381038979811 ) ) ;
#60345 = CARTESIAN_POINT ( 'NONE',  ( -18.64904950366887704, 1458.434616773794005, 227.4345046988593424 ) ) ;
#60346 = CARTESIAN_POINT ( 'NONE',  ( -87.00440039350000632, 1383.772198133360007, 307.5612418777589596 ) ) ;
#60347 = CARTESIAN_POINT ( 'NONE',  ( 20.51884491728609916, 1509.640283927850078, 230.4689269196439909 ) ) ;
#60348 = EDGE_LOOP ( 'NONE', ( #57885, #82090, #33085, #52435 ) ) ;
#60349 = VERTEX_POINT ( 'NONE', #79243 ) ;
#60350 = CARTESIAN_POINT ( 'NONE',  ( 16.84932903106719593, 1507.643820733580014, 231.2344440140070105 ) ) ;
#60351 = CARTESIAN_POINT ( 'NONE',  ( -20.86254339170000094, 1504.682062816289999, 214.2159060785090219 ) ) ;
#60352 = CARTESIAN_POINT ( 'NONE',  ( 39.76846978917860298, 1441.086563173470040, 136.8361555895239974 ) ) ;
#60354 = CARTESIAN_POINT ( 'NONE',  ( 4.031617629829999494, 1486.311417117990004, 219.1318982698989828 ) ) ;
#60353 = CARTESIAN_POINT ( 'NONE',  ( 2.752169640037664955, 1410.389826760280812, 269.3346704479379241 ) ) ;
#60355 = CARTESIAN_POINT ( 'NONE',  ( -4.926245301684949673, 1495.054961305510005, 197.8234830982279959 ) ) ;
#60356 = CIRCLE ( 'NONE', #19155, 1.999999999999998668 ) ;
#60357 = CARTESIAN_POINT ( 'NONE',  ( -109.2946818930000035, 1382.595360700089941, 297.4130465109590205 ) ) ;
#60358 = CARTESIAN_POINT ( 'NONE',  ( -12.77945754873770312, 1435.908885557353415, 150.8386072880828408 ) ) ;
#60359 = CARTESIAN_POINT ( 'NONE',  ( -20.21139152160000307, 1485.602675199130090, 191.2208696118980242 ) ) ;
#60360 = ADVANCED_FACE ( 'NONE', ( #2551 ), #30395, .T. ) ;
#60361 = CARTESIAN_POINT ( 'NONE',  ( 2.441025387419999859, 1408.998302871329997, 186.5920540833980112 ) ) ;
#60362 = CARTESIAN_POINT ( 'NONE',  ( -1.398989223888390088, 1485.780538973669991, 197.3046819373520009 ) ) ;
#60363 = CARTESIAN_POINT ( 'NONE',  ( -8.510960889389998840, 1440.269029031439914, 153.6986479344980125 ) ) ;
#60364 = CARTESIAN_POINT ( 'NONE',  ( -9.179256326701130675, 1450.524624793770045, 208.2094894903229942 ) ) ;
#60365 = LINE ( 'NONE', #2686, #71646 ) ;
#60366 = CIRCLE ( 'NONE', #12071, 1.999999999999999556 ) ;
#60367 = CARTESIAN_POINT ( 'NONE',  ( -24.95756431429999722, 1451.613974120029980, 137.4741663018980091 ) ) ;
#60368 = CARTESIAN_POINT ( 'NONE',  ( 2.463295240619999937, 1464.794365564629743, 237.1801197511979922 ) ) ;
#60369 = ORIENTED_EDGE ( 'NONE', *, *, #102051, .T. ) ;
#60370 = EDGE_CURVE ( 'NONE', #83271, #56110, #59445, .T. ) ;
#60371 = CARTESIAN_POINT ( 'NONE',  ( 18.29878862780000048, 1474.159682674189980, 194.8322854508990076 ) ) ;
#60372 = CARTESIAN_POINT ( 'NONE',  ( -44.01745644850000616, 1445.811985921539872, 270.0975557605979702 ) ) ;
#60373 = CARTESIAN_POINT ( 'NONE',  ( 17.06941271609999689, 1409.674943327129995, 224.1775087769979962 ) ) ;
#60374 = EDGE_CURVE ( 'NONE', #65430, #63746, #85610, .T. ) ;
#60376 = CARTESIAN_POINT ( 'NONE',  ( -3.922072518270000252, 1476.187451415889882, 202.7181511965089840 ) ) ;
#60375 = B_SPLINE_CURVE_WITH_KNOTS ( 'NONE', 3,
 ( #29760, #55541, #72883, #81807, #54998, #46594, #99703, #107021, #39263, #73437, #56078, #80729, #81258, #48237, #21878, #30309, #89121, #65033, #12410, #30858, #97526, #90204, #4037, #13488, #108114, #6210, #106475, #89665, #14607, #39823, #99151, #107572, #31408, #64499 ),
 .UNSPECIFIED., .F., .F.,
 ( 4, 3, 3, 3, 3, 3, 3, 3, 3, 3, 3, 4 ),
 ( -7.870238109499999801, -7.787503224266919766, -7.483736671101009819, -7.152628210470729719, -6.787049584866209351, -6.322373280637119564, -5.900059652451949965, -5.548137115487610238, -5.385973697081239742, -4.854088901389330246, -4.240705037260870114, -3.226035699099999654 ),
 .UNSPECIFIED. ) ;
#60377 = CARTESIAN_POINT ( 'NONE',  ( -1.120982774553380006E-08, 1474.398122755949998, 264.1710263624909771 ) ) ;
#60378 = CARTESIAN_POINT ( 'NONE',  ( 2.920726586082400100, 1409.795150870450016, 231.4697806816330115 ) ) ;
#60379 = CARTESIAN_POINT ( 'NONE',  ( -1.064544241000000113, 1415.263254644630024, 227.0974121259979768 ) ) ;
#60380 = CARTESIAN_POINT ( 'NONE',  ( -3.454294121580000265, 1417.605600631229890, 235.1430308038980002 ) ) ;
#60381 = CARTESIAN_POINT ( 'NONE',  ( -1.779830841699999944, 1475.353704572689821, 197.8049865350990046 ) ) ;
#60382 = CARTESIAN_POINT ( 'NONE',  ( -108.4825948470000014, 1386.816125860719922, 310.7856892562589906 ) ) ;
#60383 = CARTESIAN_POINT ( 'NONE',  ( -0.9697694473224367506, 1484.980380940773102, 182.0907361725558360 ) ) ;
#60384 = CARTESIAN_POINT ( 'NONE',  ( 3.426613460960000079, 1360.656565846710009, 207.6218459616989946 ) ) ;
#60385 = CARTESIAN_POINT ( 'NONE',  ( -46.01202577552099626, 1439.422152723799854, 266.6782865154239630 ) ) ;
#60386 = CARTESIAN_POINT ( 'NONE',  ( -3.599584570160000219, 1428.751101579730175, 185.8911643027980176 ) ) ;
#60387 = CARTESIAN_POINT ( 'NONE',  ( -8.049617774310000584, 1424.935508317819995, 210.1093181517179858 ) ) ;
#60388 = EDGE_CURVE ( 'NONE', #66989, #40567, #43651, .T. ) ;
#60389 = VERTEX_POINT ( 'NONE', #62207 ) ;
#60390 = CARTESIAN_POINT ( 'NONE',  ( 2.491655725414999800, 1516.977504706749869, 209.8569557413499922 ) ) ;
#60391 = CARTESIAN_POINT ( 'NONE',  ( -2.478438400780000439, 1438.044022645609857, 157.7045694735979851 ) ) ;
#60392 = AXIS2_PLACEMENT_3D ( 'NONE', #108795, #60067, #23676 ) ;
#60393 = CARTESIAN_POINT ( 'NONE',  ( 19.30109655617612674, 1456.551915534814498, 224.7044840561601120 ) ) ;
#60394 = CARTESIAN_POINT ( 'NONE',  ( 7.535489564291699693, 1425.549448153189815, 212.1837449646579898 ) ) ;
#60395 = EDGE_CURVE ( 'NONE', #71004, #39998, #45611, .T. ) ;
#60396 = CARTESIAN_POINT ( 'NONE',  ( -26.87827581797160192, 1451.501870722200010, 136.0699096253820244 ) ) ;
#60397 = ORIENTED_EDGE ( 'NONE', *, *, #47520, .F. ) ;
#60398 = CARTESIAN_POINT ( 'NONE',  ( -14.14461398200000097, 1452.819910075730149, 195.5024427521979931 ) ) ;
#60400 = CARTESIAN_POINT ( 'NONE',  ( -15.21580404780189966, 1513.293387712810045, 223.3414678796779924 ) ) ;
#60399 = CARTESIAN_POINT ( 'NONE',  ( -2.708183792730093131, 1524.374142163904253, 176.2566682395902262 ) ) ;
#60401 = EDGE_CURVE ( 'NONE', #83342, #23737, #86565, .T. ) ;
#60402 = DIRECTION ( 'NONE',  ( 0.000000000000000000, 0.000000000000000000, -1.000000000000000000 ) ) ;
#60403 = CARTESIAN_POINT ( 'NONE',  ( -23.95707600349131994, 1445.781625871585447, 214.3999464193026370 ) ) ;
#60404 = CARTESIAN_POINT ( 'NONE',  ( -2.458597632860000104, 1456.374695818690043, 215.3392858312989802 ) ) ;
#60405 = ADVANCED_FACE ( 'NONE', ( #36969 ), #67724, .F. ) ;
#60406 = CARTESIAN_POINT ( 'NONE',  ( -17.71193100849139768, 1522.051704408389924, 221.5709757781449980 ) ) ;
#60407 = ORIENTED_EDGE ( 'NONE', *, *, #104138, .F. ) ;
#60408 = CARTESIAN_POINT ( 'NONE',  ( -1.255427878548490028, 1407.658860642259924, 270.1374946076119841 ) ) ;
#60409 = CARTESIAN_POINT ( 'NONE',  ( 6.548200587644999793, 1516.632821972880038, 207.9912384682270101 ) ) ;
#60410 = CARTESIAN_POINT ( 'NONE',  ( 12.24805133206790053, 1420.337794571750010, 229.9787113497959865 ) ) ;
#60411 = CARTESIAN_POINT ( 'NONE',  ( 8.249102711688488299, 1435.329757872420032, 206.3470792129120071 ) ) ;
#60413 = ORIENTED_EDGE ( 'NONE', *, *, #82503, .F. ) ;
#60412 = CARTESIAN_POINT ( 'NONE',  ( -3.763781937370000108, 1369.097489338550076, 207.6218459616989946 ) ) ;
#60414 = EDGE_LOOP ( 'NONE', ( #8473, #110396, #71105, #101256 ) ) ;
#60415 = ADVANCED_FACE ( 'NONE', ( #101253 ), #6149, .T. ) ;
#60416 = CARTESIAN_POINT ( 'NONE',  ( -23.55086081228390071, 1411.110693255149727, 210.4794179021569960 ) ) ;
#60417 = CARTESIAN_POINT ( 'NONE',  ( -0.2257100754742899784, 1409.089074076840006, 185.5875059678090224 ) ) ;
#60418 = CARTESIAN_POINT ( 'NONE',  ( -17.25887910663729841, 1444.159329669600083, 200.5184087357610281 ) ) ;
#60419 = CIRCLE ( 'NONE', #40732, 0.9999999999999930056 ) ;
#60420 = CARTESIAN_POINT ( 'NONE',  ( -45.66504371789742578, 1440.259978084865224, 266.1887742723951646 ) ) ;
#60421 = EDGE_CURVE ( 'NONE', #57270, #65905, #33355, .T. ) ;
#60422 = CARTESIAN_POINT ( 'NONE',  ( -20.71123423377139972, 1497.550399210990008, 192.5020499071400195 ) ) ;
#60423 = CARTESIAN_POINT ( 'NONE',  ( -19.19682044410000188, 1430.794004629730125, 224.3914492935979865 ) ) ;
#60424 = CARTESIAN_POINT ( 'NONE',  ( 33.07189531519680514, 1465.514140148620072, 267.0777719542580257 ) ) ;
#60425 = CARTESIAN_POINT ( 'NONE',  ( -9.277930374200103358, 1464.954721498918616, 232.6830885689707316 ) ) ;
#60426 = CARTESIAN_POINT ( 'NONE',  ( -16.40477380347672209, 1421.217279018667796, 227.0028012172701040 ) ) ;
#60427 = CARTESIAN_POINT ( 'NONE',  ( -7.724732447025000504, 1517.133889586189980, 205.8614888033369823 ) ) ;
#60428 = ORIENTED_EDGE ( 'NONE', *, *, #38974, .F. ) ;
#60429 = CARTESIAN_POINT ( 'NONE',  ( 18.84662620435946323, 1457.907283617477560, 227.0809673387096836 ) ) ;
#60430 = CARTESIAN_POINT ( 'NONE',  ( -6.186741296575624993, 1516.987734611996530, 204.8208301658942219 ) ) ;
#60431 = CARTESIAN_POINT ( 'NONE',  ( 4.208243276966399549, 1434.939303095829928, 227.0652033583169782 ) ) ;
#60432 = ORIENTED_EDGE ( 'NONE', *, *, #42532, .F. ) ;
#60433 = CARTESIAN_POINT ( 'NONE',  ( 3.788285567727110337, 1508.728291974460035, 204.8186037205090031 ) ) ;
#60434 = CARTESIAN_POINT ( 'NONE',  ( 26.09509902904159873, 1452.001783465240123, 135.0935493681200228 ) ) ;
#60435 = CARTESIAN_POINT ( 'NONE',  ( -4.889439660197979265, 1508.551704408389924, 212.3011554026570025 ) ) ;
#60436 = CARTESIAN_POINT ( 'NONE',  ( -6.285004828870000004, 1389.626702675270053, 203.0565589641389863 ) ) ;
#60437 = CARTESIAN_POINT ( 'NONE',  ( -8.888758267720000106, 1385.314821192629779, 218.6605176881890031 ) ) ;
#60438 = CARTESIAN_POINT ( 'NONE',  ( 16.49791572389999672, 1409.489180299430018, 193.7307885960979945 ) ) ;
#60439 = CARTESIAN_POINT ( 'NONE',  ( 13.76936860679999874, 1444.324653571829003, 176.3340081878980641 ) ) ;
#60440 = CARTESIAN_POINT ( 'NONE',  ( 3.492283213099107275, 1439.693639858082861, 184.4976232197295190 ) ) ;
#60442 = CARTESIAN_POINT ( 'NONE',  ( -14.03293030814504050, 1379.586391581537555, 211.8749277816402810 ) ) ;
#60441 = CARTESIAN_POINT ( 'NONE',  ( 31.16645442585767611, 1524.201670966335314, 196.3723102679300894 ) ) ;
#60443 = AXIS2_PLACEMENT_3D ( 'NONE', #93356, #16620, #23932 ) ;
#60444 = CARTESIAN_POINT ( 'NONE',  ( -16.64685887467744507, 1523.847248782568613, 180.5000237996434578 ) ) ;
#60445 = CARTESIAN_POINT ( 'NONE',  ( -15.57808073540140015, 1420.358152465259991, 210.5578313205389804 ) ) ;
#60446 = CARTESIAN_POINT ( 'NONE',  ( -10.97164840699999999, 1381.332427371100039, 216.7312293341890097 ) ) ;
#60447 = CARTESIAN_POINT ( 'NONE',  ( 6.334329861979885123, 1418.381028394342138, 233.6652930423259704 ) ) ;
#60448 = ORIENTED_EDGE ( 'NONE', *, *, #1613, .T. ) ;
#60449 = CARTESIAN_POINT ( 'NONE',  ( 11.16128041097469925, 1414.913057846380070, 221.5234502185170129 ) ) ;
#60450 = CIRCLE ( 'NONE', #106848, 1.000000000000002442 ) ;
#60451 = CARTESIAN_POINT ( 'NONE',  ( -0.4620612703160609791, 1409.418054490960003, 232.8178123332089910 ) ) ;
#60452 = EDGE_CURVE ( 'NONE', #47444, #61158, #16832, .T. ) ;
#60453 = VECTOR ( 'NONE', #33788, 1000.000000000000000 ) ;
#60454 = CARTESIAN_POINT ( 'NONE',  ( -11.15749597250000136, 1390.963088241619971, 203.6399077860090188 ) ) ;
#60455 = EDGE_CURVE ( 'NONE', #30887, #104987, #41885, .T. ) ;
#60456 = CARTESIAN_POINT ( 'NONE',  ( 1.200868670922434989, 1421.369478736644396, 193.7619988307343704 ) ) ;
#60457 = CARTESIAN_POINT ( 'NONE',  ( -4.326992699981060397, 1515.158586643130093, 209.1005884788399953 ) ) ;
#60458 = CARTESIAN_POINT ( 'NONE',  ( -3.268607775400000026, 1455.844446697429930, 219.6133831120980062 ) ) ;
#60459 = CARTESIAN_POINT ( 'NONE',  ( -21.87285697696509956, 1509.490620199582054, 191.4610675759308265 ) ) ;
#60460 = CARTESIAN_POINT ( 'NONE',  ( 11.82457892589999915, 1433.344969013340005, 150.5980735906980215 ) ) ;
#60461 = CARTESIAN_POINT ( 'NONE',  ( 18.57221607090000148, 1447.675799068749939, 219.6133835466979747 ) ) ;
#60462 = CARTESIAN_POINT ( 'NONE',  ( -9.852457870043849653, 1461.554014673809888, 208.8474554947439970 ) ) ;
#60463 = CARTESIAN_POINT ( 'NONE',  ( 20.10527571410489855, 1430.877954731940235, 215.1856771490429878 ) ) ;
#60464 = CARTESIAN_POINT ( 'NONE',  ( 12.03775681428729882, 1426.191895615310159, 202.7989534666060081 ) ) ;
#60465 = CARTESIAN_POINT ( 'NONE',  ( 9.660180252660660827, 1463.103700123790077, 211.4020709551699895 ) ) ;
#60466 = EDGE_CURVE ( 'NONE', #27462, #94190, #83371, .T. ) ;
#60467 = CARTESIAN_POINT ( 'NONE',  ( -4.704661063000000532, 1486.518663884429998, 182.0064326752979866 ) ) ;
#60468 = CARTESIAN_POINT ( 'NONE',  ( 12.66920257684705398, 1398.288630080463918, 206.2055005063946851 ) ) ;
#60469 = CARTESIAN_POINT ( 'NONE',  ( -29.88894142145320032, 1509.995722311340160, 211.8654022664900083 ) ) ;
#60470 = CARTESIAN_POINT ( 'NONE',  ( -8.006373544986240987, 1424.874076710998452, 210.3858704081821145 ) ) ;
#60471 = B_SPLINE_CURVE_WITH_KNOTS ( 'NONE', 5,
 ( #10529, #47451, #91644, #98389, #82135, #21659, #56959, #73767, #107344 ),
 .UNSPECIFIED., .F., .F.,
 ( 6, 3, 6 ),
 ( 0.000000000000000000, 0.5050532947554345897, 1.000000000000000000 ),
 .UNSPECIFIED. ) ;
#60472 = CARTESIAN_POINT ( 'NONE',  ( 2.804856904796726003, 1447.114277549598228, 170.5309535257328548 ) ) ;
#60473 = CARTESIAN_POINT ( 'NONE',  ( -33.91369110859999836, 1435.681798638700002, 135.0664268289980043 ) ) ;
#60474 = CARTESIAN_POINT ( 'NONE',  ( 9.145064077180329321, 1450.428955689400027, 207.9342079399700083 ) ) ;
#60475 = CARTESIAN_POINT ( 'NONE',  ( 23.56404405089999798, 1519.913060387329779, 210.1014910071569943 ) ) ;
#60476 = CARTESIAN_POINT ( 'NONE',  ( -18.47518242017930135, 1466.235720257730009, 200.8822878153090130 ) ) ;
#60477 = CARTESIAN_POINT ( 'NONE',  ( -6.547881413045000265, 1516.647534046129977, 212.5778533554070293 ) ) ;
#60478 = CARTESIAN_POINT ( 'NONE',  ( -16.48668639225170196, 1420.457505516819765, 204.7771018081849945 ) ) ;
#60479 = CARTESIAN_POINT ( 'NONE',  ( 0.1668001638216120019, 1482.213501802149949, 181.9993034263140146 ) ) ;
#60481 = ORIENTED_EDGE ( 'NONE', *, *, #56235, .F. ) ;
#60480 = CARTESIAN_POINT ( 'NONE',  ( 28.84709935510000278, 1507.919204205830056, 206.0039977711180086 ) ) ;
#60482 = FACE_OUTER_BOUND ( 'NONE', #106775, .T. ) ;
#60483 = EDGE_CURVE ( 'NONE', #63480, #97580, #91919, .T. ) ;
#60484 = CARTESIAN_POINT ( 'NONE',  ( 0.003568499702431209702, 1467.142144108200000, 235.6416276161930057 ) ) ;
#60485 = CARTESIAN_POINT ( 'NONE',  ( 11.87504895220000023, 1433.007246834750049, 149.8850454502979801 ) ) ;
#60486 = CARTESIAN_POINT ( 'NONE',  ( -34.20278863726849750, 1451.714767517939890, 134.0999999981159760 ) ) ;
#60487 = CARTESIAN_POINT ( 'NONE',  ( -6.375118004043530462, 1508.551704408389924, 219.3472698286099956 ) ) ;
#60488 = VERTEX_POINT ( 'NONE', #39163 ) ;
#60489 = DIRECTION ( 'NONE',  ( 0.000000000000000000, 1.000000000000000000, 0.000000000000000000 ) ) ;
#60490 = CARTESIAN_POINT ( 'NONE',  ( -14.40730585596589997, 1380.239382581250084, 209.2612549436819904 ) ) ;
#60491 = CARTESIAN_POINT ( 'NONE',  ( 8.244220094398297505, 1448.357206390987585, 205.1189572764488958 ) ) ;
#60492 = DIRECTION ( 'NONE',  ( 0.000000000000000000, -0.07593562622321022026, -0.9971127221483482295 ) ) ;
#60493 = EDGE_CURVE ( 'NONE', #13288, #6825, #50842, .T. ) ;
#60494 = CARTESIAN_POINT ( 'NONE',  ( -5.494816741715999875, 1433.961689851970050, 215.8643144989760003 ) ) ;
#60495 = AXIS2_PLACEMENT_3D ( 'NONE', #34865, #69054, #1850 ) ;
#60496 = CARTESIAN_POINT ( 'NONE',  ( -109.0574111638984505, 1382.174802844307578, 310.8550843848203158 ) ) ;
#60497 = CARTESIAN_POINT ( 'NONE',  ( -10.31429908969579934, 1472.129925722029839, 207.0851132311250069 ) ) ;
#60498 = CARTESIAN_POINT ( 'NONE',  ( -34.18677586421195258, 1501.977400791986611, 198.4504086008750505 ) ) ;
#60499 = CARTESIAN_POINT ( 'NONE',  ( -10.81171441090000052, 1391.913060387289988, 204.7749328824690167 ) ) ;
#60500 = CARTESIAN_POINT ( 'NONE',  ( -68.46831016306249751, 1385.104556025459942, 262.6710340492040245 ) ) ;
#60501 = CARTESIAN_POINT ( 'NONE',  ( 2.811694757223507146, 1464.674002724843604, 236.8041411256813547 ) ) ;
#60502 = CARTESIAN_POINT ( 'NONE',  ( -3.427918555806571455, 1475.607266589915980, 218.8585788157315335 ) ) ;
#60503 = EDGE_LOOP ( 'NONE', ( #15315, #50600, #39584, #102509 ) ) ;
#60504 = CARTESIAN_POINT ( 'NONE',  ( 16.68463233076019492, 1442.773887286370609, 162.0935120523188857 ) ) ;
#60506 = VERTEX_POINT ( 'NONE', #99063 ) ;
#60505 = CARTESIAN_POINT ( 'NONE',  ( -4.682234856550000046, 1438.893385222290135, 227.1256850459990062 ) ) ;
#60507 = CARTESIAN_POINT ( 'NONE',  ( 29.16732601703412442, 1436.844822267699328, 136.7085307917412820 ) ) ;
#60508 = ORIENTED_EDGE ( 'NONE', *, *, #42564, .F. ) ;
#60509 = CARTESIAN_POINT ( 'NONE',  ( 6.645104883328971646, 1422.852120593709969, 195.1791986883735035 ) ) ;
#60510 = CARTESIAN_POINT ( 'NONE',  ( -7.816276179476305153, 1364.594548665079628, 209.6218459617148824 ) ) ;
#60511 = CARTESIAN_POINT ( 'NONE',  ( -10.02453695329999839, 1493.300892679689923, 203.8691444315089996 ) ) ;
#60512 = EDGE_CURVE ( 'NONE', #73683, #106220, #40825, .T. ) ;
#60513 = LINE ( 'NONE', #15694, #96565 ) ;
#60514 = DIRECTION ( 'NONE',  ( -0.9455185755993177343, 0.000000000000000000, 0.3255681544571540909 ) ) ;
#60515 = CARTESIAN_POINT ( 'NONE',  ( 6.016808910419999989, 1396.654460028929861, 220.0432386207980073 ) ) ;
#60516 = CARTESIAN_POINT ( 'NONE',  ( 10855.50032577649290, 5181.793945261120825, -7093.638272652226078 ) ) ;
#60517 = DIRECTION ( 'NONE',  ( -0.000000000000000000, -0.000000000000000000, 1.000000000000000000 ) ) ;
#60518 = CARTESIAN_POINT ( 'NONE',  ( -105.3788045886400511, 1309.112692017089785, 296.2006505458987249 ) ) ;
#60519 = CARTESIAN_POINT ( 'NONE',  ( -5.551604495410622953, 1369.933960282451608, 210.6218459617030021 ) ) ;
#60520 = B_SPLINE_CURVE_WITH_KNOTS ( 'NONE', 3,
 ( #92317, #23993, #23462, #66608, #31313, #31866, #101249, #13948, #47580, #30763, #65497, #15046, #73890, #82277, #91768, #57656, #83366, #99606, #99057, #58189 ),
 .UNSPECIFIED., .F., .F.,
 ( 4, 2, 1, 2, 2, 1, 1, 1, 1, 1, 2, 2, 4 ),
 ( 0.000000000000000000, 0.2499999999997811750, 0.3749999999996714295, 0.4374999999996159739, 0.4999999999995604627, 0.6249999999994507727, 0.6874999999993959277, 0.7187499999993685051, 0.7343749999993555155, 0.7421874999993490762, 0.7460937499993504085, 0.7499999999993517408, 1.000000000000000000 ),
 .UNSPECIFIED. ) ;
#60521 = VECTOR ( 'NONE', #62565, 1000.000000000000000 ) ;
#60522 = CARTESIAN_POINT ( 'NONE',  ( 2.664554167960305531, 1448.256636475937967, 183.4094032644174774 ) ) ;
#60523 = EDGE_CURVE ( 'NONE', #86013, #64533, #10886, .T. ) ;
#60524 = CARTESIAN_POINT ( 'NONE',  ( 4.026777485955000735, 1516.718889242609976, 206.8247602162870180 ) ) ;
#60525 = AXIS2_PLACEMENT_3D ( 'NONE', #15002, #75508, #49201 ) ;
#60526 = CARTESIAN_POINT ( 'NONE',  ( 2.499999990390000093, 1447.656584284949986, 165.9523963823980068 ) ) ;
#60527 = CARTESIAN_POINT ( 'NONE',  ( 16.68463225830000241, 1442.773887286369927, 162.0935120917980043 ) ) ;
#60528 = CARTESIAN_POINT ( 'NONE',  ( 45.63713230949999655, 1446.564129982419900, 268.9747493906979798 ) ) ;
#60530 = ORIENTED_EDGE ( 'NONE', *, *, #96732, .F. ) ;
#60529 = CARTESIAN_POINT ( 'NONE',  ( -68.77190087506669158, 1379.747925807530009, 280.3125204381590265 ) ) ;
#60531 = ADVANCED_FACE ( 'NONE', ( #82282 ), #65162, .T. ) ;
#60532 = DIRECTION ( 'NONE',  ( 0.9455185755993167351, 0.000000000000000000, -0.3255681544571568109 ) ) ;
#60533 = VERTEX_POINT ( 'NONE', #109690 ) ;
#60534 = CIRCLE ( 'NONE', #101648, 7.975189853890007896 ) ;
#60535 = CARTESIAN_POINT ( 'NONE',  ( -16.53526713099472900, 1514.188985850001018, 223.4099743505789490 ) ) ;
#60536 = CARTESIAN_POINT ( 'NONE',  ( -24.79630738070000007, 1449.797614630550015, 204.8702466810979956 ) ) ;
#60538 = CARTESIAN_POINT ( 'NONE',  ( 17.05828028330499890, 1410.454619143949913, 192.1468146258000047 ) ) ;
#60537 = CARTESIAN_POINT ( 'NONE',  ( -10.71712433759610050, 1425.352709571739979, 115.9742016334039931 ) ) ;
#60539 = CARTESIAN_POINT ( 'NONE',  ( -2.863787893864999656, 1516.788317650260069, 210.8382387120070121 ) ) ;
#60540 =( BOUNDED_CURVE ( )  B_SPLINE_CURVE ( 3, ( #18387, #104067, #45845, #11669 ),
 .UNSPECIFIED., .F., .T. ) 
 B_SPLINE_CURVE_WITH_KNOTS ( ( 4, 4 ),
 ( 5.970709790778379933, 6.887917497424890456 ),
 .UNSPECIFIED. ) 
 CURVE ( )  GEOMETRIC_REPRESENTATION_ITEM ( )  RATIONAL_B_SPLINE_CURVE ( ( 1.000000000000000000, 0.9311142937961904842, 0.9311142937961904842, 1.000000000000000000 ) ) 
 REPRESENTATION_ITEM ( '' )  );
#60541 = CARTESIAN_POINT ( 'NONE',  ( 18.39298867610254717, 1509.674607414416414, 185.4216858732138462 ) ) ;
#60542 = AXIS2_PLACEMENT_3D ( 'NONE', #27882, #45811, #19464 ) ;
#60543 = CARTESIAN_POINT ( 'NONE',  ( -22.09712912739999879, 1489.469559537229998, 208.2081598746609927 ) ) ;
#60544 = CARTESIAN_POINT ( 'NONE',  ( -38.63858781420000099, 1428.253854744629962, 261.7057204824979522 ) ) ;
#60545 = CARTESIAN_POINT ( 'NONE',  ( -14.08326878217680012, 1379.708207602939865, 208.2775395970890031 ) ) ;
#60546 = CARTESIAN_POINT ( 'NONE',  ( 29.61157949199080264, 1509.955833108989964, 209.6611346260839923 ) ) ;
#60547 = CARTESIAN_POINT ( 'NONE',  ( 4.421669554984550388, 1508.551704408389924, 213.1944784729480205 ) ) ;
#60548 = CARTESIAN_POINT ( 'NONE',  ( -39.39983805167630493, 1440.332349523559969, 136.7601460201240116 ) ) ;
#60549 = VERTEX_POINT ( 'NONE', #56542 ) ;
#60550 = CARTESIAN_POINT ( 'NONE',  ( 7.602373182780730154, 1397.519631357160051, 197.5586426691019994 ) ) ;
#60551 = CARTESIAN_POINT ( 'NONE',  ( 9.636560193436579880, 1462.074131928580073, 207.7511217272350166 ) ) ;
#60552 = ADVANCED_FACE ( 'NONE', ( #32966 ), #76079, .F. ) ;
#60553 = CARTESIAN_POINT ( 'NONE',  ( -18.16700093809999927, 1457.608413576630028, 229.6942240664980091 ) ) ;
#60554 = VERTEX_POINT ( 'NONE', #56413 ) ;
#60555 = ORIENTED_EDGE ( 'NONE', *, *, #104087, .T. ) ;
#60556 = CARTESIAN_POINT ( 'NONE',  ( -2.439001525050000119, 1430.488531030629929, 150.2249694046979869 ) ) ;
#60557 = CARTESIAN_POINT ( 'NONE',  ( -6.413908422285220290, 1429.087440716829860, 154.6253968713650124 ) ) ;
#60558 = ORIENTED_EDGE ( 'NONE', *, *, #95281, .F. ) ;
#60559 = CARTESIAN_POINT ( 'NONE',  ( -14.29942586552730077, 1380.320760441320090, 210.0466192271150021 ) ) ;
#60560 = VECTOR ( 'NONE', #60952, 1000.000000000000000 ) ;
#60561 = CARTESIAN_POINT ( 'NONE',  ( -11.35888576287617369, 1417.774827459571043, 198.7178256456102474 ) ) ;
#60562 = EDGE_CURVE ( 'NONE', #1934, #109446, #38284, .T. ) ;
#60563 = CARTESIAN_POINT ( 'NONE',  ( -11.87326589167020074, 1432.874500706740037, 149.9809363116050065 ) ) ;
#60564 = DIRECTION ( 'NONE',  ( -0.1867471702549219348, 2.391457216852619248E-16, 0.9824080081115885710 ) ) ;
#60565 = CARTESIAN_POINT ( 'NONE',  ( 6.648384424976800489, 1508.610125760119899, 202.0257673391629964 ) ) ;
#60566 = CARTESIAN_POINT ( 'NONE',  ( 10.09897474760730063, 1452.024231682490154, 208.5505077355719834 ) ) ;
#60567 = CARTESIAN_POINT ( 'NONE',  ( -11.66658881389999891, 1391.913060387289988, 209.7119989811589846 ) ) ;
#60568 = CARTESIAN_POINT ( 'NONE',  ( -88.50299786935610769, 1384.832684027770028, 291.5890375481939714 ) ) ;
#60569 = ORIENTED_EDGE ( 'NONE', *, *, #55740, .T. ) ;
#60570 = CARTESIAN_POINT ( 'NONE',  ( 2.870951667784999994, 1517.111322026010157, 202.5592101095969895 ) ) ;
#60571 = CARTESIAN_POINT ( 'NONE',  ( -1.704170752255000032, 1516.927039499179955, 209.8797722570040207 ) ) ;
#60572 = ORIENTED_EDGE ( 'NONE', *, *, #77509, .F. ) ;
#60573 = CARTESIAN_POINT ( 'NONE',  ( 11.81466445377120067, 1428.992090789789927, 148.8655718450160066 ) ) ;
#60574 = CARTESIAN_POINT ( 'NONE',  ( 3.864344981488097908, 1511.505229895790080, 217.2740327373093976 ) ) ;
#60575 = ORIENTED_EDGE ( 'NONE', *, *, #12720, .T. ) ;
#60576 = CARTESIAN_POINT ( 'NONE',  ( -5.367396286529749538, 1487.256192968549840, 235.6479365767530112 ) ) ;
#60577 = CARTESIAN_POINT ( 'NONE',  ( -1.549163664599672252, 1484.315319106566676, 182.5664047062095108 ) ) ;
#60578 = CARTESIAN_POINT ( 'NONE',  ( 6.944731691349999458, 1508.146090184829973, 235.5513729331979960 ) ) ;
#60579 = CARTESIAN_POINT ( 'NONE',  ( -9.642207540978898095, 1460.678569519029907, 208.4219211414859956 ) ) ;
#60580 = CARTESIAN_POINT ( 'NONE',  ( -4.938546209390000108, 1422.091193151429934, 185.5889896035980087 ) ) ;
#60581 = CARTESIAN_POINT ( 'NONE',  ( 6.401487760110000202, 1408.896291596430046, 270.4245279989980304 ) ) ;
#60582 = CARTESIAN_POINT ( 'NONE',  ( 9.224062555858578705, 1450.491461610309898, 209.1237753033059903 ) ) ;
#60583 = CARTESIAN_POINT ( 'NONE',  ( -4.845898873760000392, 1475.703792529090151, 200.0054992556989930 ) ) ;
#60584 = CARTESIAN_POINT ( 'NONE',  ( 6.817812183760000089, 1493.124444775489792, 217.9221528793789844 ) ) ;
#60585 = CARTESIAN_POINT ( 'NONE',  ( -18.89554632140000479, 1379.602095017590045, 208.7270065393099969 ) ) ;
#60586 = CARTESIAN_POINT ( 'NONE',  ( -16.92717818009999675, 1496.365422975929960, 223.9021671830980154 ) ) ;
#60588 = CARTESIAN_POINT ( 'NONE',  ( 15.48102685469999962, 1453.151875979629949, 195.5243114212979947 ) ) ;
#60587 = CARTESIAN_POINT ( 'NONE',  ( -21.53565904410000087, 1506.077647802689853, 209.2113159668479909 ) ) ;
#60589 = CARTESIAN_POINT ( 'NONE',  ( -4.734332965765398527, 1423.620278043627195, 184.5217912470845647 ) ) ;
#60590 = B_SPLINE_CURVE_WITH_KNOTS ( 'NONE', 3,
 ( #81931, #4686, #106591, #14173, #38825, #89789, #83044, #56751, #90328, #22549, #55666, #23678, #73004, #57861, #21999, #13059, #23120, #40486, #46717, #107139, #91451, #90888, #21456, #5234, #4151, #14728, #30432, #38278, #74661, #108797, #65707, #56192, #64618, #32089 ),
 .UNSPECIFIED., .F., .F.,
 ( 4, 2, 2, 1, 2, 2, 2, 2, 1, 1, 2, 2, 2, 2, 1, 1, 1, 2, 2, 4 ),
 ( 0.03289823588023810252, 0.1537859563936441187, 0.2142298166503383006, 0.2444517467786946618, 0.2595627118428728286, 0.2746736769070509121, 0.3955613974205678396, 0.4560052576774560329, 0.4862271878060093200, 0.5013381528701812417, 0.5088936354023581021, 0.5164491179345348515, 0.6373368384519590979, 0.6977806987106713876, 0.7280026288399379375, 0.7431135939045582228, 0.7506690764368684210, 0.7544468177030233536, 0.7582245589691783971, 1.000000000000000000 ),
 .UNSPECIFIED. ) ;
#60591 = CARTESIAN_POINT ( 'NONE',  ( 17.89459807364280053, 1420.234668421669994, 225.0799363196900060 ) ) ;
#60592 = CARTESIAN_POINT ( 'NONE',  ( -0.3821804589910179906, 1506.433683733660018, 187.1424611576989889 ) ) ;
#60593 = ORIENTED_EDGE ( 'NONE', *, *, #47425, .T. ) ;
#60594 = CARTESIAN_POINT ( 'NONE',  ( 18.10086162160209966, 1424.497286396790059, 224.0757393633220147 ) ) ;
#60595 = CARTESIAN_POINT ( 'NONE',  ( -20.17436656406320594, 1524.841055067849766, 180.5047911526357325 ) ) ;
#60596 = CARTESIAN_POINT ( 'NONE',  ( -2.902930634495347384, 1484.532355139261654, 183.2864040210124301 ) ) ;
#60597 = CARTESIAN_POINT ( 'NONE',  ( -14.45258110980000055, 1415.677402202029953, 212.7925583635889950 ) ) ;
#60599 = ORIENTED_EDGE ( 'NONE', *, *, #56832, .T. ) ;
#60598 = CARTESIAN_POINT ( 'NONE',  ( 0.1829789116263519921, 1515.156771665000178, 204.7948057348419866 ) ) ;
#60600 = CARTESIAN_POINT ( 'NONE',  ( -15.48888989581648623, 1415.677402280658725, 209.5875073814394796 ) ) ;
#60601 = CARTESIAN_POINT ( 'NONE',  ( 1.760769565820000215, 1508.551704924790101, 220.0361975827989909 ) ) ;
#60602 = CARTESIAN_POINT ( 'NONE',  ( -11.78833996880000079, 1427.663080501330114, 147.5992344144979995 ) ) ;
#60603 = CARTESIAN_POINT ( 'NONE',  ( -14.70619684508450042, 1424.824187292160104, 221.6451186432019824 ) ) ;
#60604 = CARTESIAN_POINT ( 'NONE',  ( -115.5939564047259296, 1390.913060387289988, 305.4204098037694735 ) ) ;
#60605 = CARTESIAN_POINT ( 'NONE',  ( -12.23669307423070052, 1377.661331666050273, 207.7794331870949804 ) ) ;
#60606 = CARTESIAN_POINT ( 'NONE',  ( -1.600048698852036821, 1402.754281879943164, 135.5999999980979851 ) ) ;
#60607 = CARTESIAN_POINT ( 'NONE',  ( -15.62010811736499782, 1514.600163677630007, 224.4888522828669863 ) ) ;
#60608 = CARTESIAN_POINT ( 'NONE',  ( 19.60792669039999936, 1475.100271358290229, 204.3343059087790152 ) ) ;
#60609 = B_SPLINE_CURVE_WITH_KNOTS ( 'NONE', 3,
 ( #73087, #31066, #65246, #31616, #39479, #98824, #4228, #92080, #83133, #5320, #22085, #90412, #56838, #6429, #13692, #64152, #73649, #98271, #107227, #32176 ),
 .UNSPECIFIED., .F., .F.,
 ( 4, 2, 2, 2, 2, 2, 2, 2, 2, 4 ),
 ( -0.3233081010012240353, -0.3219076690093550241, -0.3116608437711600454, -0.3014431805523019592, -0.2809394392387379868, -0.2394106768222920012, -0.1618956485691949998, -0.08327320055462403281, -0.04160395758957841084, 0.000000000000000000 ),
 .UNSPECIFIED. ) ;
#60610 = CARTESIAN_POINT ( 'NONE',  ( -9.297585099209999981, 1478.447333343590117, 214.0874750368789989 ) ) ;
#60611 = CARTESIAN_POINT ( 'NONE',  ( -15.69727097450000031, 1459.325973232030037, 230.3695337202979658 ) ) ;
#60613 = AXIS2_PLACEMENT_3D ( 'NONE', #8581, #26484, #84188 ) ;
#60612 = CARTESIAN_POINT ( 'NONE',  ( 4.608146781254999880, 1516.677239312369920, 206.8257210811669893 ) ) ;
#60614 = CARTESIAN_POINT ( 'NONE',  ( 26.93223535810000158, 1412.607180478629971, 266.6753325838979549 ) ) ;
#60615 = DIRECTION ( 'NONE',  ( -0.02616798426619638615, -0.9993150019883495494, -0.02616798426453448637 ) ) ;
#60616 = VECTOR ( 'NONE', #80069, 1000.000000000000000 ) ;
#60617 = CARTESIAN_POINT ( 'NONE',  ( 21.51393974440000179, 1449.725088386290281, 196.5704810921979799 ) ) ;
#60618 = CARTESIAN_POINT ( 'NONE',  ( 18.61615544290965829, 1506.404057880957225, 220.7836781479866488 ) ) ;
#60619 = CIRCLE ( 'NONE', #53505, 3.000000000000002665 ) ;
#60620 = CARTESIAN_POINT ( 'NONE',  ( -0.1860383248606379825, 1508.572757955850193, 237.9075060567579669 ) ) ;
#60621 = CARTESIAN_POINT ( 'NONE',  ( 17.27380372710132406, 1525.712830164893376, 236.6835243611168380 ) ) ;
#60622 = CARTESIAN_POINT ( 'NONE',  ( -1.474488223160000056, 1450.666087581440024, 182.8694550166979980 ) ) ;
#60623 = CARTESIAN_POINT ( 'NONE',  ( -20.23078143836107046, 1506.575640307561571, 200.2219735720721587 ) ) ;
#60624 = DIRECTION ( 'NONE',  ( -0.000000000000000000, -1.000000000000000000, -0.000000000000000000 ) ) ;
#60625 = CARTESIAN_POINT ( 'NONE',  ( -12.26000483520000017, 1442.221945175220071, 187.3548814074979987 ) ) ;
#60626 = CARTESIAN_POINT ( 'NONE',  ( 17.99383350722930075, 1429.161952351650143, 206.5116212249160128 ) ) ;
#60627 = CARTESIAN_POINT ( 'NONE',  ( 1.476727066854436776, 1407.665894515924492, 270.1373298217981755 ) ) ;
#60628 = VERTEX_POINT ( 'NONE', #23874 ) ;
#60629 = B_SPLINE_CURVE_WITH_KNOTS ( 'NONE', 3,
 ( #110063, #84306, #51259, #35005, #42869, #59675, #43973 ),
 .UNSPECIFIED., .F., .F.,
 ( 4, 3, 4 ),
 ( 1.117154302310000125, 1.576268520389739969, 1.987970115610000033 ),
 .UNSPECIFIED. ) ;
#60630 = CARTESIAN_POINT ( 'NONE',  ( -2.996785070334999634, 1512.020737142380085, 201.2284348500070053 ) ) ;
#60631 = CARTESIAN_POINT ( 'NONE',  ( -14.84172366651849906, 1409.431344798339978, 207.4607597228529983 ) ) ;
#60632 = CARTESIAN_POINT ( 'NONE',  ( -10.61667206956300014, 1508.551704408270098, 207.6874843289959927 ) ) ;
#60633 = DIRECTION ( 'NONE',  ( -0.9455185755993178454, 0.000000000000000000, 0.3255681544571537578 ) ) ;
#60634 = CARTESIAN_POINT ( 'NONE',  ( -21.96301590319999875, 1471.883841234629926, 267.3321493710980121 ) ) ;
#60636 = AXIS2_PLACEMENT_3D ( 'NONE', #65923, #14923, #83250 ) ;
#60635 = CARTESIAN_POINT ( 'NONE',  ( 29.41145195048112271, 1525.795403383247276, 196.6862061498684113 ) ) ;
#60637 = DIRECTION ( 'NONE',  ( -0.1402804634174202869, 0.9901118076173992533, 0.000000000000000000 ) ) ;
#60638 = CARTESIAN_POINT ( 'NONE',  ( -24.02854045990000031, 1507.902906315029895, 222.3115896357980148 ) ) ;
#60639 = CARTESIAN_POINT ( 'NONE',  ( -82.95076918121009157, 1384.632580800539927, 305.6340335797960392 ) ) ;
#60640 = CARTESIAN_POINT ( 'NONE',  ( -28.06373293278850056, 1384.965165955840121, 204.5801626712980124 ) ) ;
#60641 = CARTESIAN_POINT ( 'NONE',  ( 18.59870848514470154, 1425.273973280189921, 226.9824610977420036 ) ) ;
#60642 = CARTESIAN_POINT ( 'NONE',  ( -11.98951922200000020, 1442.759074889710064, 150.6922381223979812 ) ) ;
#60643 = CARTESIAN_POINT ( 'NONE',  ( -27.43400997898509885, 1507.980975032430024, 210.8257058971020115 ) ) ;
#60644 = CARTESIAN_POINT ( 'NONE',  ( 4.138993644310000164, 1515.551749209589843, 209.1218459616989946 ) ) ;
#60645 = CARTESIAN_POINT ( 'NONE',  ( -8.847652261760000414, 1384.947871987750204, 199.9248388310690245 ) ) ;
#60646 = CARTESIAN_POINT ( 'NONE',  ( -22.10231210369999744, 1409.684890133530189, 206.6229132878879966 ) ) ;
#60647 = CYLINDRICAL_SURFACE ( 'NONE', #58677, 2.000000000000000000 ) ;
#60648 = ADVANCED_FACE ( 'NONE', ( #32834 ), #40258, .F. ) ;
#60649 = CARTESIAN_POINT ( 'NONE',  ( 3.678869892360000282, 1485.512442734190245, 219.3630818239989821 ) ) ;
#60650 = CARTESIAN_POINT ( 'NONE',  ( 4.993626793399999819, 1423.332951346649907, 194.3851876207990017 ) ) ;
#60651 = EDGE_CURVE ( 'NONE', #59489, #33248, #101672, .T. ) ;
#60652 = CARTESIAN_POINT ( 'NONE',  ( 1.665548205979999974, 1442.756953654919926, 150.7199974615980125 ) ) ;
#60653 = CARTESIAN_POINT ( 'NONE',  ( 7.905003682643709340, 1460.527882303560091, 228.8958833807890016 ) ) ;
#60654 = CARTESIAN_POINT ( 'NONE',  ( 17.36692104388846047, 1525.425686270225242, 181.2365643868851635 ) ) ;
#60655 = CARTESIAN_POINT ( 'NONE',  ( -18.80013755969359934, 1505.319302960399909, 222.5373222880980109 ) ) ;
#60657 = CARTESIAN_POINT ( 'NONE',  ( -8.627683608919999969, 1383.470579637440096, 200.0452354592789845 ) ) ;
#60656 = CARTESIAN_POINT ( 'NONE',  ( -22.30625446560000213, 1409.857389892729771, 211.0156766885679929 ) ) ;
#60658 = CARTESIAN_POINT ( 'NONE',  ( 11.72068376100859943, 1426.706399951889807, 142.9991350588749981 ) ) ;
#60659 = LINE ( 'NONE', #86381, #75243 ) ;
#60660 = CARTESIAN_POINT ( 'NONE',  ( -11.88215827279999992, 1489.620311200989818, 211.9665674380289886 ) ) ;
#60661 = CARTESIAN_POINT ( 'NONE',  ( 9.629035390439231179, 1450.586402395090090, 205.0971065227769827 ) ) ;
#60662 = CARTESIAN_POINT ( 'NONE',  ( -0.4432577660195479718, 1419.360889940619927, 184.6748336100029917 ) ) ;
#60663 = CARTESIAN_POINT ( 'NONE',  ( -2.875850132345000087, 1516.647618671360078, 203.3500485059169876 ) ) ;
#60664 = CARTESIAN_POINT ( 'NONE',  ( 3.959152859930000101, 1428.396642669490120, 216.3690266601789745 ) ) ;
#60665 = CARTESIAN_POINT ( 'NONE',  ( 995.1856855245110864, 1453.395007294999914, 209.1431465539880037 ) ) ;
#60666 = CARTESIAN_POINT ( 'NONE',  ( 10.30934595618430016, 1433.523148449839937, 224.4168098436820173 ) ) ;
#60667 = CARTESIAN_POINT ( 'NONE',  ( -18.80219174870000032, 1449.632368031840087, 192.8071008208980004 ) ) ;
#60668 = FILL_AREA_STYLE_COLOUR ( '', #106654 ) ;
#60669 = VECTOR ( 'NONE', #40906, 1000.000000000000227 ) ;
#60670 = CARTESIAN_POINT ( 'NONE',  ( 41.65674512606190660, 1443.992382921810076, 135.6789720546150022 ) ) ;
#60672 = VERTEX_POINT ( 'NONE', #92748 ) ;
#60671 = CARTESIAN_POINT ( 'NONE',  ( -59.57269385937500061, 1379.722641775480042, 264.7994946068799891 ) ) ;
#60673 = EDGE_CURVE ( 'NONE', #19921, #107891, #34773, .T. ) ;
#60674 = ORIENTED_EDGE ( 'NONE', *, *, #100474, .F. ) ;
#60675 = CARTESIAN_POINT ( 'NONE',  ( 11.18588343651039985, 1434.156361913030196, 151.6248574816150096 ) ) ;
#60676 = CARTESIAN_POINT ( 'NONE',  ( 26.63180687360000221, 1507.995766902830155, 215.9642881313679936 ) ) ;
#60677 = ORIENTED_EDGE ( 'NONE', *, *, #78500, .T. ) ;
#60678 = CARTESIAN_POINT ( 'NONE',  ( -0.0002529191108078910699, 1396.476793851151797, 221.5132489248241541 ) ) ;
#60679 = CARTESIAN_POINT ( 'NONE',  ( -10.34864842518480010, 1447.803587913199863, 209.5966951726140053 ) ) ;
#60680 = CARTESIAN_POINT ( 'NONE',  ( 4.136749821589959630, 1515.492902831140100, 206.2237468939180189 ) ) ;
#60682 = CARTESIAN_POINT ( 'NONE',  ( 9.393138309199999370, 1428.175987565129844, 133.6118001900980232 ) ) ;
#60681 = CARTESIAN_POINT ( 'NONE',  ( 16.08363593346519949, 1424.545651981700075, 191.0941551133240068 ) ) ;
#60683 = CARTESIAN_POINT ( 'NONE',  ( 17.62975177240000235, 1507.813572038729944, 230.7540342202979957 ) ) ;
#60684 = AXIS2_PLACEMENT_3D ( 'NONE', #24782, #9659, #59534 ) ;
#60685 = DIRECTION ( 'NONE',  ( -1.000000000000000000, -0.000000000000000000, -0.000000000000000000 ) ) ;
#60686 = STYLED_ITEM ( 'NONE', ( #39832 ), #11085 ) ;
#60687 = CARTESIAN_POINT ( 'NONE',  ( -0.2210648318990000027, 1414.913060387329779, 192.7531927952979913 ) ) ;
#60688 = CARTESIAN_POINT ( 'NONE',  ( 15.83431121279999942, 1409.466006706529924, 225.8541798896980026 ) ) ;
#60689 = B_SPLINE_SURFACE_WITH_KNOTS ( 'NONE', 5, 1, ( 
 ( #108861, #106648 ),
 ( #38340, #107208 ),
 ( #97706, #29939 ),
 ( #65227, #55182 ),
 ( #98803, #4742 ),
 ( #108312, #90952 ) ),
 .UNSPECIFIED., .F., .F., .F.,
 ( 6, 6 ),
 ( 2, 2 ),
 ( 0.000000000000000000, 3.267792473789999708 ),
 ( 0.000000000000000000, 14.00000000000000000 ),
 .UNSPECIFIED. ) ;
#60690 = CARTESIAN_POINT ( 'NONE',  ( -7.321193745875000047, 1516.534976163889951, 211.4135222436570132 ) ) ;
#60691 = CARTESIAN_POINT ( 'NONE',  ( 13.77282262629899989, 1415.219159636060112, 197.5495014860289871 ) ) ;
#60692 = CARTESIAN_POINT ( 'NONE',  ( -14.39765041480000107, 1420.835238719779909, 210.6164402859990048 ) ) ;
#60693 = CARTESIAN_POINT ( 'NONE',  ( 5.919280288264999079, 1513.965983108850196, 201.4800680737670007 ) ) ;
#60694 = ORIENTED_EDGE ( 'NONE', *, *, #7436, .F. ) ;
#60695 = CARTESIAN_POINT ( 'NONE',  ( 14.34562267347200049, 1435.962350135230054, 149.9318665393219874 ) ) ;
#60696 = CARTESIAN_POINT ( 'NONE',  ( -0.7140353930058549459, 1431.991569043200116, 200.7371223997279799 ) ) ;
#60697 = ORIENTED_EDGE ( 'NONE', *, *, #21983, .T. ) ;
#60698 = VERTEX_POINT ( 'NONE', #26083 ) ;
#60699 = CARTESIAN_POINT ( 'NONE',  ( -7.532473206385000175, 1513.265135866640094, 216.4259342199370053 ) ) ;
#60700 = CARTESIAN_POINT ( 'NONE',  ( 16.50477753120586755, 1512.979858876954040, 197.3152680210698122 ) ) ;
#60701 = CARTESIAN_POINT ( 'NONE',  ( -11.74583952262180020, 1503.658476107915476, 208.1214586907342152 ) ) ;
#60702 = CARTESIAN_POINT ( 'NONE',  ( -5.003848160104999998, 1517.005755693489846, 216.4561742428970206 ) ) ;
#60703 = CARTESIAN_POINT ( 'NONE',  ( 3.030007752585599956, 1466.220774424609772, 198.4981827063209892 ) ) ;
#60704 = EDGE_CURVE ( 'NONE', #9968, #32551, #52612, .T. ) ;
#60705 = AXIS2_PLACEMENT_3D ( 'NONE', #58780, #92918, #8352 ) ;
#60706 = CARTESIAN_POINT ( 'NONE',  ( 12.13377226363930106, 1421.785238798449882, 208.4657368268529751 ) ) ;
#60707 = CARTESIAN_POINT ( 'NONE',  ( -35.65618109042815576, 1379.642124534350387, 218.6101405679489176 ) ) ;
#60708 = CARTESIAN_POINT ( 'NONE',  ( 4.285590139556119560, 1446.892837359970144, 155.6593302246760118 ) ) ;
#60709 = CIRCLE ( 'NONE', #40758, 2.000000000550006263 ) ;
#60710 = EDGE_CURVE ( 'NONE', #37252, #29545, #87024, .T. ) ;
#60711 = CARTESIAN_POINT ( 'NONE',  ( 0.02089333571419999674, 1507.111761158929994, 237.3522808961980104 ) ) ;
#60712 = EDGE_LOOP ( 'NONE', ( #48704, #72263, #65342, #12904, #87555 ) ) ;
#60713 = CARTESIAN_POINT ( 'NONE',  ( 0.7351097711180020200, 1516.977504706749869, 206.6301902066870184 ) ) ;
#60714 = ORIENTED_EDGE ( 'NONE', *, *, #54852, .F. ) ;
#60715 = CARTESIAN_POINT ( 'NONE',  ( -105.5930000624190086, 1378.287466303110023, 305.0491164647540359 ) ) ;
#60716 = CARTESIAN_POINT ( 'NONE',  ( -18.97264762389999859, 1509.488247232329968, 230.9952461704979783 ) ) ;
#60717 = ORIENTED_EDGE ( 'NONE', *, *, #67242, .F. ) ;
#60718 = CARTESIAN_POINT ( 'NONE',  ( -5.513225751105480299, 1508.611141565010030, 201.8002151886680053 ) ) ;
#60719 = CARTESIAN_POINT ( 'NONE',  ( -12.96785963179999968, 1409.365908024330110, 191.2854579259980312 ) ) ;
#60720 = DIRECTION ( 'NONE',  ( -1.000000000000000000, 0.000000000000000000, -1.942890293094025713E-13 ) ) ;
#60722 = ORIENTED_EDGE ( 'NONE', *, *, #55442, .F. ) ;
#60721 = CARTESIAN_POINT ( 'NONE',  ( -0.8537895742897508855, 1422.738976114379966, 192.5159534119239879 ) ) ;
#60723 = CARTESIAN_POINT ( 'NONE',  ( 19.74776305319999636, 1427.029108294729895, 221.9964930508980103 ) ) ;
#60724 = DIRECTION ( 'NONE',  ( 0.9455185755993178454, 0.000000000000000000, -0.3255681544571537578 ) ) ;
#60725 = CARTESIAN_POINT ( 'NONE',  ( -3.945738874726128387, 1515.565581977718466, 207.8717498098853014 ) ) ;
#60726 = CARTESIAN_POINT ( 'NONE',  ( -18.17365796220000007, 1441.208305948289762, 213.5442559039389891 ) ) ;
#60728 = CARTESIAN_POINT ( 'NONE',  ( 5.440910205060000671, 1437.356219380560105, 154.7142170579979847 ) ) ;
#60727 = CARTESIAN_POINT ( 'NONE',  ( -5.316196955749758146, 1522.051704408389924, 231.0177287530028423 ) ) ;
#60729 = AXIS2_PLACEMENT_3D ( 'NONE', #61553, #49427, #83549 ) ;
#60730 = B_SPLINE_SURFACE_WITH_KNOTS ( 'NONE', 5, 5, ( 
 ( #17519, #51721, #19176, #69645, #104316, #770 ),
 ( #2444, #60688, #94812, #61794, #95916, #102093 ),
 ( #18088, #59567, #103768, #52283, #27070, #61254 ),
 ( #95369, #51161, #18632, #85288, #98659, #71311 ),
 ( #89712, #12990, #107066, #106517, #29806, #70758 ),
 ( #11913, #37110, #105424, #46089, #90252, #46639 ),
 ( #88086, #4616, #47173, #28715, #11374, #21923 ),
 ( #81301, #12457, #13534, #55588, #62921, #38750 ),
 ( #55039, #56118, #96472, #54498, #5154, #72927 ),
 ( #80221, #62347, #30351, #97031, #64542, #45545 ),
 ( #89166, #72388, #47720, #81851, #80773, #19751 ),
 ( #104869, #20294, #28158, #88634, #53952, #63994 ),
 ( #79685, #2991, #4080, #3539, #38205, #37662 ),
 ( #98105, #71868, #105985, #97571, #29260, #63452 ),
 ( #20843, #21379, #101383, #84060, #82424, #73482 ) ),
 .UNSPECIFIED., .F., .F., .F.,
 ( 6, 3, 3, 3, 6 ),
 ( 6, 6 ),
 ( 21.66346097059999920, 24.40199430689999716, 27.78806269829999920, 31.17413108959999946, 40.68480120859999971 ),
 ( 0.000000000000000000, 1.455162240349999969 ),
 .UNSPECIFIED. ) ;
#60731 = CARTESIAN_POINT ( 'NONE',  ( 2.488360629304999794, 1516.616791731099966, 214.8929950451170043 ) ) ;
#60732 = CARTESIAN_POINT ( 'NONE',  ( -3.625688031972540415, 1428.567653792310011, 200.4907183003010118 ) ) ;
#60733 = DIRECTION ( 'NONE',  ( -0.6709778558543689764, 0.000000000000000000, 0.7414773880254701410 ) ) ;
#60734 = CARTESIAN_POINT ( 'NONE',  ( 27.92763725140000020, 1508.597377706630141, 207.9063415346780062 ) ) ;
#60735 = CARTESIAN_POINT ( 'NONE',  ( 2.881222757585000238, 1516.891731298979948, 211.5992195760969707 ) ) ;
#60736 = CARTESIAN_POINT ( 'NONE',  ( -11.83148041523059923, 1482.212593895280179, 207.9057076157649817 ) ) ;
#60737 = CARTESIAN_POINT ( 'NONE',  ( 30.04653961079798208, 1524.739915903632891, 222.3142848390757251 ) ) ;
#60739 = ORIENTED_EDGE ( 'NONE', *, *, #108907, .T. ) ;
#60738 = CARTESIAN_POINT ( 'NONE',  ( -85.13767067070000394, 1388.281031823789817, 290.5355680588589848 ) ) ;
#60740 = VECTOR ( 'NONE', #79368, 1000.000000000000000 ) ;
#60741 = CARTESIAN_POINT ( 'NONE',  ( 18.32013006829999924, 1469.450921912629838, 259.8063787264979965 ) ) ;
#60742 = CARTESIAN_POINT ( 'NONE',  ( 10.76075704858850024, 1490.821908851660055, 211.3234342363890050 ) ) ;
#60743 = CARTESIAN_POINT ( 'NONE',  ( 11.18076303840566155, 1522.051704408389924, 204.2578997804941707 ) ) ;
#60744 = CARTESIAN_POINT ( 'NONE',  ( -8.365520703090000509, 1508.201466052729984, 235.3634618713980160 ) ) ;
#60745 = CARTESIAN_POINT ( 'NONE',  ( -23.04921901699999864, 1449.613099141539806, 219.4632572156979791 ) ) ;
#60747 = CARTESIAN_POINT ( 'NONE',  ( 17.64171352730929954, 1409.900445066939938, 222.6954652476910042 ) ) ;
#60746 = CARTESIAN_POINT ( 'NONE',  ( 11.31243771429999967, 1433.012838418620049, 151.5204583748979985 ) ) ;
#60748 = CARTESIAN_POINT ( 'NONE',  ( -9.244699677152100392, 1448.612501353059997, 209.9872400869060129 ) ) ;
#60749 = CARTESIAN_POINT ( 'NONE',  ( -108.0218370616639874, 1383.106230495490308, 310.8121610381319897 ) ) ;
#60750 = ORIENTED_EDGE ( 'NONE', *, *, #86442, .F. ) ;
#60751 = CARTESIAN_POINT ( 'NONE',  ( -4.620008245204999753, 1516.777260590120022, 203.3472363101570011 ) ) ;
#60752 = CARTESIAN_POINT ( 'NONE',  ( 0.2135597935630000055, 1406.506901924230078, 269.4986771210980123 ) ) ;
#60753 = CARTESIAN_POINT ( 'NONE',  ( -16.68463225830000241, 1445.052233488290085, 162.0935120917980043 ) ) ;
#60754 = AXIS2_PLACEMENT_3D ( 'NONE', #45979, #37562, #18530 ) ;
#60755 = DIRECTION ( 'NONE',  ( 1.000000000000000000, 2.249639673992764790E-32, 1.224646799147350002E-16 ) ) ;
#60756 = FACE_OUTER_BOUND ( 'NONE', #54893, .T. ) ;
#60757 = CARTESIAN_POINT ( 'NONE',  ( -40.19808943040000315, 1445.100537817090071, 136.9456357583980264 ) ) ;
#60758 = FACE_OUTER_BOUND ( 'NONE', #106700, .T. ) ;
#60759 = CARTESIAN_POINT ( 'NONE',  ( -41.30732298605509811, 1440.913060409350010, 261.0633855307339672 ) ) ;
#60760 = VECTOR ( 'NONE', #37596, 1000.000000000000227 ) ;
#60761 = CARTESIAN_POINT ( 'NONE',  ( -25.87097295179999890, 1447.207377453609979, 138.1950503254980163 ) ) ;
#60762 = CARTESIAN_POINT ( 'NONE',  ( 3.996802888650000299E-15, 1462.614442895030152, 248.0989693021979861 ) ) ;
#60763 = CARTESIAN_POINT ( 'NONE',  ( -109.7278721679999904, 1385.840206276699973, 297.1154854894589903 ) ) ;
#60764 = CARTESIAN_POINT ( 'NONE',  ( 11.77838848180700104, 1479.583172727889860, 209.4916819176700074 ) ) ;
#60765 = CARTESIAN_POINT ( 'NONE',  ( 5.095071723817279796, 1506.876855224960082, 219.6410062831469929 ) ) ;
#60766 = CARTESIAN_POINT ( 'NONE',  ( -41.84160635743404555, 1444.586462184261563, 269.6439780239310835 ) ) ;
#60767 = ORIENTED_EDGE ( 'NONE', *, *, #36509, .F. ) ;
#60768 = CIRCLE ( 'NONE', #92935, 0.9999999999999972244 ) ;
#60769 = CARTESIAN_POINT ( 'NONE',  ( -43.50000000000000000, 1440.913060387330006, 271.1218459616979999 ) ) ;
#60770 = CARTESIAN_POINT ( 'NONE',  ( 12.06145328220000046, 1433.903212736219984, 146.4342173386980051 ) ) ;
#60771 = CARTESIAN_POINT ( 'NONE',  ( -22.08622291482368638, 1523.382868172864164, 184.4183880513178337 ) ) ;
#60772 = CARTESIAN_POINT ( 'NONE',  ( 16.67515766384740061, 1499.299502726869832, 188.3559378578410133 ) ) ;
#60773 = CARTESIAN_POINT ( 'NONE',  ( -0.4730976197839999453, 1415.788367959630023, 233.4112646266979993 ) ) ;
#60775 = CARTESIAN_POINT ( 'NONE',  ( 12.98226713004290112, 1414.913060387349788, 198.3280232619060257 ) ) ;
#60774 = CARTESIAN_POINT ( 'NONE',  ( 11.76282542499999906, 1501.584099486789910, 210.8989423168290216 ) ) ;
#60776 = CARTESIAN_POINT ( 'NONE',  ( -28.32265146449999804, 1509.673549455229931, 210.9825397907879960 ) ) ;
#60777 = CARTESIAN_POINT ( 'NONE',  ( 7.984492602029999553, 1423.987908843459991, 211.8850966666189777 ) ) ;
#60778 = CARTESIAN_POINT ( 'NONE',  ( -17.51671525713139843, 1384.869800455989889, 220.0655268698560008 ) ) ;
#60779 = CIRCLE ( 'NONE', #17789, 1.999999999999999556 ) ;
#60780 = CARTESIAN_POINT ( 'NONE',  ( -7.872185816540564929, 1417.087241613852939, 230.9975226091719662 ) ) ;
#60781 = CARTESIAN_POINT ( 'NONE',  ( -18.95816141779999953, 1416.822690122629865, 207.7797354037080027 ) ) ;
#60782 = CARTESIAN_POINT ( 'NONE',  ( -16.09938272070019849, 1414.913060387399810, 208.8977458501949798 ) ) ;
#60783 = CARTESIAN_POINT ( 'NONE',  ( 24.76897219210000145, 1435.437797603480021, 136.5355265435979959 ) ) ;
#60784 = CARTESIAN_POINT ( 'NONE',  ( -8.919399434642100388, 1396.224532680279935, 202.5884989200089876 ) ) ;
#60785 = ORIENTED_EDGE ( 'NONE', *, *, #66585, .F. ) ;
#60786 = CARTESIAN_POINT ( 'NONE',  ( -17.25862514696109784, 1410.597661782969908, 225.9222092880160062 ) ) ;
#60787 = CARTESIAN_POINT ( 'NONE',  ( 9.709302419510001059, 1435.943783413959864, 148.7752736812980174 ) ) ;
#60788 = ORIENTED_EDGE ( 'NONE', *, *, #69222, .F. ) ;
#60789 = ORIENTED_EDGE ( 'NONE', *, *, #102212, .T. ) ;
#60790 = CARTESIAN_POINT ( 'NONE',  ( 3.895917434060000240, 1499.417515733289974, 230.0327334827989887 ) ) ;
#60791 = CARTESIAN_POINT ( 'NONE',  ( 7.500396670941167798, 1516.934665496271919, 209.1219157010845322 ) ) ;
#60793 = CARTESIAN_POINT ( 'NONE',  ( -1.299578229957530029, 1457.370843945099978, 219.6854510378979910 ) ) ;
#60792 = CARTESIAN_POINT ( 'NONE',  ( 11.08043720809999932, 1426.486562227929880, 96.53290481169779014 ) ) ;
#60794 = CARTESIAN_POINT ( 'NONE',  ( -0.5711511081509990095, 1457.745025693589923, 202.2735493682390029 ) ) ;
#60795 = CARTESIAN_POINT ( 'NONE',  ( -11.16671941230000087, 1433.086908617769950, 151.6208637079979837 ) ) ;
#60796 = CARTESIAN_POINT ( 'NONE',  ( -2.505371996947532764, 1421.285840239624122, 184.5372720782322062 ) ) ;
#60797 = CARTESIAN_POINT ( 'NONE',  ( 7.545761559389999817, 1424.826522491729975, 212.1621923280889916 ) ) ;
#60798 = B_SPLINE_CURVE_WITH_KNOTS ( 'NONE', 3,
 ( #88804, #37854, #27241, #19369, #54129, #106156, #61978, #11549, #27790, #29434, #72039, #2066, #53571, #3722, #88256, #36197, #63633, #45725, #70381, #95545, #18818, #87718, #78750, #79862, #21018, #37304, #3172, #12087, #10436, #105617, #9881, #104498, #28901, #63097, #45169, #80409, #86590, #44050, #78188, #4784 ),
 .UNSPECIFIED., .F., .F.,
 ( 4, 3, 3, 3, 3, 3, 3, 3, 3, 3, 3, 3, 3, 4 ),
 ( 0.8628048341553139489, 0.9513106579048509204, 1.049709543750630081, 1.141232170367520116, 1.227831679639869833, 1.304547853099820021, 1.314431188912210002, 1.386913577912220141, 1.463820618845149912, 1.546979327982200170, 1.643200469919150031, 1.736730672401769926, 1.817733512948600083, 1.883620747549999752 ),
 .UNSPECIFIED. ) ;
#60799 = CARTESIAN_POINT ( 'NONE',  ( 7.755379691499999062, 1459.738853293389866, 228.9106028235989925 ) ) ;
#60800 = CARTESIAN_POINT ( 'NONE',  ( 7.823092546549999859, 1509.180139508929869, 181.1432147337980041 ) ) ;
#60801 = CARTESIAN_POINT ( 'NONE',  ( 2.499404917449999708, 1449.013041636889966, 182.6008070574980025 ) ) ;
#60802 = CARTESIAN_POINT ( 'NONE',  ( 8.099654910236120386, 1364.797801192799852, 208.3718459617061285 ) ) ;
#60804 = VERTEX_POINT ( 'NONE', #64566 ) ;
#60803 = CARTESIAN_POINT ( 'NONE',  ( 4.974027067470000674, 1455.144349094690142, 217.5915564868190017 ) ) ;
#60805 = ORIENTED_EDGE ( 'NONE', *, *, #109539, .T. ) ;
#60806 = ADVANCED_FACE ( 'NONE', ( #38775 ), #96629, .F. ) ;
#60807 = CARTESIAN_POINT ( 'NONE',  ( -40.26396437200000378, 1444.186536724029793, 137.1012290770979973 ) ) ;
#60808 = CARTESIAN_POINT ( 'NONE',  ( 7.461942709067347579, 1510.835436365588748, 202.9437500974225657 ) ) ;
#60809 = CARTESIAN_POINT ( 'NONE',  ( -2.328501808469999990, 1473.856926935030060, 270.2917565481980091 ) ) ;
#60810 = CARTESIAN_POINT ( 'NONE',  ( 7.568706834503317715, 1500.286747494142901, 200.6010021183646472 ) ) ;
#60811 = CARTESIAN_POINT ( 'NONE',  ( -2.043810040229999903, 1485.976622560129954, 182.1080309692979995 ) ) ;
#60812 = VECTOR ( 'NONE', #44269, 1000.000000000000000 ) ;
#60813 = CARTESIAN_POINT ( 'NONE',  ( -31.81429855202636858, 1524.964158026965606, 201.5864206136516543 ) ) ;
#60814 = CARTESIAN_POINT ( 'NONE',  ( 14.03281819417741794, 1434.988470691964494, 148.9022204816306783 ) ) ;
#60815 = EDGE_CURVE ( 'NONE', #60256, #88934, #19338, .T. ) ;
#60816 = CARTESIAN_POINT ( 'NONE',  ( 21.13431350049999935, 1409.651086877429861, 206.4149709229679956 ) ) ;
#60817 = SURFACE_SIDE_STYLE ('',( #77048 ) ) ;
#60818 = CARTESIAN_POINT ( 'NONE',  ( -2.500000000000000000, 1448.208035806080034, 170.3313966091649831 ) ) ;
#60819 = CARTESIAN_POINT ( 'NONE',  ( 8.792358245598531852, 1369.487036709539780, 209.6218459617033432 ) ) ;
#60820 = CARTESIAN_POINT ( 'NONE',  ( 15.26728741790000043, 1409.446205812130074, 212.2704896688680094 ) ) ;
#60821 = CARTESIAN_POINT ( 'NONE',  ( -24.18815601759459710, 1410.823802913859936, 267.6036696494369949 ) ) ;
#60822 = FACE_OUTER_BOUND ( 'NONE', #72532, .T. ) ;
#60823 = EDGE_LOOP ( 'NONE', ( #95233, #82550, #106928, #24558 ) ) ;
#60824 = FACE_OUTER_BOUND ( 'NONE', #1307, .T. ) ;
#60825 = CARTESIAN_POINT ( 'NONE',  ( 13.46738723530000037, 1443.320881723499951, 188.5256231623980057 ) ) ;
#60826 = B_SPLINE_SURFACE_WITH_KNOTS ( 'NONE', 5, 5, ( 
 ( #16998, #6982, #7535, #108893, #32186, #110547 ),
 ( #41133, #102133, #50109, #67467, #75314, #76394 ),
 ( #101572, #25412, #84234, #66370, #269, #59604 ),
 ( #50649, #66916, #32736, #84780, #41691, #8625 ),
 ( #8076, #100489, #68570, #75850, #42247, #93721 ),
 ( #51198, #85328, #17562, #42800, #76960, #101025 ) ),
 .UNSPECIFIED., .F., .F., .F.,
 ( 6, 6 ),
 ( 6, 6 ),
 ( 5.893388896115880016, 9.819930328984119328 ),
 ( -0.0002947352041177890396, 0.5000000000000000000 ),
 .UNSPECIFIED. ) ;
#60827 = ORIENTED_EDGE ( 'NONE', *, *, #84518, .F. ) ;
#60828 = ORIENTED_EDGE ( 'NONE', *, *, #15472, .F. ) ;
#60829 = FACE_OUTER_BOUND ( 'NONE', #94020, .T. ) ;
#60830 = CARTESIAN_POINT ( 'NONE',  ( -7.450033292399999674, 1367.931913175460068, 207.6218459616989946 ) ) ;
#60831 = CARTESIAN_POINT ( 'NONE',  ( -6.548821979184999975, 1516.688761843659904, 213.1592242262869945 ) ) ;
#60832 = CARTESIAN_POINT ( 'NONE',  ( -16.64354896040000042, 1485.485022283829949, 188.0123015010980225 ) ) ;
#60833 = ORIENTED_EDGE ( 'NONE', *, *, #96028, .F. ) ;
#60834 = CARTESIAN_POINT ( 'NONE',  ( -105.6883447180000104, 1374.461008904089795, 304.2218452742590102 ) ) ;
#60835 = CARTESIAN_POINT ( 'NONE',  ( 10.06907646880000051, 1416.520322351229879, 224.7759792403979873 ) ) ;
#60836 = CARTESIAN_POINT ( 'NONE',  ( -2.294209667535000108, 1516.603620185149794, 203.3509623682169831 ) ) ;
#60837 = TOROIDAL_SURFACE ( 'NONE', #93002, 10.71315034250000053, 1.000000000000000000 ) ;
#60838 = CARTESIAN_POINT ( 'NONE',  ( -26.76880870690000336, 1508.588124793430097, 202.6010433452480015 ) ) ;
#60839 = B_SPLINE_SURFACE_WITH_KNOTS ( 'NONE', 5, 5, ( 
 ( #87640, #110618, #17067, #85397, #34465, #68641, #77578, #18198, #103296 ),
 ( #102741, #1420, #26037, #60230, #17627, #51832, #103873, #85969, #35009 ),
 ( #69190, #60800, #35560, #27173, #69756, #61358, #38313, #3101, #13640 ),
 ( #55155, #12573, #47280, #2550, #88738, #71426, #56232, #45656, #36675 ),
 ( #22035, #97132, #98221, #79795, #20401, #70868, #105542, #4715, #55703 ),
 ( #46753, #12022, #11480, #89276, #37230, #46202, #90362, #19858, #21491 ),
 ( #28829, #89824, #13096, #80336, #97677, #80884, #81403, #63027, #73037 ),
 ( #4180, #88188, #64100, #72492, #107176, #104981, #96586, #38859, #3653 ),
 ( #37782, #54606, #106083, #71971, #30468, #29361, #63562, #28271, #106621 ) ),
 .UNSPECIFIED., .F., .F., .F.,
 ( 6, 3, 6 ),
 ( 6, 3, 6 ),
 ( 51.29209723529999820, 55.80647300139999345, 63.23243013249999933 ),
 ( 0.000000000000000000, 1.000000000000000000, 2.000000000000000000 ),
 .UNSPECIFIED. ) ;
#60840 = CARTESIAN_POINT ( 'NONE',  ( -1.530913323750000110, 1457.944503865530123, 229.8438706612979843 ) ) ;
#60841 = CARTESIAN_POINT ( 'NONE',  ( -50.84652256599999731, 1385.021217850319999, 226.1755936018590205 ) ) ;
#60842 = CARTESIAN_POINT ( 'NONE',  ( -65.64734824971920091, 1384.709125050150305, 256.5005590946320240 ) ) ;
#60843 = CARTESIAN_POINT ( 'NONE',  ( -5.096744314220000405, 1407.739527842629968, 197.0259025076979924 ) ) ;
#60844 = CARTESIAN_POINT ( 'NONE',  ( -13.86092708470000012, 1410.765486845930127, 227.1170267252979897 ) ) ;
#60845 = AXIS2_PLACEMENT_3D ( 'NONE', #35728, #79945, #21108 ) ;
#60847 = ORIENTED_EDGE ( 'NONE', *, *, #44574, .T. ) ;
#60846 = CARTESIAN_POINT ( 'NONE',  ( -4.161170380569999772, 1448.299083496910043, 185.1109000857979936 ) ) ;
#60848 = CARTESIAN_POINT ( 'NONE',  ( -25.80250405271350189, 1449.911705762070142, 209.5154266393010118 ) ) ;
#60849 = CARTESIAN_POINT ( 'NONE',  ( 27.85639448530000095, 1508.131721228930019, 211.5797927016579933 ) ) ;
#60850 = CARTESIAN_POINT ( 'NONE',  ( 10.60194594222889819, 1460.225020076690043, 206.5389690418479915 ) ) ;
#60851 = CARTESIAN_POINT ( 'NONE',  ( -25.11961111550000325, 1435.876096999659921, 137.1228181144979601 ) ) ;
#60853 = CARTESIAN_POINT ( 'NONE',  ( 2.880592928985000079, 1516.859514182039902, 211.9868180862470126 ) ) ;
#60852 = CIRCLE ( 'NONE', #12551, 1.000000000000000888 ) ;
#60854 = CARTESIAN_POINT ( 'NONE',  ( -68.68965169780000224, 1379.747958860950121, 279.9890510275590145 ) ) ;
#60855 = CARTESIAN_POINT ( 'NONE',  ( -13.86092830220000138, 1410.765486874730186, 227.1170284388979894 ) ) ;
#60856 = CARTESIAN_POINT ( 'NONE',  ( 7.334062741534030039, 1482.070311934039864, 210.1443595876939696 ) ) ;
#60857 = CARTESIAN_POINT ( 'NONE',  ( 17.74493927494756917, 1410.896455599894807, 193.0440146115597884 ) ) ;
#60858 = SHAPE_REPRESENTATION ( 'Cutting Blade', ( #21632 ), #78983 ) ;
#60859 = CARTESIAN_POINT ( 'NONE',  ( 1.122033391945000069, 1516.972341476009888, 208.3659064338399673 ) ) ;
#60860 = ORIENTED_EDGE ( 'NONE', *, *, #110417, .F. ) ;
#60861 = DIRECTION ( 'NONE',  ( 0.005791248591755682358, -0.9990828997313954130, -0.04242429615273902305 ) ) ;
#60862 = CARTESIAN_POINT ( 'NONE',  ( -5.198406060209999957, 1412.834820857829982, 231.9113671903980105 ) ) ;
#60863 = CARTESIAN_POINT ( 'NONE',  ( -27.62433227900000077, 1384.972991153419798, 225.6333370715589979 ) ) ;
#60864 = ORIENTED_EDGE ( 'NONE', *, *, #58492, .T. ) ;
#60865 = CARTESIAN_POINT ( 'NONE',  ( -15.94747805094890225, 1385.291421466249858, 219.6205707809359922 ) ) ;
#60866 = CARTESIAN_POINT ( 'NONE',  ( -3.567860816820000114, 1429.016874681090030, 201.2351213331789950 ) ) ;
#60867 = CARTESIAN_POINT ( 'NONE',  ( 12.71795666588089979, 1434.880588916799979, 150.2406740331289825 ) ) ;
#60868 = CARTESIAN_POINT ( 'NONE',  ( 16.70365182916559732, 1488.409533293340019, 230.3427702791729814 ) ) ;
#60869 = CARTESIAN_POINT ( 'NONE',  ( -22.16710374047699972, 1508.409791915999904, 225.9459590737800170 ) ) ;
#60870 = CARTESIAN_POINT ( 'NONE',  ( -1.804213505890000180, 1410.351307731129964, 186.0507930254979954 ) ) ;
#60871 = CARTESIAN_POINT ( 'NONE',  ( 1.869907053503540029, 1431.184470418000046, 218.4272402479099924 ) ) ;
#60872 = DIRECTION ( 'NONE',  ( 1.000000000000000000, 0.000000000000000000, 0.000000000000000000 ) ) ;
#60873 = AXIS2_PLACEMENT_3D ( 'NONE', #22551, #57326, #56754 ) ;
#60875 = CARTESIAN_POINT ( 'NONE',  ( 10.77497579070000100, 1480.716349263289885, 211.2103358511090221 ) ) ;
#60874 = CARTESIAN_POINT ( 'NONE',  ( -1.706797824074999914, 1517.164987839469859, 214.9112406324369999 ) ) ;
#60876 = CARTESIAN_POINT ( 'NONE',  ( 19.59880151960000205, 1507.802454151830034, 188.8055342685979952 ) ) ;
#60877 = CARTESIAN_POINT ( 'NONE',  ( -6.941727290454999810, 1516.882217593000178, 216.4530290611770056 ) ) ;
#60878 = ORIENTED_EDGE ( 'NONE', *, *, #33065, .F. ) ;
#60879 = CARTESIAN_POINT ( 'NONE',  ( 1.126138108584999964, 1517.208444099459939, 201.3951612445669923 ) ) ;
#60880 = DIRECTION ( 'NONE',  ( 9.500914144214121536E-47, -1.000000000000000000, 1.836970198721029688E-16 ) ) ;
#60881 = ORIENTED_EDGE ( 'NONE', *, *, #6388, .F. ) ;
#60882 = CARTESIAN_POINT ( 'NONE',  ( 2.250613398900000117, 1417.526871923430008, 235.1186440458980087 ) ) ;
#60883 = B_SPLINE_CURVE_WITH_KNOTS ( 'NONE', 5,
 ( #99211, #74048, #23056, #91392, #14670, #50501, #100335, #23622, #41540 ),
 .UNSPECIFIED., .F., .F.,
 ( 6, 3, 6 ),
 ( 0.000000000000000000, 0.9031158850279928929, 1.000000000000000000 ),
 .UNSPECIFIED. ) ;
#60884 = CARTESIAN_POINT ( 'NONE',  ( -3.829620113550000315, 1515.551704408389924, 207.2788837304390199 ) ) ;
#60885 = CARTESIAN_POINT ( 'NONE',  ( 2.774855403480000149, 1441.656174316490024, 218.2502874549990111 ) ) ;
#60886 = CARTESIAN_POINT ( 'NONE',  ( -33.45065857237997875, 1524.841055067850220, 198.7780394437810401 ) ) ;
#60887 = CARTESIAN_POINT ( 'NONE',  ( -21.63718167644571722, 1524.600389084707103, 234.6742851132877945 ) ) ;
#60888 = AXIS2_PLACEMENT_3D ( 'NONE', #11835, #62840, #63911 ) ;
#60889 = CARTESIAN_POINT ( 'NONE',  ( -2.500000000000000000, 1448.831161628929976, 156.2564907446979987 ) ) ;
#60890 = CARTESIAN_POINT ( 'NONE',  ( 32.02808312589916540, 1512.187213306747481, 198.2787714533495489 ) ) ;
#60891 = CARTESIAN_POINT ( 'NONE',  ( -7.125888594031689394, 1458.093400128074336, 215.4885673113955136 ) ) ;
#60892 = LINE ( 'NONE', #68734, #70024 ) ;
#60893 = DIRECTION ( 'NONE',  ( 1.755985294532464991E-16, -1.000000000000000000, 1.338183447452830017E-16 ) ) ;
#60895 = CARTESIAN_POINT ( 'NONE',  ( 4.329089011153910427, 1515.078531749479907, 207.6981595341280240 ) ) ;
#60894 = CARTESIAN_POINT ( 'NONE',  ( -10.14847552845580125, 1472.086894961059897, 209.7189879088959685 ) ) ;
#60896 = CARTESIAN_POINT ( 'NONE',  ( 0.5624690339869999889, 1416.828040475229955, 190.4759594386979984 ) ) ;
#60897 = EDGE_LOOP ( 'NONE', ( #25653, #97931, #70356, #66205 ) ) ;
#60898 = CARTESIAN_POINT ( 'NONE',  ( 1.555728358237469910, 1415.258594621700013, 191.1344422060440138 ) ) ;
#60899 = CARTESIAN_POINT ( 'NONE',  ( -4.554948924557931100, 1508.731372610989865, 211.6097697110380125 ) ) ;
#60900 = CARTESIAN_POINT ( 'NONE',  ( -24.35286325639999916, 1437.423069115099906, 210.8262286111179833 ) ) ;
#60901 = CARTESIAN_POINT ( 'NONE',  ( 8.490083184937372351, 1410.581744779529799, 187.8574485642506318 ) ) ;
#60902 = DIRECTION ( 'NONE',  ( -1.755985294532469921E-16, 1.000000000000000000, -1.338183447452830017E-16 ) ) ;
#60903 = CARTESIAN_POINT ( 'NONE',  ( -5.682125987650000098, 1507.354943063129895, 181.2351845632980201 ) ) ;
#60904 = CARTESIAN_POINT ( 'NONE',  ( -11.08201610607340015, 1470.229490766139861, 211.6946857826129929 ) ) ;
#60905 = CARTESIAN_POINT ( 'NONE',  ( -4.633397090840619903, 1377.913060387289988, 204.3568503472270095 ) ) ;
#60906 = CARTESIAN_POINT ( 'NONE',  ( 14.43086732081240164, 1426.807478003820052, 195.4949745959340248 ) ) ;
#60907 = CARTESIAN_POINT ( 'NONE',  ( -58.77327825612210432, 1383.798380756109964, 278.4814665550280210 ) ) ;
#60908 = CARTESIAN_POINT ( 'NONE',  ( 10.51221079110000112, 1452.545965898430040, 151.2436542503979808 ) ) ;
#60909 = CARTESIAN_POINT ( 'NONE',  ( -5.105764674260594660, 1391.864935413667126, 214.6138670560712285 ) ) ;
#60910 = DIRECTION ( 'NONE',  ( -0.9702683578407158560, 7.674209871302701496E-33, 0.2420316379589265432 ) ) ;
#60912 = ORIENTED_EDGE ( 'NONE', *, *, #8257, .F. ) ;
#60911 = CARTESIAN_POINT ( 'NONE',  ( 10.55831763905420040, 1452.305717713109971, 208.8223436732269818 ) ) ;
#60913 = CARTESIAN_POINT ( 'NONE',  ( -1.499137301450000237, 1414.988015881430101, 226.5174425183980134 ) ) ;
#60914 = CARTESIAN_POINT ( 'NONE',  ( -78.74259975059999306, 1381.827890489759966, 283.5083833816589731 ) ) ;
#60915 = CARTESIAN_POINT ( 'NONE',  ( 30.31940284292419818, 1523.382868172864164, 222.4933038710543087 ) ) ;
#60916 = ORIENTED_EDGE ( 'NONE', *, *, #36296, .F. ) ;
#60917 = ORIENTED_EDGE ( 'NONE', *, *, #16880, .F. ) ;
#60918 = CARTESIAN_POINT ( 'NONE',  ( 14.26923756360000084, 1444.927653052269989, 189.5513799252980220 ) ) ;
#60919 = CARTESIAN_POINT ( 'NONE',  ( -2.458567915935879533, 1456.374676718179899, 215.3392989940770121 ) ) ;
#60920 = CARTESIAN_POINT ( 'NONE',  ( 39.05972573424099892, 1439.798937998340080, 136.7091803653709974 ) ) ;
#60922 = CARTESIAN_POINT ( 'NONE',  ( -37.00345278059999998, 1461.786582490830142, 266.5575584642980402 ) ) ;
#60921 = DIRECTION ( 'NONE',  ( -0.000000000000000000, -1.000000000000000000, -0.000000000000000000 ) ) ;
#60923 = CARTESIAN_POINT ( 'NONE',  ( 8.589517928433638261, 1436.682903382349878, 208.3531420449839686 ) ) ;
#60924 = CARTESIAN_POINT ( 'NONE',  ( -108.9551702540000093, 1381.838302694970025, 297.6631244000589618 ) ) ;
#60925 = CARTESIAN_POINT ( 'NONE',  ( -0.3241128059390138150, 1452.022536283229101, 183.1062973748274203 ) ) ;
#60926 = CARTESIAN_POINT ( 'NONE',  ( -19.96587381370000003, 1485.439095484030076, 190.8600527859979934 ) ) ;
#60927 = CARTESIAN_POINT ( 'NONE',  ( 3.782002931730000128, 1409.981075011729899, 185.9772857123979861 ) ) ;
#60928 = CARTESIAN_POINT ( 'NONE',  ( -1.244053264164739936, 1485.816359186060026, 197.2880502459559864 ) ) ;
#60929 = CARTESIAN_POINT ( 'NONE',  ( -10.64187455999999976, 1435.613678569329977, 152.0651246931979870 ) ) ;
#60930 = CARTESIAN_POINT ( 'NONE',  ( 8.091201492491240543, 1435.785803388039994, 206.2618594566330046 ) ) ;
#60931 = CARTESIAN_POINT ( 'NONE',  ( -2.500000007081530029, 1439.558618342239924, 156.0464143015570073 ) ) ;
#60932 = AXIS2_PLACEMENT_3D ( 'NONE', #39395, #81376, #38831 ) ;
#60933 = CARTESIAN_POINT ( 'NONE',  ( -15.34339624849999950, 1451.140281357629874, 150.0590434767980241 ) ) ;
#60934 = DIRECTION ( 'NONE',  ( -1.000000000000000000, 0.000000000000000000, 0.000000000000000000 ) ) ;
#60935 = ORIENTED_EDGE ( 'NONE', *, *, #11965, .F. ) ;
#60936 = CARTESIAN_POINT ( 'NONE',  ( -3.744311016452680274, 1509.032041868229953, 213.3627935371090132 ) ) ;
#60937 = CARTESIAN_POINT ( 'NONE',  ( -2.834728103336690008, 1469.264061671030049, 187.4402886115690023 ) ) ;
#60938 = CARTESIAN_POINT ( 'NONE',  ( -42.85030839420000603, 1440.913081031859974, 270.2009482344979574 ) ) ;
#60939 = CARTESIAN_POINT ( 'NONE',  ( -19.37374569213905318, 1526.382868172863937, 234.3668155954421479 ) ) ;
#60940 = CARTESIAN_POINT ( 'NONE',  ( 16.99430370389999823, 1409.506514545230175, 222.6853181780980151 ) ) ;
#60941 = CARTESIAN_POINT ( 'NONE',  ( -14.93990653130000013, 1474.157326975930118, 223.6788132323979994 ) ) ;
#60942 = B_SPLINE_CURVE_WITH_KNOTS ( 'NONE', 5,
 ( #89620, #47089, #80682, #38665, #89074, #22386, #13442, #81215, #88540 ),
 .UNSPECIFIED., .F., .F.,
 ( 6, 3, 6 ),
 ( -24.98742667679999840, -15.52868752870000080, -11.38875369420000006 ),
 .UNSPECIFIED. ) ;
#60943 = CARTESIAN_POINT ( 'NONE',  ( 12.54268436849999979, 1408.913060387329779, 196.5791615931979948 ) ) ;
#60944 = CARTESIAN_POINT ( 'NONE',  ( 2.808747117329370102, 1409.051439747440099, 230.5333268725640039 ) ) ;
#60946 = EDGE_CURVE ( 'NONE', #60389, #89576, #18775, .T. ) ;
#60945 = CARTESIAN_POINT ( 'NONE',  ( -13.36486944041102909, 1507.695946263434280, 209.3487293591950333 ) ) ;
#60947 = CARTESIAN_POINT ( 'NONE',  ( -6.600008894830000195, 1418.414698087630086, 233.6632623300980072 ) ) ;
#60948 = CIRCLE ( 'NONE', #50225, 33.13701971169416538 ) ;
#60949 = CARTESIAN_POINT ( 'NONE',  ( -0.03561849193722856077, 1486.236081325239866, 181.8148870998357438 ) ) ;
#60950 = CARTESIAN_POINT ( 'NONE',  ( 4.466423236866957858, 1359.830825915227024, 207.6218459616987673 ) ) ;
#60951 = CARTESIAN_POINT ( 'NONE',  ( -45.59604923203520599, 1439.446907945650082, 268.9759714630910139 ) ) ;
#60952 = DIRECTION ( 'NONE',  ( -1.755985294532469921E-16, 1.000000000000000000, -1.338183447452831989E-16 ) ) ;
#60953 = VERTEX_POINT ( 'NONE', #103914 ) ;
#60954 = CARTESIAN_POINT ( 'NONE',  ( -8.172692409730000662, 1424.011347619940125, 209.9196331268980202 ) ) ;
#60955 = ORIENTED_EDGE ( 'NONE', *, *, #88228, .F. ) ;
#60956 = CARTESIAN_POINT ( 'NONE',  ( 3.269025135755000200, 1517.026534522949987, 210.2412850599169758 ) ) ;
#60957 = CIRCLE ( 'NONE', #26967, 0.9999999999999865663 ) ;
#60958 = LINE ( 'NONE', #95084, #26936 ) ;
#60959 = DIRECTION ( 'NONE',  ( -0.1580583862851100141, 0.05644942065497404043, -0.9858148961304372682 ) ) ;
#60960 = CARTESIAN_POINT ( 'NONE',  ( 7.539499508402939476, 1425.640709783210013, 212.1844604678450139 ) ) ;
#60961 = CARTESIAN_POINT ( 'NONE',  ( -27.01407896124499786, 1450.680786773039927, 136.4484523802679803 ) ) ;
#60962 = ORIENTED_EDGE ( 'NONE', *, *, #63226, .F. ) ;
#60963 = LINE ( 'NONE', #36280, #6291 ) ;
#60965 = CARTESIAN_POINT ( 'NONE',  ( -15.31239857737409871, 1512.759354980449871, 222.7072629143739846 ) ) ;
#60964 = CARTESIAN_POINT ( 'NONE',  ( -11.01047251046239772, 1492.285776553619826, 207.1645913320990076 ) ) ;
#60966 = CARTESIAN_POINT ( 'NONE',  ( 0.7521604934737978754, 1487.535995793384245, 219.9383163343715637 ) ) ;
#60967 = VECTOR ( 'NONE', #27529, 999.9999999999998863 ) ;
#60968 = CARTESIAN_POINT ( 'NONE',  ( -11.60004869885204215, 1426.273944179774844, 138.2686100621498326 ) ) ;
#60969 = CARTESIAN_POINT ( 'NONE',  ( 0.3221681605929990200, 1455.007013527990011, 215.7786709544189989 ) ) ;
#60970 = CARTESIAN_POINT ( 'NONE',  ( -8.534885686993231246, 1438.016363115470085, 207.5311831631819643 ) ) ;
#60971 = ORIENTED_EDGE ( 'NONE', *, *, #8213, .T. ) ;
#60972 = CARTESIAN_POINT ( 'NONE',  ( -1.196949206029229940, 1410.397523253659983, 269.3347634687119694 ) ) ;
#60973 = CARTESIAN_POINT ( 'NONE',  ( -4.042388539304999640, 1517.045004075700035, 208.3857484934819979 ) ) ;
#60974 = CARTESIAN_POINT ( 'NONE',  ( 13.24771706019070017, 1421.178600750019996, 230.4496027819150186 ) ) ;
#60975 = CARTESIAN_POINT ( 'NONE',  ( -19.39905127559999798, 1468.965135066929861, 192.1826618881979982 ) ) ;
#60977 = ORIENTED_EDGE ( 'NONE', *, *, #88350, .F. ) ;
#60976 = CARTESIAN_POINT ( 'NONE',  ( -7.826724685212123056, 1365.218692947454656, 209.6218459617148824 ) ) ;
#60978 = ORIENTED_EDGE ( 'NONE', *, *, #22759, .F. ) ;
#60979 = CARTESIAN_POINT ( 'NONE',  ( -23.38128641711469768, 1410.008593999159984, 209.8535812185940017 ) ) ;
#60980 = EDGE_CURVE ( 'NONE', #65868, #95431, #34686, .T. ) ;
#60981 = CARTESIAN_POINT ( 'NONE',  ( -0.3106955533052500051, 1408.923910294080088, 186.0628693114450130 ) ) ;
#60982 = CARTESIAN_POINT ( 'NONE',  ( 3.746090737668994031, 1425.475261178803976, 185.1844613459034576 ) ) ;
#60983 = CARTESIAN_POINT ( 'NONE',  ( 2.149988386126029882E-09, 1405.989059316979819, 266.9611530767110139 ) ) ;
#60984 = CARTESIAN_POINT ( 'NONE',  ( -18.88141956535340071, 1416.640375553479998, 207.5746397123190263 ) ) ;
#60985 = CARTESIAN_POINT ( 'NONE',  ( -18.27573668750000380, 1415.858434028029933, 224.7156095421980240 ) ) ;
#60986 = CARTESIAN_POINT ( 'NONE',  ( 28.38717579456189810, 1468.332634182270112, 266.6432885125559551 ) ) ;
#60987 = CARTESIAN_POINT ( 'NONE',  ( -11.67647783385400118, 1391.913060387289988, 209.3864368603249773 ) ) ;
#60988 = CARTESIAN_POINT ( 'NONE',  ( -16.74235579373888783, 1421.658761381258273, 226.9177557065965232 ) ) ;
#60989 = CARTESIAN_POINT ( 'NONE',  ( -2.879956963085000154, 1516.827328999679821, 205.8693153165069702 ) ) ;
#60990 = ORIENTED_EDGE ( 'NONE', *, *, #18594, .F. ) ;
#60991 = CARTESIAN_POINT ( 'NONE',  ( -13.71357727154099848, 1452.801776351230046, 223.1831243803320035 ) ) ;
#60992 = CARTESIAN_POINT ( 'NONE',  ( 1.500031508154069826, 1465.928657607109926, 182.9103486047420120 ) ) ;
#60993 = CARTESIAN_POINT ( 'NONE',  ( 23.25743447129999808, 1409.985665278929901, 208.2666287018330138 ) ) ;
#60994 = VERTEX_POINT ( 'NONE', #27760 ) ;
#60996 = B_SPLINE_CURVE_WITH_KNOTS ( 'NONE', 3,
 ( #14694, #6839, #42662, #9055 ),
 .UNSPECIFIED., .F., .F.,
 ( 4, 4 ),
 ( 0.000000000000000000, 1.000000000000000000 ),
 .UNSPECIFIED. ) ;
#60995 = CARTESIAN_POINT ( 'NONE',  ( 3.747824384289230260, 1508.879013859839915, 204.8753724212450038 ) ) ;
#60997 = CARTESIAN_POINT ( 'NONE',  ( 26.06503905432269974, 1450.770786748769979, 136.6891037940139881 ) ) ;
#60998 = B_SPLINE_SURFACE_WITH_KNOTS ( 'NONE', 5, 5, ( 
 ( #29370, #105552, #63035, #29920, #79251, #44541 ),
 ( #96033, #97140, #19866, #63570, #20409, #3662 ),
 ( #10367, #96595, #97686, #89286, #104988, #36683 ),
 ( #104435, #12581, #87648, #54615, #10935, #19304 ),
 ( #46211, #46763, #18751, #28280, #53506, #45665 ),
 ( #88746, #78686, #80893, #27728, #70322, #2002 ) ),
 .UNSPECIFIED., .F., .F., .F.,
 ( 6, 6 ),
 ( 6, 6 ),
 ( 17.66400699469150126, 74.90934630149999407 ),
 ( -1.063042706849999883E-07, 2.000000253050000065 ),
 .UNSPECIFIED. ) ;
#60999 = CARTESIAN_POINT ( 'NONE',  ( -3.219327822889010093, 1508.551704408389924, 213.9993814675680142 ) ) ;
#61000 = CARTESIAN_POINT ( 'NONE',  ( -16.15572484810000020, 1388.284171620699908, 201.6770185590890208 ) ) ;
#61001 = CARTESIAN_POINT ( 'NONE',  ( -18.67054469633437819, 1509.506033879027882, 231.0930226666867782 ) ) ;
#61002 = CARTESIAN_POINT ( 'NONE',  ( 17.27342326200000144, 1409.516261619430225, 195.0577033843979962 ) ) ;
#61003 = CARTESIAN_POINT ( 'NONE',  ( 13.59716640859999970, 1444.740067931808653, 176.5566119326980754 ) ) ;
#61004 = DIRECTION ( 'NONE',  ( 0.9234275994329012027, -0.3778483828125600574, 0.06717193023519940631 ) ) ;
#61006 = CARTESIAN_POINT ( 'NONE',  ( -22.79821983952800935, 1432.341711721006504, 215.5993225015029395 ) ) ;
#61005 = CARTESIAN_POINT ( 'NONE',  ( 0.2586465989230000151, 1417.355845570129759, 235.2053782485980093 ) ) ;
#61007 = DIRECTION ( 'NONE',  ( -1.000000000000000000, -8.659264000688481006E-15, 8.115801398047521537E-15 ) ) ;
#61008 = DIRECTION ( 'NONE',  ( 1.836970198721029688E-16, 1.000000000000000000, 0.000000000000000000 ) ) ;
#61009 = CARTESIAN_POINT ( 'NONE',  ( -9.032305492669999936, 1381.079015021919986, 217.6610502493890067 ) ) ;
#61010 = CARTESIAN_POINT ( 'NONE',  ( 5.784638319815000429, 1516.939574742129935, 213.7356083271170064 ) ) ;
#61011 = CARTESIAN_POINT ( 'NONE',  ( 2.273033093151271000, 1525.821544997590308, 240.9339456143063387 ) ) ;
#61012 = VERTEX_POINT ( 'NONE', #61395 ) ;
#61013 = VECTOR ( 'NONE', #92723, 1000.000000000000000 ) ;
#61014 = CARTESIAN_POINT ( 'NONE',  ( -9.721168970463079262, 1481.243685912169894, 204.9479208362279792 ) ) ;
#61015 = CARTESIAN_POINT ( 'NONE',  ( -0.5079764917598921237, 1409.869867835000150, 233.0824847780489790 ) ) ;
#61016 = ADVANCED_FACE ( 'NONE', ( #19900 ), #54101, .F. ) ;
#61017 = CARTESIAN_POINT ( 'NONE',  ( -20.03233416495636021, 1508.143838515403331, 209.6381387959671088 ) ) ;
#61018 = EDGE_CURVE ( 'NONE', #7065, #16730, #4342, .T. ) ;
#61019 = DIRECTION ( 'NONE',  ( -0.5877852522924625900, 0.000000000000000000, 0.8090169943749551118 ) ) ;
#61020 = AXIS2_PLACEMENT_3D ( 'NONE', #83003, #64581, #13570 ) ;
#61021 = ADVANCED_FACE ( 'NONE', ( #52983 ), #50159, .F. ) ;
#61022 = CARTESIAN_POINT ( 'NONE',  ( 0.07181797918499399636, 1506.512156827046965, 231.1702880130284825 ) ) ;
#61023 = CARTESIAN_POINT ( 'NONE',  ( -17.83186622679999900, 1447.284048007129968, 214.3676144197979738 ) ) ;
#61024 = DIRECTION ( 'NONE',  ( -0.6736849260863837507, 0.000000000000000000, 0.7390186874254154326 ) ) ;
#61025 = EDGE_CURVE ( 'NONE', #64595, #4305, #2596, .T. ) ;
#61026 = CARTESIAN_POINT ( 'NONE',  ( 11.33026613920000081, 1433.819327792829881, 151.4886452754979871 ) ) ;
#61027 = CARTESIAN_POINT ( 'NONE',  ( 10.05164999379999990, 1455.338937666430184, 224.8635561966979708 ) ) ;
#61029 = EDGE_CURVE ( 'NONE', #5297, #69813, #105686, .T. ) ;
#61028 = CARTESIAN_POINT ( 'NONE',  ( 25.87170757128150100, 1440.913060398189828, 221.1805615932169928 ) ) ;
#61030 = CONICAL_SURFACE ( 'NONE', #103915, 6.911399307709998219, 0.04363323129990067523 ) ;
#61031 = CARTESIAN_POINT ( 'NONE',  ( 14.12397228379999881, 1429.152045054989912, 195.0086682020989883 ) ) ;
#61032 = CARTESIAN_POINT ( 'NONE',  ( 22.93995821741230046, 1507.616838180419791, 210.4000209873630070 ) ) ;
#61033 = CARTESIAN_POINT ( 'NONE',  ( 9.634457963308390660, 1463.394280929989918, 210.8800767048959983 ) ) ;
#61034 = ADVANCED_FACE ( 'NONE', ( #26678 ), #81200, .T. ) ;
#61035 = CARTESIAN_POINT ( 'NONE',  ( -9.702419644859999082, 1486.515158439930019, 183.3000319968979852 ) ) ;
#61036 = CARTESIAN_POINT ( 'NONE',  ( 11.68470739478344633, 1398.259505493948609, 214.8239554649159118 ) ) ;
#61037 = CARTESIAN_POINT ( 'NONE',  ( -7.474145394509370099, 1509.174061155270010, 238.5777524316769984 ) ) ;
#61038 = CARTESIAN_POINT ( 'NONE',  ( 24.49050335010000268, 1430.357935310629955, 211.3741248221880085 ) ) ;
#61039 = CARTESIAN_POINT ( 'NONE',  ( -16.16965275211135022, 1420.192159313676257, 209.3182675821363148 ) ) ;
#61040 = CARTESIAN_POINT ( 'NONE',  ( 25.37586499933865980, 1436.619698531014137, 137.3878537005881526 ) ) ;
#61041 = CARTESIAN_POINT ( 'NONE',  ( 3.408157919748749709, 1507.642492428714831, 220.3333379687577747 ) ) ;
#61042 = CARTESIAN_POINT ( 'NONE',  ( 18.32584131703820063, 1473.764089907340121, 194.8973952594539867 ) ) ;
#61043 = CARTESIAN_POINT ( 'NONE',  ( -1.119717754394999876, 1517.038650117239968, 212.5846815975970117 ) ) ;
#61044 = EDGE_CURVE ( 'NONE', #35056, #39470, #53530, .T. ) ;
#61045 = DIRECTION ( 'NONE',  ( 0.8672669759446699489, 0.000000000000000000, 0.4978433412588613716 ) ) ;
#61046 = CARTESIAN_POINT ( 'NONE',  ( 0.1599398962665600221, 1486.303002522280167, 181.8235866827639882 ) ) ;
#61048 = ORIENTED_EDGE ( 'NONE', *, *, #63909, .F. ) ;
#61047 = CARTESIAN_POINT ( 'NONE',  ( 3.500614145640000174, 1441.116913297490100, 218.4019928104889914 ) ) ;
#61049 = CARTESIAN_POINT ( 'NONE',  ( -20.87866911129999892, 1445.052233488290085, 177.0630364655980031 ) ) ;
#61050 = VECTOR ( 'NONE', #109883, 1000.000000000000000 ) ;
#61051 = CARTESIAN_POINT ( 'NONE',  ( -6.325225975639999554, 1381.402069227939819, 201.1200243473190028 ) ) ;
#61052 = DIRECTION ( 'NONE',  ( 0.7063774289747313251, 0.04540766091858271930, -0.7063774289747313251 ) ) ;
#61054 = VERTEX_POINT ( 'NONE', #104502 ) ;
#61053 = CARTESIAN_POINT ( 'NONE',  ( -34.54825073237489619, 1451.683981886159927, 134.0999999981819713 ) ) ;
#61055 = CARTESIAN_POINT ( 'NONE',  ( -2.691673115819169571, 1508.551704408389924, 220.0244384242639910 ) ) ;
#61056 = VERTEX_POINT ( 'NONE', #50792 ) ;
#61058 = EDGE_CURVE ( 'NONE', #32612, #21086, #57972, .T. ) ;
#61057 = CARTESIAN_POINT ( 'NONE',  ( -38.62985698160660775, 1443.711942231680041, 137.1840658718770101 ) ) ;
#61059 = CIRCLE ( 'NONE', #66406, 1.000000000000000888 ) ;
#61060 = CARTESIAN_POINT ( 'NONE',  ( -13.97255973646679905, 1390.368318560739908, 209.8293641130019864 ) ) ;
#61061 = CARTESIAN_POINT ( 'NONE',  ( 7.314234105809116038, 1447.455669405640265, 203.7241742676247327 ) ) ;
#61062 =( NAMED_UNIT ( * ) PLANE_ANGLE_UNIT ( ) SI_UNIT ( $, .RADIAN. ) );
#61063 = EDGE_CURVE ( 'NONE', #60035, #10764, #96345, .T. ) ;
#61064 = CARTESIAN_POINT ( 'NONE',  ( -2.845570814896624334, 1367.865368787501211, 208.4582261696480430 ) ) ;
#61065 = CARTESIAN_POINT ( 'NONE',  ( -3.139089597500000384, 1433.097404256189975, 217.7316571164689947 ) ) ;
#61066 = CARTESIAN_POINT ( 'NONE',  ( -10.90103824469269966, 1471.515098176560059, 206.8303341461960088 ) ) ;
#61067 = CARTESIAN_POINT ( 'NONE',  ( -12.26982168579999843, 1378.706401005240195, 210.4710064293389848 ) ) ;
#61068 = CARTESIAN_POINT ( 'NONE',  ( -12.50888813809999967, 1391.368279522899911, 208.1679514191799854 ) ) ;
#61069 = CARTESIAN_POINT ( 'NONE',  ( -71.50884848185910414, 1385.119804080199856, 268.9689710269449847 ) ) ;
#61070 = CARTESIAN_POINT ( 'NONE',  ( -16.88443202019999845, 1417.732921807629964, 191.5454170170979751 ) ) ;
#61071 = CARTESIAN_POINT ( 'NONE',  ( -30.32475187390000215, 1379.724315040820102, 214.4187306602189835 ) ) ;
#61072 = ORIENTED_EDGE ( 'NONE', *, *, #34587, .F. ) ;
#61074 = ADVANCED_FACE ( 'NONE', ( #105622 ), #104471, .T. ) ;
#61073 = VECTOR ( 'NONE', #73799, 1000.000000000000114 ) ;
#61075 = CARTESIAN_POINT ( 'NONE',  ( -32.02808312589908013, 1512.187213306747481, 219.9649204700466782 ) ) ;
#61077 = VERTEX_POINT ( 'NONE', #11553 ) ;
#61076 = CARTESIAN_POINT ( 'NONE',  ( -2.992871990574130336, 1438.525994072939966, 227.4702121500120029 ) ) ;
#61078 = CARTESIAN_POINT ( 'NONE',  ( 8.095719555432868475, 1465.757095899850128, 214.8014529992200039 ) ) ;
#61079 = EDGE_LOOP ( 'NONE', ( #70338, #55068, #2831 ) ) ;
#61080 = CARTESIAN_POINT ( 'NONE',  ( 10.80134480061119895, 1441.261220175989820, 153.0805715986579969 ) ) ;
#61081 = CARTESIAN_POINT ( 'NONE',  ( -7.040068640382609821, 1363.032232768721542, 210.6218459617142003 ) ) ;
#61082 = CARTESIAN_POINT ( 'NONE',  ( -7.769942807339999646, 1494.070509797290015, 200.0359136334189998 ) ) ;
#61083 = CARTESIAN_POINT ( 'NONE',  ( 29.11541691865991055, 1509.936068994953985, 213.9146698034000167 ) ) ;
#61084 = CARTESIAN_POINT ( 'NONE',  ( -32.74318896774677512, 1524.667648926078300, 222.0534297170888465 ) ) ;
#61085 = CARTESIAN_POINT ( 'NONE',  ( 18.99409280968322378, 1437.722685762978472, 213.2647665747184931 ) ) ;
#61086 = CARTESIAN_POINT ( 'NONE',  ( 1.621061852049999974, 1416.517833579129956, 232.6452868846980095 ) ) ;
#61087 = CARTESIAN_POINT ( 'NONE',  ( -7.068319539573729493, 1516.559613835828259, 211.6298318704503174 ) ) ;
#61088 = CARTESIAN_POINT ( 'NONE',  ( -23.54196934549975495, 1507.885283471533057, 223.3642576937991748 ) ) ;
#61089 = CARTESIAN_POINT ( 'NONE',  ( -4.736400914510313420, 1369.930404928426242, 207.6218459616987673 ) ) ;
#61090 = CARTESIAN_POINT ( 'NONE',  ( 11.86629848900230044, 1432.349867578880094, 149.9824231379060109 ) ) ;
#61091 = CARTESIAN_POINT ( 'NONE',  ( 1.548977426030000215, 1456.873932682089844, 199.3713739669490224 ) ) ;
#61092 = CARTESIAN_POINT ( 'NONE',  ( 0.7350231981660010350, 1516.970035769810011, 206.8242163110469960 ) ) ;
#61093 = CARTESIAN_POINT ( 'NONE',  ( -12.95480792804799997, 1435.606741788159979, 150.6280057355330086 ) ) ;
#61094 =( GEOMETRIC_REPRESENTATION_CONTEXT ( 3 ) GLOBAL_UNCERTAINTY_ASSIGNED_CONTEXT ( ( #44623 ) ) GLOBAL_UNIT_ASSIGNED_CONTEXT ( ( #45674, #105561, #62483 ) ) REPRESENTATION_CONTEXT ( 'NONE', 'WORKASPACE' ) );
#61095 = DIRECTION ( 'NONE',  ( 0.000000000000000000, 0.000000000000000000, -1.000000000000000000 ) ) ;
#61096 = CARTESIAN_POINT ( 'NONE',  ( -1.011662833449999965, 1497.725169660189977, 197.8465252784990298 ) ) ;
#61098 = ORIENTED_EDGE ( 'NONE', *, *, #31174, .T. ) ;
#61097 = CARTESIAN_POINT ( 'NONE',  ( 0.6251717133059989662, 1495.142630955389905, 220.4307413487989891 ) ) ;
#61099 = FACE_OUTER_BOUND ( 'NONE', #72033, .T. ) ;
#61100 = VERTEX_POINT ( 'NONE', #21022 ) ;
#61101 = CARTESIAN_POINT ( 'NONE',  ( -24.03538182599999828, 1410.920334414829995, 208.4371777575090050 ) ) ;
#61103 = CARTESIAN_POINT ( 'NONE',  ( 16.32935405069350310, 1409.491649162750036, 193.0798514163919890 ) ) ;
#61102 = CARTESIAN_POINT ( 'NONE',  ( -11.02063524594970012, 1425.659888206090045, 115.9715217809829966 ) ) ;
#61104 = CARTESIAN_POINT ( 'NONE',  ( 7.337153768115000751, 1517.119374999550018, 212.3815752680669959 ) ) ;
#61105 = ADVANCED_FACE ( 'NONE', ( #46286 ), #6301, .T. ) ;
#61106 = AXIS2_PLACEMENT_3D ( 'NONE', #88791, #38373, #64719 ) ;
#61107 = CARTESIAN_POINT ( 'NONE',  ( 29.78388735113269803, 1510.063495189237528, 213.0748577344430430 ) ) ;
#61108 = CARTESIAN_POINT ( 'NONE',  ( 3.609688916579999299E-14, 1407.650947606430009, 270.1377425326979846 ) ) ;
#61109 = CARTESIAN_POINT ( 'NONE',  ( -36.92073679659999641, 1428.724884009829793, 259.2254597838979748 ) ) ;
#61110 = CARTESIAN_POINT ( 'NONE',  ( -12.61627177722139947, 1378.992494172049874, 208.8788604928810173 ) ) ;
#61111 = CARTESIAN_POINT ( 'NONE',  ( 17.15305875377343980, 1460.277650823117938, 228.6392876217846890 ) ) ;
#61112 = CARTESIAN_POINT ( 'NONE',  ( -5.087359574289999742, 1391.865221655589949, 214.5720747206590033 ) ) ;
#61113 = CARTESIAN_POINT ( 'NONE',  ( -37.10899643540120252, 1437.976758828390075, 136.5628136915640027 ) ) ;
#61114 = VERTEX_POINT ( 'NONE', #109475 ) ;
#61115 = CARTESIAN_POINT ( 'NONE',  ( 9.494968296011210285, 1396.244631986520062, 215.6531529143859984 ) ) ;
#61116 = CARTESIAN_POINT ( 'NONE',  ( 9.493856384438370100, 1462.266385979010010, 206.9294982016510289 ) ) ;
#61117 = CARTESIAN_POINT ( 'NONE',  ( -17.86382746079999606, 1458.127315681930213, 228.6833203829979766 ) ) ;
#61118 = ORIENTED_EDGE ( 'NONE', *, *, #74621, .T. ) ;
#61119 = ORIENTED_EDGE ( 'NONE', *, *, #32476, .F. ) ;
#61120 = CARTESIAN_POINT ( 'NONE',  ( -29.29953909818101110, 1509.936973869758503, 211.6148270279188353 ) ) ;
#61121 = CARTESIAN_POINT ( 'NONE',  ( 8.771177098789999960, 1423.989855107869971, 196.4170041723990039 ) ) ;
#61122 = EDGE_CURVE ( 'NONE', #14800, #93336, #6893, .T. ) ;
#61123 = ORIENTED_EDGE ( 'NONE', *, *, #91157, .T. ) ;
#61124 = AXIS2_PLACEMENT_3D ( 'NONE', #86223, #103009, #26306 ) ;
#61125 = CARTESIAN_POINT ( 'NONE',  ( -0.1623179403020000022, 1419.314774686130022, 227.4763468986980115 ) ) ;
#61126 = DIRECTION ( 'NONE',  ( 0.5161917810414575758, -0.8564730265368828421, 0.000000000000000000 ) ) ;
#61127 = CARTESIAN_POINT ( 'NONE',  ( -11.95688248459999947, 1441.464442770860160, 187.7513092272979804 ) ) ;
#61128 = CARTESIAN_POINT ( 'NONE',  ( -5.607190395569999986, 1461.190304871029866, 234.0072117241979868 ) ) ;
#61129 = CARTESIAN_POINT ( 'NONE',  ( 6.032863516324240116, 1508.551565390750284, 201.9555854317009960 ) ) ;
#61130 = CARTESIAN_POINT ( 'NONE',  ( 16.06428795287859757, 1416.913060341709979, 208.9262477897280235 ) ) ;
#61131 = CARTESIAN_POINT ( 'NONE',  ( -11.63792774969999932, 1391.913060387289988, 210.2958033881990048 ) ) ;
#61132 = CARTESIAN_POINT ( 'NONE',  ( -102.2551658410750122, 1384.881266493530120, 296.6246253060550089 ) ) ;
#61133 = VERTEX_POINT ( 'NONE', #107254 ) ;
#61134 = CARTESIAN_POINT ( 'NONE',  ( 3.451033388965000004, 1517.025653221279981, 203.3353183697670090 ) ) ;
#61135 = CARTESIAN_POINT ( 'NONE',  ( 3.455495833855000143, 1516.939877939420057, 209.1085718841020196 ) ) ;
#61136 = EDGE_LOOP ( 'NONE', ( #28168, #10461, #58693, #12997, #45122 ) ) ;
#61137 = CARTESIAN_POINT ( 'NONE',  ( 11.85286409514619876, 1431.415910222289767, 149.9047070638239916 ) ) ;
#61138 = CIRCLE ( 'NONE', #70003, 1.999999999999997780 ) ;
#61139 = EDGE_CURVE ( 'NONE', #68458, #101156, #61571, .T. ) ;
#61140 = CARTESIAN_POINT ( 'NONE',  ( 5.399591216012582962, 1511.369014876942174, 217.1050657725866415 ) ) ;
#61141 = ORIENTED_EDGE ( 'NONE', *, *, #68564, .T. ) ;
#61142 = CARTESIAN_POINT ( 'NONE',  ( -20.20959865099510111, 1501.977400791986611, 182.0120230947222524 ) ) ;
#61143 = DIRECTION ( 'NONE',  ( 0.000000000000000000, 0.000000000000000000, -1.000000000000000000 ) ) ;
#61144 = CARTESIAN_POINT ( 'NONE',  ( 11.15178539160000071, 1509.130341218730109, 235.1839298150979971 ) ) ;
#61145 = CARTESIAN_POINT ( 'NONE',  ( -31.32995031131182628, 1523.678648413191695, 221.9013357025048947 ) ) ;
#61146 = CARTESIAN_POINT ( 'NONE',  ( -6.086798803919999834, 1421.074767261429997, 186.7378509026979998 ) ) ;
#61147 = CARTESIAN_POINT ( 'NONE',  ( 4.801570118712710666, 1410.589679230010006, 269.3375611599190051 ) ) ;
#61148 = CARTESIAN_POINT ( 'NONE',  ( 1.916730757326210011, 1474.810910458910030, 220.3788423859229795 ) ) ;
#61149 = CARTESIAN_POINT ( 'NONE',  ( -12.76143310688880028, 1502.479526517909790, 209.7877290102630070 ) ) ;
#61150 = CARTESIAN_POINT ( 'NONE',  ( -2.386039747897999774, 1422.172641114239923, 193.0199730022190181 ) ) ;
#61151 = DIRECTION ( 'NONE',  ( 3.828568698926946970E-16, 0.000000000000000000, -1.000000000000000000 ) ) ;
#61152 = CARTESIAN_POINT ( 'NONE',  ( 0.02427673352570664661, 1410.268364199324424, 233.2207279706304917 ) ) ;
#61154 = FACE_OUTER_BOUND ( 'NONE', #1134, .T. ) ;
#61153 = CARTESIAN_POINT ( 'NONE',  ( 17.52163758029999840, 1458.428370499130097, 228.8923014477979905 ) ) ;
#61155 = CARTESIAN_POINT ( 'NONE',  ( -68.63354038381854139, 1379.747798109386622, 280.2252688739458790 ) ) ;
#61156 = CARTESIAN_POINT ( 'NONE',  ( 17.62513008079359977, 1411.506380282780128, 224.8263663906670047 ) ) ;
#61157 = CARTESIAN_POINT ( 'NONE',  ( -6.088832748515000226, 1511.778199792620171, 200.6487770440270140 ) ) ;
#61158 = VERTEX_POINT ( 'NONE', #24343 ) ;
#61159 = AXIS2_PLACEMENT_3D ( 'NONE', #69565, #148, #68451 ) ;
#61160 = CARTESIAN_POINT ( 'NONE',  ( 18.36028095489519885, 1424.508247878629845, 223.5128313417529853 ) ) ;
#61161 = CARTESIAN_POINT ( 'NONE',  ( -21.14964295068569200, 1525.231887713368451, 233.8093806080460126 ) ) ;
#61162 = ADVANCED_FACE ( 'NONE', ( #65827 ), #7539, .T. ) ;
#61163 = DIRECTION ( 'NONE',  ( 5.980589973904019347E-17, -1.000000000000000000, 1.736889445713099699E-16 ) ) ;
#61164 = CARTESIAN_POINT ( 'NONE',  ( -14.50669600419999838, 1415.739699861750069, 213.7658224764589932 ) ) ;
#61165 = TOROIDAL_SURFACE ( 'NONE', #34351, 9.500000000000000000, 0.5000000000000000000 ) ;
#61167 = EDGE_LOOP ( 'NONE', ( #4760, #344, #102748, #21100 ) ) ;
#61166 = CARTESIAN_POINT ( 'NONE',  ( 0.5084571940859650141, 1515.143473212400067, 204.7944575026920120 ) ) ;
#61168 = CARTESIAN_POINT ( 'NONE',  ( -4.487249772970000272, 1509.038615934189920, 211.6097810847190033 ) ) ;
#61169 = CARTESIAN_POINT ( 'NONE',  ( -10.16240527536719895, 1472.558926193989919, 209.8189312950259762 ) ) ;
#61170 = EDGE_CURVE ( 'NONE', #102300, #5040, #60262, .T. ) ;
#61171 = CARTESIAN_POINT ( 'NONE',  ( -16.30700481400000257, 1416.815860950479873, 208.9555291761199953 ) ) ;
#61172 = CARTESIAN_POINT ( 'NONE',  ( -10.88738708772158503, 1426.874992181416246, 149.3593185091482098 ) ) ;
#61173 = CARTESIAN_POINT ( 'NONE',  ( -10.76791425542679903, 1461.753518644530004, 211.3311938081530172 ) ) ;
#61174 = CARTESIAN_POINT ( 'NONE',  ( -0.7369207764249980919, 1448.730978137489956, 189.9692764656990107 ) ) ;
#61175 = CARTESIAN_POINT ( 'NONE',  ( -14.96231793096499985, 1514.242353506929931, 224.3370816714669900 ) ) ;
#61176 = CARTESIAN_POINT ( 'NONE',  ( 15.48246398699999915, 1412.746519260829928, 227.3113515368980018 ) ) ;
#61177 = EDGE_CURVE ( 'NONE', #93500, #73642, #65621, .T. ) ;
#61178 = CARTESIAN_POINT ( 'NONE',  ( -11.16953914029999950, 1480.956324499390121, 211.2841307966789941 ) ) ;
#61179 = CARTESIAN_POINT ( 'NONE',  ( -16.32302350474599706, 1459.452451149466015, 228.9511142845270228 ) ) ;
#61180 = CARTESIAN_POINT ( 'NONE',  ( -3.268235758764999943, 1516.890356958860139, 206.2562572478169898 ) ) ;
#61181 = CARTESIAN_POINT ( 'NONE',  ( 35.95138954689999622, 1418.606347009430010, 266.9995350096980360 ) ) ;
#61182 = CARTESIAN_POINT ( 'NONE',  ( 23.74295614150000233, 1435.754861767519969, 139.8124097129980044 ) ) ;
#61183 = CARTESIAN_POINT ( 'NONE',  ( 19.58675617150000292, 1469.160532835930098, 191.3852724613979888 ) ) ;
#61184 = ADVANCED_FACE ( 'NONE', ( #95430 ), #102685, .T. ) ;
#61185 = CARTESIAN_POINT ( 'NONE',  ( -23.47462919730000408, 1434.801338017199896, 212.9388864702380033 ) ) ;
#61186 = CARTESIAN_POINT ( 'NONE',  ( -12.53282948625640003, 1378.856475634480148, 208.0411585582419889 ) ) ;
#61187 = DIRECTION ( 'NONE',  ( 0.000000000000000000, 1.000000000000000000, 0.000000000000000000 ) ) ;
#61188 = CARTESIAN_POINT ( 'NONE',  ( -1.514898281969999871, 1450.642619721169922, 182.9341259013979766 ) ) ;
#61189 = CARTESIAN_POINT ( 'NONE',  ( -20.25058511782390269, 1506.578946199203983, 200.2602131604447209 ) ) ;
#61190 = CARTESIAN_POINT ( 'NONE',  ( -16.79976345160000406, 1416.845603011260209, 208.5245642856469885 ) ) ;
#61191 = CARTESIAN_POINT ( 'NONE',  ( -12.53141519090000067, 1442.576458613880050, 187.0189377207979931 ) ) ;
#61192 = DIRECTION ( 'NONE',  ( -0.000000000000000000, -1.000000000000000000, -0.000000000000000000 ) ) ;
#61193 = CARTESIAN_POINT ( 'NONE',  ( -33.52368697869999892, 1435.668148531879979, 135.0787117157979935 ) ) ;
#61194 = CARTESIAN_POINT ( 'NONE',  ( -11.98993776207835360, 1454.255640063151986, 224.7705267360378798 ) ) ;
#61195 = VERTEX_POINT ( 'NONE', #8095 ) ;
#61196 = CARTESIAN_POINT ( 'NONE',  ( -2.942029669205000086, 1512.314860029340025, 201.2300684455470048 ) ) ;
#61197 = CARTESIAN_POINT ( 'NONE',  ( -13.86277928319429975, 1409.397159307180118, 203.5545281553519885 ) ) ;
#61198 = ADVANCED_FACE ( 'NONE', ( #78069 ), #110045, .T. ) ;
#61199 = CARTESIAN_POINT ( 'NONE',  ( 17.76252328105603695, 1432.742624752195979, 213.6654124838215694 ) ) ;
#61200 = CARTESIAN_POINT ( 'NONE',  ( 3.584503077415259753, 1486.500511906220027, 219.3043361390229791 ) ) ;
#61201 = CIRCLE ( 'NONE', #104076, 38.73358384181149461 ) ;
#61202 = CARTESIAN_POINT ( 'NONE',  ( -23.35296189450000170, 1470.315870435830220, 269.4730450806980002 ) ) ;
#61203 = CARTESIAN_POINT ( 'NONE',  ( -30.31052258194604931, 1523.604703353109699, 195.7506062427371774 ) ) ;
#61204 = CARTESIAN_POINT ( 'NONE',  ( 0.4176721281191659862, 1418.917014445500172, 184.6748447018700006 ) ) ;
#61205 = EDGE_CURVE ( 'NONE', #15055, #99409, #47251, .T. ) ;
#61206 = CARTESIAN_POINT ( 'NONE',  ( 18.06747689609889918, 1424.498894469510105, 224.1058871671330053 ) ) ;
#61207 = CARTESIAN_POINT ( 'NONE',  ( -66.37942218196469923, 1384.673250244690053, 290.6307320938429939 ) ) ;
#61208 = CARTESIAN_POINT ( 'NONE',  ( -3.331783404088238143, 1517.051704408389924, 220.8088060444078451 ) ) ;
#61209 = CARTESIAN_POINT ( 'NONE',  ( 17.71170296313739811, 1423.327007561619894, 226.2336102880809960 ) ) ;
#61210 = CARTESIAN_POINT ( 'NONE',  ( 20.86076292830000156, 1508.959448910729861, 227.6903812582980038 ) ) ;
#61211 = CARTESIAN_POINT ( 'NONE',  ( 14.03776961820000047, 1452.420640915330068, 222.8370746057979943 ) ) ;
#61212 = CYLINDRICAL_SURFACE ( 'NONE', #26685, 26.50000000000001421 ) ;
#61213 = CARTESIAN_POINT ( 'NONE',  ( 4.138543415650000057, 1515.492058123790002, 207.2788820903290059 ) ) ;
#61214 = CARTESIAN_POINT ( 'NONE',  ( 3483.362703962769956, 1009.280093926950144, 1152.220420213539910 ) ) ;
#61215 = CARTESIAN_POINT ( 'NONE',  ( -23.88946018079999689, 1411.108009500230082, 207.7971124514679957 ) ) ;
#61216 =( BOUNDED_CURVE ( )  B_SPLINE_CURVE ( 3, ( #103717, #102586, #9106, #42717 ),
 .UNSPECIFIED., .F., .T. ) 
 B_SPLINE_CURVE_WITH_KNOTS ( ( 4, 4 ),
 ( 3.232438304859030165, 3.299804565595920280 ),
 .UNSPECIFIED. ) 
 CURVE ( )  GEOMETRIC_REPRESENTATION_ITEM ( )  RATIONAL_B_SPLINE_CURVE ( ( 1.000000000000000000, 0.9996218513307064679, 0.9996218513307064679, 1.000000000000000000 ) ) 
 REPRESENTATION_ITEM ( '' )  );
#61217 = CARTESIAN_POINT ( 'NONE',  ( 16.67302254290000008, 1414.971352895729979, 208.8753141282829802 ) ) ;
#61218 = AXIS2_PLACEMENT_3D ( 'NONE', #66257, #57306, #56729 ) ;
#61219 = CARTESIAN_POINT ( 'NONE',  ( 3.771951471599999994, 1485.940416477589906, 219.2135237292989984 ) ) ;
#61220 = CARTESIAN_POINT ( 'NONE',  ( 11.31762120106029990, 1479.526292956740008, 208.6195515253680242 ) ) ;
#61221 = CARTESIAN_POINT ( 'NONE',  ( -106.4020496450190052, 1391.913060387289988, 304.2007955189830568 ) ) ;
#61222 = CARTESIAN_POINT ( 'NONE',  ( 20.77053033756469702, 1455.448302278209894, 207.2432090845329924 ) ) ;
#61223 = CARTESIAN_POINT ( 'NONE',  ( 16.49279160078992490, 1525.408337840050308, 181.2883413873725260 ) ) ;
#61224 = CARTESIAN_POINT ( 'NONE',  ( -31.03138008755339783, 1441.878430314559864, 137.2367898525090197 ) ) ;
#61226 = CARTESIAN_POINT ( 'NONE',  ( -10.05179545849999911, 1382.519305957850065, 200.9245173917790055 ) ) ;
#61225 = CARTESIAN_POINT ( 'NONE',  ( 14.28619591199671390, 1517.015067828388510, 192.2953432750010165 ) ) ;
#61227 = CARTESIAN_POINT ( 'NONE',  ( -5.100030730249999422, 1391.870657718589882, 203.7628047703390166 ) ) ;
#61228 = DIRECTION ( 'NONE',  ( 0.000000000000000000, 1.000000000000000000, 0.000000000000000000 ) ) ;
#61229 = CARTESIAN_POINT ( 'NONE',  ( -15.53900113990620113, 1420.370647695649950, 210.6480565532440039 ) ) ;
#61230 = CARTESIAN_POINT ( 'NONE',  ( -23.21169520710000000, 1420.930134560530178, 211.3054972004780154 ) ) ;
#61231 = CARTESIAN_POINT ( 'NONE',  ( 4.138543391158296281, 1515.492058413688710, 206.7917118350202088 ) ) ;
#61232 = CARTESIAN_POINT ( 'NONE',  ( -2.489617576474999705, 1516.665179208830068, 204.1258511445269903 ) ) ;
#61233 = CARTESIAN_POINT ( 'NONE',  ( -30.95751052620457600, 1525.821544997590081, 201.4531494772889459 ) ) ;
#61234 = PRESENTATION_STYLE_ASSIGNMENT (( #103746 ) ) ;
#61235 = CARTESIAN_POINT ( 'NONE',  ( -15.43521629878640056, 1485.016445856970222, 187.3278621968299831 ) ) ;
#61236 = CARTESIAN_POINT ( 'NONE',  ( 2.147315937701882227, 1476.624887484032342, 198.5454470367664328 ) ) ;
#61237 = AXIS2_PLACEMENT_3D ( 'NONE', #79985, #11143, #44751 ) ;
#61238 = CARTESIAN_POINT ( 'NONE',  ( 5.415999934931220672, 1505.806266447880034, 219.5704311486180131 ) ) ;
#61239 = CARTESIAN_POINT ( 'NONE',  ( 37.36839315630000158, 1449.335722529840041, 136.3140007074979962 ) ) ;
#61241 = EDGE_LOOP ( 'NONE', ( #54507, #77037, #31038, #23481 ) ) ;
#61240 = CARTESIAN_POINT ( 'NONE',  ( -59.50571812958200013, 1379.724539154309923, 264.8335893427189944 ) ) ;
#61242 = ORIENTED_EDGE ( 'NONE', *, *, #3502, .T. ) ;
#61243 = CARTESIAN_POINT ( 'NONE',  ( 11.24610669039820010, 1434.034494598100082, 151.5766399473429829 ) ) ;
#61244 = CARTESIAN_POINT ( 'NONE',  ( 21.15382147014735281, 1525.425665131969254, 183.9878842466098376 ) ) ;
#61245 = VERTEX_POINT ( 'NONE', #8061 ) ;
#61246 = CARTESIAN_POINT ( 'NONE',  ( -105.1577856459999936, 1379.115010806019882, 304.6242328078590162 ) ) ;
#61247 = CARTESIAN_POINT ( 'NONE',  ( -10.35637635652009969, 1448.251843012599920, 208.5390742616600050 ) ) ;
#61248 = FACE_OUTER_BOUND ( 'NONE', #27982, .T. ) ;
#61250 = CARTESIAN_POINT ( 'NONE',  ( 1.546867617820790075, 1416.839692126689897, 190.2222510973109877 ) ) ;
#61249 = CARTESIAN_POINT ( 'NONE',  ( 16.02111279596229920, 1422.399697759369701, 191.1604070481699864 ) ) ;
#61251 = CARTESIAN_POINT ( 'NONE',  ( 6.121488579075629488, 1465.717471025350051, 212.7485050010139958 ) ) ;
#61252 = CARTESIAN_POINT ( 'NONE',  ( 1.990304530710000241, 1507.640980020629740, 181.1916917869979784 ) ) ;
#61253 = CARTESIAN_POINT ( 'NONE',  ( -0.2465318334200000405, 1414.971352895729979, 192.4488234187979856 ) ) ;
#61254 = CARTESIAN_POINT ( 'NONE',  ( 15.96357422200000009, 1410.842840262029995, 226.9345609355980002 ) ) ;
#61255 = CARTESIAN_POINT ( 'NONE',  ( -3.251888867474999945, 1516.793978928989873, 211.6142896211370044 ) ) ;
#61256 = DIRECTION ( 'NONE',  ( 7.205227288424627209E-20, 0.9876883405951701889, 0.1564344650400262826 ) ) ;
#61257 = CARTESIAN_POINT ( 'NONE',  ( -10.55504723130449918, 1423.013874365220090, 207.2063886206990162 ) ) ;
#61258 = CARTESIAN_POINT ( 'NONE',  ( 7.263042179585000646, 1512.240414293140020, 202.3122947996570247 ) ) ;
#61259 = ORIENTED_EDGE ( 'NONE', *, *, #36617, .T. ) ;
#61260 = CARTESIAN_POINT ( 'NONE',  ( 13.68291348452850009, 1434.996735757539909, 148.9906729220649879 ) ) ;
#61261 = DIRECTION ( 'NONE',  ( 0.9942586961433749204, 0.000000000000000000, -0.1070030146457386366 ) ) ;
#61262 = ORIENTED_EDGE ( 'NONE', *, *, #32722, .F. ) ;
#61263 = ORIENTED_EDGE ( 'NONE', *, *, #39933, .F. ) ;
#61264 = ORIENTED_EDGE ( 'NONE', *, *, #32258, .F. ) ;
#61265 = CARTESIAN_POINT ( 'NONE',  ( -8.191860474865000796, 1512.696049264750172, 216.1202668200969867 ) ) ;
#61266 = CARTESIAN_POINT ( 'NONE',  ( -3.068665118410000225, 1464.761382153330032, 237.1705660322979838 ) ) ;
#61267 = EDGE_CURVE ( 'NONE', #48668, #89451, #25519, .T. ) ;
#61268 = CARTESIAN_POINT ( 'NONE',  ( 29.22958591724099975, 1509.933780020319773, 206.4713313096740137 ) ) ;
#61269 = CARTESIAN_POINT ( 'NONE',  ( -7.717505791104999346, 1516.857914730730045, 216.8393517232070167 ) ) ;
#61270 = CARTESIAN_POINT ( 'NONE',  ( 2.495485017165389952, 1466.055911289739925, 198.3720333978750148 ) ) ;
#61271 = CARTESIAN_POINT ( 'NONE',  ( -19.09275713913258699, 1441.344922765982346, 209.9503379368030380 ) ) ;
#61272 = CARTESIAN_POINT ( 'NONE',  ( -51.28450536721118880, 1379.693347499785432, 242.1435806264775863 ) ) ;
#61273 = CARTESIAN_POINT ( 'NONE',  ( 4.221729048143290086, 1446.223289964359992, 169.8973273558370067 ) ) ;
#61274 = CARTESIAN_POINT ( 'NONE',  ( 8.654266642250069808, 1437.837011637059959, 209.6701303830640200 ) ) ;
#61275 = EDGE_LOOP ( 'NONE', ( #20002, #68539, #12601, #1408 ) ) ;
#61276 = CARTESIAN_POINT ( 'NONE',  ( 5.771149074885000729, 1516.616791731099966, 206.6334853027970269 ) ) ;
#61277 = ORIENTED_EDGE ( 'NONE', *, *, #29028, .F. ) ;
#61278 = CARTESIAN_POINT ( 'NONE',  ( 19.62250382303630047, 1440.913060387330006, 213.8950623188489999 ) ) ;
#61279 = EDGE_CURVE ( 'NONE', #89888, #54724, #109832, .T. ) ;
#61280 = CARTESIAN_POINT ( 'NONE',  ( -17.69093279879999869, 1507.793158530429764, 186.8252671473979944 ) ) ;
#61281 = EDGE_LOOP ( 'NONE', ( #69550, #14344, #67630, #12609 ) ) ;
#61282 = CARTESIAN_POINT ( 'NONE',  ( -33.93390015750107835, 1451.270656932794054, 135.9469490811935657 ) ) ;
#61283 = CARTESIAN_POINT ( 'NONE',  ( -15.18915102340000089, 1410.375618971030008, 190.8776686048979911 ) ) ;
#61284 = CARTESIAN_POINT ( 'NONE',  ( -24.35834046960000165, 1442.143026477599960, 211.4091606738980147 ) ) ;
#61285 = CARTESIAN_POINT ( 'NONE',  ( 2.018257968592299889, 1423.421772701890177, 192.6172488092990136 ) ) ;
#61286 = CARTESIAN_POINT ( 'NONE',  ( 11.49747572422220188, 1414.913060387329779, 220.3427040978150160 ) ) ;
#61287 = CARTESIAN_POINT ( 'NONE',  ( -13.06845456229791047, 1434.810982766093957, 146.9332176485133630 ) ) ;
#61288 = PLANE ( 'NONE',  #66374 ) ;
#61289 = CARTESIAN_POINT ( 'NONE',  ( -12.84579503169999803, 1434.992946303999815, 194.0992193082979895 ) ) ;
#61291 = CARTESIAN_POINT ( 'NONE',  ( 8.249359711299819153, 1435.329571781400091, 206.3472986359390120 ) ) ;
#61290 = CARTESIAN_POINT ( 'NONE',  ( 22.01290455779290767, 1522.906363951597314, 182.8785777331706015 ) ) ;
#61292 = CARTESIAN_POINT ( 'NONE',  ( 7.331812085974999782, 1516.906641539930206, 215.6759973964769870 ) ) ;
#61293 = CARTESIAN_POINT ( 'NONE',  ( -3.357462532821310131, 1428.720380741769986, 200.3803434257089862 ) ) ;
#61294 = CARTESIAN_POINT ( 'NONE',  ( 6.170974574032440430, 1511.326458810320219, 216.6586639964210121 ) ) ;
#61295 = CARTESIAN_POINT ( 'NONE',  ( 28.45104061960000053, 1509.631525885230076, 207.4803073972880156 ) ) ;
#61296 = CARTESIAN_POINT ( 'NONE',  ( -0.7355686809059980291, 1517.012231669750008, 212.3888856620870058 ) ) ;
#61297 = CARTESIAN_POINT ( 'NONE',  ( -11.80920141334000029, 1482.273830016230022, 207.6845722505150036 ) ) ;
#61298 = CARTESIAN_POINT ( 'NONE',  ( -17.22789533397991235, 1486.134374014700143, 187.8660400835535711 ) ) ;
#61300 = ORIENTED_EDGE ( 'NONE', *, *, #68243, .T. ) ;
#61299 = CARTESIAN_POINT ( 'NONE',  ( -85.85832257059999506, 1385.179345198489955, 289.6849318678590066 ) ) ;
#61301 = CARTESIAN_POINT ( 'NONE',  ( 28.09269446560000105, 1442.732147117420254, 231.9538848060979888 ) ) ;
#61302 = EDGE_CURVE ( 'NONE', #110436, #108856, #59806, .T. ) ;
#61303 = CARTESIAN_POINT ( 'NONE',  ( 3.838688366592032608, 1449.941958011591623, 184.1981631407757618 ) ) ;
#61304 = CARTESIAN_POINT ( 'NONE',  ( -27.73912773776899954, 1509.881732072950172, 218.7146610652550009 ) ) ;
#61305 = CARTESIAN_POINT ( 'NONE',  ( -8.472821806374909670, 1509.208940765679927, 237.1966872052409769 ) ) ;
#61306 = EDGE_CURVE ( 'NONE', #87539, #104414, #6823, .T. ) ;
#61307 = CARTESIAN_POINT ( 'NONE',  ( -20.54907931089999806, 1454.472754293929938, 224.8058317932980117 ) ) ;
#61308 = ADVANCED_FACE ( 'NONE', ( #81880 ), #4469, .F. ) ;
#61310 = CARTESIAN_POINT ( 'NONE',  ( 17.99628978319960027, 1410.830115193840129, 222.9828712447109922 ) ) ;
#61309 = DIRECTION ( 'NONE',  ( 0.9861488065241343914, 0.1648740305507690185, -0.01808550361393360464 ) ) ;
#61311 = DIRECTION ( 'NONE',  ( 0.000000000000000000, 1.000000000000000000, 0.000000000000000000 ) ) ;
#61312 = CARTESIAN_POINT ( 'NONE',  ( -1.842963721827329815, 1515.551704300040001, 205.2922259627210053 ) ) ;
#61313 = ORIENTED_EDGE ( 'NONE', *, *, #25079, .T. ) ;
#61314 = CARTESIAN_POINT ( 'NONE',  ( -5.008848238024999233, 1516.858456333729919, 204.1217621043670079 ) ) ;
#61315 = CARTESIAN_POINT ( 'NONE',  ( 0.1075625203479999986, 1405.989059426929998, 266.9611530679979978 ) ) ;
#61316 = CARTESIAN_POINT ( 'NONE',  ( 27.79064032830000031, 1508.605033450530073, 207.7520403031080036 ) ) ;
#61317 = EDGE_CURVE ( 'NONE', #67344, #108102, #11527, .T. ) ;
#61318 = CARTESIAN_POINT ( 'NONE',  ( -4.041028775053940565E-06, 1471.436293264230017, 269.3346704911970164 ) ) ;
#61319 = CARTESIAN_POINT ( 'NONE',  ( 2.478173748110000130, 1439.527585047869934, 157.7653643411979658 ) ) ;
#61320 = CARTESIAN_POINT ( 'NONE',  ( 3.284535177480000012, 1466.923997773790006, 218.9072142754990011 ) ) ;
#61321 = CARTESIAN_POINT ( 'NONE',  ( -20.01701399148389982, 1508.375005217440048, 188.9474772628149992 ) ) ;
#61322 = CARTESIAN_POINT ( 'NONE',  ( -44.35579534389660239, 1440.913060402619976, 264.7564585019449623 ) ) ;
#61323 = CARTESIAN_POINT ( 'NONE',  ( 34.03745954885479819, 1450.435860261120069, 136.2418865863519954 ) ) ;
#61324 = CARTESIAN_POINT ( 'NONE',  ( -1.958645825849109734, 1450.346086741789804, 154.2463840937579960 ) ) ;
#61325 = CARTESIAN_POINT ( 'NONE',  ( 0.8066343449330010129, 1430.937684729390185, 200.0727349034889926 ) ) ;
#61326 = CARTESIAN_POINT ( 'NONE',  ( 4.758051368188402463, 1442.166524513745799, 216.6176570306145663 ) ) ;
#61327 = CARTESIAN_POINT ( 'NONE',  ( -0.8454865857380020611, 1508.321029480389825, 220.8622050322990162 ) ) ;
#61328 = FACE_OUTER_BOUND ( 'NONE', #32478, .T. ) ;
#61329 = VERTEX_POINT ( 'NONE', #33129 ) ;
#61330 = CARTESIAN_POINT ( 'NONE',  ( -31.70762145559999468, 1417.952368988429953, 271.1218459616979999 ) ) ;
#61331 = CARTESIAN_POINT ( 'NONE',  ( 0.09726404165740129559, 1484.801171650590049, 198.3753413853989969 ) ) ;
#61332 = DIRECTION ( 'NONE',  ( -0.6736849260863839728, 0.000000000000000000, 0.7390186874254150995 ) ) ;
#61333 = CARTESIAN_POINT ( 'NONE',  ( -0.5895635512679999746, 1417.370800527230131, 235.1640457548979839 ) ) ;
#61334 = CARTESIAN_POINT ( 'NONE',  ( 12.50980606740000134, 1501.173550771890177, 211.4238265534589800 ) ) ;
#61335 = CARTESIAN_POINT ( 'NONE',  ( -32.09235212274882088, 1525.402221411319488, 196.2603058525792790 ) ) ;
#61336 = EDGE_CURVE ( 'NONE', #77903, #21803, #24121, .T. ) ;
#61337 = DIRECTION ( 'NONE',  ( 0.9147450530333530727, 0.03449475076686789321, -0.4025563316115395862 ) ) ;
#61338 = CARTESIAN_POINT ( 'NONE',  ( -21.76319146545460015, 1384.856752773889866, 221.7575919100939927 ) ) ;
#61339 = CARTESIAN_POINT ( 'NONE',  ( -18.34708879960000161, 1415.579607672129896, 208.2154979986029844 ) ) ;
#61340 = CARTESIAN_POINT ( 'NONE',  ( 3.909710721586100224, 1517.051704408389924, 220.4764703678949900 ) ) ;
#61341 = CARTESIAN_POINT ( 'NONE',  ( 26.52894651520460201, 1435.730259070040120, 136.2304755143660202 ) ) ;
#61343 = EDGE_CURVE ( 'NONE', #80182, #69002, #89584, .T. ) ;
#61342 = CARTESIAN_POINT ( 'NONE',  ( -13.33659772418124767, 1443.292211361891077, 169.3747828019180872 ) ) ;
#61344 = EDGE_LOOP ( 'NONE', ( #41103, #79925, #51095, #56931, #57580, #43588 ) ) ;
#61345 = CARTESIAN_POINT ( 'NONE',  ( -16.22271312188570036, 1409.479543335319931, 225.1382318463119816 ) ) ;
#61346 = CARTESIAN_POINT ( 'NONE',  ( -20.06572793885469963, 1485.934154802469948, 214.0281146234499943 ) ) ;
#61347 = ORIENTED_EDGE ( 'NONE', *, *, #11516, .F. ) ;
#61348 = CARTESIAN_POINT ( 'NONE',  ( -11.67169904690000060, 1501.458093416090151, 211.3450001677690295 ) ) ;
#61349 = CARTESIAN_POINT ( 'NONE',  ( 6.564931535518120143, 1516.660079020903368, 205.4906681412120406 ) ) ;
#61351 = CARTESIAN_POINT ( 'NONE',  ( -16.68597733941929917, 1461.099535985040120, 230.2790158113629957 ) ) ;
#61350 = CARTESIAN_POINT ( 'NONE',  ( 11.09105272649999918, 1426.482985488930126, 97.30048952069790857 ) ) ;
#61352 = DIRECTION ( 'NONE',  ( -1.000000000000000000, 0.000000000000000000, 0.000000000000000000 ) ) ;
#61353 = CARTESIAN_POINT ( 'NONE',  ( 4.408870434958439333, 1425.824683284920184, 185.4670092970000042 ) ) ;
#61354 = B_SPLINE_CURVE_WITH_KNOTS ( 'NONE', 5,
 ( #20498, #54708, #79338, #88834, #97775, #2649, #36777, #12120, #46312, #37887, #106185, #29467 ),
 .UNSPECIFIED., .F., .F.,
 ( 6, 3, 3, 6 ),
 ( 0.000000000000000000, 0.1473537928490198934, 0.5736768964245098079, 1.000000000000000000 ),
 .UNSPECIFIED. ) ;
#61355 = CARTESIAN_POINT ( 'NONE',  ( -5.779603138255000161, 1516.738222552470233, 201.4074744291170020 ) ) ;
#61356 = CARTESIAN_POINT ( 'NONE',  ( 7.669609405850000172, 1425.609943377740137, 211.8990498311490001 ) ) ;
#61357 = CARTESIAN_POINT ( 'NONE',  ( -14.38096556510000035, 1422.143733531690032, 196.2925564653990023 ) ) ;
#61358 = CARTESIAN_POINT ( 'NONE',  ( 7.361717033309999714, 1508.153716861730118, 182.4941886473980048 ) ) ;
#61359 = CARTESIAN_POINT ( 'NONE',  ( -109.5441724340000036, 1378.991699893399982, 306.1169303483130193 ) ) ;
#61360 = CARTESIAN_POINT ( 'NONE',  ( 8.635439922379047673, 1365.453094710691630, 210.6218459617142003 ) ) ;
#61362 = VERTEX_POINT ( 'NONE', #104752 ) ;
#61361 = CARTESIAN_POINT ( 'NONE',  ( -5.374569360760125036, 1464.404629561533966, 236.8301563712954874 ) ) ;
#61363 = EDGE_LOOP ( 'NONE', ( #52975, #83784, #10599, #57797, #34472, #56563, #59335, #9949, #70874 ) ) ;
#61364 = CARTESIAN_POINT ( 'NONE',  ( 7.481780845334932373, 1510.769285165366227, 203.0163852401010729 ) ) ;
#61365 = CARTESIAN_POINT ( 'NONE',  ( 4.359368621329999693E-15, 1471.436294014630221, 269.3346704429980036 ) ) ;
#61366 = CARTESIAN_POINT ( 'NONE',  ( 6.913706168296744892, 1500.103688322486505, 200.0567346946345708 ) ) ;
#61367 = CARTESIAN_POINT ( 'NONE',  ( -2.794587184679999670, 1486.518066062529897, 181.7593184408980278 ) ) ;
#61368 = B_SPLINE_CURVE_WITH_KNOTS ( 'NONE', 5,
 ( #49521, #83106, #6941, #109422, #101531, #58466, #92593, #6400, #24820 ),
 .UNSPECIFIED., .F., .F.,
 ( 6, 3, 6 ),
 ( 127.6642502654205487, 131.5832540680000022, 137.5414126590000023 ),
 .UNSPECIFIED. ) ;
#61369 = CARTESIAN_POINT ( 'NONE',  ( -31.12456774391179337, 1525.960063244516959, 201.1524202391566405 ) ) ;
#61370 = CARTESIAN_POINT ( 'NONE',  ( 7.799999999999999822, 1402.913060387289988, 209.1218459616989946 ) ) ;
#61371 = CARTESIAN_POINT ( 'NONE',  ( 21.62710397070000212, 1409.668295492329889, 206.7322786019380203 ) ) ;
#61372 = FACE_OUTER_BOUND ( 'NONE', #93033, .T. ) ;
#61373 = CARTESIAN_POINT ( 'NONE',  ( 7.890486628608978315, 1368.832605670318799, 207.6218459616987673 ) ) ;
#61374 = CARTESIAN_POINT ( 'NONE',  ( 6.993398322862810268, 1409.157275238040029, 195.4924656238740113 ) ) ;
#61375 = CARTESIAN_POINT ( 'NONE',  ( 5.576759338873839723E-05, 1405.989119098810079, 266.9610487349989967 ) ) ;
#61376 = CARTESIAN_POINT ( 'NONE',  ( -13.91110666395790041, 1435.008848373910041, 148.8314041724960077 ) ) ;
#61377 = ORIENTED_EDGE ( 'NONE', *, *, #50407, .T. ) ;
#61378 = CARTESIAN_POINT ( 'NONE',  ( -11.30198679499999947, 1432.355652606760032, 151.5220046058980188 ) ) ;
#61379 = CARTESIAN_POINT ( 'NONE',  ( 13.50628347229999981, 1442.279780698270088, 189.1190317712979834 ) ) ;
#61380 = VERTEX_POINT ( 'NONE', #13977 ) ;
#61381 = VERTEX_POINT ( 'NONE', #91250 ) ;
#61382 = CARTESIAN_POINT ( 'NONE',  ( -22.28696231330000188, 1506.798305107829947, 208.8466800722590051 ) ) ;
#61383 = CARTESIAN_POINT ( 'NONE',  ( -9.655745333040000489, 1363.739547551590022, 207.6218459616989946 ) ) ;
#61384 = CARTESIAN_POINT ( 'NONE',  ( -2.286446363765000100, 1517.042661899400173, 213.7475398352470108 ) ) ;
#61385 = CARTESIAN_POINT ( 'NONE',  ( 3.991161783265000818, 1511.207707629420156, 216.9064051716169956 ) ) ;
#61386 = B_SPLINE_SURFACE_WITH_KNOTS ( 'NONE', 5, 5, ( 
 ( #87852, #62108, #19509, #62673, #11140, #79440 ),
 ( #2752, #36872, #96794, #54258, #88384, #45851 ),
 ( #79983, #3302, #89482, #105751, #91129, #39633 ),
 ( #12777, #55348, #47490, #73802, #46954, #54795 ),
 ( #64305, #97327, #88927, #30674, #48599, #12213 ),
 ( #38517, #82733, #64861, #81613, #90572, #39057 ) ),
 .UNSPECIFIED., .F., .F., .F.,
 ( 6, 6 ),
 ( 6, 6 ),
 ( 6.281102661440000290, 8.354490254749999067 ),
 ( 0.000000000000000000, 1.450255543799999991 ),
 .UNSPECIFIED. ) ;
#61387 = ORIENTED_EDGE ( 'NONE', *, *, #32902, .F. ) ;
#61388 = CARTESIAN_POINT ( 'NONE',  ( -64.85694393360000731, 1375.750462046670009, 269.1292758464589951 ) ) ;
#61389 = CARTESIAN_POINT ( 'NONE',  ( -106.6345736060380034, 1378.913060387289988, 301.6740162769929725 ) ) ;
#61390 = CARTESIAN_POINT ( 'NONE',  ( -2.488360667435000284, 1516.616791731099966, 203.3506968572170308 ) ) ;
#61391 = CARTESIAN_POINT ( 'NONE',  ( -26.57809186909999966, 1508.585461716229929, 202.0629932667179958 ) ) ;
#61392 = CARTESIAN_POINT ( 'NONE',  ( -5.181410188784999704, 1510.418062979269962, 201.5729736320070060 ) ) ;
#61393 = CARTESIAN_POINT ( 'NONE',  ( -94.50884446960000673, 1385.089621650810159, 294.8626808758589846 ) ) ;
#61394 = CARTESIAN_POINT ( 'NONE',  ( -58.92658587845429707, 1384.666467992389926, 241.7252083246220025 ) ) ;
#61395 = CARTESIAN_POINT ( 'NONE',  ( 5.059013353549999259, 1501.257177412389865, 229.8390314845989906 ) ) ;
#61396 = CARTESIAN_POINT ( 'NONE',  ( -8.327525192625062189, 1438.484961729265706, 206.5299198730474473 ) ) ;
#61398 = ORIENTED_EDGE ( 'NONE', *, *, #55850, .T. ) ;
#61397 = CARTESIAN_POINT ( 'NONE',  ( -12.07722023368130593, 1511.957228877181251, 194.2728863314506214 ) ) ;
#61399 = CARTESIAN_POINT ( 'NONE',  ( 27.42695472179999783, 1451.955572177629847, 134.9063961680979844 ) ) ;
#61400 = FACE_OUTER_BOUND ( 'NONE', #23002, .T. ) ;
#61401 = CARTESIAN_POINT ( 'NONE',  ( 19.28184285025260181, 1456.939734798050267, 224.6612775436279890 ) ) ;
#61402 = CARTESIAN_POINT ( 'NONE',  ( -24.39026675770000097, 1435.355298166539797, 136.4119318075979947 ) ) ;
#61403 = CARTESIAN_POINT ( 'NONE',  ( 7.725372132234999967, 1517.158319634930194, 211.9946825927569876 ) ) ;
#61404 = CARTESIAN_POINT ( 'NONE',  ( -67.31912871069998516, 1379.744358027319777, 277.0891020787589696 ) ) ;
#61405 = CARTESIAN_POINT ( 'NONE',  ( 0.01871782600107488662, 1507.454862520212146, 237.3968338320200075 ) ) ;
#61406 = DIRECTION ( 'NONE',  ( -0.3363363969979660806, 0.9417419115949053898, 0.000000000000000000 ) ) ;
#61407 = CARTESIAN_POINT ( 'NONE',  ( 19.18147675296038557, 1410.944559830756589, 195.6234844512586335 ) ) ;
#61408 = CARTESIAN_POINT ( 'NONE',  ( -2.879318455905000018, 1516.995911393979895, 208.3865093923290033 ) ) ;
#61409 = ORIENTED_EDGE ( 'NONE', *, *, #68491, .T. ) ;
#61410 = CARTESIAN_POINT ( 'NONE',  ( 2.500000000000000000, 1437.283720389809787, 157.6542335194979785 ) ) ;
#61411 = CARTESIAN_POINT ( 'NONE',  ( -1.368591974409999912, 1412.843971119630169, 233.0744961443979832 ) ) ;
#61412 = CARTESIAN_POINT ( 'NONE',  ( -43.09011427770000324, 1385.164419251190111, 247.5010251099589880 ) ) ;
#61413 = EDGE_LOOP ( 'NONE', ( #12080, #45013 ) ) ;
#61414 = CARTESIAN_POINT ( 'NONE',  ( -105.5185485394360114, 1378.942001926445982, 304.0419961266803170 ) ) ;
#61415 = CARTESIAN_POINT ( 'NONE',  ( -3.382909239710000016, 1428.856116242189955, 200.7987450405690026 ) ) ;
#61416 = CARTESIAN_POINT ( 'NONE',  ( 11.84288159193510026, 1435.129470572849868, 151.2381383328829827 ) ) ;
#61417 = ADVANCED_FACE ( 'NONE', ( #81187 ), #57124, .F. ) ;
#61418 = CARTESIAN_POINT ( 'NONE',  ( 15.05624239712749990, 1469.004309107100198, 230.3228700955960164 ) ) ;
#61419 = CARTESIAN_POINT ( 'NONE',  ( -22.10329645359099970, 1509.714832913870168, 228.9299748702250099 ) ) ;
#61420 = FACE_OUTER_BOUND ( 'NONE', #104048, .T. ) ;
#61421 = CARTESIAN_POINT ( 'NONE',  ( -0.04703688478509999993, 1408.914702951529762, 231.7816009520980174 ) ) ;
#61422 = CARTESIAN_POINT ( 'NONE',  ( -14.45783243223209880, 1416.839692136300073, 221.3920770721769884 ) ) ;
#61424 = CARTESIAN_POINT ( 'NONE',  ( 6.824596843277944913, 1424.786834349993342, 213.4892281956427098 ) ) ;
#61423 = CARTESIAN_POINT ( 'NONE',  ( 1.711311228545000063, 1516.591755933730155, 214.8926661113670207 ) ) ;
#61425 = CARTESIAN_POINT ( 'NONE',  ( -5.663447254089540195, 1391.839989632750076, 215.0012937448320258 ) ) ;
#61426 = CARTESIAN_POINT ( 'NONE',  ( 1.128757561074999805, 1516.608208975040043, 216.8328129478670121 ) ) ;
#61427 = ORIENTED_EDGE ( 'NONE', *, *, #31211, .T. ) ;
#61428 = CARTESIAN_POINT ( 'NONE',  ( 4.035536225084999984, 1517.086065052259983, 201.3983658527070020 ) ) ;
#61429 = CARTESIAN_POINT ( 'NONE',  ( -6.195568093309999469, 1495.113783496430187, 181.4148133623980073 ) ) ;
#61430 = ORIENTED_EDGE ( 'NONE', *, *, #16752, .T. ) ;
#61431 = CARTESIAN_POINT ( 'NONE',  ( 0.6621667027629999369, 1417.277712856329799, 235.8679543975979982 ) ) ;
#61432 = EDGE_CURVE ( 'NONE', #33631, #100091, #99082, .T. ) ;
#61433 = DIRECTION ( 'NONE',  ( 1.402715769532790202E-14, -1.000000000000000000, 4.930380657631320281E-31 ) ) ;
#61434 = CARTESIAN_POINT ( 'NONE',  ( 8.792772900901731248, 1511.562335007999991, 203.1497331793660237 ) ) ;
#61435 = CARTESIAN_POINT ( 'NONE',  ( 5.440512190109999757, 1424.738065781850082, 191.9794586101990319 ) ) ;
#61436 = CARTESIAN_POINT ( 'NONE',  ( -31.44837959398599736, 1512.187213306747481, 197.3353852117985525 ) ) ;
#61437 = CARTESIAN_POINT ( 'NONE',  ( 2.566893074593609807E-08, 1406.911841303630126, 196.1218459607310081 ) ) ;
#61438 = CARTESIAN_POINT ( 'NONE',  ( -2.712106650090000404, 1447.524051941180005, 157.8378498936980066 ) ) ;
#61439 = CARTESIAN_POINT ( 'NONE',  ( -11.86716023049999968, 1432.353341358199941, 147.6509521729980179 ) ) ;
#61440 = CARTESIAN_POINT ( 'NONE',  ( -14.25739833390000122, 1435.140225252410119, 149.2707004493980207 ) ) ;
#61441 = EDGE_CURVE ( 'NONE', #74194, #68962, #91906, .T. ) ;
#61442 = CARTESIAN_POINT ( 'NONE',  ( -11.86716023049999968, 1432.353341358199941, 147.6509521729980179 ) ) ;
#61443 = CARTESIAN_POINT ( 'NONE',  ( -1.746314907631250080, 1462.701329518090006, 183.7072431146600024 ) ) ;
#61445 = CARTESIAN_POINT ( 'NONE',  ( 0.5950580025862760580, 1496.414336839329962, 186.9683653809459827 ) ) ;
#61444 = CARTESIAN_POINT ( 'NONE',  ( 1.234665194121939980, 1409.459554382089891, 232.4871809079789955 ) ) ;
#61446 = DIRECTION ( 'NONE',  ( 0.000000000000000000, -1.000000000000000000, 0.000000000000000000 ) ) ;
#61447 = ORIENTED_EDGE ( 'NONE', *, *, #81103, .F. ) ;
#61448 = CARTESIAN_POINT ( 'NONE',  ( 1.552532731868270011, 1415.658863691610122, 190.6831114793849906 ) ) ;
#61449 = FACE_OUTER_BOUND ( 'NONE', #39032, .T. ) ;
#61450 = CARTESIAN_POINT ( 'NONE',  ( -11.87502386937130083, 1433.007271227619867, 149.9804723889419904 ) ) ;
#61451 = CARTESIAN_POINT ( 'NONE',  ( 2.866730800962757897, 1410.390819565074935, 185.6792981423243418 ) ) ;
#61452 = CARTESIAN_POINT ( 'NONE',  ( -16.68463225901000158, 1445.052233488270076, 162.0935120915889911 ) ) ;
#61453 = CARTESIAN_POINT ( 'NONE',  ( 21.12212911287033279, 1511.187213306747708, 235.8226600804184443 ) ) ;
#61454 = CARTESIAN_POINT ( 'NONE',  ( -14.38070771612859922, 1509.494654091789926, 182.9202028628729977 ) ) ;
#61455 = CARTESIAN_POINT ( 'NONE',  ( -10.47436587960249987, 1490.889567392339814, 212.4387624771430012 ) ) ;
#61456 = CARTESIAN_POINT ( 'NONE',  ( -9.299417676539981414, 1446.922214017639817, 190.6945055697750036 ) ) ;
#61457 = CARTESIAN_POINT ( 'NONE',  ( -87.69898847370659212, 1383.771786689919963, 307.6789132609320063 ) ) ;
#61458 = CARTESIAN_POINT ( 'NONE',  ( -109.7957506965259995, 1384.357922284569895, 311.3498508118249788 ) ) ;
#61460 = EDGE_CURVE ( 'NONE', #60549, #27879, #92165, .T. ) ;
#61459 = DIRECTION ( 'NONE',  ( 0.6456859402676993209, 6.919574257186762174E-11, -0.7636030818040332457 ) ) ;
#61462 = ORIENTED_EDGE ( 'NONE', *, *, #65928, .T. ) ;
#61461 = CARTESIAN_POINT ( 'NONE',  ( 10.50858185005970036, 1452.061377940429793, 208.2223096714919848 ) ) ;
#61463 = CARTESIAN_POINT ( 'NONE',  ( -1.547463840030000037, 1414.913060387329779, 225.9340782259980074 ) ) ;
#61464 = CARTESIAN_POINT ( 'NONE',  ( -85.83179656309999928, 1383.342000450830028, 289.7170741207590368 ) ) ;
#61465 = CARTESIAN_POINT ( 'NONE',  ( 20.00533500179399837, 1509.034491922330062, 229.7041300313120189 ) ) ;
#61466 = EDGE_LOOP ( 'NONE', ( #68559, #102370, #58064, #81190, #59234, #72935, #3604, #78149, #16325, #86705, #36842, #45001, #52500, #65784 ) ) ;
#61467 = EDGE_LOOP ( 'NONE', ( #103175, #74037, #92459, #82305 ) ) ;
#61468 = CARTESIAN_POINT ( 'NONE',  ( 17.61796568584639999, 1509.217857668270199, 231.5269859153089840 ) ) ;
#61469 = LINE ( 'NONE', #95595, #88597 ) ;
#61470 = CARTESIAN_POINT ( 'NONE',  ( 12.77009498041144653, 1442.833833548704433, 169.4527319213308942 ) ) ;
#61472 = CARTESIAN_POINT ( 'NONE',  ( -13.60516178560000000, 1473.691177536529949, 264.8398105707980221 ) ) ;
#61471 = CARTESIAN_POINT ( 'NONE',  ( -32.28466283162165240, 1511.187213306747708, 199.0684425896249081 ) ) ;
#61473 = CARTESIAN_POINT ( 'NONE',  ( 8.616245162164020144, 1437.218212072470124, 208.3935038613939810 ) ) ;
#61474 = CARTESIAN_POINT ( 'NONE',  ( -108.5985451479999995, 1381.860774011350031, 297.8915311670589858 ) ) ;
#61475 = CARTESIAN_POINT ( 'NONE',  ( -113.4000000000000057, 1305.733110638860126, 304.2218459572590064 ) ) ;
#61476 = CARTESIAN_POINT ( 'NONE',  ( -19.69052972445629734, 1491.856921643429814, 228.3926998087940206 ) ) ;
#61477 = CARTESIAN_POINT ( 'NONE',  ( 12.38635162149999935, 1409.511637224330116, 190.7239812732980226 ) ) ;
#61478 = CARTESIAN_POINT ( 'NONE',  ( 5.210919876389999317, 1421.200875282130028, 185.9499441207979942 ) ) ;
#61479 = CARTESIAN_POINT ( 'NONE',  ( -5.268693358010000161, 1440.707873534420060, 154.8524945673979971 ) ) ;
#61480 = CARTESIAN_POINT ( 'NONE',  ( 12.48849012109999990, 1435.526020131319910, 150.8975386375979895 ) ) ;
#61481 = CARTESIAN_POINT ( 'NONE',  ( -13.11765501578049964, 1422.301116625370014, 203.8560779122109921 ) ) ;
#61482 = CARTESIAN_POINT ( 'NONE',  ( -11.00301372470000061, 1492.094802143589959, 210.0154403701209844 ) ) ;
#61483 = CARTESIAN_POINT ( 'NONE',  ( 2.194849219480000002, 1464.708290797229893, 236.4512993078980116 ) ) ;
#61484 = EDGE_LOOP ( 'NONE', ( #72628, #30696 ) ) ;
#61485 = CARTESIAN_POINT ( 'NONE',  ( -18.64588652299999794, 1416.828040475229955, 208.5593769277110141 ) ) ;
#61486 = CARTESIAN_POINT ( 'NONE',  ( 20.47195266477429954, 1476.322114778060040, 217.8381695920240020 ) ) ;
#61487 = CARTESIAN_POINT ( 'NONE',  ( -38.62502730119999939, 1456.952829106630134, 270.2651245533980386 ) ) ;
#61488 = FACE_OUTER_BOUND ( 'NONE', #23546, .T. ) ;
#61489 = CARTESIAN_POINT ( 'NONE',  ( 17.45344422499999837, 1410.019001477129905, 223.6090892349980095 ) ) ;
#61490 = CARTESIAN_POINT ( 'NONE',  ( -14.79501691930000007, 1474.161825565029858, 223.6789521170979924 ) ) ;
#61491 = CARTESIAN_POINT ( 'NONE',  ( 0.9746356023110001043, 1408.913060387329779, 190.4091760167980283 ) ) ;
#61492 = CARTESIAN_POINT ( 'NONE',  ( 2.769033333149520271, 1409.009757263489973, 230.2538554199990131 ) ) ;
#61493 = CARTESIAN_POINT ( 'NONE',  ( 2.483039260530000014, 1508.999772102629777, 238.0619777341980239 ) ) ;
#61494 = CARTESIAN_POINT ( 'NONE',  ( -4.174809892219999874, 1417.498982180929943, 233.1641891595979814 ) ) ;
#61495 = CARTESIAN_POINT ( 'NONE',  ( -9.447779140010000631, 1460.630169784690224, 214.7547266466890221 ) ) ;
#61496 = CARTESIAN_POINT ( 'NONE',  ( -4.745098151869999725, 1360.923919868640041, 207.6218459616989946 ) ) ;
#61497 = CARTESIAN_POINT ( 'NONE',  ( -44.83505966559869904, 1432.107508427250195, 267.6405665847250361 ) ) ;
#61498 = CARTESIAN_POINT ( 'NONE',  ( -3.598240451819999741, 1426.013882560829870, 186.0138310293980055 ) ) ;
#61499 = VERTEX_POINT ( 'NONE', #14531 ) ;
#61500 = CARTESIAN_POINT ( 'NONE',  ( -8.389049334679999248, 1423.485351373390131, 210.3439883204590046 ) ) ;
#61501 = AXIS2_PLACEMENT_3D ( 'NONE', #72152, #44171, #37419 ) ;
#61502 = VERTEX_POINT ( 'NONE', #40292 ) ;
#61503 = CARTESIAN_POINT ( 'NONE',  ( 0.7559394982620020187, 1516.972341476009888, 210.2438793621770117 ) ) ;
#61504 = CARTESIAN_POINT ( 'NONE',  ( 6.391938807520832988, 1508.551704408389696, 202.1089244633390365 ) ) ;
#61505 = CARTESIAN_POINT ( 'NONE',  ( -17.61101880491722582, 1419.781712659406367, 206.7560216166721716 ) ) ;
#61506 = DIRECTION ( 'NONE',  ( -0.02616798426453448984, -0.9993150019883495494, 0.02616798426619649023 ) ) ;
#61507 = CIRCLE ( 'NONE', #22121, 2.000000000000000000 ) ;
#61508 = CARTESIAN_POINT ( 'NONE',  ( -3.428237969637699667, 1497.215611306809706, 221.0357606766309857 ) ) ;
#61509 = B_SPLINE_SURFACE_WITH_KNOTS ( 'NONE', 5, 5, ( 
 ( #50960, #42547, #43110, #94591, #17870, #44780, #89510, #104660, #97899 ),
 ( #88956, #96266, #20098, #12248, #72726, #29067, #46437, #55378, #80569 ),
 ( #105222, #45880, #79474, #21171, #72195, #38015, #105784, #27957, #30142 ),
 ( #54291, #3884, #80017, #2783, #54832, #3338, #81105, #70543, #20628 ),
 ( #12801, #46981, #106315, #87316, #62140, #36351, #78930, #37462, #63782 ),
 ( #11175, #4422, #19543, #63250, #97359, #38547, #106850, #29597, #36903 ) ),
 .UNSPECIFIED., .F., .F., .F.,
 ( 6, 6 ),
 ( 6, 3, 6 ),
 ( 18.71477090770000018, 31.31580451349999805 ),
 ( 0.000000000000000000, 1.000000000000000000, 2.000000000000000000 ),
 .UNSPECIFIED. ) ;
#61510 = ORIENTED_EDGE ( 'NONE', *, *, #3542, .F. ) ;
#61511 = DIRECTION ( 'NONE',  ( 0.2054769195713296304, -0.000000000000000000, 0.9786619618251631847 ) ) ;
#61513 = CARTESIAN_POINT ( 'NONE',  ( 13.43268769770000048, 1434.818091166330078, 195.7542001346979816 ) ) ;
#61512 = CYLINDRICAL_SURFACE ( 'NONE', #99734, 2.000000000000003553 ) ;
#61514 =( BOUNDED_CURVE ( )  B_SPLINE_CURVE ( 3, ( #36227, #62008, #78223, #443 ),
 .UNSPECIFIED., .F., .F. ) 
 B_SPLINE_CURVE_WITH_KNOTS ( ( 4, 4 ),
 ( 3.450515127324310427, 4.712388980386121418 ),
 .UNSPECIFIED. ) 
 CURVE ( )  GEOMETRIC_REPRESENTATION_ITEM ( )  RATIONAL_B_SPLINE_CURVE ( ( 1.000000000000000000, 0.8716501122551647551, 0.8716501122551647551, 1.000000000000000000 ) ) 
 REPRESENTATION_ITEM ( '' )  );
#61515 = CARTESIAN_POINT ( 'NONE',  ( 11.18562212430000002, 1414.421228241719973, 205.5619752052589888 ) ) ;
#61516 = CARTESIAN_POINT ( 'NONE',  ( -14.35058941781813147, 1517.151704408390060, 193.9977807835901729 ) ) ;
#61517 = CARTESIAN_POINT ( 'NONE',  ( 7.243833416339999332, 1473.411017056090031, 218.0151120354589978 ) ) ;
#61518 = CARTESIAN_POINT ( 'NONE',  ( -9.056850508124879795, 1439.359654142089994, 207.7004169096410067 ) ) ;
#61519 = VERTEX_POINT ( 'NONE', #74477 ) ;
#61520 = CARTESIAN_POINT ( 'NONE',  ( -2.984254467278609990, 1410.459656091350098, 269.3356736250599965 ) ) ;
#61521 = CARTESIAN_POINT ( 'NONE',  ( -4.044319925355000400, 1517.073005577650065, 208.0013022344469960 ) ) ;
#61522 = CARTESIAN_POINT ( 'NONE',  ( 12.44762265580000005, 1419.324415493729930, 229.2325656297979890 ) ) ;
#61523 = FACE_OUTER_BOUND ( 'NONE', #23859, .T. ) ;
#61525 = ORIENTED_EDGE ( 'NONE', *, *, #12302, .F. ) ;
#61524 = CARTESIAN_POINT ( 'NONE',  ( -8.696701630039340714, 1367.135748871443866, 210.6218459616987957 ) ) ;
#61526 = ORIENTED_EDGE ( 'NONE', *, *, #67477, .T. ) ;
#61527 = CARTESIAN_POINT ( 'NONE',  ( -15.56469051740000076, 1506.798305107229908, 193.1680121121979994 ) ) ;
#61528 = CARTESIAN_POINT ( 'NONE',  ( -0.1587077902524139938, 1408.918602603690033, 186.0281839096400063 ) ) ;
#61529 = CARTESIAN_POINT ( 'NONE',  ( -11.01799577076803338, 1438.323741232346265, 152.2811882100368450 ) ) ;
#61530 = CARTESIAN_POINT ( 'NONE',  ( -0.02092469023549359958, 1409.011326956849871, 185.9381130483309903 ) ) ;
#61531 = CARTESIAN_POINT ( 'NONE',  ( -18.89626061867770090, 1416.765224585220039, 207.5748551965540116 ) ) ;
#61532 = CARTESIAN_POINT ( 'NONE',  ( -21.64080353419999980, 1425.805544261529803, 218.6154348525679723 ) ) ;
#61533 = CARTESIAN_POINT ( 'NONE',  ( 33.01176666536340321, 1465.417536072469829, 268.6111601533029898 ) ) ;
#61534 = CARTESIAN_POINT ( 'NONE',  ( -2.762021882724490229, 1466.850348183065080, 235.0881963227743654 ) ) ;
#61535 = CARTESIAN_POINT ( 'NONE',  ( 10.97111050090000184, 1445.273638288909979, 185.1428967657980138 ) ) ;
#61536 = CARTESIAN_POINT ( 'NONE',  ( -0.01327408612949850138, 1516.939877939420057, 205.6663500982469941 ) ) ;
#61537 = EDGE_LOOP ( 'NONE', ( #65525, #80230, #52293 ) ) ;
#61538 = CARTESIAN_POINT ( 'NONE',  ( 5.649719750514999639, 1514.243099272629934, 201.4728115316369781 ) ) ;
#61539 = CARTESIAN_POINT ( 'NONE',  ( 1.519281268484470093, 1457.051486531649971, 183.2989482105110142 ) ) ;
#61540 = CARTESIAN_POINT ( 'NONE',  ( 23.23064387430000011, 1409.829316784929915, 208.7297343454509928 ) ) ;
#61541 = ORIENTED_EDGE ( 'NONE', *, *, #36371, .F. ) ;
#61542 = LINE ( 'NONE', #10567, #7033 ) ;
#61543 = CARTESIAN_POINT ( 'NONE',  ( 25.74098603697060028, 1450.968017009530058, 136.8501568074100021 ) ) ;
#61544 = CARTESIAN_POINT ( 'NONE',  ( 14.45750869480000134, 1416.828040475729949, 196.8520545944980142 ) ) ;
#61545 = CARTESIAN_POINT ( 'NONE',  ( -9.321299325100000033, 1391.019964971690115, 208.8523807111220094 ) ) ;
#61546 = CARTESIAN_POINT ( 'NONE',  ( 6.805044835120149571, 1517.051704409849890, 212.9954169445540231 ) ) ;
#61547 = CARTESIAN_POINT ( 'NONE',  ( 18.64060035870000220, 1410.060184558130004, 195.0159613159980267 ) ) ;
#61548 = CARTESIAN_POINT ( 'NONE',  ( 17.11714625305219073, 1444.740067931810245, 162.7561045841208909 ) ) ;
#61549 = CARTESIAN_POINT ( 'NONE',  ( 2.910924238241502149, 1439.670359696568312, 183.9847715977047073 ) ) ;
#61551 = CARTESIAN_POINT ( 'NONE',  ( -18.59676279164743562, 1424.397502145024191, 224.8776118054202868 ) ) ;
#61550 = CARTESIAN_POINT ( 'NONE',  ( -2.330134126090000368, 1515.551704408389924, 205.2922258481490303 ) ) ;
#61552 = CARTESIAN_POINT ( 'NONE',  ( 0.7034066635819330449, 1450.888494735919949, 181.3301578859269796 ) ) ;
#61553 = CARTESIAN_POINT ( 'NONE',  ( -7.500000019064999357, 1508.551704408389924, 209.1218459511669892 ) ) ;
#61554 = CARTESIAN_POINT ( 'NONE',  ( -9.448886036450000248, 1383.288095429739997, 218.3547579606889997 ) ) ;
#61555 = CARTESIAN_POINT ( 'NONE',  ( -3.255340964424999761, 1516.962555622980062, 213.7459452615670159 ) ) ;
#61556 = DIRECTION ( 'NONE',  ( 0.000000000000000000, -1.000000000000000000, 0.000000000000000000 ) ) ;
#61557 = VERTEX_POINT ( 'NONE', #108604 ) ;
#61558 = CARTESIAN_POINT ( 'NONE',  ( -17.04997523780000179, 1417.320533121529934, 207.2791714270889827 ) ) ;
#61559 = CARTESIAN_POINT ( 'NONE',  ( 22.14913372576120310, 1525.402221411349956, 235.6690521037248232 ) ) ;
#61560 = CARTESIAN_POINT ( 'NONE',  ( 1234.711986934300057, 50.13405481578730161, -9668.243368257830298 ) ) ;
#61561 = CARTESIAN_POINT ( 'NONE',  ( -0.8395495568287499877, 1420.844234838699776, 193.7400646645540974 ) ) ;
#61562 = CARTESIAN_POINT ( 'NONE',  ( -0.2751659207381170202, 1506.798305148240161, 231.4088083080649767 ) ) ;
#61563 = CARTESIAN_POINT ( 'NONE',  ( -3.444929438629999563, 1456.909266842430043, 224.8635561661979807 ) ) ;
#61564 = CARTESIAN_POINT ( 'NONE',  ( 44.21391152859995088, 1449.831963904944814, 266.2303393994977796 ) ) ;
#61565 = CARTESIAN_POINT ( 'NONE',  ( 11.68203264559999965, 1433.008677914059945, 150.9219369944979974 ) ) ;
#61566 = CARTESIAN_POINT ( 'NONE',  ( 17.24149055319999846, 1446.934121893590145, 209.1218459616979999 ) ) ;
#61567 = CARTESIAN_POINT ( 'NONE',  ( 27.13067724103490264, 1440.913060389899783, 227.4319135845050255 ) ) ;
#61568 = CARTESIAN_POINT ( 'NONE',  ( 2.550034483959999765, 1426.916722803340235, 188.7149418613990122 ) ) ;
#61569 = FACE_OUTER_BOUND ( 'NONE', #11487, .T. ) ;
#61570 = B_SPLINE_CURVE_WITH_KNOTS ( 'NONE', 5,
 ( #78738, #2053, #36186, #18253, #86578, #27778, #9326, #35618, #94407, #70369, #11539, #19357, #61410, #18806, #62526, #17683, #79851, #69814, #10984, #103931, #10424 ),
 .UNSPECIFIED., .F., .F.,
 ( 6, 3, 3, 3, 3, 3, 6 ),
 ( 37.36625346989999485, 38.00991709350000036, 40.59642292560000243, 43.18292875779999918, 44.87875381330000124, 46.52360639289999966, 46.78685122110000094 ),
 .UNSPECIFIED. ) ;
#61571 = CIRCLE ( 'NONE', #15005, 23.99999935407219454 ) ;
#61572 = CARTESIAN_POINT ( 'NONE',  ( 9.680246906815670016, 1463.834245979629941, 210.7210319866079828 ) ) ;
#61573 = CARTESIAN_POINT ( 'NONE',  ( 11.75704293633499908, 1511.932705841380084, 199.9008530307569913 ) ) ;
#61574 = CARTESIAN_POINT ( 'NONE',  ( -7.460636413916523324, 1509.035273822891668, 203.0850875598481196 ) ) ;
#61575 = CARTESIAN_POINT ( 'NONE',  ( -7.580762144500440058, 1509.258003769659808, 239.0111317755749951 ) ) ;
#61576 = CARTESIAN_POINT ( 'NONE',  ( 24.69009492180000009, 1430.360063174630113, 210.5561083012179893 ) ) ;
#61577 = CIRCLE ( 'NONE', #6159, 7.799999999999999822 ) ;
#61578 = CARTESIAN_POINT ( 'NONE',  ( 33.93019615848955084, 1524.726013923371283, 220.5829544587961095 ) ) ;
#61579 = CARTESIAN_POINT ( 'NONE',  ( 25.91181804669769662, 1436.667520981494818, 136.9959711219258054 ) ) ;
#61580 = CARTESIAN_POINT ( 'NONE',  ( -30.85555029051230136, 1383.840996389519887, 228.7204722429899846 ) ) ;
#61581 = CARTESIAN_POINT ( 'NONE',  ( 18.68390451703509925, 1457.534965007319897, 220.6831946007679903 ) ) ;
#61582 = CARTESIAN_POINT ( 'NONE',  ( -3.447264387095000160, 1516.858765657450249, 212.5828932618570093 ) ) ;
#61583 = CARTESIAN_POINT ( 'NONE',  ( 1732.234191736389675, 11221.53578756870047, 2410.535515148488230 ) ) ;
#61584 = CARTESIAN_POINT ( 'NONE',  ( 0.1663705600157490139, 1482.467207184779909, 181.9884040192069961 ) ) ;
#61586 = ORIENTED_EDGE ( 'NONE', *, *, #74078, .F. ) ;
#61585 = CARTESIAN_POINT ( 'NONE',  ( 3.251026391689999961, 1442.093601194490020, 217.4966399718589969 ) ) ;
#61587 = CARTESIAN_POINT ( 'NONE',  ( -0.9041356905230000240, 1416.839648764230105, 228.0296119439979918 ) ) ;
#61588 = CARTESIAN_POINT ( 'NONE',  ( -1.112595545632909995E-15, 1378.856372334279968, 208.5307368469939888 ) ) ;
#61589 = CARTESIAN_POINT ( 'NONE',  ( -20.47737311789999737, 1507.835268392529997, 189.6592733436979756 ) ) ;
#61591 = ORIENTED_EDGE ( 'NONE', *, *, #77087, .F. ) ;
#61590 = CARTESIAN_POINT ( 'NONE',  ( -34.94829774809100087, 1451.625365366279766, 134.0999999983029909 ) ) ;
#61592 = CARTESIAN_POINT ( 'NONE',  ( -7.289512158268499853, 1508.551704406979979, 219.1144417387279759 ) ) ;
#61593 = ORIENTED_EDGE ( 'NONE', *, *, #91091, .F. ) ;
#61594 = B_SPLINE_SURFACE_WITH_KNOTS ( 'NONE', 5, 5, ( 
 ( #86545, #3682, #19323, #87666, #61936, #103900 ),
 ( #52968, #9839, #44006, #70340, #1445, #27200 ),
 ( #44558, #79269, #10955, #78708, #2579, #78143 ),
 ( #46233, #95501, #36701, #71456, #87100, #96615 ),
 ( #10387, #70895, #2021, #62494, #19883, #88215 ),
 ( #79823, #3129, #105011, #80366, #36156, #11509 ) ),
 .UNSPECIFIED., .F., .F., .F.,
 ( 6, 6 ),
 ( 6, 6 ),
 ( 21.97924354190000074, 24.12443845669999831 ),
 ( 0.000000000000000000, 2.000000000000000000 ),
 .UNSPECIFIED. ) ;
#61595 = CARTESIAN_POINT ( 'NONE',  ( -12.29063289509999990, 1392.314904069939985, 209.7401570312620152 ) ) ;
#61596 = CARTESIAN_POINT ( 'NONE',  ( -15.42960834800000036, 1414.913060387329779, 213.9579542055979857 ) ) ;
#61597 = CARTESIAN_POINT ( 'NONE',  ( -16.66700976312892735, 1523.530935881284904, 237.7590780485276127 ) ) ;
#61598 = CARTESIAN_POINT ( 'NONE',  ( 23.42684948969804992, 1410.407670420856903, 207.9130917326585859 ) ) ;
#61599 = CARTESIAN_POINT ( 'NONE',  ( -2.832025688439999911, 1432.290876391289885, 217.1988707364989750 ) ) ;
#61600 = CARTESIAN_POINT ( 'NONE',  ( -17.17241001986462123, 1511.187213306747708, 238.6251415217917895 ) ) ;
#61601 = CARTESIAN_POINT ( 'NONE',  ( 13.18296707766739928, 1409.373419738079974, 216.1545172977099867 ) ) ;
#61602 = CARTESIAN_POINT ( 'NONE',  ( -11.97267500829999953, 1391.195698933469885, 205.7774971565190185 ) ) ;
#61603 = CARTESIAN_POINT ( 'NONE',  ( -91.57239150403411543, 1385.197581008679890, 293.4610811371219938 ) ) ;
#61604 = CARTESIAN_POINT ( 'NONE',  ( -17.62970124079999934, 1421.466017064829884, 191.9566022962980014 ) ) ;
#61605 = CARTESIAN_POINT ( 'NONE',  ( -66.34652574609999931, 1379.749084393009980, 275.3210452576589660 ) ) ;
#61606 = EDGE_LOOP ( 'NONE', ( #18331, #29630, #79356, #27743 ) ) ;
#61607 = CARTESIAN_POINT ( 'NONE',  ( 12.29736470286800021, 1491.830670002519810, 208.2396171870099977 ) ) ;
#61609 = VERTEX_POINT ( 'NONE', #31892 ) ;
#61608 = DIRECTION ( 'NONE',  ( 0.000000000000000000, -1.000000000000000000, 0.000000000000000000 ) ) ;
#61610 = CARTESIAN_POINT ( 'NONE',  ( 9.033634059603929956, 1464.908125515270058, 213.0612947626739810 ) ) ;
#61611 = ORIENTED_EDGE ( 'NONE', *, *, #63890, .T. ) ;
#61612 = CARTESIAN_POINT ( 'NONE',  ( 1.842962215417941030, 1515.551704407336274, 205.1377642066082672 ) ) ;
#61613 = CARTESIAN_POINT ( 'NONE',  ( 6.161840689439245899, 1363.362512618330584, 208.3718459617061285 ) ) ;
#61614 = CARTESIAN_POINT ( 'NONE',  ( -1.480799215376189970, 1496.171220128179812, 196.8656195411859926 ) ) ;
#61615 = B_SPLINE_CURVE_WITH_KNOTS ( 'NONE', 3,
 ( #68655, #104997, #102756, #1433 ),
 .UNSPECIFIED., .F., .F.,
 ( 4, 4 ),
 ( 0.000000000000000000, 0.0002220129587134779374 ),
 .UNSPECIFIED. ) ;
#61616 = CARTESIAN_POINT ( 'NONE',  ( 29.83089294303868400, 1462.373024423122388, 269.4690121057988677 ) ) ;
#61617 = CARTESIAN_POINT ( 'NONE',  ( -32.99911596133562597, 1524.244163922424150, 222.0809728102186114 ) ) ;
#61618 = CARTESIAN_POINT ( 'NONE',  ( -0.02816727408130000054, 1396.454734798629943, 221.5795905815979836 ) ) ;
#61619 = CARTESIAN_POINT ( 'NONE',  ( 32.54480841269636926, 1524.547873515804895, 201.1604127401539586 ) ) ;
#61620 = CARTESIAN_POINT ( 'NONE',  ( -4.148213077643431390, 1517.003210141817590, 215.3943059606615122 ) ) ;
#61621 = CARTESIAN_POINT ( 'NONE',  ( -19.49005507420071481, 1486.272062043716232, 189.7901318363738596 ) ) ;
#61622 = CARTESIAN_POINT ( 'NONE',  ( -9.938521104460262379, 1368.703998991882372, 209.6218459617033432 ) ) ;
#61623 = CARTESIAN_POINT ( 'NONE',  ( -8.756942758513574177, 1511.516807858200764, 214.9135418063871725 ) ) ;
#61624 = CARTESIAN_POINT ( 'NONE',  ( 0.7135562203500009915, 1457.486859021590135, 199.6029537853190163 ) ) ;
#61625 = CARTESIAN_POINT ( 'NONE',  ( 5.770883563884999568, 1516.603620185149794, 206.8276363026970159 ) ) ;
#61626 = CARTESIAN_POINT ( 'NONE',  ( -2.356894939219843721, 1525.394081235439444, 176.3139379204273496 ) ) ;
#61627 = B_SPLINE_SURFACE_WITH_KNOTS ( 'NONE', 3, 5, ( 
 ( #84045, #5140, #41507, #109809, #67276, #101370 ),
 ( #24660, #58861, #13519, #47707, #25777, #59975 ),
 ( #42054, #102487, #95212, #33626, #43708, #52670 ),
 ( #103035, #86805, #17922, #10096, #70049, #64 ) ),
 .UNSPECIFIED., .F., .F., .F.,
 ( 4, 4 ),
 ( 6, 6 ),
 ( 5.479561955569999476, 5.505632801470000004 ),
 ( 0.000000000000000000, 1.000000000000000000 ),
 .UNSPECIFIED. ) ;
#61628 = CARTESIAN_POINT ( 'NONE',  ( -15.85691707105240233, 1416.756521790129909, 226.9090633924639917 ) ) ;
#61629 = DIRECTION ( 'NONE',  ( 3.828588921590000582E-16, 0.000000000000000000, 1.000000000000000000 ) ) ;
#61631 = VERTEX_POINT ( 'NONE', #66078 ) ;
#61630 = CARTESIAN_POINT ( 'NONE',  ( -68.77190087506669158, 1379.747925807530009, 280.3125204381590265 ) ) ;
#61632 = CARTESIAN_POINT ( 'NONE',  ( -3.290427993577100100E-15, 1522.051704408389924, 209.1218459616989946 ) ) ;
#61633 = ORIENTED_EDGE ( 'NONE', *, *, #27517, .F. ) ;
#61634 = CARTESIAN_POINT ( 'NONE',  ( 20.04380005080000160, 1410.189663056929930, 264.7217086931980248 ) ) ;
#61635 = EDGE_CURVE ( 'NONE', #84894, #109869, #56199, .T. ) ;
#61636 = CARTESIAN_POINT ( 'NONE',  ( -26.53588231930000063, 1469.248395155229900, 208.5390332338009785 ) ) ;
#61638 = CARTESIAN_POINT ( 'NONE',  ( 16.27481265766170182, 1409.481380943289878, 193.1811559459430043 ) ) ;
#61637 = CARTESIAN_POINT ( 'NONE',  ( -0.5349228561300000129, 1502.013778628930140, 181.0478107783980022 ) ) ;
#61639 = EDGE_CURVE ( 'NONE', #3955, #23258, #33525, .T. ) ;
#61640 = CARTESIAN_POINT ( 'NONE',  ( -3.251888867474999945, 1516.793978928989873, 211.6142896211370044 ) ) ;
#61641 = CARTESIAN_POINT ( 'NONE',  ( 8.991744574390811096, 1509.227061438039982, 181.2342617849590169 ) ) ;
#61642 = CARTESIAN_POINT ( 'NONE',  ( -21.00608537249999941, 1420.811742010229864, 244.4374624675979817 ) ) ;
#61643 = CARTESIAN_POINT ( 'NONE',  ( -13.24974103930710001, 1379.480115360689979, 208.4658629847600082 ) ) ;
#61644 = EDGE_CURVE ( 'NONE', #105869, #101745, #21335, .T. ) ;
#61645 = CARTESIAN_POINT ( 'NONE',  ( 17.46643367109724210, 1460.003880594037355, 228.4215481240995302 ) ) ;
#61646 = EDGE_CURVE ( 'NONE', #19916, #68294, #27915, .T. ) ;
#61647 = CARTESIAN_POINT ( 'NONE',  ( 4.751795985444269732, 1508.551704408389924, 212.6676576963480159 ) ) ;
#61648 = B_SPLINE_CURVE_WITH_KNOTS ( 'NONE', 3,
 ( #57020, #97882, #91145, #5489, #30688, #81629, #73817, #4405, #22813, #106834, #55915, #64319, #48617, #54813, #64875, #88940, #72180, #21157, #39648, #98982, #29582, #6041, #71645, #63767, #30127, #21711, #105765, #55362, #89495, #90034, #110703, #14971, #6593, #102292, #41846, #33994, #15518, #49715 ),
 .UNSPECIFIED., .F., .F.,
 ( 4, 2, 2, 2, 1, 1, 2, 2, 2, 2, 2, 1, 1, 2, 2, 2, 2, 1, 1, 2, 2, 4 ),
 ( 0.000000000000000000, 0.1250000000000867639, 0.1875000000001262046, 0.2187500000001459111, 0.2343750000001556810, 0.2421875000001605105, 0.2460937500001808276, 0.2500000000002011724, 0.3750000000002833844, 0.4375000000003333445, 0.4687500000002819966, 0.4843750000001906808, 0.4921875000001450506, 0.4960937500001328382, 0.5000000000001205702, 0.6249999999981388221, 0.6874999999972273290, 0.7187499999967783548, 0.7343749999965537567, 0.7421874999965470954, 0.7499999999965404340, 1.000000000000000000 ),
 .UNSPECIFIED. ) ;
#61649 = CARTESIAN_POINT ( 'NONE',  ( 30.82338449939999947, 1451.380982548830161, 136.0366644220979992 ) ) ;
#61650 = ORIENTED_EDGE ( 'NONE', *, *, #43488, .F. ) ;
#61651 = CARTESIAN_POINT ( 'NONE',  ( 12.55301046429960010, 1396.410217408039898, 207.1735117289620121 ) ) ;
#61652 = CARTESIAN_POINT ( 'NONE',  ( 9.691001514874608702, 1460.607649338439842, 206.2887977507070048 ) ) ;
#61653 = CARTESIAN_POINT ( 'NONE',  ( -17.73420755029999896, 1458.087872027529784, 230.3493948207980395 ) ) ;
#61654 = ORIENTED_EDGE ( 'NONE', *, *, #41943, .F. ) ;
#61655 = ORIENTED_EDGE ( 'NONE', *, *, #25479, .F. ) ;
#61656 = AXIS2_PLACEMENT_3D ( 'NONE', #103358, #60861, #26660 ) ;
#61657 = CARTESIAN_POINT ( 'NONE',  ( -29.25822673101280103, 1509.934902468239898, 211.7095298021968688 ) ) ;
#61658 = CARTESIAN_POINT ( 'NONE',  ( 8.185842985679999018, 1424.900152294199870, 195.0776991219990180 ) ) ;
#61659 = VERTEX_POINT ( 'NONE', #35204 ) ;
#61660 = DIRECTION ( 'NONE',  ( -0.8771707016849432659, 0.03063147587993800616, 0.4792006602572261298 ) ) ;
#61661 = DIRECTION ( 'NONE',  ( 1.755985294532464991E-16, -1.000000000000000000, 1.338183447452830017E-16 ) ) ;
#61662 = AXIS2_PLACEMENT_3D ( 'NONE', #88119, #3573, #29292 ) ;
#61663 = CARTESIAN_POINT ( 'NONE',  ( 3.068292148159999111E-16, 1443.913060387330006, 150.8032249175980155 ) ) ;
#61664 = AXIS2_PLACEMENT_3D ( 'NONE', #63942, #4567, #106468 ) ;
#61665 = CARTESIAN_POINT ( 'NONE',  ( 27.44625298708299965, 1509.338202929293629, 206.1591719864515539 ) ) ;
#61666 = CARTESIAN_POINT ( 'NONE',  ( 6.141397696570729536, 1509.034509440879901, 201.6091292273739839 ) ) ;
#61667 = CARTESIAN_POINT ( 'NONE',  ( 10.01188687081839923, 1451.710540692399945, 207.8449781661669817 ) ) ;
#61668 = CARTESIAN_POINT ( 'NONE',  ( -7.105427357599999217E-15, 1405.913060387330006, 146.1721969590979882 ) ) ;
#61669 = EDGE_CURVE ( 'NONE', #101516, #57941, #76230, .T. ) ;
#61670 = CARTESIAN_POINT ( 'NONE',  ( 15.54069288670000049, 1507.627023022229878, 225.9574102441980017 ) ) ;
#61671 = ORIENTED_EDGE ( 'NONE', *, *, #30125, .T. ) ;
#61672 = CARTESIAN_POINT ( 'NONE',  ( 4.032397901875000024, 1516.981965530290154, 203.3362630185569913 ) ) ;
#61673 = CARTESIAN_POINT ( 'NONE',  ( -7.323390445344999833, 1516.613712827999962, 210.2512321725070024 ) ) ;
#61674 = EDGE_LOOP ( 'NONE', ( #105570, #58634, #109549, #38884, #58073 ) ) ;
#61675 = CARTESIAN_POINT ( 'NONE',  ( 11.86432389000050058, 1432.211847865620030, 149.9809511090870160 ) ) ;
#61676 = CARTESIAN_POINT ( 'NONE',  ( 12.90042423989156539, 1444.934230273330741, 186.7320187782142966 ) ) ;
#61677 = ORIENTED_EDGE ( 'NONE', *, *, #870, .T. ) ;
#61678 = CARTESIAN_POINT ( 'NONE',  ( -15.66042904120755530, 1506.491018782441415, 193.6263806956001758 ) ) ;
#61679 = CARTESIAN_POINT ( 'NONE',  ( -13.32090919908733184, 1443.086052842848630, 169.4274452085711573 ) ) ;
#61680 = CARTESIAN_POINT ( 'NONE',  ( 7.178613415919999241, 1509.106095133629879, 236.6937018893979996 ) ) ;
#61681 = EDGE_CURVE ( 'NONE', #80762, #87917, #108233, .T. ) ;
#61682 = CARTESIAN_POINT ( 'NONE',  ( -2.546183590178249911, 1469.518995656580046, 218.8843719520340017 ) ) ;
#61683 = CARTESIAN_POINT ( 'NONE',  ( -5.249809024070000163, 1423.060572135929988, 185.6431024777980099 ) ) ;
#61684 = CARTESIAN_POINT ( 'NONE',  ( 1.476720148826540013, 1407.665894306529935, 270.1373298275569823 ) ) ;
#61685 = CARTESIAN_POINT ( 'NONE',  ( 9.219719605386430317, 1450.420523551490078, 208.9716825880909994 ) ) ;
#61686 = CARTESIAN_POINT ( 'NONE',  ( -109.8861939232002243, 1383.682673601628721, 297.0706783926800654 ) ) ;
#61687 = EDGE_CURVE ( 'NONE', #50393, #98226, #52021, .T. ) ;
#61688 = CARTESIAN_POINT ( 'NONE',  ( -2.243780305749810022, 1421.777182300220147, 193.4398524306369893 ) ) ;
#61689 = CARTESIAN_POINT ( 'NONE',  ( -44.12060424749999754, 1379.737242085850085, 229.5711980135589840 ) ) ;
#61690 = CARTESIAN_POINT ( 'NONE',  ( 0.03018028484158630925, 1410.288634417731828, 233.2216252247569059 ) ) ;
#61692 = CARTESIAN_POINT ( 'NONE',  ( 13.79590907669999922, 1416.844618642430078, 196.3342910144979783 ) ) ;
#61691 = CARTESIAN_POINT ( 'NONE',  ( -16.37972239500000171, 1503.881811289090138, 209.1238707911080041 ) ) ;
#61693 = CARTESIAN_POINT ( 'NONE',  ( -68.70081072619076679, 1379.747840807290004, 280.2881824009641605 ) ) ;
#61694 = CARTESIAN_POINT ( 'NONE',  ( -9.950123583630629653, 1439.590930467720227, 208.1650611593379949 ) ) ;
#61695 = CARTESIAN_POINT ( 'NONE',  ( -3.910936927762319382, 1506.384142095322204, 187.5277711242953558 ) ) ;
#61696 = EDGE_LOOP ( 'NONE', ( #32012, #95216, #110554, #93205 ) ) ;
#61697 = CARTESIAN_POINT ( 'NONE',  ( 36.06124926539999365, 1440.913060387330006, 262.6648722463980334 ) ) ;
#61698 = FACE_OUTER_BOUND ( 'NONE', #44771, .T. ) ;
#61699 = CARTESIAN_POINT ( 'NONE',  ( -18.37487226820799080, 1526.382868172863937, 182.5038319547590788 ) ) ;
#61700 = AXIS2_PLACEMENT_3D ( 'NONE', #110096, #33371, #16011 ) ;
#61701 = CARTESIAN_POINT ( 'NONE',  ( 4.554577183490000181, 1505.451005863290220, 220.6211971874989786 ) ) ;
#61702 = CARTESIAN_POINT ( 'NONE',  ( -14.25826133790000050, 1415.677402202029953, 214.0085705200789903 ) ) ;
#61704 = ORIENTED_EDGE ( 'NONE', *, *, #86265, .T. ) ;
#61703 = CARTESIAN_POINT ( 'NONE',  ( -1.179283247376800015, 1515.094876538340031, 204.7931849540779865 ) ) ;
#61705 = CARTESIAN_POINT ( 'NONE',  ( -17.31754310717619916, 1417.857287168520088, 205.5202013651170034 ) ) ;
#61706 = DIRECTION ( 'NONE',  ( 1.755985294532464991E-16, -1.000000000000000000, 1.338183447452830017E-16 ) ) ;
#61707 = CARTESIAN_POINT ( 'NONE',  ( -1.538335019100957712, 1450.609501681909705, 154.2722877154876926 ) ) ;
#61708 = DIRECTION ( 'NONE',  ( -0.9980919085851078787, 0.06174578541841399537, 0.000000000000000000 ) ) ;
#61709 = CARTESIAN_POINT ( 'NONE',  ( 12.61087482253499914, 1512.195694528090144, 224.2019839780669770 ) ) ;
#61710 = CARTESIAN_POINT ( 'NONE',  ( -8.887191752339999695, 1441.011119473389954, 186.5506309111979704 ) ) ;
#61711 = CIRCLE ( 'NONE', #18734, 2.000000000000001776 ) ;
#61712 = CARTESIAN_POINT ( 'NONE',  ( 14.31460734255390044, 1509.452787273769900, 235.1998026213640003 ) ) ;
#61713 = CARTESIAN_POINT ( 'NONE',  ( 5.992819232552546005, 1414.913060387329779, 220.0916279853276762 ) ) ;
#61714 = CARTESIAN_POINT ( 'NONE',  ( 11.97711953749976566, 1433.612589388432525, 149.8655202104944237 ) ) ;
#61715 = CARTESIAN_POINT ( 'NONE',  ( 11.74455360470000187, 1415.078310370329973, 229.3304074566979978 ) ) ;
#61716 = DIRECTION ( 'NONE',  ( -0.000000000000000000, -1.000000000000000000, -0.000000000000000000 ) ) ;
#61717 = CARTESIAN_POINT ( 'NONE',  ( -16.16331440049999912, 1459.159538815530141, 229.6201761408979962 ) ) ;
#61718 = CARTESIAN_POINT ( 'NONE',  ( -3.461995196814999787, 1516.906233342200039, 206.2559344154570056 ) ) ;
#61719 = CARTESIAN_POINT ( 'NONE',  ( 45.63714522919999439, 1438.938960590560100, 268.9747551788980218 ) ) ;
#61720 = CARTESIAN_POINT ( 'NONE',  ( -32.39315898239540559, 1526.178928173328131, 216.9314351822684728 ) ) ;
#61721 = CARTESIAN_POINT ( 'NONE',  ( 22.15911651489999912, 1435.271885453649929, 140.1193622846980134 ) ) ;
#61722 = CARTESIAN_POINT ( 'NONE',  ( 19.70550280570000012, 1469.160055952030007, 191.5645849787979955 ) ) ;
#61723 = PRODUCT_DEFINITION ( 'UNKNOWN', '', #56603, #21031 ) ;
#61724 = CARTESIAN_POINT ( 'NONE',  ( 20.13566257103952850, 1506.560172254411782, 218.2038963799658120 ) ) ;
#61725 = CARTESIAN_POINT ( 'NONE',  ( -13.78554130023140090, 1379.661829793600191, 208.1182657059560199 ) ) ;
#61726 = CARTESIAN_POINT ( 'NONE',  ( -17.44898219039999887, 1420.862956884029927, 226.4473557759979769 ) ) ;
#61727 = DIRECTION ( 'NONE',  ( 0.000000000000000000, 0.000000000000000000, 1.000000000000000000 ) ) ;
#61728 = CARTESIAN_POINT ( 'NONE',  ( -41.49258008709740153, 1443.691026079749918, 136.5669671037899775 ) ) ;
#61729 = CARTESIAN_POINT ( 'NONE',  ( -17.49859601832923417, 1506.366982239744175, 195.8448425805984527 ) ) ;
#61730 = CARTESIAN_POINT ( 'NONE',  ( -18.00081235489999898, 1415.932617989529945, 205.2446752400179832 ) ) ;
#61731 = CARTESIAN_POINT ( 'NONE',  ( -12.45220969719999893, 1442.685518086189859, 186.6444734887980132 ) ) ;
#61732 = CARTESIAN_POINT ( 'NONE',  ( -7.594207177912499773, 1384.073165582419961, 219.0227910255269990 ) ) ;
#61733 = CARTESIAN_POINT ( 'NONE',  ( -28.12789902060000102, 1435.479491205339855, 135.2461919473980174 ) ) ;
#61734 = ORIENTED_EDGE ( 'NONE', *, *, #51525, .F. ) ;
#61735 = CARTESIAN_POINT ( 'NONE',  ( 5.671687374334005938, 1510.518062812720245, 216.6698829330774458 ) ) ;
#61736 = CARTESIAN_POINT ( 'NONE',  ( -14.16617799454949989, 1409.407754223660049, 213.8599483261789942 ) ) ;
#61737 = EDGE_CURVE ( 'NONE', #84088, #91565, #75864, .T. ) ;
#61738 = FACE_OUTER_BOUND ( 'NONE', #54845, .T. ) ;
#61739 = CARTESIAN_POINT ( 'NONE',  ( -38.12305826662554864, 1442.831169986191071, 136.9078781414296486 ) ) ;
#61740 = CARTESIAN_POINT ( 'NONE',  ( -44.90007994049999951, 1451.198737828930007, 268.2456369373979896 ) ) ;
#61741 = CARTESIAN_POINT ( 'NONE',  ( -17.07205270619999737, 1501.040019927530011, 224.0489642073979724 ) ) ;
#61742 = CARTESIAN_POINT ( 'NONE',  ( 0.1616573738338789867, 1420.153416094779914, 183.7945939761100078 ) ) ;
#61743 = ADVANCED_FACE ( 'NONE', ( #96222 ), #100167, .T. ) ;
#61744 = CARTESIAN_POINT ( 'NONE',  ( -26.64291118699999927, 1508.595174534829994, 214.1515268407479766 ) ) ;
#61745 = CARTESIAN_POINT ( 'NONE',  ( -62.29576501915909859, 1384.687103135880079, 284.7157575292210367 ) ) ;
#61746 = CARTESIAN_POINT ( 'NONE',  ( -10.29144330875089963, 1384.933285862410003, 200.0364846665950154 ) ) ;
#61747 = CARTESIAN_POINT ( 'NONE',  ( 17.12821735161499959, 1423.039456014099869, 226.8410098145990048 ) ) ;
#61748 = CARTESIAN_POINT ( 'NONE',  ( 20.85997183230000118, 1508.960091291929984, 227.7506528288980121 ) ) ;
#61749 = LINE ( 'NONE', #62880, #295 ) ;
#61750 = CARTESIAN_POINT ( 'NONE',  ( -105.7942887633819993, 1378.913060387289988, 304.0474587704230203 ) ) ;
#61751 = CARTESIAN_POINT ( 'NONE',  ( 4.217994498490000410, 1515.470302801990101, 208.3798112177819917 ) ) ;
#61752 = CARTESIAN_POINT ( 'NONE',  ( -7.965680540240001051, 1384.926148861439970, 199.4891222871690104 ) ) ;
#61753 = CARTESIAN_POINT ( 'NONE',  ( 1.420259601960000229, 1466.712985171129958, 235.0376566307980113 ) ) ;
#61754 = LINE ( 'NONE', #18049, #67638 ) ;
#61755 = CARTESIAN_POINT ( 'NONE',  ( 3.487592429898332291, 1508.783371651612924, 204.5758637223170808 ) ) ;
#61756 = ADVANCED_FACE ( 'NONE', ( #1627 ), #63210, .T. ) ;
#61757 = CARTESIAN_POINT ( 'NONE',  ( 3.428010664469999913, 1421.954222488810274, 194.0794391570989887 ) ) ;
#61758 = CARTESIAN_POINT ( 'NONE',  ( 22.27261620720000224, 1409.690837284130112, 212.5637969276579895 ) ) ;
#61759 = B_SPLINE_SURFACE_WITH_KNOTS ( 'NONE', 5, 5, ( 
 ( #46173, #78644, #52906, #1388, #104947, #105506 ),
 ( #3618, #19259, #62995, #10325, #35529, #79211 ),
 ( #69723, #1959, #28238, #27689, #61873, #88160 ),
 ( #97103, #80302, #28796, #87038, #37197, #103841 ),
 ( #94889, #45623, #54575, #36641, #10894, #79762 ),
 ( #27142, #53462, #70284, #20369, #18165, #52362 ),
 ( #88710, #61327, #36097, #86479, #95445, #87607 ),
 ( #45068, #2518, #3070, #11990, #107700, #64069 ),
 ( #99275, #91453, #81373, #30434, #47797, #73567 ) ),
 .UNSPECIFIED., .F., .F., .F.,
 ( 6, 3, 6 ),
 ( 6, 6 ),
 ( 3.503225402400000021, 8.166373431240000258, 13.04304411370000061 ),
 ( 0.000000000000000000, 2.000000000000000000 ),
 .UNSPECIFIED. ) ;
#61760 = DIRECTION ( 'NONE',  ( 0.5877852522924709167, 0.000000000000000000, 0.8090169943749491166 ) ) ;
#61761 = CARTESIAN_POINT ( 'NONE',  ( 20.84180957800000300, 1457.800270462289973, 206.7197162310789906 ) ) ;
#61762 = CARTESIAN_POINT ( 'NONE',  ( -14.45783243223209880, 1416.839692136300073, 221.3920770721769884 ) ) ;
#61764 = CARTESIAN_POINT ( 'NONE',  ( -10.63394288230000129, 1381.391042983399984, 201.9860236516190071 ) ) ;
#61763 = CARTESIAN_POINT ( 'NONE',  ( -11.87502393780000176, 1433.007271555939951, 149.9804723930980117 ) ) ;
#61765 = CARTESIAN_POINT ( 'NONE',  ( -5.166416716789999697, 1391.906184330890028, 203.6779378933989904 ) ) ;
#61766 = CARTESIAN_POINT ( 'NONE',  ( -18.69816095120731347, 1526.382868172863937, 234.8576566410005171 ) ) ;
#61767 = CARTESIAN_POINT ( 'NONE',  ( -11.36252066009999950, 1490.577502786289870, 210.2371618091489722 ) ) ;
#61768 = CARTESIAN_POINT ( 'NONE',  ( -24.91018336865660743, 1509.782943158774287, 193.9316171199673420 ) ) ;
#61769 = CARTESIAN_POINT ( 'NONE',  ( -9.832966357650001044, 1364.062280235949856, 210.6218459616991936 ) ) ;
#61770 = CARTESIAN_POINT ( 'NONE',  ( -4.621897862544999569, 1516.858533673840157, 204.5099662467769974 ) ) ;
#61771 = B_SPLINE_CURVE_WITH_KNOTS ( 'NONE', 3,
 ( #63217, #82171, #5471, #20593 ),
 .UNSPECIFIED., .F., .F.,
 ( 4, 4 ),
 ( -36.72426899450000093, -23.80234877754210032 ),
 .UNSPECIFIED. ) ;
#61772 = CARTESIAN_POINT ( 'NONE',  ( 1.058603163941309822, 1414.913060387330006, 192.7445404878875763 ) ) ;
#61773 = EDGE_CURVE ( 'NONE', #68158, #107607, #25876, .T. ) ;
#61774 = CARTESIAN_POINT ( 'NONE',  ( -14.18548177819419998, 1485.573726300379803, 186.3991088774869809 ) ) ;
#61775 = CARTESIAN_POINT ( 'NONE',  ( 1.932231105370000090, 1508.750808003230077, 237.3393916369980161 ) ) ;
#61776 = CARTESIAN_POINT ( 'NONE',  ( 8.301429727154969740, 1503.992660670129908, 218.3431214713440056 ) ) ;
#61777 = CARTESIAN_POINT ( 'NONE',  ( 41.14071512850430423, 1444.183191039890062, 136.8991235379290003 ) ) ;
#61779 = ORIENTED_EDGE ( 'NONE', *, *, #98012, .T. ) ;
#61778 = CARTESIAN_POINT ( 'NONE',  ( -66.39208760710349111, 1379.743175614790061, 277.0517417713629698 ) ) ;
#61780 = ORIENTED_EDGE ( 'NONE', *, *, #107789, .T. ) ;
#61781 = CARTESIAN_POINT ( 'NONE',  ( 11.16774673678820129, 1434.096752951460076, 151.6376635257900034 ) ) ;
#61782 = CARTESIAN_POINT ( 'NONE',  ( 21.64969004981279355, 1524.547873515805122, 183.5515527622214051 ) ) ;
#61783 = ORIENTED_EDGE ( 'NONE', *, *, #83682, .F. ) ;
#61784 = CARTESIAN_POINT ( 'NONE',  ( -0.02999094720359275421, 1457.653887067397136, 199.5863383128643420 ) ) ;
#61786 = EDGE_CURVE ( 'NONE', #93671, #51820, #4379, .T. ) ;
#61785 = CIRCLE ( 'NONE', #102884, 2.000000000000001776 ) ;
#61787 = CARTESIAN_POINT ( 'NONE',  ( 1.547463840030000037, 1414.913060387329779, 192.3096136973980208 ) ) ;
#61789 = FACE_OUTER_BOUND ( 'NONE', #46328, .T. ) ;
#61788 = CARTESIAN_POINT ( 'NONE',  ( 18.53418652026280000, 1507.620785850910124, 188.5293807599879869 ) ) ;
#61790 = FACE_OUTER_BOUND ( 'NONE', #93246, .T. ) ;
#61791 = EDGE_CURVE ( 'NONE', #10311, #26525, #22234, .T. ) ;
#61792 = CARTESIAN_POINT ( 'NONE',  ( 1.100342456369999944, 1488.175276620729846, 181.8693589272980091 ) ) ;
#61793 = CARTESIAN_POINT ( 'NONE',  ( -105.8748966381740075, 1378.913060387980067, 304.8767970569450085 ) ) ;
#61794 = CARTESIAN_POINT ( 'NONE',  ( 16.23184890680000336, 1409.981663893229779, 226.5335387243980279 ) ) ;
#61795 = SURFACE_STYLE_FILL_AREA ( #28159 ) ;
#61796 = CARTESIAN_POINT ( 'NONE',  ( -7.710285875814999912, 1516.582197289609894, 212.3822242253069987 ) ) ;
#61798 = CIRCLE ( 'NONE', #108270, 1.000000000000010436 ) ;
#61797 = CARTESIAN_POINT ( 'NONE',  ( -3.887243918150000104E-16, 1418.913060387330006, 172.2701767054979882 ) ) ;
#61799 = CARTESIAN_POINT ( 'NONE',  ( -4.877525059390000806, 1387.235931102789891, 214.6572145122790118 ) ) ;
#61800 = CARTESIAN_POINT ( 'NONE',  ( -20.26516707829999930, 1485.407934329090040, 205.1093585495989942 ) ) ;
#61801 = ORIENTED_EDGE ( 'NONE', *, *, #53726, .T. ) ;
#61802 = CARTESIAN_POINT ( 'NONE',  ( 13.65820430843470135, 1435.058683561780072, 149.3325756827849773 ) ) ;
#61803 = EDGE_LOOP ( 'NONE', ( #2267, #68400, #67488 ) ) ;
#61804 = ORIENTED_EDGE ( 'NONE', *, *, #14581, .F. ) ;
#61805 = ORIENTED_EDGE ( 'NONE', *, *, #28761, .F. ) ;
#61806 = ADVANCED_FACE ( 'NONE', ( #88918 ), #12204, .F. ) ;
#61807 = CARTESIAN_POINT ( 'NONE',  ( 12.73783686771306378, 1445.004038133846052, 169.4561619195475544 ) ) ;
#61808 = CARTESIAN_POINT ( 'NONE',  ( -1.063679678840000031, 1465.068952327929992, 237.9910134151979832 ) ) ;
#61809 = CARTESIAN_POINT ( 'NONE',  ( 17.85438889637121918, 1451.055155745748152, 147.6149896967176289 ) ) ;
#61810 = CARTESIAN_POINT ( 'NONE',  ( -8.297448150139999257, 1384.938007610199747, 218.7034661405789961 ) ) ;
#61811 = CARTESIAN_POINT ( 'NONE',  ( 9.727603105489999180, 1462.797525513090022, 208.2922963384270361 ) ) ;
#61812 = EDGE_CURVE ( 'NONE', #28705, #28187, #17363, .T. ) ;
#61813 = CARTESIAN_POINT ( 'NONE',  ( -12.63540103640000112, 1379.206155667370012, 208.6368498725950076 ) ) ;
#61814 = CARTESIAN_POINT ( 'NONE',  ( -32.26928162443899595, 1379.633198882570241, 215.6001090146092167 ) ) ;
#61815 = CARTESIAN_POINT ( 'NONE',  ( 2.840552573029999639, 1464.907901564989970, 199.6779196415990043 ) ) ;
#61816 = CARTESIAN_POINT ( 'NONE',  ( 8.617688953975729760, 1437.241789755910077, 208.4440105384769879 ) ) ;
#61817 = ORIENTED_EDGE ( 'NONE', *, *, #8349, .F. ) ;
#61818 = CARTESIAN_POINT ( 'NONE',  ( -1.717432486395000124, 1516.836638729160086, 206.8395443540670158 ) ) ;
#61819 = ORIENTED_EDGE ( 'NONE', *, *, #44595, .F. ) ;
#61820 = CARTESIAN_POINT ( 'NONE',  ( 26.83521609794189899, 1440.913060387330006, 244.5852667276629973 ) ) ;
#61821 = CARTESIAN_POINT ( 'NONE',  ( -17.79309622859999962, 1508.782084903129999, 186.6536652249980079 ) ) ;
#61822 = ORIENTED_EDGE ( 'NONE', *, *, #95986, .T. ) ;
#61823 = CARTESIAN_POINT ( 'NONE',  ( 25.42631525001290171, 1450.800432264039955, 137.2067223160219953 ) ) ;
#61824 = CARTESIAN_POINT ( 'NONE',  ( -14.94386443490000005, 1409.601552534729990, 191.3531982347979863 ) ) ;
#61825 = CARTESIAN_POINT ( 'NONE',  ( -46.82073828382691971, 1379.680985121969115, 239.8219845903596195 ) ) ;
#61826 = B_SPLINE_CURVE_WITH_KNOTS ( 'NONE', 3,
 ( #60968, #64139, #95093, #18359, #44151, #98259, #78286, #1600, #35737, #104038 ),
 .UNSPECIFIED., .F., .F.,
 ( 4, 2, 2, 2, 4 ),
 ( 1.051150819890804081E-15, 0.0002615007907132596392, 0.0005230015814254681443, 0.0007845023721376766495, 0.001046003162849885263 ),
 .UNSPECIFIED. ) ;
#61827 = CARTESIAN_POINT ( 'NONE',  ( -24.38909170209999999, 1441.406328540210097, 211.3558879569780231 ) ) ;
#61828 = CARTESIAN_POINT ( 'NONE',  ( -10.79382126600000014, 1414.913060387329779, 196.1395803457980094 ) ) ;
#61829 = CARTESIAN_POINT ( 'NONE',  ( -11.75869035857540013, 1519.551704408389924, 190.9442076533970010 ) ) ;
#61830 = CARTESIAN_POINT ( 'NONE',  ( -13.01246536547306398, 1434.785318802752727, 146.9694555298348462 ) ) ;
#61831 = EDGE_CURVE ( 'NONE', #51540, #94625, #22265, .T. ) ;
#61832 = CARTESIAN_POINT ( 'NONE',  ( 16.67046851633390148, 1516.551188146170034, 222.1952932998519827 ) ) ;
#61833 = CARTESIAN_POINT ( 'NONE',  ( 22.68396052030000121, 1435.289475021379985, 139.2169948456979967 ) ) ;
#61835 = CARTESIAN_POINT ( 'NONE',  ( 5.172586535390000684, 1492.767659076290101, 188.8148697515989909 ) ) ;
#61834 = CARTESIAN_POINT ( 'NONE',  ( 15.73551128017709466, 1409.462558017715537, 192.7683535211936317 ) ) ;
#61836 = B_SPLINE_CURVE_WITH_KNOTS ( 'NONE', 5,
 ( #60101, #96449, #98633, #11892, #3515, #79112 ),
 .UNSPECIFIED., .F., .F.,
 ( 6, 6 ),
 ( -88.89713672530000110, -20.08879725519999226 ),
 .UNSPECIFIED. ) ;
#61837 = CARTESIAN_POINT ( 'NONE',  ( -1.706797824074999914, 1517.164987839469859, 214.9112406324369999 ) ) ;
#61838 = ADVANCED_FACE ( 'NONE', ( #80531 ), #23267, .T. ) ;
#61839 = DIRECTION ( 'NONE',  ( 0.000000000000000000, 0.000000000000000000, -1.000000000000000000 ) ) ;
#61840 = CARTESIAN_POINT ( 'NONE',  ( 5.495614718128320142, 1510.802068165409992, 216.7138213142690120 ) ) ;
#61841 = CARTESIAN_POINT ( 'NONE',  ( 30.61618914730548724, 1525.211473355384669, 221.5983863950426382 ) ) ;
#61842 = CARTESIAN_POINT ( 'NONE',  ( 4.042729802795000715, 1516.919782530640077, 212.3762473738369749 ) ) ;
#61843 = AXIS2_PLACEMENT_3D ( 'NONE', #100420, #108269, #65733 ) ;
#61844 = CARTESIAN_POINT ( 'NONE',  ( 4.329791490734999471, 1515.051704408389924, 212.4519801359869859 ) ) ;
#61845 = CARTESIAN_POINT ( 'NONE',  ( 30.57064947821818635, 1523.844789899200805, 221.8563555303887540 ) ) ;
#61847 = ORIENTED_EDGE ( 'NONE', *, *, #74879, .T. ) ;
#61846 = CARTESIAN_POINT ( 'NONE',  ( -86.93140579660001777, 1384.976593077780080, 307.7302223600589741 ) ) ;
#61848 = DIRECTION ( 'NONE',  ( 0.03489949670250328678, -0.9993908270190956511, 0.000000000000000000 ) ) ;
#61849 = CARTESIAN_POINT ( 'NONE',  ( 25.82475784490000237, 1456.303105448229871, 244.3435519335980075 ) ) ;
#61850 = CARTESIAN_POINT ( 'NONE',  ( -18.63536074199999959, 1457.257477148429871, 229.6471845788980204 ) ) ;
#61851 = DIRECTION ( 'NONE',  ( 0.3090169943749447312, 0.000000000000000000, -0.9510565162951544194 ) ) ;
#61852 = CARTESIAN_POINT ( 'NONE',  ( -7.949591086192760336, 1509.190922234509799, 237.3729886602710053 ) ) ;
#61853 = CARTESIAN_POINT ( 'NONE',  ( -21.13871847430000273, 1453.538022492230084, 224.2160773190980194 ) ) ;
#61855 = CARTESIAN_POINT ( 'NONE',  ( 17.49213541791160154, 1409.748594249720099, 222.5804550065900287 ) ) ;
#61854 = DIRECTION ( 'NONE',  ( -0.9235788661519466203, -0.3792384726311378018, -0.05639378400042227568 ) ) ;
#61856 = CARTESIAN_POINT ( 'NONE',  ( -0.08972462337150000078, 1506.809279316830043, 187.0844409784980371 ) ) ;
#61857 = CARTESIAN_POINT ( 'NONE',  ( -105.1077133852530068, 1379.453477749980038, 305.4638311486609723 ) ) ;
#61858 = EDGE_LOOP ( 'NONE', ( #60530, #75097, #58333, #4070 ) ) ;
#61859 = CARTESIAN_POINT ( 'NONE',  ( 0.7369041709050019318, 1517.080322339569875, 204.1102945640870132 ) ) ;
#61860 = FACE_OUTER_BOUND ( 'NONE', #9929, .T. ) ;
#61861 = CARTESIAN_POINT ( 'NONE',  ( 4.487249773072029768, 1509.038615930399828, 211.6097810847319920 ) ) ;
#61862 = EDGE_CURVE ( 'NONE', #101705, #73940, #109906, .T. ) ;
#61863 = CIRCLE ( 'NONE', #60089, 29.84605316702132072 ) ;
#61864 = CARTESIAN_POINT ( 'NONE',  ( 37.91363576014470027, 1455.431640273400035, 269.5661993588879568 ) ) ;
#61865 = CARTESIAN_POINT ( 'NONE',  ( 2.478856071480000089, 1433.873643567909994, 157.5618534805980175 ) ) ;
#61866 =( BOUNDED_CURVE ( )  B_SPLINE_CURVE ( 3, ( #57467, #31127, #22149, #56350 ),
 .UNSPECIFIED., .F., .T. ) 
 B_SPLINE_CURVE_WITH_KNOTS ( ( 4, 4 ),
 ( 4.993841937945130205, 5.632217541602730471 ),
 .UNSPECIFIED. ) 
 CURVE ( )  GEOMETRIC_REPRESENTATION_ITEM ( )  RATIONAL_B_SPLINE_CURVE ( ( 1.000000000000000000, 0.9663270635670118125, 0.9663270635670118125, 1.000000000000000000 ) ) 
 REPRESENTATION_ITEM ( '' )  );
#61867 = FACE_OUTER_BOUND ( 'NONE', #37942, .T. ) ;
#61868 = CARTESIAN_POINT ( 'NONE',  ( -45.00576737213309997, 1440.913060397780100, 265.4746514701479896 ) ) ;
#61869 = CARTESIAN_POINT ( 'NONE',  ( -26.72647157590000333, 1447.183840207770118, 137.1854294550980171 ) ) ;
#61870 = CARTESIAN_POINT ( 'NONE',  ( 1.842704255619313169, 1450.383521515580469, 154.3038121965128653 ) ) ;
#61871 = CARTESIAN_POINT ( 'NONE',  ( 1.799617396100000155, 1431.296477605490281, 200.2099161714889988 ) ) ;
#61872 = CARTESIAN_POINT ( 'NONE',  ( 10.15211825780419197, 1462.852281282112926, 213.4500083841329854 ) ) ;
#61873 = CARTESIAN_POINT ( 'NONE',  ( 2.444246758109999806, 1506.180962866889786, 221.2807778021990259 ) ) ;
#61874 = CARTESIAN_POINT ( 'NONE',  ( 17.53454537772509880, 1416.240002716455592, 192.2859374383096167 ) ) ;
#61875 = CIRCLE ( 'NONE', #42176, 2.000006063936102141 ) ;
#61876 = ORIENTED_EDGE ( 'NONE', *, *, #109015, .F. ) ;
#61877 = CARTESIAN_POINT ( 'NONE',  ( 3.686666017499999892, 1448.977420087960127, 184.1966211689980071 ) ) ;
#61878 = ADVANCED_FACE ( 'NONE', ( #32324 ), #824, .F. ) ;
#61879 = CARTESIAN_POINT ( 'NONE',  ( -0.4112623051359989845, 1484.199768852090074, 198.4089546266989998 ) ) ;
#61880 = CARTESIAN_POINT ( 'NONE',  ( 4.362527623401529553, 1466.289975156470064, 199.7053707134959950 ) ) ;
#61881 = CARTESIAN_POINT ( 'NONE',  ( -0.3391533370919999624, 1475.982599279930128, 267.2349199512980249 ) ) ;
#61882 = CARTESIAN_POINT ( 'NONE',  ( 5.172586535390000684, 1492.767659076290101, 188.8148697515989909 ) ) ;
#61883 = CARTESIAN_POINT ( 'NONE',  ( -33.42844755916929245, 1522.861859112238335, 196.1165140606796058 ) ) ;
#61884 = DIRECTION ( 'NONE',  ( -0.000000000000000000, -1.000000000000000000, -0.000000000000000000 ) ) ;
#61885 = CARTESIAN_POINT ( 'NONE',  ( -13.66835502576310013, 1384.880622718460017, 219.1890757919979933 ) ) ;
#61886 = B_SPLINE_CURVE_WITH_KNOTS ( 'NONE', 5,
 ( #82803, #13930, #23980, #39136, #73314, #74983 ),
 .UNSPECIFIED., .F., .F.,
 ( 6, 6 ),
 ( 0.000000000000000000, 1.000000000000000000 ),
 .UNSPECIFIED. ) ;
#61887 = CARTESIAN_POINT ( 'NONE',  ( -18.89315557560000158, 1416.535385209229844, 208.2130245880870234 ) ) ;
#61888 = CARTESIAN_POINT ( 'NONE',  ( -4.500000000000000000, 1439.615672362369878, 183.5288080717980108 ) ) ;
#61889 = CARTESIAN_POINT ( 'NONE',  ( 7.889086915934699462, 1512.111360402248920, 206.1534947800682289 ) ) ;
#61890 = CARTESIAN_POINT ( 'NONE',  ( -10.55660206177969940, 1396.281705055399925, 205.8010626438610018 ) ) ;
#61891 = EDGE_CURVE ( 'NONE', #103208, #62022, #103335, .T. ) ;
#61892 = CARTESIAN_POINT ( 'NONE',  ( -16.09626466356160179, 1409.475145151020115, 225.1332147237440040 ) ) ;
#61893 = CARTESIAN_POINT ( 'NONE',  ( 11.97724519069999971, 1441.600846913620217, 147.6096801420980000 ) ) ;
#61894 = VERTEX_POINT ( 'NONE', #40718 ) ;
#61895 = CARTESIAN_POINT ( 'NONE',  ( -20.59664500270120158, 1507.763472350329948, 190.3621299389660066 ) ) ;
#61896 = CARTESIAN_POINT ( 'NONE',  ( -15.85591190879999779, 1415.880081504350073, 209.4912631162540038 ) ) ;
#61897 = CARTESIAN_POINT ( 'NONE',  ( -0.1314159319799989845, 1442.749364073790048, 202.9452834803589951 ) ) ;
#61899 = CARTESIAN_POINT ( 'NONE',  ( -9.862207263486190811, 1438.620019707270103, 210.3541762680239913 ) ) ;
#61898 = CARTESIAN_POINT ( 'NONE',  ( 9.958422982289999226, 1425.240937812430047, 91.92796437169779722 ) ) ;
#61900 = CARTESIAN_POINT ( 'NONE',  ( 0.4156708952280039338, 1507.115992466239732, 180.9569215093680157 ) ) ;
#61901 = ADVANCED_FACE ( 'NONE', ( #32854 ), #34519, .F. ) ;
#61902 = CARTESIAN_POINT ( 'NONE',  ( -13.51610093808349333, 1442.913060377700731, 151.4871142704430440 ) ) ;
#61903 = CARTESIAN_POINT ( 'NONE',  ( -109.9718049258029993, 1384.472301579249915, 311.4373116341799914 ) ) ;
#61904 = CARTESIAN_POINT ( 'NONE',  ( 7.681541415779999937, 1425.833909046620192, 211.9025755004689984 ) ) ;
#61905 = CARTESIAN_POINT ( 'NONE',  ( 8.129467950829999623, 1461.711574958590063, 228.8738014342989970 ) ) ;
#61906 = FACE_BOUND ( 'NONE', #24290, .T. ) ;
#61907 = CARTESIAN_POINT ( 'NONE',  ( 7.891777486555000110, 1512.314860029340025, 206.1798163010270173 ) ) ;
#61908 = CARTESIAN_POINT ( 'NONE',  ( 3.895672787440000118, 1449.598608009080181, 184.2305619520979860 ) ) ;
#61909 = CARTESIAN_POINT ( 'NONE',  ( 9.925983360928359645, 1364.303202023261974, 210.6218459616987957 ) ) ;
#61911 = ORIENTED_EDGE ( 'NONE', *, *, #18926, .F. ) ;
#61910 = CARTESIAN_POINT ( 'NONE',  ( -7.139643295716398441, 1463.933016821221599, 236.1633024888363934 ) ) ;
#61912 = ORIENTED_EDGE ( 'NONE', *, *, #83503, .T. ) ;
#61913 = CIRCLE ( 'NONE', #90482, 7.146147325060000277 ) ;
#61914 = CARTESIAN_POINT ( 'NONE',  ( -41.49212309149999811, 1443.779876761469950, 136.5764441233980051 ) ) ;
#61915 = AXIS2_PLACEMENT_3D ( 'NONE', #25922, #76912, #16953 ) ;
#61916 = CARTESIAN_POINT ( 'NONE',  ( -14.82206140629999958, 1409.430658177129999, 192.2978730262979923 ) ) ;
#61917 = CARTESIAN_POINT ( 'NONE',  ( -3.081957766449999969, 1471.965628206130077, 270.0718125651980017 ) ) ;
#61918 = CARTESIAN_POINT ( 'NONE',  ( -7.784559239514999618, 1511.207707629420156, 213.1130077534970155 ) ) ;
#61919 = CARTESIAN_POINT ( 'NONE',  ( 0.1523726883269999888, 1486.225463480429880, 181.8688073209980018 ) ) ;
#61920 = CARTESIAN_POINT ( 'NONE',  ( -31.11295621078938467, 1525.790286462509584, 201.8987511033408566 ) ) ;
#61921 = EDGE_CURVE ( 'NONE', #43145, #29266, #59197, .T. ) ;
#61922 = CARTESIAN_POINT ( 'NONE',  ( -2.641120632158299841, 1464.700422726399893, 198.8576235399000041 ) ) ;
#61923 = CARTESIAN_POINT ( 'NONE',  ( -35.92258139975950115, 1450.175254039669881, 136.2201275893520176 ) ) ;
#61924 = CARTESIAN_POINT ( 'NONE',  ( -2.500000000000059952, 1448.813856349769821, 156.5098158667020130 ) ) ;
#61925 = CARTESIAN_POINT ( 'NONE',  ( 5.795460316590049565, 1396.115442321129876, 218.5178396626099868 ) ) ;
#61926 = CARTESIAN_POINT ( 'NONE',  ( 3.536371054309000339, 1409.036553185790126, 194.1218458967759943 ) ) ;
#61927 = CARTESIAN_POINT ( 'NONE',  ( -1.507529438030280167, 1406.789552898120064, 269.6496621541520540 ) ) ;
#61928 = ADVANCED_FACE ( 'NONE', ( #17127 ), #57547, .F. ) ;
#61929 = CARTESIAN_POINT ( 'NONE',  ( -14.45919768630980151, 1435.871793938970086, 149.8088992138540050 ) ) ;
#61930 = ORIENTED_EDGE ( 'NONE', *, *, #19397, .F. ) ;
#61931 = DIRECTION ( 'NONE',  ( 0.4428464831282420966, -0.8932998904726507927, -0.07682641513501356489 ) ) ;
#61932 = CARTESIAN_POINT ( 'NONE',  ( 12.51650399660000090, 1442.246764597770152, 188.0677751049979918 ) ) ;
#61933 = ORIENTED_EDGE ( 'NONE', *, *, #48738, .F. ) ;
#61934 = ORIENTED_EDGE ( 'NONE', *, *, #1613, .F. ) ;
#61935 = EDGE_CURVE ( 'NONE', #11723, #35481, #36619, .T. ) ;
#61936 = CARTESIAN_POINT ( 'NONE',  ( -4.267145199109999787, 1453.908306484889863, 199.9833665867990078 ) ) ;
#61937 = CARTESIAN_POINT ( 'NONE',  ( -10.02185219039999886, 1364.916310432309956, 207.6218459616989946 ) ) ;
#61938 = CARTESIAN_POINT ( 'NONE',  ( -5.000083865865000199, 1516.858456333729919, 214.1306941701269864 ) ) ;
#61939 = CARTESIAN_POINT ( 'NONE',  ( 4.427981723884999887, 1510.423579818969984, 216.6708627338570068 ) ) ;
#61940 = EDGE_CURVE ( 'NONE', #60010, #23487, #22723, .T. ) ;
#61941 = AXIS2_PLACEMENT_3D ( 'NONE', #16452, #83686, #34395 ) ;
#61942 = ORIENTED_EDGE ( 'NONE', *, *, #86062, .F. ) ;
#61943 = CARTESIAN_POINT ( 'NONE',  ( 15.66449074470000014, 1427.615315534789943, 199.7467549911789888 ) ) ;
#61944 = CARTESIAN_POINT ( 'NONE',  ( -85.54616801939999959, 1378.671092583530026, 296.2627734746589567 ) ) ;
#61945 = CARTESIAN_POINT ( 'NONE',  ( -105.7942887633819993, 1378.913060387289988, 304.0474587704230203 ) ) ;
#61946 = CARTESIAN_POINT ( 'NONE',  ( 7.713117802984999827, 1516.690345681169902, 204.1174038931170003 ) ) ;
#61947 = B_SPLINE_CURVE_WITH_KNOTS ( 'NONE', 4,
 ( #101698, #24989, #65392, #56985, #99497, #7658, #40163, #7116, #22779 ),
 .UNSPECIFIED., .F., .F.,
 ( 5, 4, 5 ),
 ( 0.000000000000000000, 0.9999685429682046989, 1.000000000000000000 ),
 .UNSPECIFIED. ) ;
#61948 = CARTESIAN_POINT ( 'NONE',  ( -28.02005516190000023, 1440.913060387330006, 248.0989693021979861 ) ) ;
#61949 = CARTESIAN_POINT ( 'NONE',  ( -103.7379679780000004, 1385.000870667160143, 296.9192581611590072 ) ) ;
#61950 = CARTESIAN_POINT ( 'NONE',  ( 9.481395134947719683, 1462.257910684749959, 206.9075228777909956 ) ) ;
#61951 = CARTESIAN_POINT ( 'NONE',  ( -5.824582710369999639, 1409.283474491729976, 230.9652227488979861 ) ) ;
#61953 = EDGE_LOOP ( 'NONE', ( #73261, #9966 ) ) ;
#61952 = CARTESIAN_POINT ( 'NONE',  ( -1.655764672069989230, 1452.024870244869135, 184.0828371579059137 ) ) ;
#61954 = EDGE_CURVE ( 'NONE', #37990, #43895, #27668, .T. ) ;
#61955 = DIRECTION ( 'NONE',  ( -0.02616798426500960631, 0.9993150019883682011, 0.02616798426500950570 ) ) ;
#61956 = CARTESIAN_POINT ( 'NONE',  ( -25.37446848917170072, 1440.913060497199922, 218.3462857971420021 ) ) ;
#61957 = CARTESIAN_POINT ( 'NONE',  ( -13.37005892530000040, 1384.196513454120122, 218.9076047076389955 ) ) ;
#61958 = CARTESIAN_POINT ( 'NONE',  ( -22.08622291482368638, 1523.382868172864164, 184.4183880513178337 ) ) ;
#61959 = CARTESIAN_POINT ( 'NONE',  ( -25.17810084989999808, 1436.605446963749955, 137.6240872485979878 ) ) ;
#61960 = ADVANCED_FACE ( 'NONE', ( #26098, #86025 ), #77633, .T. ) ;
#61961 = CARTESIAN_POINT ( 'NONE',  ( -4.608417544644999531, 1516.691389976299888, 211.6120918846570191 ) ) ;
#61962 = CARTESIAN_POINT ( 'NONE',  ( -67.68830324459999304, 1379.745299480660151, 277.8290332001590173 ) ) ;
#61963 = CARTESIAN_POINT ( 'NONE',  ( 0.01162473798205385794, 1508.119767624307997, 237.6719974036047347 ) ) ;
#61964 = CARTESIAN_POINT ( 'NONE',  ( -8.557209110492459914, 1448.617779613390212, 212.3361752075699940 ) ) ;
#61965 = CARTESIAN_POINT ( 'NONE',  ( -13.67844609351699958, 1504.250379464319849, 227.6838296026270143 ) ) ;
#61966 = CARTESIAN_POINT ( 'NONE',  ( 1.709766494024999917, 1516.959716008189844, 209.1091877442879934 ) ) ;
#61967 = ORIENTED_EDGE ( 'NONE', *, *, #64427, .T. ) ;
#61968 = DIRECTION ( 'NONE',  ( 9.230617842401318720E-47, -1.000000000000000000, 1.836970198721029688E-16 ) ) ;
#61969 = CARTESIAN_POINT ( 'NONE',  ( -13.88578263259999979, 1410.294695765230017, 227.0726749396980040 ) ) ;
#61970 = CARTESIAN_POINT ( 'NONE',  ( -36.11306192460000375, 1385.070985855290019, 235.4717389730590185 ) ) ;
#61971 = ORIENTED_EDGE ( 'NONE', *, *, #98052, .T. ) ;
#61972 = DIRECTION ( 'NONE',  ( 0.7382608262429739554, 0.6622882068469760908, -0.1278486742459950254 ) ) ;
#61973 = PLANE ( 'NONE',  #88910 ) ;
#61974 = CARTESIAN_POINT ( 'NONE',  ( 16.80235653624059822, 1469.007454033449903, 229.3029007443279852 ) ) ;
#61975 = CARTESIAN_POINT ( 'NONE',  ( -24.02854486914899823, 1507.902871221900114, 222.3115732752750091 ) ) ;
#61976 = DIRECTION ( 'NONE',  ( 1.755985294532464991E-16, -1.000000000000000000, 1.338183447452830017E-16 ) ) ;
#61977 = CARTESIAN_POINT ( 'NONE',  ( 10.73803961559999998, 1423.675746264540066, 203.2436441965290044 ) ) ;
#61978 = CARTESIAN_POINT ( 'NONE',  ( 0.1132867808292180034, 1420.456998724389905, 182.7041194852360206 ) ) ;
#61980 = CARTESIAN_POINT ( 'NONE',  ( -3.540703860449999851, 1421.447957905329986, 185.5466525330979835 ) ) ;
#61979 = CARTESIAN_POINT ( 'NONE',  ( 4.037378256055000669, 1516.688761843659904, 215.6706679112870120 ) ) ;
#61981 = CARTESIAN_POINT ( 'NONE',  ( -5.930127944598639900, 1391.913057044489960, 215.1135602292339968 ) ) ;
#61982 = CARTESIAN_POINT ( 'NONE',  ( 10.73061977934889910, 1470.167071072400176, 207.1537691930359983 ) ) ;
#61983 = ORIENTED_EDGE ( 'NONE', *, *, #37814, .T. ) ;
#61984 = CARTESIAN_POINT ( 'NONE',  ( -11.16128041099520019, 1414.913057846380070, 196.7202417048659981 ) ) ;
#61985 = CARTESIAN_POINT ( 'NONE',  ( 9.018659374699888431, 1423.185120360550172, 211.3902366515449955 ) ) ;
#61986 = CARTESIAN_POINT ( 'NONE',  ( -18.97665094185341772, 1526.382868172863937, 185.2759924068388671 ) ) ;
#61987 = ORIENTED_EDGE ( 'NONE', *, *, #23436, .F. ) ;
#61988 = CARTESIAN_POINT ( 'NONE',  ( 2.046266125239999845, 1417.477797419130184, 235.2693601201980016 ) ) ;
#61989 = CARTESIAN_POINT ( 'NONE',  ( 9.152846453431976670, 1436.773426841208902, 153.0359782892105329 ) ) ;
#61990 = CARTESIAN_POINT ( 'NONE',  ( 7.936754916012690231, 1511.432897564909808, 203.2990511617569780 ) ) ;
#61991 = CARTESIAN_POINT ( 'NONE',  ( 3.015233801489999976, 1443.190137595490114, 217.5000105274690156 ) ) ;
#61992 = CARTESIAN_POINT ( 'NONE',  ( -31.74003925670054116, 1524.382868172804365, 201.6871716353068678 ) ) ;
#61993 = CARTESIAN_POINT ( 'NONE',  ( -3.171072485709999889, 1451.871858332230204, 182.7750508701979868 ) ) ;
#61994 = CARTESIAN_POINT ( 'NONE',  ( 18.47106347599999765, 1415.579607678529783, 210.5150304694180079 ) ) ;
#61995 = CARTESIAN_POINT ( 'NONE',  ( -18.26759032049999831, 1425.063529675129985, 226.1973866133980096 ) ) ;
#61996 = CARTESIAN_POINT ( 'NONE',  ( -22.66323514130000305, 1435.715412731579818, 141.6350653710979941 ) ) ;
#61997 = DIRECTION ( 'NONE',  ( -5.980589973904019347E-17, 1.000000000000000000, -1.736889445713099699E-16 ) ) ;
#61999 = CARTESIAN_POINT ( 'NONE',  ( -4.993938974811324094, 1391.677352696793832, 203.5345363725389802 ) ) ;
#61998 = CARTESIAN_POINT ( 'NONE',  ( 0.4536707880366389611, 1408.928902979399936, 232.1183505920600112 ) ) ;
#62000 = DIRECTION ( 'NONE',  ( -0.7063774289747313251, 0.04540766091858271930, -0.7063774289747313251 ) ) ;
#62001 = ORIENTED_EDGE ( 'NONE', *, *, #98919, .F. ) ;
#62002 = CARTESIAN_POINT ( 'NONE',  ( 1.555417156611949903, 1415.301705643749983, 191.0707738022140063 ) ) ;
#62003 = DIRECTION ( 'NONE',  ( -0.8672669759446630655, 0.000000000000000000, 0.4978433412588735285 ) ) ;
#62004 = CARTESIAN_POINT ( 'NONE',  ( -24.07234762469999723, 1436.256975754479981, 211.0558319517779751 ) ) ;
#62005 = CARTESIAN_POINT ( 'NONE',  ( -4.450958129710000044, 1483.189406595490027, 199.4355188422489960 ) ) ;
#62006 = CARTESIAN_POINT ( 'NONE',  ( -21.62164173379369814, 1519.551704408389924, 210.2163513719069954 ) ) ;
#62007 = CARTESIAN_POINT ( 'NONE',  ( -3.498438759191051073, 1426.007621855026855, 185.8749847655367091 ) ) ;
#62008 = CARTESIAN_POINT ( 'NONE',  ( -19.57175081134495187, 1452.229599788696760, 144.4156370990241669 ) ) ;
#62009 = DIRECTION ( 'NONE',  ( 0.9858563016923833633, 0.000000000000000000, 0.1675928173085483863 ) ) ;
#62011 = CIRCLE ( 'NONE', #67364, 1.999999999999999556 ) ;
#62010 = CARTESIAN_POINT ( 'NONE',  ( -6.080444312649149197, 1488.995743380849945, 218.2866348719960001 ) ) ;
#62012 = CARTESIAN_POINT ( 'NONE',  ( 18.68389199464829886, 1457.534885685930021, 220.6832065729649912 ) ) ;
#62013 = CARTESIAN_POINT ( 'NONE',  ( -92.10450461559780422, 1383.768992061189920, 309.1587668656890173 ) ) ;
#62014 = CARTESIAN_POINT ( 'NONE',  ( -109.6411560373970104, 1384.508416019190008, 311.3033268927259769 ) ) ;
#62015 = CARTESIAN_POINT ( 'NONE',  ( -5.045364366626095887, 1391.811351688237664, 214.6675329302748594 ) ) ;
#62016 = CARTESIAN_POINT ( 'NONE',  ( -1.730531345579879865, 1516.544444245470004, 201.4125486926729991 ) ) ;
#62018 = ORIENTED_EDGE ( 'NONE', *, *, #78146, .F. ) ;
#62017 = CARTESIAN_POINT ( 'NONE',  ( 25.78167512749999801, 1509.813387183829946, 195.1140785605980170 ) ) ;
#62019 = DIRECTION ( 'NONE',  ( -0.5877852522924585932, 0.000000000000000000, 0.8090169943749579984 ) ) ;
#62020 = CARTESIAN_POINT ( 'NONE',  ( -90.19765245659999664, 1379.339186696669913, 300.1519328718590032 ) ) ;
#62021 = CARTESIAN_POINT ( 'NONE',  ( 19.91241810695860082, 1508.791614727160095, 229.5527701831059915 ) ) ;
#62022 = VERTEX_POINT ( 'NONE', #44593 ) ;
#62023 = ORIENTED_EDGE ( 'NONE', *, *, #54807, .F. ) ;
#62024 = CARTESIAN_POINT ( 'NONE',  ( -20.69303424980000372, 1486.764600954290017, 209.1218459616989946 ) ) ;
#62025 = B_SPLINE_CURVE_WITH_KNOTS ( 'NONE', 5,
 ( #88331, #11624, #31714, #75402, #48545, #100017, #100570, #23851, #15451 ),
 .UNSPECIFIED., .F., .F.,
 ( 6, 3, 6 ),
 ( 0.000000000000000000, 0.5459884364902550802, 1.000000000000000000 ),
 .UNSPECIFIED. ) ;
#62026 = CARTESIAN_POINT ( 'NONE',  ( 18.03151512659999867, 1424.669534113930013, 225.2917716953979834 ) ) ;
#62027 = CARTESIAN_POINT ( 'NONE',  ( -29.79881796581627640, 1526.748660780343698, 196.6633055964660457 ) ) ;
#62029 = CARTESIAN_POINT ( 'NONE',  ( -14.25478685789999922, 1474.931945797630078, 267.1909358522980256 ) ) ;
#62028 = CARTESIAN_POINT ( 'NONE',  ( 18.95069757339999938, 1434.818091166489921, 209.1678375094830074 ) ) ;
#62030 = CARTESIAN_POINT ( 'NONE',  ( -5.445054425793269814, 1494.866999379700246, 198.0707246423999948 ) ) ;
#62031 = CARTESIAN_POINT ( 'NONE',  ( -11.13407163250000131, 1433.980143678790000, 151.6624242815980210 ) ) ;
#62032 = CARTESIAN_POINT ( 'NONE',  ( 24.02854436560000195, 1507.902905841229767, 195.9321017799980211 ) ) ;
#62033 = CARTESIAN_POINT ( 'NONE',  ( -1.000362776118160035E-16, 1517.151704408390060, 209.1218459616989946 ) ) ;
#62034 = CARTESIAN_POINT ( 'NONE',  ( 6.015966285260000213, 1410.497582365630024, 186.7561560874980273 ) ) ;
#62035 = CARTESIAN_POINT ( 'NONE',  ( 5.243795696529999439, 1423.891122896129900, 185.6630549162979946 ) ) ;
#62036 = CARTESIAN_POINT ( 'NONE',  ( -10.37614202680000020, 1435.190620644159935, 152.2457775527979891 ) ) ;
#62037 = CARTESIAN_POINT ( 'NONE',  ( 8.766760964599999539, 1437.289887157169915, 153.2969297041979928 ) ) ;
#62038 = CARTESIAN_POINT ( 'NONE',  ( -14.29542475900360010, 1421.697851824200143, 203.6378746937919857 ) ) ;
#62039 = CARTESIAN_POINT ( 'NONE',  ( 3.141370515551505260, 1525.159196711359755, 241.5359652250428155 ) ) ;
#62040 = CARTESIAN_POINT ( 'NONE',  ( 2.484906683780000236, 1472.794382616990106, 219.0213525527389891 ) ) ;
#62041 = ORIENTED_EDGE ( 'NONE', *, *, #22062, .T. ) ;
#62042 = CARTESIAN_POINT ( 'NONE',  ( 1.861700016370000164E-09, 1407.650947845630071, 270.1377426662980383 ) ) ;
#62043 = CARTESIAN_POINT ( 'NONE',  ( -17.81193786781770427, 1488.806627658329944, 195.1587721144809962 ) ) ;
#62044 = CARTESIAN_POINT ( 'NONE',  ( -42.86216812819999689, 1450.287397759410169, 270.1125555652979529 ) ) ;
#62045 = CARTESIAN_POINT ( 'NONE',  ( 9.539810668950000405, 1420.903745483679813, 197.1733355697989793 ) ) ;
#62046 = CARTESIAN_POINT ( 'NONE',  ( 6.620521211799999861, 1440.451554611820029, 154.8188655977980090 ) ) ;
#62047 = CARTESIAN_POINT ( 'NONE',  ( -17.17241001986523941, 1512.187213306747481, 179.6185504016045797 ) ) ;
#62048 = EDGE_CURVE ( 'NONE', #80209, #51888, #53558, .T. ) ;
#62049 = CARTESIAN_POINT ( 'NONE',  ( -110.0629084955440078, 1384.909053975289908, 296.9513011978259556 ) ) ;
#62050 = EDGE_CURVE ( 'NONE', #65298, #51033, #69250, .T. ) ;
#62051 = CARTESIAN_POINT ( 'NONE',  ( 2.927258396572999910, 1410.119448063770278, 231.5909967517320069 ) ) ;
#62052 = CARTESIAN_POINT ( 'NONE',  ( 1.862958190160000083, 1508.877376266829970, 238.0546627234980122 ) ) ;
#62053 = CARTESIAN_POINT ( 'NONE',  ( -7.934490975959999304, 1418.851980705729829, 233.0693007919979891 ) ) ;
#62054 = CARTESIAN_POINT ( 'NONE',  ( -6.496128480939999505, 1458.243874865590215, 216.1639725907290028 ) ) ;
#62055 = CARTESIAN_POINT ( 'NONE',  ( 10.46820095950955398, 1363.150210183547188, 207.6218459616987673 ) ) ;
#62056 = CARTESIAN_POINT ( 'NONE',  ( -43.43515788656559806, 1430.093275174819837, 266.2527815779079674 ) ) ;
#62057 = CARTESIAN_POINT ( 'NONE',  ( -2.500000000000000000, 1428.666845053830002, 184.0221679455979995 ) ) ;
#62058 = ORIENTED_EDGE ( 'NONE', *, *, #107746, .F. ) ;
#62059 = CARTESIAN_POINT ( 'NONE',  ( 26.41103520988268016, 1435.419834908374014, 135.2945580757277639 ) ) ;
#62060 = ORIENTED_EDGE ( 'NONE', *, *, #35246, .T. ) ;
#62061 = CARTESIAN_POINT ( 'NONE',  ( -2.477975353594999763, 1516.839862955080207, 210.2583935552169976 ) ) ;
#62062 = DIRECTION ( 'NONE',  ( -1.000000000000000000, 0.000000000000000000, 0.000000000000000000 ) ) ;
#62063 = CARTESIAN_POINT ( 'NONE',  ( 17.60627508980000044, 1410.895669370830092, 224.8086596393980017 ) ) ;
#62064 = CARTESIAN_POINT ( 'NONE',  ( -14.07411318249999965, 1410.402452814530079, 190.2626066483979912 ) ) ;
#62065 = CIRCLE ( 'NONE', #92380, 2.000000000000072387 ) ;
#62066 = EDGE_CURVE ( 'NONE', #82950, #73589, #41969, .T. ) ;
#62067 = CARTESIAN_POINT ( 'NONE',  ( 2.236830499208590339, 1495.676457082710158, 221.2569898128769807 ) ) ;
#62068 = ORIENTED_EDGE ( 'NONE', *, *, #93114, .F. ) ;
#62069 = CARTESIAN_POINT ( 'NONE',  ( -14.47990272989999916, 1470.812340170329890, 194.5754142818979915 ) ) ;
#62071 = CARTESIAN_POINT ( 'NONE',  ( 19.63722818192610120, 1517.151704408390060, 218.2362632616380154 ) ) ;
#62070 = CARTESIAN_POINT ( 'NONE',  ( 0.3483522942510000053, 1452.334144580529937, 183.2984807459980061 ) ) ;
#62072 = CARTESIAN_POINT ( 'NONE',  ( -11.52804851922353890, 1414.677402202029953, 206.9304647618809270 ) ) ;
#62073 = CARTESIAN_POINT ( 'NONE',  ( -17.76510163610419823, 1508.542006963650238, 211.8150015411889910 ) ) ;
#62074 = CARTESIAN_POINT ( 'NONE',  ( 7.881803347790000025, 1471.528388462790190, 215.6156897165890030 ) ) ;
#62075 = CARTESIAN_POINT ( 'NONE',  ( -9.522384955721390654, 1439.330048506679987, 208.4251047430030042 ) ) ;
#62076 = ORIENTED_EDGE ( 'NONE', *, *, #40652, .T. ) ;
#62077 = CARTESIAN_POINT ( 'NONE',  ( -8.584304488529250321, 1409.159098409799981, 270.4209911071269516 ) ) ;
#62078 = CARTESIAN_POINT ( 'NONE',  ( 7.710966977635000497, 1516.608208975040043, 207.9930883710269711 ) ) ;
#62079 = CARTESIAN_POINT ( 'NONE',  ( -1.525139958810000085, 1427.692446166030095, 112.4493539157979995 ) ) ;
#62080 = CARTESIAN_POINT ( 'NONE',  ( 8.505169765932141246, 1436.416344830570097, 207.7641285517320000 ) ) ;
#62082 = ORIENTED_EDGE ( 'NONE', *, *, #28769, .F. ) ;
#62081 = CARTESIAN_POINT ( 'NONE',  ( -6.838394287845894759, 1365.988278472367028, 209.6218459617148824 ) ) ;
#62083 = EDGE_LOOP ( 'NONE', ( #35637, #26883, #22360, #46926 ) ) ;
#62084 = CARTESIAN_POINT ( 'NONE',  ( 44.97774548475524625, 1446.717870710880106, 268.9931714851094284 ) ) ;
#62085 = CARTESIAN_POINT ( 'NONE',  ( 8.710714953028380947, 1511.457792576163911, 203.5654966221206905 ) ) ;
#62086 = CARTESIAN_POINT ( 'NONE',  ( 3.632694880006927640, 1424.801563358291560, 184.7977647149654956 ) ) ;
#62087 = CARTESIAN_POINT ( 'NONE',  ( -0.01853033842224269950, 1408.987905777800052, 186.0079448517529954 ) ) ;
#62088 = CIRCLE ( 'NONE', #22695, 1.000004583512053902 ) ;
#62089 = EDGE_CURVE ( 'NONE', #27091, #60488, #49102, .T. ) ;
#62090 = CARTESIAN_POINT ( 'NONE',  ( -18.43253908699789889, 1415.651572961160127, 207.5692543878770095 ) ) ;
#62091 = CARTESIAN_POINT ( 'NONE',  ( -17.50642310480000319, 1415.863568519329874, 225.9737455361980096 ) ) ;
#62092 = CARTESIAN_POINT ( 'NONE',  ( 22.25458370657720053, 1471.079518017990040, 269.4963396272059981 ) ) ;
#62093 = CARTESIAN_POINT ( 'NONE',  ( -4.778891795048164859, 1466.453819146259320, 234.5096049691970848 ) ) ;
#62094 = CARTESIAN_POINT ( 'NONE',  ( 5.861641773170000569, 1445.997555159400008, 183.2089869270980103 ) ) ;
#62095 = CARTESIAN_POINT ( 'NONE',  ( 7.708770007014999592, 1516.524310051880093, 206.8307984429870032 ) ) ;
#62096 = EDGE_CURVE ( 'NONE', #10122, #92390, #9753, .T. ) ;
#62097 = VERTEX_POINT ( 'NONE', #52449 ) ;
#62098 = CARTESIAN_POINT ( 'NONE',  ( 23.33541660002344287, 1411.088284388518787, 212.4521946157103116 ) ) ;
#62099 = CARTESIAN_POINT ( 'NONE',  ( 1.508487166569379978, 1461.824335589909879, 183.0899350828030094 ) ) ;
#62100 = ORIENTED_EDGE ( 'NONE', *, *, #44245, .F. ) ;
#62101 = FACE_OUTER_BOUND ( 'NONE', #39478, .T. ) ;
#62102 = CARTESIAN_POINT ( 'NONE',  ( 25.61519007770650092, 1452.018576294739887, 135.1698835824450100 ) ) ;
#62103 = CARTESIAN_POINT ( 'NONE',  ( -22.74352257909999864, 1409.874439094229956, 210.5210124972680035 ) ) ;
#62104 = CARTESIAN_POINT ( 'NONE',  ( -19.18216750550000071, 1385.279599344249846, 220.5028985859590023 ) ) ;
#62105 = CARTESIAN_POINT ( 'NONE',  ( -18.70459388414779767, 1509.566239243649989, 231.7064163625079800 ) ) ;
#62106 = CARTESIAN_POINT ( 'NONE',  ( 16.87335319769999842, 1409.502290865030091, 193.5015210144979960 ) ) ;
#62107 = CARTESIAN_POINT ( 'NONE',  ( -3.750390061399999642, 1495.937738748590164, 198.1516812963990049 ) ) ;
#62108 = CARTESIAN_POINT ( 'NONE',  ( 16.63506069319999980, 1409.493969507229849, 224.8086549762979871 ) ) ;
#62110 = CARTESIAN_POINT ( 'NONE',  ( -18.86156570322403780, 1424.747429002025456, 224.4550601468019977 ) ) ;
#62109 = CARTESIAN_POINT ( 'NONE',  ( 0.7618663611100000566, 1416.510331848630130, 233.5782494407980039 ) ) ;
#62111 = CARTESIAN_POINT ( 'NONE',  ( 0.3569283261391170137, 1452.331401915339939, 183.2344466057309944 ) ) ;
#62112 = CIRCLE ( 'NONE', #26330, 30.65926195008838562 ) ;
#62113 = CARTESIAN_POINT ( 'NONE',  ( -10.04451165320000072, 1380.536316001939895, 216.6372458847690154 ) ) ;
#62114 = CARTESIAN_POINT ( 'NONE',  ( 3.265407117845000151, 1516.754149861460064, 213.7315192116670062 ) ) ;
#62115 = CARTESIAN_POINT ( 'NONE',  ( 2.444993193446221014, 1524.972383263452912, 242.2724965207514174 ) ) ;
#62116 = ORIENTED_EDGE ( 'NONE', *, *, #77606, .T. ) ;
#62117 = CARTESIAN_POINT ( 'NONE',  ( -18.55121668013607206, 1466.210258097253245, 216.5807023832959999 ) ) ;
#62118 = CARTESIAN_POINT ( 'NONE',  ( 21.41758936356528054, 1524.330813522192102, 234.0369194964263784 ) ) ;
#62119 = CARTESIAN_POINT ( 'NONE',  ( -0.5052195027655379533, 1409.815383004930027, 233.0624941665790004 ) ) ;
#62120 = CARTESIAN_POINT ( 'NONE',  ( 8535.261851439174279, 2833.596074015790236, 11230.49242346789651 ) ) ;
#62121 = CARTESIAN_POINT ( 'NONE',  ( -39.75209972814790405, 1446.403744002959911, 136.7362441017349965 ) ) ;
#62122 = CARTESIAN_POINT ( 'NONE',  ( -4.327218846663630103, 1515.149950449780135, 208.7360365624930125 ) ) ;
#62123 = CARTESIAN_POINT ( 'NONE',  ( -23.42675388609999843, 1443.575607731430182, 234.3916895697979612 ) ) ;
#62124 = FACE_OUTER_BOUND ( 'NONE', #107846, .T. ) ;
#62125 = CARTESIAN_POINT ( 'NONE',  ( 11.85885706300000031, 1433.132861810290024, 150.3130965059980042 ) ) ;
#62126 = CARTESIAN_POINT ( 'NONE',  ( -1.842963219480119985, 1515.064792700640055, 204.7923971808919816 ) ) ;
#62127 = CARTESIAN_POINT ( 'NONE',  ( 27.24318804543259986, 1440.913060389329758, 227.9385435188879683 ) ) ;
#62128 = CARTESIAN_POINT ( 'NONE',  ( -109.5279943120000041, 1385.221486439480032, 297.1347434786590043 ) ) ;
#62129 = CARTESIAN_POINT ( 'NONE',  ( 3.026717173399090299, 1424.965164304149994, 188.8885481931689867 ) ) ;
#62130 = ORIENTED_EDGE ( 'NONE', *, *, #68063, .T. ) ;
#62131 = B_SPLINE_CURVE_WITH_KNOTS ( 'NONE', 3,
 ( #76850, #68463, #15793, #24213, #103124, #43251, #58400, #84129, #101464, #92524, #9624, #16353, #49994, #51100 ),
 .UNSPECIFIED., .F., .F.,
 ( 4, 2, 2, 1, 2, 2, 1, 4 ),
 ( 0.000000000000000000, 0.3416613661786893630, 0.4270767077233605380, 0.4697843784956968749, 0.4911382138818642384, 0.5018151315749493913, 0.5124920492680344886, 0.6833227323573606293 ),
 .UNSPECIFIED. ) ;
#62132 = DIRECTION ( 'NONE',  ( 0.000000000000000000, -0.02617694830808806397, 0.9996573249755517088 ) ) ;
#62133 = CARTESIAN_POINT ( 'NONE',  ( 9.677599926597229896, 1463.237891885529962, 210.5383111002819874 ) ) ;
#62134 = AXIS2_PLACEMENT_3D ( 'NONE', #101042, #102151, #60183 ) ;
#62135 = CARTESIAN_POINT ( 'NONE',  ( -13.52118962660000001, 1485.980279578529917, 185.5139189508979882 ) ) ;
#62136 = CARTESIAN_POINT ( 'NONE',  ( -1.532299087870000021, 1444.082491599790046, 199.5897746526189849 ) ) ;
#62137 = CARTESIAN_POINT ( 'NONE',  ( 2.139180587729999861, 1474.716718025229966, 234.7298911498980090 ) ) ;
#62138 = CARTESIAN_POINT ( 'NONE',  ( 25.05872055529999898, 1449.799157988799834, 212.4667254601980062 ) ) ;
#62139 = CARTESIAN_POINT ( 'NONE',  ( -16.48256533165833204, 1420.110686815605959, 208.7021220505580743 ) ) ;
#62140 = CARTESIAN_POINT ( 'NONE',  ( -15.66010638180000214, 1508.960088055129972, 231.8745902587980083 ) ) ;
#62141 = CARTESIAN_POINT ( 'NONE',  ( -32.29029968710140253, 1383.839140599110124, 230.3723284232519859 ) ) ;
#62142 = CARTESIAN_POINT ( 'NONE',  ( -3.865363954398979729, 1508.610338847399817, 204.7110934479420052 ) ) ;
#62143 = CARTESIAN_POINT ( 'NONE',  ( -9.803834995107230554, 1517.051704408389924, 196.6215198571080123 ) ) ;
#62144 = CARTESIAN_POINT ( 'NONE',  ( -25.11187825681734509, 1509.789986500208670, 193.4229894714747218 ) ) ;
#62145 = CARTESIAN_POINT ( 'NONE',  ( 0.1608976399961470072, 1485.726857135249929, 181.8483459938640010 ) ) ;
#62147 = ORIENTED_EDGE ( 'NONE', *, *, #95973, .T. ) ;
#62146 = CARTESIAN_POINT ( 'NONE',  ( 3.814972826460000022, 1441.101450695089852, 217.8538525646389985 ) ) ;
#62148 = CARTESIAN_POINT ( 'NONE',  ( -1.342027840399999894, 1416.827520120730014, 228.0802440864979985 ) ) ;
#62149 = CARTESIAN_POINT ( 'NONE',  ( -10.04827894765687724, 1389.656101278125107, 201.8970266557225557 ) ) ;
#62150 = CARTESIAN_POINT ( 'NONE',  ( -3.951758682210000817, 1475.564030158489913, 199.4458604787490117 ) ) ;
#62152 = ORIENTED_EDGE ( 'NONE', *, *, #89173, .T. ) ;
#62151 = CARTESIAN_POINT ( 'NONE',  ( -32.48417584039620465, 1524.659802833171170, 217.0704217325891250 ) ) ;
#62153 = CARTESIAN_POINT ( 'NONE',  ( -6.305951052519140454, 1508.551704408389924, 219.3648472223130170 ) ) ;
#62154 = EDGE_LOOP ( 'NONE', ( #107953, #37236, #65792, #57608 ) ) ;
#62155 = CARTESIAN_POINT ( 'NONE',  ( -15.55634920516500053, 1516.551704408390151, 224.6781951372670108 ) ) ;
#62156 = CARTESIAN_POINT ( 'NONE',  ( -16.96258621739999839, 1415.088016306429836, 209.3926059833199815 ) ) ;
#62157 = CARTESIAN_POINT ( 'NONE',  ( -2.706144844479429157, 1509.031773379787637, 238.5943737788366548 ) ) ;
#62158 = CARTESIAN_POINT ( 'NONE',  ( 18.61829529775840086, 1507.564341563429934, 227.6679763394169811 ) ) ;
#62159 = CARTESIAN_POINT ( 'NONE',  ( -3.220674682859999916, 1433.265634983390100, 218.1214075930489855 ) ) ;
#62160 = CARTESIAN_POINT ( 'NONE',  ( -10.72965402270880020, 1471.641146218699987, 206.8906404078279877 ) ) ;
#62161 = AXIS2_PLACEMENT_3D ( 'NONE', #15117, #21308, #90177 ) ;
#62162 = CARTESIAN_POINT ( 'NONE',  ( 8.995981003084148497, 1409.227206965499818, 221.0723839244040221 ) ) ;
#62163 = CARTESIAN_POINT ( 'NONE',  ( 18.29112916889999951, 1425.477396046229842, 224.8880732489979835 ) ) ;
#62164 = CARTESIAN_POINT ( 'NONE',  ( -88.49990301145820126, 1385.187970965449949, 291.5961977735890400 ) ) ;
#62165 = CARTESIAN_POINT ( 'NONE',  ( -17.10576414770000042, 1413.991245370330034, 191.8646404599980144 ) ) ;
#62166 = CARTESIAN_POINT ( 'NONE',  ( -21.25567046294848694, 1379.716576505264129, 209.8535136764940887 ) ) ;
#62167 = EDGE_LOOP ( 'NONE', ( #103862, #34727, #38507, #42805, #109640 ) ) ;
#62168 = CARTESIAN_POINT ( 'NONE',  ( 10.95588612120169891, 1490.084719449429940, 208.7631480041860357 ) ) ;
#62170 = ORIENTED_EDGE ( 'NONE', *, *, #107452, .F. ) ;
#62169 = CARTESIAN_POINT ( 'NONE',  ( -3.767448257705639847, 1438.693583706480013, 227.3301816780199829 ) ) ;
#62171 = ORIENTED_EDGE ( 'NONE', *, *, #27647, .F. ) ;
#62172 =( BOUNDED_SURFACE ( )  B_SPLINE_SURFACE ( 3, 2, ( 
 ( #56780, #67403, #33214 ),
 ( #65190, #14758, #22576 ),
 ( #101502, #23152, #74143 ),
 ( #49490, #15834, #57891 ),
 ( #48389, #108825, #58991 ),
 ( #31560, #24789, #7467 ),
 ( #91479, #93120, #100424 ),
 ( #99302, #57354, #83613 ),
 ( #48945, #41067, #73596 ),
 ( #50584, #66849, #75245 ),
 ( #40515, #109936, #107725 ),
 ( #109395, #66306, #100959 ),
 ( #82532, #83076, #32671 ),
 ( #32121, #90918, #24255 ) ),
 .UNSPECIFIED., .F., .F., .F. ) 
 B_SPLINE_SURFACE_WITH_KNOTS ( ( 4, 2, 2, 2, 2, 2, 4 ),
 ( 3, 3 ),
 ( 0.000000000000000000, 0.0009440840677143978732, 0.001416126101571596810, 0.001888168135428795746, 0.002360210169285994683, 0.002832252203143193620, 0.003776336270857591493 ),
 ( 0.000000000000000000, 1.000000000000000000 ),
 .UNSPECIFIED. ) 
 GEOMETRIC_REPRESENTATION_ITEM ( )  RATIONAL_B_SPLINE_SURFACE ( (
 ( 1.000000000000000000, 0.8070209408750101954, 1.000000000000000000),
 ( 1.000000000000000000, 0.8215603905280027819, 1.000000000000000000),
 ( 1.000000000000000000, 0.8340988699066211876, 1.000000000000000000),
 ( 1.000000000000000000, 0.8516751610455791655, 1.000000000000000000),
 ( 1.000000000000000000, 0.8573697395154757928, 1.000000000000000000),
 ( 1.000000000000000000, 0.8683586635661659781, 1.000000000000000000),
 ( 1.000000000000000000, 0.8736518481709149020, 1.000000000000000000),
 ( 1.000000000000000000, 0.8840377753029594610, 1.000000000000000000),
 ( 1.000000000000000000, 0.8891294171303589788, 1.000000000000000000),
 ( 1.000000000000000000, 0.8992456600576572701, 1.000000000000000000),
 ( 1.000000000000000000, 0.9042785869254481579, 1.000000000000000000),
 ( 1.000000000000000000, 0.9189749222835162934, 1.000000000000000000),
 ( 1.000000000000000000, 0.9283978182351000363, 1.000000000000000000),
 ( 1.000000000000000000, 0.9376006582765954445, 1.000000000000000000) ) ) 
 REPRESENTATION_ITEM ( '' )  SURFACE ( )  );
#62173 = CARTESIAN_POINT ( 'NONE',  ( -12.18885905889360011, 1416.259629948840029, 194.7430301466939966 ) ) ;
#62174 = CARTESIAN_POINT ( 'NONE',  ( -2.273521285762763355, 1361.498772813854885, 207.6218459616988241 ) ) ;
#62175 = CARTESIAN_POINT ( 'NONE',  ( -11.93399382900000028, 1433.811405297789861, 150.6808762289980166 ) ) ;
#62176 = CARTESIAN_POINT ( 'NONE',  ( 17.58886893820438857, 1468.615884927995467, 269.3766193917544456 ) ) ;
#62177 = CARTESIAN_POINT ( 'NONE',  ( 11.98162358222930024, 1427.378834198339973, 208.3083443427269970 ) ) ;
#62178 = CARTESIAN_POINT ( 'NONE',  ( 1.113913563919999961, 1395.951959106130062, 220.1286928646979959 ) ) ;
#62179 = CARTESIAN_POINT ( 'NONE',  ( 22.39107469191120359, 1501.813592075909810, 209.7187615008220121 ) ) ;
#62180 = CARTESIAN_POINT ( 'NONE',  ( -6.003502551534990239, 1516.754677662452423, 213.6177932582572794 ) ) ;
#62181 = CARTESIAN_POINT ( 'NONE',  ( -0.8956140690670000293, 1476.679333595129947, 182.3599195072980024 ) ) ;
#62182 = CARTESIAN_POINT ( 'NONE',  ( -6.371134682375720892, 1368.423166410909971, 210.6218459616991936 ) ) ;
#62183 = CARTESIAN_POINT ( 'NONE',  ( -25.89297068493667808, 1436.665709121180498, 137.0068548018288084 ) ) ;
#62184 = CARTESIAN_POINT ( 'NONE',  ( -6.951175166914999259, 1517.170721208160103, 206.8315896683770063 ) ) ;
#62185 = CIRCLE ( 'NONE', #90761, 12.34219900309999929 ) ;
#62186 = CARTESIAN_POINT ( 'NONE',  ( -12.94285051013109999, 1434.751085630199896, 149.1919155958750025 ) ) ;
#62187 = DIRECTION ( 'NONE',  ( 1.224227143275421080E-16, 0.02617694830808806397, -0.9996573249755517088 ) ) ;
#62188 = CARTESIAN_POINT ( 'NONE',  ( -113.4000000000000057, 1306.913060387289988, 304.2218459572590064 ) ) ;
#62189 = CARTESIAN_POINT ( 'NONE',  ( -68.77190087506669158, 1379.747925807530009, 280.3125204381590265 ) ) ;
#62190 = CARTESIAN_POINT ( 'NONE',  ( 41.60066495211719939, 1444.057103930600078, 136.0676697147460175 ) ) ;
#62191 = ORIENTED_EDGE ( 'NONE', *, *, #40063, .F. ) ;
#62192 = EDGE_CURVE ( 'NONE', #33885, #104546, #61570, .T. ) ;
#62193 = CARTESIAN_POINT ( 'NONE',  ( 45.31148016700000625, 1435.337548181589909, 266.2043215618979843 ) ) ;
#62194 = CARTESIAN_POINT ( 'NONE',  ( -26.05067190950000011, 1469.243640235329849, 206.2660147011979745 ) ) ;
#62196 = CARTESIAN_POINT ( 'NONE',  ( -1.278194139027049925, 1507.616839994659813, 232.0618046316060088 ) ) ;
#62195 = CARTESIAN_POINT ( 'NONE',  ( -11.06188711399999924, 1426.914830454830053, 95.14035786269791117 ) ) ;
#62197 = CARTESIAN_POINT ( 'NONE',  ( -6.546302780145000000, 1516.577434278289957, 211.6089493897669911 ) ) ;
#62198 = CARTESIAN_POINT ( 'NONE',  ( -21.35837619870000026, 1471.309462467329922, 208.0048516116980295 ) ) ;
#62199 = CARTESIAN_POINT ( 'NONE',  ( -33.93598214789999901, 1424.339496380530136, 259.3467867270979923 ) ) ;
#62200 = CYLINDRICAL_SURFACE ( 'NONE', #109097, 2.000000000000003553 ) ;
#62201 = CARTESIAN_POINT ( 'NONE',  ( 28.91692647261170279, 1509.557647286829933, 209.5387477244159982 ) ) ;
#62202 = EDGE_CURVE ( 'NONE', #44739, #102101, #11791, .T. ) ;
#62203 = DIRECTION ( 'NONE',  ( -0.9980919085851078787, -0.06174578541841399537, 0.000000000000000000 ) ) ;
#62204 = CARTESIAN_POINT ( 'NONE',  ( 33.92643312500000263, 1450.868062273570104, 136.1711485282980050 ) ) ;
#62205 = ORIENTED_EDGE ( 'NONE', *, *, #99420, .F. ) ;
#62206 = CARTESIAN_POINT ( 'NONE',  ( -2.500000000000000000, 1432.353968296120001, 157.4944290049979827 ) ) ;
#62207 = CARTESIAN_POINT ( 'NONE',  ( 4.487249753806469954, 1509.038615938009798, 205.6342535008409982 ) ) ;
#62208 = CARTESIAN_POINT ( 'NONE',  ( -18.01357308700000104, 1458.773660595129968, 228.0936931546980020 ) ) ;
#62209 = ORIENTED_EDGE ( 'NONE', *, *, #42040, .F. ) ;
#62210 = EDGE_LOOP ( 'NONE', ( #7083, #79570, #68262, #64992, #47223 ) ) ;
#62211 = AXIS2_PLACEMENT_3D ( 'NONE', #74530, #63934, #4024 ) ;
#62212 = CARTESIAN_POINT ( 'NONE',  ( 10.13538064839599961, 1453.511863947389884, 212.2751250215330003 ) ) ;
#62213 = CARTESIAN_POINT ( 'NONE',  ( 9.146125554490000198, 1424.112737737530097, 196.6908568651990095 ) ) ;
#62214 = ORIENTED_EDGE ( 'NONE', *, *, #89073, .F. ) ;
#62215 = CARTESIAN_POINT ( 'NONE',  ( -0.2626479354700000379, 1424.305209145230037, 227.7945639678980285 ) ) ;
#62216 = CARTESIAN_POINT ( 'NONE',  ( 7.837683663321347360, 1446.693895632879048, 154.0817846991284910 ) ) ;
#62217 = CARTESIAN_POINT ( 'NONE',  ( 17.19739463999647100, 1525.960063244516959, 236.2603809477409982 ) ) ;
#62218 = AXIS2_PLACEMENT_3D ( 'NONE', #9151, #43315, #19171 ) ;
#62219 = CARTESIAN_POINT ( 'NONE',  ( -3.883780448710000055, 1489.060101785230017, 235.7933154220980043 ) ) ;
#62220 = CARTESIAN_POINT ( 'NONE',  ( 5.513207778675930371, 1508.731180391300086, 201.6768823099739905 ) ) ;
#62221 = PRESENTATION_LAYER_ASSIGNMENT (  '', '', ( #28228 ) ) ;
#62222 = CARTESIAN_POINT ( 'NONE',  ( 45.63098875785350117, 1442.771072822339875, 266.1895104264430074 ) ) ;
#62223 = CARTESIAN_POINT ( 'NONE',  ( 5.059013353549999259, 1501.257177412389865, 229.8390314845989906 ) ) ;
#62224 = CARTESIAN_POINT ( 'NONE',  ( 0.05774186599319999780, 1420.439312890830251, 183.3105440342980046 ) ) ;
#62225 = EDGE_LOOP ( 'NONE', ( #4130, #4938, #69313, #104230 ) ) ;
#62226 = CARTESIAN_POINT ( 'NONE',  ( -6.556022232634999725, 1516.833525648419936, 202.1813725979570222 ) ) ;
#62227 = CARTESIAN_POINT ( 'NONE',  ( -4.612671377915000370, 1516.783665406140017, 209.8782801844560026 ) ) ;
#62228 = ORIENTED_EDGE ( 'NONE', *, *, #62414, .F. ) ;
#62229 = CARTESIAN_POINT ( 'NONE',  ( 11.85801740980349983, 1431.772258989899910, 149.9533191514260011 ) ) ;
#62230 = CARTESIAN_POINT ( 'NONE',  ( 5.381311896276537610, 1511.468585895425122, 217.4468093684960763 ) ) ;
#62231 = ORIENTED_EDGE ( 'NONE', *, *, #27476, .F. ) ;
#62232 = CARTESIAN_POINT ( 'NONE',  ( 6.325886374943740620, 1422.669378755508660, 139.1419511335710695 ) ) ;
#62233 = CARTESIAN_POINT ( 'NONE',  ( -13.51812398686054451, 1443.501467202828962, 169.4008117781592375 ) ) ;
#62234 = CARTESIAN_POINT ( 'NONE',  ( 5.043681905660000631, 1508.915672638330079, 236.8001211188980051 ) ) ;
#62235 = CARTESIAN_POINT ( 'NONE',  ( -8.848880573389370952, 1470.096389303520255, 214.8940742741490055 ) ) ;
#62236 = CARTESIAN_POINT ( 'NONE',  ( 16.50977420799199891, 1452.336526367869965, 146.7133680455360150 ) ) ;
#62237 = CARTESIAN_POINT ( 'NONE',  ( 3.182038384110000173, 1408.010183206830106, 270.2907995557980598 ) ) ;
#62238 = CARTESIAN_POINT ( 'NONE',  ( 9.191577631451519181, 1450.202143376990080, 208.5180113977080225 ) ) ;
#62239 = CARTESIAN_POINT ( 'NONE',  ( -109.7763673550909544, 1383.370472583167611, 297.1349124586991479 ) ) ;
#62240 = CARTESIAN_POINT ( 'NONE',  ( 10.46269290780000105, 1491.122602396189905, 212.5073314721190059 ) ) ;
#62241 = CARTESIAN_POINT ( 'NONE',  ( -26.09133589079999993, 1379.618104246070061, 211.3566207186690065 ) ) ;
#62242 = CARTESIAN_POINT ( 'NONE',  ( 0.02672782265863862458, 1410.277270240254211, 233.2211595074259378 ) ) ;
#62244 = CARTESIAN_POINT ( 'NONE',  ( -1.541850711665649963E-13, 1515.064792882589927, 213.4512947377390049 ) ) ;
#62243 = CARTESIAN_POINT ( 'NONE',  ( -20.32158151839999860, 1505.095178026389931, 209.5373622212030114 ) ) ;
#62245 = CARTESIAN_POINT ( 'NONE',  ( 10.97694524628009916, 1422.961345275170061, 206.9164947625000082 ) ) ;
#62246 = AXIS2_PLACEMENT_3D ( 'NONE', #90613, #82772, #91720 ) ;
#62247 = CARTESIAN_POINT ( 'NONE',  ( -9.877301730868230933, 1439.855027102960094, 207.5146903145040085 ) ) ;
#62248 = CARTESIAN_POINT ( 'NONE',  ( -7.181020183025000669, 1512.881909847350016, 202.1577903523970008 ) ) ;
#62249 = ORIENTED_EDGE ( 'NONE', *, *, #16467, .T. ) ;
#62250 = CARTESIAN_POINT ( 'NONE',  ( 23.42675388609999843, 1440.913060387330006, 234.3916895593979746 ) ) ;
#62251 = CARTESIAN_POINT ( 'NONE',  ( -8.301987938657498844, 1512.913060387330006, 185.0111222839169898 ) ) ;
#62252 = CARTESIAN_POINT ( 'NONE',  ( -66.37566924875659424, 1385.037721167210066, 290.6307433382449972 ) ) ;
#62253 = CARTESIAN_POINT ( 'NONE',  ( -13.51610093809999924, 1443.913060387330006, 169.3501091259980171 ) ) ;
#62254 = CARTESIAN_POINT ( 'NONE',  ( 5.062625036090000030, 1505.549198612089867, 220.0219801153990034 ) ) ;
#62255 = DIRECTION ( 'NONE',  ( 0.9076935351921801010, 0.1286034085550979977, -0.3994416221155894786 ) ) ;
#62257 = EDGE_LOOP ( 'NONE', ( #87349, #64348, #100436, #108438 ) ) ;
#62256 = CARTESIAN_POINT ( 'NONE',  ( -1.629715277743620128, 1515.068677689339893, 204.7924989132399958 ) ) ;
#62258 = CARTESIAN_POINT ( 'NONE',  ( -15.84040666245470064, 1415.881310014747442, 209.7199984178415093 ) ) ;
#62259 = CARTESIAN_POINT ( 'NONE',  ( -24.15795475150000016, 1443.642594450309844, 212.0312900464880101 ) ) ;
#62260 = CARTESIAN_POINT ( 'NONE',  ( -0.5717982397045180409, 1450.893092752919983, 154.2461502927169761 ) ) ;
#62261 = CARTESIAN_POINT ( 'NONE',  ( -19.15298488520000220, 1464.559837765089924, 213.8319524061190009 ) ) ;
#62262 = CARTESIAN_POINT ( 'NONE',  ( 15.12442018213500106, 1514.217947259989842, 223.9588328087669993 ) ) ;
#62263 = CARTESIAN_POINT ( 'NONE',  ( 5.360823395318768725, 1422.262019483632912, 143.3077198672117163 ) ) ;
#62264 = CARTESIAN_POINT ( 'NONE',  ( 30.10957446088429990, 1509.964507489280095, 213.6424367098229880 ) ) ;
#62265 = CARTESIAN_POINT ( 'NONE',  ( -34.18677586421173231, 1501.977400791986611, 219.7932833225216882 ) ) ;
#62266 = CARTESIAN_POINT ( 'NONE',  ( -13.91344329490000042, 1453.313060387329870, 223.0352892571980021 ) ) ;
#62267 = CARTESIAN_POINT ( 'NONE',  ( 9.365061209729999447, 1417.415607571329929, 230.4107670011979678 ) ) ;
#62268 = CARTESIAN_POINT ( 'NONE',  ( -6.369643009819999868, 1476.618821349690052, 217.4015008671389921 ) ) ;
#62270 = CARTESIAN_POINT ( 'NONE',  ( -16.27761471759999878, 1460.158989628929930, 228.4983889328979956 ) ) ;
#62269 = AXIS2_PLACEMENT_3D ( 'NONE', #88319, #11614, #45790 ) ;
#62271 = CARTESIAN_POINT ( 'NONE',  ( 6.933879402874999265, 1516.560253536979872, 206.6353711893569880 ) ) ;
#62272 = CARTESIAN_POINT ( 'NONE',  ( 45.59816521089999952, 1434.873519021199854, 266.9907516340980465 ) ) ;
#62273 = CARTESIAN_POINT ( 'NONE',  ( 38.49765372689370224, 1444.525112227430100, 137.1053225086949681 ) ) ;
#62274 = CARTESIAN_POINT ( 'NONE',  ( 18.99827228379999866, 1436.394236938839867, 146.4527104209979882 ) ) ;
#62275 = CARTESIAN_POINT ( 'NONE',  ( 19.30811431869999950, 1488.591121188929947, 189.5534381757979929 ) ) ;
#62276 = CARTESIAN_POINT ( 'NONE',  ( 29.75998665772953444, 1509.996183727615517, 208.5887809057482798 ) ) ;
#62277 = CARTESIAN_POINT ( 'NONE',  ( -12.26530734194249916, 1377.620920188950095, 208.0499041502589819 ) ) ;
#62279 = EDGE_CURVE ( 'NONE', #102287, #104433, #36063, .T. ) ;
#62278 = CARTESIAN_POINT ( 'NONE',  ( 12.26996142119999966, 1416.831925149330118, 223.5794496915980005 ) ) ;
#62280 = DIRECTION ( 'NONE',  ( 4.465978680329379737E-17, 1.000000000000000000, -2.349386720892264891E-16 ) ) ;
#62281 = CARTESIAN_POINT ( 'NONE',  ( -38.57261905365100318, 1437.400638483769853, 135.9606806742719982 ) ) ;
#62282 = CARTESIAN_POINT ( 'NONE',  ( -8.524719538440001187, 1409.210750153330082, 197.0779234733980161 ) ) ;
#62283 = CARTESIAN_POINT ( 'NONE',  ( -17.17379625170000423, 1415.087974639930053, 205.5614638525080125 ) ) ;
#62284 = CARTESIAN_POINT ( 'NONE',  ( -12.76843643930000027, 1441.647446156619935, 188.0548363060980250 ) ) ;
#62285 = EDGE_CURVE ( 'NONE', #35225, #88507, #21462, .T. ) ;
#62286 = FACE_OUTER_BOUND ( 'NONE', #97872, .T. ) ;
#62287 = EDGE_CURVE ( 'NONE', #47969, #31004, #56271, .T. ) ;
#62288 = CARTESIAN_POINT ( 'NONE',  ( -33.54530754720000374, 1436.144128905479874, 136.3106138590979981 ) ) ;
#62289 = DIRECTION ( 'NONE',  ( -1.000000000000000000, 0.000000000000000000, 0.000000000000000000 ) ) ;
#62290 = EDGE_LOOP ( 'NONE', ( #15970, #43183, #102397, #84047, #43712 ) ) ;
#62291 = CARTESIAN_POINT ( 'NONE',  ( 5.773315218126072068, 1510.559702728265165, 216.6621837239362947 ) ) ;
#62292 = CARTESIAN_POINT ( 'NONE',  ( 28.02579834570000017, 1443.109842421789835, 137.4877371059980078 ) ) ;
#62293 = AXIS2_PLACEMENT_3D ( 'NONE', #41852, #100641, #102298 ) ;
#62294 = CARTESIAN_POINT ( 'NONE',  ( -13.13536861967500080, 1507.686078907830051, 209.3105439006200186 ) ) ;
#62295 = CARTESIAN_POINT ( 'NONE',  ( -33.79457713422360854, 1443.086052842850677, 154.8159889477085756 ) ) ;
#62296 = CARTESIAN_POINT ( 'NONE',  ( -44.39744386319999592, 1450.996159658330043, 269.0084819576979953 ) ) ;
#62297 = CARTESIAN_POINT ( 'NONE',  ( -15.81122951014150146, 1460.391797869179982, 222.7693532890990014 ) ) ;
#62298 = CIRCLE ( 'NONE', #8619, 1.999994853189497102 ) ;
#62299 = CARTESIAN_POINT ( 'NONE',  ( 0.1982234778270909881, 1420.450287161010010, 183.1181652783670017 ) ) ;
#62300 = CARTESIAN_POINT ( 'NONE',  ( 20.28160989826444194, 1526.000688113825163, 233.4099348503541762 ) ) ;
#62301 = CARTESIAN_POINT ( 'NONE',  ( -105.2189605138059960, 1384.590928737530021, 311.1873984220050033 ) ) ;
#62302 = CARTESIAN_POINT ( 'NONE',  ( -44.08363024569199951, 1385.000492669140158, 217.2190647443480032 ) ) ;
#62303 = CARTESIAN_POINT ( 'NONE',  ( 17.60455211062490122, 1424.145611629559880, 228.5323410459380113 ) ) ;
#62304 = CARTESIAN_POINT ( 'NONE',  ( 20.85715831889999805, 1508.960610664029900, 227.8108771944980049 ) ) ;
#62305 = AXIS2_PLACEMENT_3D ( 'NONE', #25182, #101889, #58814 ) ;
#62306 = CARTESIAN_POINT ( 'NONE',  ( 13.96291724000000123, 1452.419068613830177, 222.9619438482979774 ) ) ;
#62307 = B_SPLINE_CURVE_WITH_KNOTS ( 'NONE', 5,
 ( #1801, #77930, #18003, #1237, #42675, #76278 ),
 .UNSPECIFIED., .F., .F.,
 ( 6, 6 ),
 ( 302.5784080160000258, 307.6101328560000070 ),
 .UNSPECIFIED. ) ;
#62308 = B_SPLINE_CURVE_WITH_KNOTS ( 'NONE', 3,
 ( #31245, #44634, #34002, #87172, #60325, #19393, #27820, #96119, #85490, #436, #86612, #42971, #8235, #69288 ),
 .UNSPECIFIED., .F., .F.,
 ( 4, 2, 2, 2, 2, 2, 4 ),
 ( 0.000000000000000000, 0.1250000000000107969, 0.2500000000000215938, 0.3750000000000324185, 0.5000000000000431877, 0.7500000000000215383, 1.000000000000000000 ),
 .UNSPECIFIED. ) ;
#62309 = DIRECTION ( 'NONE',  ( 0.000000000000000000, 0.000000000000000000, -1.000000000000000000 ) ) ;
#62310 = CARTESIAN_POINT ( 'NONE',  ( 4.175269160410000069, 1515.456655180189955, 207.6381344832090008 ) ) ;
#62311 = CARTESIAN_POINT ( 'NONE',  ( -8.604279045229999312, 1384.934799959460179, 199.8686450314289971 ) ) ;
#62312 = VECTOR ( 'NONE', #92343, 1000.000000000000000 ) ;
#62313 = CARTESIAN_POINT ( 'NONE',  ( 3.280305111311562882, 1420.304449242272540, 137.1408355299612083 ) ) ;
#62314 = CARTESIAN_POINT ( 'NONE',  ( 15.47007019100000136, 1415.932617989529945, 199.1349231852080095 ) ) ;
#62315 = CARTESIAN_POINT ( 'NONE',  ( -11.76272948489999948, 1415.263254653229978, 195.3313732026979892 ) ) ;
#62316 = CARTESIAN_POINT ( 'NONE',  ( 0.3057263173670020096, 1422.515503742850115, 193.2688871159990072 ) ) ;
#62317 = CARTESIAN_POINT ( 'NONE',  ( 23.13869945629999947, 1409.885570435330010, 211.1617192280779989 ) ) ;
#62318 = CARTESIAN_POINT ( 'NONE',  ( -107.2902847454959954, 1391.913060387289988, 307.3027153792770036 ) ) ;
#62319 = CARTESIAN_POINT ( 'NONE',  ( 0.5708501887139260100, 1460.784142812889968, 230.4191102857249973 ) ) ;
#62320 = CARTESIAN_POINT ( 'NONE',  ( -16.16632277704758280, 1511.187213306747708, 236.8966194768525497 ) ) ;
#62322 = CARTESIAN_POINT ( 'NONE',  ( -11.71629925696549890, 1426.709133827190044, 142.6847339683789926 ) ) ;
#62321 = DIRECTION ( 'NONE',  ( -0.9942586961433765858, 0.000000000000000000, -0.1070030146457237041 ) ) ;
#62323 = CARTESIAN_POINT ( 'NONE',  ( -0.5000711780859999900, 1414.384141482430095, 233.3460081316979995 ) ) ;
#62324 = DIRECTION ( 'NONE',  ( 0.000000000000000000, 0.000000000000000000, 1.000000000000000000 ) ) ;
#62325 = CARTESIAN_POINT ( 'NONE',  ( -11.10693645390000128, 1491.078836222690143, 210.0430879654600176 ) ) ;
#62326 = DIRECTION ( 'NONE',  ( -0.9455185755993178454, 0.000000000000000000, 0.3255681544571537578 ) ) ;
#62327 = CARTESIAN_POINT ( 'NONE',  ( -9.178315062059999363, 1363.109187794150102, 210.6218459616991936 ) ) ;
#62328 = CARTESIAN_POINT ( 'NONE',  ( 5.773668814845000163, 1516.734985836460055, 205.0832084693769843 ) ) ;
#62329 = COLOUR_RGB ( '', 0.31764706, 0.68627451, 0.89019608) ;
#62330 = DIRECTION ( 'NONE',  ( -0.6736849260863841948, 0.000000000000000000, 0.7390186874254148774 ) ) ;
#62331 = CARTESIAN_POINT ( 'NONE',  ( -18.09406587330949634, 1485.999646426020036, 188.6973973258030242 ) ) ;
#62332 = CARTESIAN_POINT ( 'NONE',  ( -1778.470085355049832, -2339.246371527900010, 9314.971673131300122 ) ) ;
#62333 = CARTESIAN_POINT ( 'NONE',  ( -4.251699738499429948, 1441.330574127689943, 160.8255607727610084 ) ) ;
#62335 = ORIENTED_EDGE ( 'NONE', *, *, #104907, .T. ) ;
#62334 = CARTESIAN_POINT ( 'NONE',  ( -60.26586262799999361, 1379.746226298030024, 265.9249327376589918 ) ) ;
#62336 = ORIENTED_EDGE ( 'NONE', *, *, #26145, .T. ) ;
#62337 = CARTESIAN_POINT ( 'NONE',  ( 21.83164632205673072, 1524.739915903617430, 184.6225764830850835 ) ) ;
#62338 = ORIENTED_EDGE ( 'NONE', *, *, #40540, .T. ) ;
#62339 = CARTESIAN_POINT ( 'NONE',  ( 19.91075572344603017, 1526.211523310372058, 184.7300489233186624 ) ) ;
#62340 = CARTESIAN_POINT ( 'NONE',  ( 1.270728227940000066, 1414.996442546130083, 191.7853923321980005 ) ) ;
#62342 = CARTESIAN_POINT ( 'NONE',  ( 0.6486754834729999697, 1508.983017796130071, 179.4114288221979905 ) ) ;
#62341 = CARTESIAN_POINT ( 'NONE',  ( 15.97151636080159776, 1420.696294072290129, 191.2129961429930063 ) ) ;
#62343 = CARTESIAN_POINT ( 'NONE',  ( 11.91388749740000108, 1435.945967586000052, 151.0354243678980026 ) ) ;
#62344 = B_SPLINE_CURVE_WITH_KNOTS ( 'NONE', 5,
 ( #76506, #110656, #33949, #68143, #93842, #79283, #104467, #61397, #45699 ),
 .UNSPECIFIED., .F., .F.,
 ( 6, 3, 6 ),
 ( 0.000000000000000000, 0.5000000000000000000, 1.000000000000000000 ),
 .UNSPECIFIED. ) ;
#62345 = CARTESIAN_POINT ( 'NONE',  ( -24.50899199022319763, 1451.899203611129906, 137.2765321853150056 ) ) ;
#62346 = CARTESIAN_POINT ( 'NONE',  ( -105.8136274632349938, 1378.913060387269979, 304.5029232650449558 ) ) ;
#62347 = CARTESIAN_POINT ( 'NONE',  ( 10.73243676400000091, 1409.287845338830039, 228.4682584063980073 ) ) ;
#62348 = EDGE_CURVE ( 'NONE', #61054, #26950, #101460, .T. ) ;
#62349 = CARTESIAN_POINT ( 'NONE',  ( 0.01328393942530149870, 1516.939580991450157, 212.3834982571270018 ) ) ;
#62350 = CARTESIAN_POINT ( 'NONE',  ( 40.94560254887699813, 1440.384112706230098, 134.0999999980729740 ) ) ;
#62351 = CARTESIAN_POINT ( 'NONE',  ( -9.873494421475939475, 1422.989223822590020, 208.5817921780659958 ) ) ;
#62352 = CARTESIAN_POINT ( 'NONE',  ( 16.85775989529999919, 1430.051104475889815, 201.2392674849789955 ) ) ;
#62353 = ORIENTED_EDGE ( 'NONE', *, *, #4323, .F. ) ;
#62354 = CARTESIAN_POINT ( 'NONE',  ( -17.51440181060990042, 1442.103983326210027, 219.2287785421630133 ) ) ;
#62355 = CARTESIAN_POINT ( 'NONE',  ( -5.013264346206871558, 1375.415296214948967, 203.5257471534737874 ) ) ;
#62356 = ORIENTED_EDGE ( 'NONE', *, *, #93859, .F. ) ;
#62357 = ORIENTED_EDGE ( 'NONE', *, *, #60704, .T. ) ;
#62358 = ORIENTED_EDGE ( 'NONE', *, *, #38617, .F. ) ;
#62359 = CARTESIAN_POINT ( 'NONE',  ( 12.82869999662352001, 1444.968790463791493, 169.4459206408119485 ) ) ;
#62360 = CARTESIAN_POINT ( 'NONE',  ( 16.78936285056073885, 1513.473960732874730, 196.0527388798289223 ) ) ;
#62361 = CARTESIAN_POINT ( 'NONE',  ( 23.08678647408801154, 1450.877676292979459, 141.6717762082134300 ) ) ;
#62362 = CARTESIAN_POINT ( 'NONE',  ( -8.861951559199999551, 1384.939357637759940, 218.6849988088989960 ) ) ;
#62363 = CARTESIAN_POINT ( 'NONE',  ( 10.94770426880000080, 1460.983543286389931, 208.7734656400390065 ) ) ;
#62364 = CARTESIAN_POINT ( 'NONE',  ( -18.53455667172896426, 1445.620152175496969, 214.4552813252731198 ) ) ;
#62365 = CARTESIAN_POINT ( 'NONE',  ( -49.10452650019272625, 1379.685310564211932, 237.8554457964596338 ) ) ;
#62366 = CARTESIAN_POINT ( 'NONE',  ( 4.235647993021450119, 1446.341752434789896, 163.6975868290139999 ) ) ;
#62367 = CARTESIAN_POINT ( 'NONE',  ( 2.561957929796739641, 1389.413060387289988, 207.5609578920601450 ) ) ;
#62368 = ORIENTED_EDGE ( 'NONE', *, *, #68117, .F. ) ;
#62369 = CARTESIAN_POINT ( 'NONE',  ( 2.282622912365000367, 1516.861367446839949, 206.8218623544969716 ) ) ;
#62370 = ORIENTED_EDGE ( 'NONE', *, *, #104913, .T. ) ;
#62371 = CARTESIAN_POINT ( 'NONE',  ( 23.72057897983120256, 1440.913060387330006, 234.6026702862579896 ) ) ;
#62372 = CARTESIAN_POINT ( 'NONE',  ( -1.247677516857949989E-10, 1452.913060387320002, 152.5211338456990120 ) ) ;
#62373 = ORIENTED_EDGE ( 'NONE', *, *, #9057, .F. ) ;
#62374 = CARTESIAN_POINT ( 'NONE',  ( 26.53635440841820170, 1450.860531430359970, 136.4336726719780017 ) ) ;
#62375 = CARTESIAN_POINT ( 'NONE',  ( -14.62400382660000098, 1410.796324103030202, 190.5396985440980018 ) ) ;
#62376 = CARTESIAN_POINT ( 'NONE',  ( -46.87897873459490938, 1379.681191137500036, 239.9263311024370751 ) ) ;
#62378 = LINE ( 'NONE', #37148, #67015 ) ;
#62377 = CARTESIAN_POINT ( 'NONE',  ( -24.41180956639999877, 1441.164382444379953, 212.0429753022879993 ) ) ;
#62379 = CARTESIAN_POINT ( 'NONE',  ( 3.420678028885419941, 1423.764636203429973, 192.8424018407250173 ) ) ;
#62380 = CARTESIAN_POINT ( 'NONE',  ( -1.116585105924089969E-07, 1397.914279478820163, 196.1218459578329885 ) ) ;
#62381 = CARTESIAN_POINT ( 'NONE',  ( -5.102340803919999779, 1483.010473641589897, 199.7820758705289848 ) ) ;
#62382 = DIRECTION ( 'NONE',  ( -4.481801771516530428E-20, -1.000000000000000000, -2.868959329816139585E-18 ) ) ;
#62384 = EDGE_CURVE ( 'NONE', #19394, #98779, #82028, .T. ) ;
#62383 = CARTESIAN_POINT ( 'NONE',  ( -2.416613126590000160, 1507.334987533289905, 221.5267771657990181 ) ) ;
#62386 = CARTESIAN_POINT ( 'NONE',  ( 18.29188182340000068, 1431.768652859389704, 209.1218459616989946 ) ) ;
#62385 = CARTESIAN_POINT ( 'NONE',  ( 6.763640255447179445E-10, 1465.118916387369836, 238.1343321182859825 ) ) ;
#62387 = CIRCLE ( 'NONE', #96311, 24.00543915299668640 ) ;
#62388 = CARTESIAN_POINT ( 'NONE',  ( 6.556022194504999234, 1516.833525648419936, 216.0623193043769845 ) ) ;
#62389 = AXIS2_PLACEMENT_3D ( 'NONE', #12153, #87783, #1567 ) ;
#62390 = CARTESIAN_POINT ( 'NONE',  ( -0.5614708061910009818, 1469.825031502190086, 216.3963468629289935 ) ) ;
#62391 = CARTESIAN_POINT ( 'NONE',  ( 5.385694280313019000, 1511.434991102970116, 217.4429023633459792 ) ) ;
#62392 = VECTOR ( 'NONE', #64314, 1000.000000000000000 ) ;
#62393 = CARTESIAN_POINT ( 'NONE',  ( 28.49020452800000314, 1509.161987680929997, 209.1165913312309783 ) ) ;
#62394 = CARTESIAN_POINT ( 'NONE',  ( 7.725372132234999967, 1517.158319634930194, 211.9946825927569876 ) ) ;
#62395 = FACE_OUTER_BOUND ( 'NONE', #35891, .T. ) ;
#62396 = CARTESIAN_POINT ( 'NONE',  ( -3.423171246829689984, 1483.455259025470241, 199.0242790757120019 ) ) ;
#62398 = ORIENTED_EDGE ( 'NONE', *, *, #9699, .T. ) ;
#62397 = CARTESIAN_POINT ( 'NONE',  ( -83.92017472829999747, 1389.470547577029947, 291.9741855502589942 ) ) ;
#62399 = CARTESIAN_POINT ( 'NONE',  ( -18.49117142422373306, 1508.844092023391795, 229.9893364342464963 ) ) ;
#62400 = CARTESIAN_POINT ( 'NONE',  ( 5.038677020569999776, 1466.838857910729985, 244.5742075766979724 ) ) ;
#62401 = CARTESIAN_POINT ( 'NONE',  ( -19.16951723229999871, 1456.627470220629903, 228.8719212425980061 ) ) ;
#62402 = CARTESIAN_POINT ( 'NONE',  ( -14.83515152120000025, 1415.726119505169891, 205.6144808782789823 ) ) ;
#62403 = CARTESIAN_POINT ( 'NONE',  ( 2.922921630359999856, 1411.762167022229960, 231.6921255610980097 ) ) ;
#62404 = CARTESIAN_POINT ( 'NONE',  ( -18.51604897450000209, 1457.427690017329951, 227.8249311441979899 ) ) ;
#62406 = CARTESIAN_POINT ( 'NONE',  ( 2.500000000000000000, 1424.377232884329942, 154.7346221771979913 ) ) ;
#62405 = CARTESIAN_POINT ( 'NONE',  ( -23.24262678208922850, 1411.085038142911571, 205.4946917536888122 ) ) ;
#62407 = CARTESIAN_POINT ( 'NONE',  ( -9.526026435753081500, 1449.078195667740147, 208.0234617775689969 ) ) ;
#62408 = CARTESIAN_POINT ( 'NONE',  ( -105.9895980336749943, 1381.595986325180093, 309.4771618232359742 ) ) ;
#62409 = AXIS2_PLACEMENT_3D ( 'NONE', #58737, #51436, #33503 ) ;
#62410 = ORIENTED_EDGE ( 'NONE', *, *, #104050, .F. ) ;
#62411 = CARTESIAN_POINT ( 'NONE',  ( 7.324914918154999732, 1516.685667699390024, 204.5043554653269950 ) ) ;
#62412 = CARTESIAN_POINT ( 'NONE',  ( 0.5563350144439999090, 1406.068590282230161, 269.0455876907979587 ) ) ;
#62413 = CARTESIAN_POINT ( 'NONE',  ( -1.129779230740000084, 1515.569191395689813, 213.0910028086289856 ) ) ;
#62414 = EDGE_CURVE ( 'NONE', #86711, #16155, #3966, .T. ) ;
#62415 = CARTESIAN_POINT ( 'NONE',  ( 18.94924769094170358, 1469.137992140839970, 269.8899230648469825 ) ) ;
#62416 = EDGE_CURVE ( 'NONE', #20182, #84728, #32080, .T. ) ;
#62417 = CARTESIAN_POINT ( 'NONE',  ( 5.492221782479999703, 1439.600215925509929, 154.7521915351979942 ) ) ;
#62418 = CARTESIAN_POINT ( 'NONE',  ( -27.65015241038279825, 1446.921110007989910, 137.0757170956930224 ) ) ;
#62419 = EDGE_CURVE ( 'NONE', #70558, #83569, #101027, .T. ) ;
#62420 = CARTESIAN_POINT ( 'NONE',  ( -41.11110488297649823, 1440.913060408669935, 260.8062336396970409 ) ) ;
#62421 = CARTESIAN_POINT ( 'NONE',  ( -26.88188727640000053, 1446.276387282099904, 137.3361927622979977 ) ) ;
#62422 = CARTESIAN_POINT ( 'NONE',  ( 2.096062236828794667, 1450.108350418862301, 154.3469676365364762 ) ) ;
#62423 = CARTESIAN_POINT ( 'NONE',  ( -2.500000000000000000, 1448.894380601670036, 183.1110194938549967 ) ) ;
#62424 = EDGE_CURVE ( 'NONE', #36324, #66046, #100928, .T. ) ;
#62425 = CARTESIAN_POINT ( 'NONE',  ( 2.307020818445200128, 1449.832034875119916, 154.5197330722639890 ) ) ;
#62426 = EDGE_CURVE ( 'NONE', #89941, #64661, #106307, .T. ) ;
#62427 = CARTESIAN_POINT ( 'NONE',  ( 25.61394260045869942, 1439.706797436489978, 138.2743463228129883 ) ) ;
#62428 = CARTESIAN_POINT ( 'NONE',  ( 19.87032293674588956, 1498.069103587679137, 189.6526576822627987 ) ) ;
#62429 = ORIENTED_EDGE ( 'NONE', *, *, #60455, .F. ) ;
#62430 = CARTESIAN_POINT ( 'NONE',  ( -13.66603629819999810, 1410.384381565130070, 271.1218459616979999 ) ) ;
#62431 = EDGE_CURVE ( 'NONE', #36236, #76707, #16107, .T. ) ;
#62432 = CARTESIAN_POINT ( 'NONE',  ( 2.998248178699999933, 1486.828675832889985, 197.9694548352990182 ) ) ;
#62433 = DIRECTION ( 'NONE',  ( 0.000000000000000000, 1.000000000000000000, 0.000000000000000000 ) ) ;
#62434 = CARTESIAN_POINT ( 'NONE',  ( -0.8750415373510000983, 1475.042296104029901, 269.6498237395979913 ) ) ;
#62435 = CARTESIAN_POINT ( 'NONE',  ( -27.01382282590000017, 1451.969727051930022, 134.9184453750980026 ) ) ;
#62436 = CARTESIAN_POINT ( 'NONE',  ( -28.66654242860000323, 1509.598009360030119, 210.2644538831880254 ) ) ;
#62437 = CARTESIAN_POINT ( 'NONE',  ( -3.520715165324825424, 1448.288866220005502, 184.8838926225799071 ) ) ;
#62438 = CARTESIAN_POINT ( 'NONE',  ( -21.26129628348120448, 1384.858351126920070, 221.5120817745969930 ) ) ;
#62439 = CIRCLE ( 'NONE', #15932, 3.500000000000003109 ) ;
#62440 = B_SPLINE_SURFACE_WITH_KNOTS ( 'NONE', 5, 5, ( 
 ( #79646, #44387, #10776, #3494, #71825, #45504 ),
 ( #27022, #70166, #96432, #37622, #105945, #44948 ),
 ( #29224, #87489, #2948, #95871, #46046, #54455 ),
 ( #11874, #104278, #20798, #55000, #19137, #79095 ),
 ( #105386, #2403, #9646, #36521, #77967, #1275 ),
 ( #88048, #70714, #28674, #62306, #61211, #11333 ) ),
 .UNSPECIFIED., .F., .F., .F.,
 ( 6, 6 ),
 ( 6, 6 ),
 ( 30.32814661849999993, 107.3223151649999920 ),
 ( -5.551115123129999410E-17, 1.000000000000000000 ),
 .UNSPECIFIED. ) ;
#62441 = CARTESIAN_POINT ( 'NONE',  ( -18.76751273909999895, 1416.021639799829927, 207.7595312934080312 ) ) ;
#62442 = LINE ( 'NONE', #88171, #91210 ) ;
#62443 = CARTESIAN_POINT ( 'NONE',  ( 26.51151404034260040, 1435.625518892859873, 136.0790046155120194 ) ) ;
#62444 = CARTESIAN_POINT ( 'NONE',  ( -6.860236169661860117, 1396.152625115059891, 217.7799412713499976 ) ) ;
#62445 = EDGE_CURVE ( 'NONE', #15037, #85994, #2760, .T. ) ;
#62446 = CARTESIAN_POINT ( 'NONE',  ( -15.07723704620000049, 1422.393407695729820, 228.4053989051980125 ) ) ;
#62447 = CIRCLE ( 'NONE', #92848, 1.000000000000000888 ) ;
#62448 = CARTESIAN_POINT ( 'NONE',  ( -16.86826392510550221, 1409.748713083289886, 225.5163491958089992 ) ) ;
#62449 = CARTESIAN_POINT ( 'NONE',  ( 9.690208402899999740, 1434.541746329560056, 148.7586030823979968 ) ) ;
#62450 = ORIENTED_EDGE ( 'NONE', *, *, #55672, .F. ) ;
#62451 = CARTESIAN_POINT ( 'NONE',  ( -11.33467682473018989, 1502.178027852193054, 207.3042251687307669 ) ) ;
#62453 = ADVANCED_FACE ( 'NONE', ( #8079 ), #25093, .F. ) ;
#62452 = CARTESIAN_POINT ( 'NONE',  ( 1.137528735100000077, 1408.952783766029825, 230.8528660165980000 ) ) ;
#62454 = CARTESIAN_POINT ( 'NONE',  ( -17.28616084879999804, 1505.118892507889996, 223.1516167556989956 ) ) ;
#62456 = CARTESIAN_POINT ( 'NONE',  ( -9.976093183941980413, 1439.379388325520040, 208.6707327245020167 ) ) ;
#62455 = CARTESIAN_POINT ( 'NONE',  ( 11.19049484690000007, 1426.041365595529896, 112.6496013507980081 ) ) ;
#62457 = DIRECTION ( 'NONE',  ( 0.000000000000000000, 0.000000000000000000, -1.000000000000000000 ) ) ;
#62458 = ADVANCED_FACE ( 'NONE', ( #40866 ), #83192, .T. ) ;
#62459 = FACE_OUTER_BOUND ( 'NONE', #30261, .T. ) ;
#62460 = CARTESIAN_POINT ( 'NONE',  ( -2.485217232065000115, 1516.534320418310244, 201.4128137944169907 ) ) ;
#62461 = VECTOR ( 'NONE', #8016, 1000.000000000000000 ) ;
#62462 = CARTESIAN_POINT ( 'NONE',  ( 7.598639282229999736, 1424.430323257039845, 212.2253573777790052 ) ) ;
#62463 = DIRECTION ( 'NONE',  ( 0.2054769195713296304, -0.000000000000000000, -0.9786619618251631847 ) ) ;
#62464 = CARTESIAN_POINT ( 'NONE',  ( 15.00522596483500060, 1511.839858410419993, 197.1933472413670074 ) ) ;
#62465 = CARTESIAN_POINT ( 'NONE',  ( 7.594039249315000184, 1512.142919181319940, 206.8921143228970152 ) ) ;
#62466 = CARTESIAN_POINT ( 'NONE',  ( -84.31100485922900134, 1379.600296255510102, 298.0934801170350283 ) ) ;
#62467 = AXIS2_PLACEMENT_3D ( 'NONE', #86582, #61972, #76525 ) ;
#62468 = EDGE_CURVE ( 'NONE', #98527, #65089, #48184, .T. ) ;
#62469 = CARTESIAN_POINT ( 'NONE',  ( 9.842969107809999230, 1365.740588703660023, 207.6218459616989946 ) ) ;
#62471 = VERTEX_POINT ( 'NONE', #15093 ) ;
#62470 = CARTESIAN_POINT ( 'NONE',  ( -14.92438923741863732, 1460.034730685946442, 231.4439063516318527 ) ) ;
#62472 = ORIENTED_EDGE ( 'NONE', *, *, #18763, .F. ) ;
#62473 = CARTESIAN_POINT ( 'NONE',  ( -10.26338073471560008, 1521.551704408389924, 184.6900425920350131 ) ) ;
#62474 = AXIS2_PLACEMENT_3D ( 'NONE', #6353, #84698, #108812 ) ;
#62475 = CARTESIAN_POINT ( 'NONE',  ( -15.60376662210000198, 1409.457955924729958, 192.7658650750980200 ) ) ;
#62476 = CARTESIAN_POINT ( 'NONE',  ( 10.78330898009999927, 1453.313060387329870, 226.3563104863980016 ) ) ;
#62477 = CARTESIAN_POINT ( 'NONE',  ( -7.933914964464999109, 1511.279956263560052, 214.2433585108670115 ) ) ;
#62479 = CARTESIAN_POINT ( 'NONE',  ( -0.2876053136995322945, 1410.303643378096240, 185.0329637903212188 ) ) ;
#62478 = CARTESIAN_POINT ( 'NONE',  ( -8.205450199690000446, 1383.672729848519793, 218.6026122865090144 ) ) ;
#62480 = CARTESIAN_POINT ( 'NONE',  ( 22.97053994450000047, 1507.867546928429874, 193.7497404625980266 ) ) ;
#62481 = CARTESIAN_POINT ( 'NONE',  ( 9.862951377130659836, 1517.051704408389924, 189.8497022437369708 ) ) ;
#62482 = CARTESIAN_POINT ( 'NONE',  ( 21.20068119730000333, 1409.653404488529986, 206.8526477052579935 ) ) ;
#62483 =( NAMED_UNIT ( * ) SI_UNIT ( $, .STERADIAN. ) SOLID_ANGLE_UNIT ( ) );
#62484 = DIRECTION ( 'NONE',  ( -1.755985294532469921E-16, 1.000000000000000000, -1.338183447452831989E-16 ) ) ;
#62485 = CARTESIAN_POINT ( 'NONE',  ( 6.873845516911429421, 1396.153100362309942, 217.7692040646560088 ) ) ;
#62486 = CARTESIAN_POINT ( 'NONE',  ( 3.118363024329799948, 1407.662358049740078, 196.0555615279870096 ) ) ;
#62487 = CARTESIAN_POINT ( 'NONE',  ( -6.051417934638940288, 1406.798915588060026, 269.4859423177459803 ) ) ;
#62488 = DIRECTION ( 'NONE',  ( 0.000000000000000000, 1.000000000000000000, 0.000000000000000000 ) ) ;
#62489 = EDGE_LOOP ( 'NONE', ( #53722, #94319, #16849, #34889 ) ) ;
#62490 = CARTESIAN_POINT ( 'NONE',  ( -11.30129387189999868, 1432.307760205480008, 151.5220333356979836 ) ) ;
#62491 = CARTESIAN_POINT ( 'NONE',  ( 12.70666910289999940, 1441.123310893239932, 188.6801198206979961 ) ) ;
#62492 = VERTEX_POINT ( 'NONE', #82323 ) ;
#62493 = VERTEX_POINT ( 'NONE', #107519 ) ;
#62494 = CARTESIAN_POINT ( 'NONE',  ( -3.410565249569999846, 1454.671646890489910, 199.9594833787289758 ) ) ;
#62495 = CARTESIAN_POINT ( 'NONE',  ( 9.943976501839999926, 1365.461622992600041, 207.6218459616989946 ) ) ;
#62496 = VECTOR ( 'NONE', #9919, 999.9999999999998863 ) ;
#62497 = CARTESIAN_POINT ( 'NONE',  ( 1.131796810615000037, 1516.659138130710289, 214.8948242487770131 ) ) ;
#62498 = CARTESIAN_POINT ( 'NONE',  ( 4.824494990945000339, 1511.382391139620040, 217.5855882746469945 ) ) ;
#62499 = ADVANCED_FACE ( 'NONE', ( #5622 ), #66240, .F. ) ;
#62500 = ORIENTED_EDGE ( 'NONE', *, *, #76302, .T. ) ;
#62501 = CYLINDRICAL_SURFACE ( 'NONE', #39307, 2.000000000000003553 ) ;
#62502 = CARTESIAN_POINT ( 'NONE',  ( -88.45813511300001153, 1378.648767874889927, 298.0129420291590350 ) ) ;
#62503 = EDGE_CURVE ( 'NONE', #56035, #39464, #97652, .T. ) ;
#62504 = CARTESIAN_POINT ( 'NONE',  ( -105.8009562800430103, 1378.913060387269979, 303.8747423308259386 ) ) ;
#62505 = CARTESIAN_POINT ( 'NONE',  ( -6.559798094425000059, 1516.987478262539980, 204.5068286042669854 ) ) ;
#62506 = CARTESIAN_POINT ( 'NONE',  ( -20.49387964680000351, 1440.913060387330006, 220.0331557225980248 ) ) ;
#62507 = CARTESIAN_POINT ( 'NONE',  ( -106.7756681350000036, 1384.894991215109940, 297.1173194602590115 ) ) ;
#62508 = CARTESIAN_POINT ( 'NONE',  ( 4.115882860026048640, 1509.032014410905504, 204.7576542507069064 ) ) ;
#62509 = CARTESIAN_POINT ( 'NONE',  ( -5.193270068679999518, 1409.597742502030087, 231.5844012271980148 ) ) ;
#62511 = ORIENTED_EDGE ( 'NONE', *, *, #43802, .F. ) ;
#62510 = CARTESIAN_POINT ( 'NONE',  ( -11.95969313620000207, 1446.500039657790012, 187.4450217382979815 ) ) ;
#62512 = CARTESIAN_POINT ( 'NONE',  ( -14.45326777613875358, 1435.576065321126180, 149.6094576131308429 ) ) ;
#62513 = CARTESIAN_POINT ( 'NONE',  ( 3.060046442946298573, 1442.201648411282804, 217.5704250861406592 ) ) ;
#62514 = CARTESIAN_POINT ( 'NONE',  ( -1.252324120818309726E-15, 1383.870885931430166, 218.4497379877689980 ) ) ;
#62516 = ADVANCED_FACE ( 'NONE', ( #50936 ), #11154, .F. ) ;
#62515 = DIRECTION ( 'NONE',  ( 0.000000000000000000, -1.000000000000000000, 6.123233995736769734E-17 ) ) ;
#62517 = CARTESIAN_POINT ( 'NONE',  ( 43.83783482102600004, 1431.613819724010000, 269.7043230160370513 ) ) ;
#62518 = CARTESIAN_POINT ( 'NONE',  ( 5.011367946795000528, 1516.974592746400049, 212.5716232859570027 ) ) ;
#62519 = VECTOR ( 'NONE', #90020, 1000.000000000000000 ) ;
#62520 = CARTESIAN_POINT ( 'NONE',  ( -66.64551715449999847, 1379.743402054680018, 275.6922576809590169 ) ) ;
#62521 = CARTESIAN_POINT ( 'NONE',  ( 0.002486211556402507725, 1508.917723295689939, 238.6614435536396286 ) ) ;
#62522 = CARTESIAN_POINT ( 'NONE',  ( -30.24979188206167180, 1524.075000532257263, 222.4742415268079583 ) ) ;
#62523 = CARTESIAN_POINT ( 'NONE',  ( -21.44637720709119577, 1506.412686512840082, 216.0243823771180018 ) ) ;
#62524 = CARTESIAN_POINT ( 'NONE',  ( -2.480427292634999947, 1516.872851364150165, 209.8797317620669673 ) ) ;
#62525 = ORIENTED_EDGE ( 'NONE', *, *, #42808, .F. ) ;
#62526 = CARTESIAN_POINT ( 'NONE',  ( 2.500000000000000000, 1438.230658608039903, 157.6902399668979911 ) ) ;
#62527 = CARTESIAN_POINT ( 'NONE',  ( -5.228345434639999567, 1420.444146442230021, 232.2530053203980174 ) ) ;
#62528 =( BOUNDED_CURVE ( )  B_SPLINE_CURVE ( 3, ( #71925, #38809, #89770, #30965 ),
 .UNSPECIFIED., .F., .T. ) 
 B_SPLINE_CURVE_WITH_KNOTS ( ( 4, 4 ),
 ( 4.672237621782279859, 4.820400371478359425 ),
 .UNSPECIFIED. ) 
 CURVE ( )  GEOMETRIC_REPRESENTATION_ITEM ( )  RATIONAL_B_SPLINE_CURVE ( ( 1.000000000000000000, 0.9981714864442265966, 0.9981714864442265966, 1.000000000000000000 ) ) 
 REPRESENTATION_ITEM ( '' )  );
#62529 = CARTESIAN_POINT ( 'NONE',  ( -38.50281909529999780, 1385.190821792449924, 239.3058332809590070 ) ) ;
#62530 = ORIENTED_EDGE ( 'NONE', *, *, #57642, .F. ) ;
#62531 = CARTESIAN_POINT ( 'NONE',  ( -35.04101985798630636, 1385.208921701160079, 234.2276399419079951 ) ) ;
#62532 = AXIS2_PLACEMENT_3D ( 'NONE', #85111, #100801, #15677 ) ;
#62533 = EDGE_CURVE ( 'NONE', #32820, #56035, #102766, .T. ) ;
#62534 = CARTESIAN_POINT ( 'NONE',  ( -2.480175237380000119, 1429.207669949490082, 200.0830572027790026 ) ) ;
#62535 = CARTESIAN_POINT ( 'NONE',  ( 17.10527938397160241, 1469.008053439460127, 229.1126572397060102 ) ) ;
#62536 = CARTESIAN_POINT ( 'NONE',  ( -25.50992329942920023, 1509.803886753590177, 223.6772097800239862 ) ) ;
#62537 = ADVANCED_FACE ( 'NONE', ( #95691 ), #11681, .T. ) ;
#62538 = CARTESIAN_POINT ( 'NONE',  ( -24.91159428870000170, 1442.158245878219759, 210.4732786028779969 ) ) ;
#62539 = CARTESIAN_POINT ( 'NONE',  ( 0.1426546239810000116, 1409.853703253230151, 233.2022054432979985 ) ) ;
#62540 = CARTESIAN_POINT ( 'NONE',  ( -10.02843955878900140, 1517.051704408389924, 185.3723613107750054 ) ) ;
#62542 = CARTESIAN_POINT ( 'NONE',  ( 21.03123203779729877, 1507.789098030329797, 226.0655639048319756 ) ) ;
#62541 = CARTESIAN_POINT ( 'NONE',  ( -1.124289693584999972, 1517.184063036290127, 215.6857614941170027 ) ) ;
#62543 = CARTESIAN_POINT ( 'NONE',  ( 19.06717825319999804, 1508.525021977130109, 188.3911631520979881 ) ) ;
#62544 = CARTESIAN_POINT ( 'NONE',  ( 9.903643697897789977, 1469.012723375830092, 207.5198563789629986 ) ) ;
#62545 = EDGE_LOOP ( 'NONE', ( #87080, #56579, #46652, #75835, #45750, #87273, #92038, #27968 ) ) ;
#62546 = CARTESIAN_POINT ( 'NONE',  ( -12.74994028582299954, 1415.933499560010205, 196.6186742867360238 ) ) ;
#62547 = FACE_OUTER_BOUND ( 'NONE', #40865, .T. ) ;
#62548 = ORIENTED_EDGE ( 'NONE', *, *, #38173, .T. ) ;
#62549 = CIRCLE ( 'NONE', #21395, 1.000000000000000888 ) ;
#62550 = CARTESIAN_POINT ( 'NONE',  ( 3.175611140780000063, 1421.547207231229777, 184.0610320840980307 ) ) ;
#62551 = EDGE_CURVE ( 'NONE', #63587, #77632, #47328, .T. ) ;
#62552 = CARTESIAN_POINT ( 'NONE',  ( -21.83863730836054629, 1523.580203803270933, 183.2673815773256649 ) ) ;
#62553 = CARTESIAN_POINT ( 'NONE',  ( 18.90950544697915703, 1416.818673806273864, 209.9484509850840084 ) ) ;
#62554 = UNCERTAINTY_MEASURE_WITH_UNIT (LENGTH_MEASURE( 1.000000000000000082E-05 ), #41521, 'distance_accuracy_value', 'NONE');
#62555 = CARTESIAN_POINT ( 'NONE',  ( 2.907186931900000104, 1441.882235772590093, 217.8664262967990055 ) ) ;
#62556 = CARTESIAN_POINT ( 'NONE',  ( -30.11977250498258130, 1524.538768545233779, 195.8653401176965758 ) ) ;
#62557 = FACE_OUTER_BOUND ( 'NONE', #30613, .T. ) ;
#62558 = CARTESIAN_POINT ( 'NONE',  ( 17.40764059099999628, 1414.996444526030018, 210.6782161193179945 ) ) ;
#62560 = ADVANCED_FACE ( 'NONE', ( #45858 ), #20523, .T. ) ;
#62559 = CARTESIAN_POINT ( 'NONE',  ( -18.96495392289999771, 1425.684290752429888, 226.5179610041979856 ) ) ;
#62561 = CARTESIAN_POINT ( 'NONE',  ( -20.19975713530000050, 1435.203085175510068, 142.9756137166980068 ) ) ;
#62562 = DIRECTION ( 'NONE',  ( 9.367506770274749475E-14, 0.000000000000000000, 1.000000000000000000 ) ) ;
#62563 = CARTESIAN_POINT ( 'NONE',  ( 7.012921468763117616, 1508.551704408389924, 215.5137847777533580 ) ) ;
#62565 = DIRECTION ( 'NONE',  ( -0.000000000000000000, -0.000000000000000000, 1.000000000000000000 ) ) ;
#62564 = DIRECTION ( 'NONE',  ( -0.5877852522924673639, 0.000000000000000000, 0.8090169943749514481 ) ) ;
#62566 = CARTESIAN_POINT ( 'NONE',  ( 27.09589979614590050, 1438.319408107809977, 136.9553273407819916 ) ) ;
#62567 = ORIENTED_EDGE ( 'NONE', *, *, #98706, .F. ) ;
#62568 = CARTESIAN_POINT ( 'NONE',  ( -7.756912786389999148, 1508.430206397490110, 219.4938868140989996 ) ) ;
#62569 = CARTESIAN_POINT ( 'NONE',  ( 27.04494987192744659, 1509.634160115218492, 216.9800109594045523 ) ) ;
#62570 = EDGE_CURVE ( 'NONE', #42748, #21389, #20073, .T. ) ;
#62571 = CARTESIAN_POINT ( 'NONE',  ( 12.10384758683500017, 1512.631076693560090, 200.5535322512070024 ) ) ;
#62572 = CARTESIAN_POINT ( 'NONE',  ( -1.954671169420000076, 1485.152615037190117, 198.1756556538989855 ) ) ;
#62573 = AXIS2_PLACEMENT_3D ( 'NONE', #47139, #39829, #82926 ) ;
#62574 = CARTESIAN_POINT ( 'NONE',  ( -16.53125420670000167, 1418.541487540729804, 202.7561987471289910 ) ) ;
#62575 = CARTESIAN_POINT ( 'NONE',  ( -2.478617600774434049, 1524.659802833172535, 242.4723780654675522 ) ) ;
#62576 = CARTESIAN_POINT ( 'NONE',  ( 11.77972227726102616, 1435.190141807486953, 151.2912773572372487 ) ) ;
#62577 = B_SPLINE_SURFACE_WITH_KNOTS ( 'NONE', 5, 5, ( 
 ( #69609, #1281, #42170, #51128, #70173, #102054 ),
 ( #34314, #103728, #110472, #102593, #25893, #69053 ),
 ( #76322, #50577, #18593, #27030, #84704, #33750 ),
 ( #8004, #103153, #77975, #67944, #77431, #16380 ),
 ( #9656, #34864, #25338, #16926, #59532, #52791 ),
 ( #43828, #85253, #52245, #17482, #93644, #86371 ),
 ( #35422, #61219, #60649, #94772, #24779, #26455 ),
 ( #8552, #732, #95333, #78536, #86925, #44394 ),
 ( #60092, #58978, #93109, #10216, #42724, #1847 ) ),
 .UNSPECIFIED., .F., .F., .F.,
 ( 6, 3, 6 ),
 ( 6, 6 ),
 ( 0.000000000000000000, 1.560949918229999955, 3.121899836449999910 ),
 ( 0.000000000000000000, 2.000000000000000000 ),
 .UNSPECIFIED. ) ;
#62578 = CARTESIAN_POINT ( 'NONE',  ( 32.78250617288044566, 1512.187213306747481, 218.3079823578266314 ) ) ;
#62579 = CARTESIAN_POINT ( 'NONE',  ( -18.59026783009990069, 1509.562244740590131, 185.7097730471209900 ) ) ;
#62580 = EDGE_CURVE ( 'NONE', #10196, #104308, #3317, .T. ) ;
#62581 = EDGE_CURVE ( 'NONE', #26364, #86670, #26709, .T. ) ;
#62582 = CARTESIAN_POINT ( 'NONE',  ( -4.237929439762339712, 1486.921074483630036, 220.3845766509240036 ) ) ;
#62583 = CARTESIAN_POINT ( 'NONE',  ( -22.15968325629999924, 1485.573345355790025, 217.2083650093589995 ) ) ;
#62584 = CARTESIAN_POINT ( 'NONE',  ( -85.31977994509040286, 1383.773333636219832, 306.6464895601730518 ) ) ;
#62585 = CARTESIAN_POINT ( 'NONE',  ( -109.6626209149679880, 1383.298351538420093, 311.2476010510089850 ) ) ;
#62586 = DIRECTION ( 'NONE',  ( -8.673617379884027583E-16, 0.000000000000000000, 1.000000000000000000 ) ) ;
#62587 = CARTESIAN_POINT ( 'NONE',  ( 7.069907484889999871, 1426.666557891380080, 213.2414385277990050 ) ) ;
#62589 = ORIENTED_EDGE ( 'NONE', *, *, #32431, .F. ) ;
#62588 = CARTESIAN_POINT ( 'NONE',  ( 22.79519389169999855, 1509.727640877830027, 190.2016567581979984 ) ) ;
#62590 = CIRCLE ( 'NONE', #67919, 1.999999999999994227 ) ;
#62591 = CARTESIAN_POINT ( 'NONE',  ( -94.49938873620000379, 1383.385654720950015, 294.8908487859590082 ) ) ;
#62592 = CARTESIAN_POINT ( 'NONE',  ( -0.8945946638535250406, 1417.298095655010002, 235.8147265033050246 ) ) ;
#62593 = ORIENTED_EDGE ( 'NONE', *, *, #4899, .F. ) ;
#62594 = ORIENTED_EDGE ( 'NONE', *, *, #265, .F. ) ;
#62595 = CARTESIAN_POINT ( 'NONE',  ( 13.12363690099999936, 1441.384603101129869, 188.9419487780980091 ) ) ;
#62596 = CARTESIAN_POINT ( 'NONE',  ( -109.7177239279999981, 1384.918725008840056, 297.0861730621589913 ) ) ;
#62597 = CARTESIAN_POINT ( 'NONE',  ( 13.11628250257718520, 1443.038395467839564, 169.4035201152188108 ) ) ;
#62599 = CARTESIAN_POINT ( 'NONE',  ( -11.55307712329999958, 1469.479397749430063, 255.2309127613979740 ) ) ;
#62598 = CARTESIAN_POINT ( 'NONE',  ( 35.04047526790853340, 1424.095413727867026, 269.5320722744115756 ) ) ;
#62600 = EDGE_CURVE ( 'NONE', #65949, #35843, #20605, .T. ) ;
#62601 = CARTESIAN_POINT ( 'NONE',  ( 9.390592470051840834, 1435.626267691329986, 208.9162517377799873 ) ) ;
#62602 = CARTESIAN_POINT ( 'NONE',  ( -11.90370000490000102, 1433.409417285139853, 150.2262481879979816 ) ) ;
#62603 = CARTESIAN_POINT ( 'NONE',  ( 11.45577226660000036, 1502.286415424589904, 208.3140783707030153 ) ) ;
#62604 = CARTESIAN_POINT ( 'NONE',  ( -19.05006020489999941, 1485.976765364930088, 189.5158719427979861 ) ) ;
#62605 = CARTESIAN_POINT ( 'NONE',  ( 11.42864686989999967, 1410.242058359229986, 189.4498630199979914 ) ) ;
#62606 = CARTESIAN_POINT ( 'NONE',  ( 4.908548385079999576, 1422.370476885929975, 184.3612921802979940 ) ) ;
#62608 = EDGE_CURVE ( 'NONE', #79161, #80182, #54803, .T. ) ;
#62607 = CARTESIAN_POINT ( 'NONE',  ( -1.475794679986299984, 1515.075282686699893, 213.4510200518020042 ) ) ;
#62609 = CARTESIAN_POINT ( 'NONE',  ( -20.39147186913014664, 1526.073429442291854, 185.1130304870873715 ) ) ;
#62610 = CARTESIAN_POINT ( 'NONE',  ( -15.83806605205309914, 1420.932712493960025, 203.3750394557980314 ) ) ;
#62611 = CARTESIAN_POINT ( 'NONE',  ( 19.53786426059039982, 1512.187213306747481, 238.7197124308265188 ) ) ;
#62613 = ORIENTED_EDGE ( 'NONE', *, *, #69224, .F. ) ;
#62612 = CYLINDRICAL_SURFACE ( 'NONE', #74799, 2.000000000000003553 ) ;
#62614 = ORIENTED_EDGE ( 'NONE', *, *, #8081, .F. ) ;
#62615 = CARTESIAN_POINT ( 'NONE',  ( 1.997114501359403604, 1517.051704408389924, 188.3688149103338958 ) ) ;
#62616 = CARTESIAN_POINT ( 'NONE',  ( -22.18488176075830154, 1483.996195745850173, 216.8908803982089921 ) ) ;
#62617 = CARTESIAN_POINT ( 'NONE',  ( -15.45910334130000052, 1472.202164814229945, 270.0849031532980007 ) ) ;
#62618 = CARTESIAN_POINT ( 'NONE',  ( 12.02531869610000115, 1420.571450649919825, 199.9272147486889821 ) ) ;
#62619 = CARTESIAN_POINT ( 'NONE',  ( 3.364556988579999963, 1443.913060387330006, 155.8032249175980155 ) ) ;
#62620 = CARTESIAN_POINT ( 'NONE',  ( -15.18343130929999951, 1495.928917307730217, 224.4314295560979815 ) ) ;
#62621 = AXIS2_PLACEMENT_3D ( 'NONE', #94244, #34354, #79136 ) ;
#62622 = CARTESIAN_POINT ( 'NONE',  ( 14.59882275830000076, 1475.513060387329915, 194.5230232028980026 ) ) ;
#62623 = CARTESIAN_POINT ( 'NONE',  ( -12.36841580329999779, 1419.558714398729990, 228.6604469819980068 ) ) ;
#62624 = DIRECTION ( 'NONE',  ( 5.364597654988746180E-15, -0.5877852522921409584, 0.8090169943751888137 ) ) ;
#62625 = CARTESIAN_POINT ( 'NONE',  ( 9.989381280457715562, 1361.309659810096264, 208.3718459617010978 ) ) ;
#62626 = CARTESIAN_POINT ( 'NONE',  ( -44.92397794980949755, 1433.724551782629987, 266.4419929911069858 ) ) ;
#62627 = AXIS2_PLACEMENT_3D ( 'NONE', #18766, #362, #34488 ) ;
#62628 = EDGE_LOOP ( 'NONE', ( #92608, #4492, #89698, #89401 ) ) ;
#62629 = CARTESIAN_POINT ( 'NONE',  ( -7.961002066000000710, 1424.384911837800018, 210.5206767801589933 ) ) ;
#62630 = ORIENTED_EDGE ( 'NONE', *, *, #10758, .F. ) ;
#62631 = CARTESIAN_POINT ( 'NONE',  ( -4.028611259245000298, 1516.744381837270112, 210.2562039408269925 ) ) ;
#62632 = CARTESIAN_POINT ( 'NONE',  ( 15.20184466319999927, 1507.442701412029919, 192.3795476405979912 ) ) ;
#62633 = CARTESIAN_POINT ( 'NONE',  ( -20.86058274790000056, 1508.959351158429854, 190.3690864228979933 ) ) ;
#62634 = CARTESIAN_POINT ( 'NONE',  ( -14.56904612549999989, 1425.418745057229899, 189.7987151475979886 ) ) ;
#62635 = CARTESIAN_POINT ( 'NONE',  ( -3.897009771321175986, 1521.951704408389787, 187.2231132109079113 ) ) ;
#62636 = ORIENTED_EDGE ( 'NONE', *, *, #87021, .F. ) ;
#62637 = CARTESIAN_POINT ( 'NONE',  ( 10.22326110114815201, 1374.913060387290216, 204.3929701860967896 ) ) ;
#62638 = CARTESIAN_POINT ( 'NONE',  ( -6.554764199395000546, 1516.786099423779888, 201.4062207291269999 ) ) ;
#62639 = CARTESIAN_POINT ( 'NONE',  ( 9.578155386300000629, 1471.786587761589772, 213.7186015179489971 ) ) ;
#62640 = CARTESIAN_POINT ( 'NONE',  ( -9.671333196654149589, 1440.258410182710122, 206.4805632831669868 ) ) ;
#62641 = ORIENTED_EDGE ( 'NONE', *, *, #3143, .F. ) ;
#62642 = CARTESIAN_POINT ( 'NONE',  ( -13.09932316763100069, 1411.200286183310027, 270.0791247197240068 ) ) ;
#62643 = CARTESIAN_POINT ( 'NONE',  ( 1.704170714124999986, 1516.927039499179955, 208.3639196453299860 ) ) ;
#62644 = CARTESIAN_POINT ( 'NONE',  ( -1.496858517070000172, 1428.056401037730211, 101.8807690336980016 ) ) ;
#62645 = CARTESIAN_POINT ( 'NONE',  ( 9.528477832624719923, 1434.647097723040133, 206.8891366029810115 ) ) ;
#62647 = VERTEX_POINT ( 'NONE', #87291 ) ;
#62646 = CARTESIAN_POINT ( 'NONE',  ( -7.951609945375088806, 1366.194798799167529, 210.6218459617142003 ) ) ;
#62648 = ORIENTED_EDGE ( 'NONE', *, *, #76302, .F. ) ;
#62649 = CARTESIAN_POINT ( 'NONE',  ( 45.60270269536359677, 1442.242646908569441, 268.9756891917134567 ) ) ;
#62650 = CARTESIAN_POINT ( 'NONE',  ( 11.38585543042319870, 1471.209044977530084, 209.9613054878209937 ) ) ;
#62651 = CARTESIAN_POINT ( 'NONE',  ( 3.627217813073119856, 1424.534510419196295, 184.5254139637974617 ) ) ;
#62652 = AXIS2_PLACEMENT_3D ( 'NONE', #80028, #107972, #89521 ) ;
#62653 = CARTESIAN_POINT ( 'NONE',  ( -113.4000000000000057, 1391.913060387289988, 304.2218459572590064 ) ) ;
#62654 = CARTESIAN_POINT ( 'NONE',  ( -20.66004298134364348, 1506.560172258414468, 216.9379300855220265 ) ) ;
#62655 = CARTESIAN_POINT ( 'NONE',  ( 2.560290627914949990, 1439.616563506700004, 157.6871905427350100 ) ) ;
#62656 = CARTESIAN_POINT ( 'NONE',  ( -0.0001242829754057280032, 1476.076625553489748, 267.5369961020650749 ) ) ;
#62657 = CARTESIAN_POINT ( 'NONE',  ( 12.61566532500000015, 1416.819756528530206, 223.3235035255980279 ) ) ;
#62658 = CARTESIAN_POINT ( 'NONE',  ( 7.451360406109999168, 1445.833858733300076, 184.1298986146979928 ) ) ;
#62659 = CARTESIAN_POINT ( 'NONE',  ( 3.445407533985000104, 1516.764084769670262, 206.8237970085970119 ) ) ;
#62660 = EDGE_LOOP ( 'NONE', ( #47196, #27964, #41336 ) ) ;
#62661 = DIRECTION ( 'NONE',  ( 0.5032920991128611021, 0.8641163480519101769, 0.000000000000000000 ) ) ;
#62662 = CARTESIAN_POINT ( 'NONE',  ( 1.520870652216739893, 1456.386238873960110, 183.3280966458629848 ) ) ;
#62663 = ORIENTED_EDGE ( 'NONE', *, *, #22699, .F. ) ;
#62665 = VECTOR ( 'NONE', #6651, 1000.000000000000114 ) ;
#62664 = CARTESIAN_POINT ( 'NONE',  ( 11.86629848729999992, 1432.349867583790001, 149.9824242020979739 ) ) ;
#62666 = ADVANCED_FACE ( 'NONE', ( #79448 ), #5379, .T. ) ;
#62667 = CARTESIAN_POINT ( 'NONE',  ( 24.88563714215300138, 1451.888913396479893, 136.5992973529910159 ) ) ;
#62668 = CARTESIAN_POINT ( 'NONE',  ( 14.44947381900000138, 1416.568813549730066, 196.8603287955980079 ) ) ;
#62669 = CARTESIAN_POINT ( 'NONE',  ( -24.59348072959999953, 1389.777865159989915, 218.7886947571089991 ) ) ;
#62670 = CARTESIAN_POINT ( 'NONE',  ( -18.65451756193940014, 1507.632629711779828, 229.7110761618599781 ) ) ;
#62671 = CARTESIAN_POINT ( 'NONE',  ( 17.65747903809999997, 1409.529673141430067, 194.8433731264979940 ) ) ;
#62672 = CARTESIAN_POINT ( 'NONE',  ( 22.12674011680000064, 1409.685743178530174, 208.3470065124739676 ) ) ;
#62673 = CARTESIAN_POINT ( 'NONE',  ( 17.41346922039999967, 1410.020394367130166, 224.8086586025980012 ) ) ;
#62674 = CARTESIAN_POINT ( 'NONE',  ( -20.22025100119805074, 1426.743699746497214, 222.0673968628566968 ) ) ;
#62675 = CARTESIAN_POINT ( 'NONE',  ( 0.3900490083317569301, 1451.467585376839907, 182.7676827736779899 ) ) ;
#62676 = CARTESIAN_POINT ( 'NONE',  ( 17.76546875260000036, 1430.865606781589804, 204.9340536459789917 ) ) ;
#62677 = CARTESIAN_POINT ( 'NONE',  ( -7.714371541114999786, 1516.738222552470233, 214.9014490703569891 ) ) ;
#62678 = CARTESIAN_POINT ( 'NONE',  ( 2.664543536380612920, 1524.964158026966061, 241.7076164033512100 ) ) ;
#62679 = ORIENTED_EDGE ( 'NONE', *, *, #68157, .F. ) ;
#62680 = CARTESIAN_POINT ( 'NONE',  ( -17.28926732269999889, 1417.627268025079957, 207.2086015117089914 ) ) ;
#62681 = CARTESIAN_POINT ( 'NONE',  ( 22.52214966618161895, 1524.244163922423468, 236.5012798002490513 ) ) ;
#62682 = CARTESIAN_POINT ( 'NONE',  ( -0.4378591917222510177, 1409.291352615860205, 232.6949995814360364 ) ) ;
#62683 = CARTESIAN_POINT ( 'NONE',  ( -20.79738390328759579, 1512.187213306747481, 181.2030061003473236 ) ) ;
#62684 = CARTESIAN_POINT ( 'NONE',  ( -37.55592389275750520, 1449.175610547529914, 136.3350282757720038 ) ) ;
#62685 = DIRECTION ( 'NONE',  ( 1.755985294532469921E-16, -1.000000000000000000, 1.338183447452831989E-16 ) ) ;
#62686 = CARTESIAN_POINT ( 'NONE',  ( -19.62446893450000118, 1440.913060387330006, 214.3676144200779845 ) ) ;
#62687 = CIRCLE ( 'NONE', #28683, 4.003638137702854038 ) ;
#62688 = CARTESIAN_POINT ( 'NONE',  ( -1.749739496465730015, 1458.392920694240047, 183.8987760949310086 ) ) ;
#62690 = EDGE_CURVE ( 'NONE', #29266, #71450, #78806, .T. ) ;
#62689 = DIRECTION ( 'NONE',  ( 0.9970203751124364633, -0.07713865185920967815, 0.000000000000000000 ) ) ;
#62691 = CARTESIAN_POINT ( 'NONE',  ( -0.3022264190282230034, 1475.058218936390176, 269.6445798187899641 ) ) ;
#62692 = B_SPLINE_SURFACE_WITH_KNOTS ( 'NONE', 5, 5, ( 
 ( #58568, #83207, #48521, #82660, #5951, #74278 ),
 ( #49072, #33335, #31139, #14881, #84303, #56910 ),
 ( #110060, #107850, #65324, #40096, #66432, #75376 ),
 ( #74819, #5395, #31689, #24384, #40648, #41749 ),
 ( #82094, #65871, #99991, #100548, #50175, #108965 ),
 ( #23828, #58020, #93251, #92155, #49619, #75908 ),
 ( #39553, #83752, #7048, #99434, #41206, #23283 ),
 ( #32791, #67530, #7594, #91043, #101630, #24919 ),
 ( #59129, #73727, #78109, #95470, #43422, #8137 ) ),
 .UNSPECIFIED., .F., .F., .F.,
 ( 6, 3, 6 ),
 ( 6, 6 ),
 ( 6.826668448630000685E-15, 3.228996143019999820, 6.457992286039999641 ),
 ( 0.000000000000000000, 2.000000000000000000 ),
 .UNSPECIFIED. ) ;
#62693 = CARTESIAN_POINT ( 'NONE',  ( -9.622986749620970670, 1460.696243629709898, 210.1029813304209881 ) ) ;
#62694 = CARTESIAN_POINT ( 'NONE',  ( -20.90646223069999721, 1508.014129115030073, 227.8602063216980014 ) ) ;
#62695 = CARTESIAN_POINT ( 'NONE',  ( 10.57324062335630011, 1500.889090984059976, 204.6344996329069943 ) ) ;
#62696 = ORIENTED_EDGE ( 'NONE', *, *, #101364, .F. ) ;
#62697 = ADVANCED_FACE ( 'NONE', ( #59759 ), #45601, .T. ) ;
#62698 = CIRCLE ( 'NONE', #57252, 2.000000000000000000 ) ;
#62699 = CARTESIAN_POINT ( 'NONE',  ( -26.60753696249999933, 1509.169818246329896, 201.4350730330979786 ) ) ;
#62700 = AXIS2_PLACEMENT_3D ( 'NONE', #98107, #5721, #99196 ) ;
#62701 = DIRECTION ( 'NONE',  ( 5.980589973904019347E-17, -1.000000000000000000, 1.736889445713099699E-16 ) ) ;
#62702 = EDGE_CURVE ( 'NONE', #106344, #3400, #85521, .T. ) ;
#62703 = CARTESIAN_POINT ( 'NONE',  ( -6.940787512450000030, 1485.992914485530264, 182.8505493415979970 ) ) ;
#62704 = CARTESIAN_POINT ( 'NONE',  ( -2.596261494520250679, 1525.907212628473644, 240.7735774411711986 ) ) ;
#62705 = CARTESIAN_POINT ( 'NONE',  ( -13.53908046754547634, 1489.771924351148527, 192.3260543307453361 ) ) ;
#62706 = AXIS2_PLACEMENT_3D ( 'NONE', #26632, #84339, #92735 ) ;
#62707 = CARTESIAN_POINT ( 'NONE',  ( 24.93712286909999776, 1430.363841012629791, 209.4446161091190106 ) ) ;
#62708 = ADVANCED_FACE ( 'NONE', ( #24465 ), #41189, .F. ) ;
#62709 = CARTESIAN_POINT ( 'NONE',  ( -16.91899155701270629, 1419.993940084556698, 207.8764500463518630 ) ) ;
#62710 = CARTESIAN_POINT ( 'NONE',  ( 7.156887453669999566, 1427.109879847909951, 213.1306117699590175 ) ) ;
#62711 = CARTESIAN_POINT ( 'NONE',  ( -18.28047778769730058, 1383.855358566239829, 220.1279645894470036 ) ) ;
#62712 = CARTESIAN_POINT ( 'NONE',  ( -2.537545712159490652, 1430.163801573863793, 201.1758857049043741 ) ) ;
#62713 = CARTESIAN_POINT ( 'NONE',  ( -16.81223434880759982, 1414.913060387349788, 207.5743820648510223 ) ) ;
#62714 = CARTESIAN_POINT ( 'NONE',  ( 5.597778194180000888, 1506.679269386989972, 219.3685102149989916 ) ) ;
#62715 = CARTESIAN_POINT ( 'NONE',  ( -2.330134126628495839, 1515.551704408385831, 205.1377642093399061 ) ) ;
#62717 = EDGE_LOOP ( 'NONE', ( #16101, #78315, #41960, #5663 ) ) ;
#62716 = CARTESIAN_POINT ( 'NONE',  ( -2.873810095670000120, 1489.508126606890073, 188.4097326925989933 ) ) ;
#62718 = CARTESIAN_POINT ( 'NONE',  ( -1.342110535129999782, 1416.822692871130130, 228.0800075106980103 ) ) ;
#62719 = CARTESIAN_POINT ( 'NONE',  ( -3.078458295609999951, 1382.319662484240098, 217.8852017108989969 ) ) ;
#62720 = CARTESIAN_POINT ( 'NONE',  ( -4.301547056329999563, 1475.041466652889994, 199.3382836939389904 ) ) ;
#62722 = ORIENTED_EDGE ( 'NONE', *, *, #85806, .F. ) ;
#62721 = CARTESIAN_POINT ( 'NONE',  ( -32.06248218119481663, 1524.739915903617430, 216.1098515782979064 ) ) ;
#62723 = CARTESIAN_POINT ( 'NONE',  ( -6.236956084921230214, 1508.551704408389924, 219.3822772563589751 ) ) ;
#62724 = ORIENTED_EDGE ( 'NONE', *, *, #4250, .F. ) ;
#62725 = CARTESIAN_POINT ( 'NONE',  ( -11.99567239095710036, 1390.320064639609882, 213.8405493935750030 ) ) ;
#62726 = CARTESIAN_POINT ( 'NONE',  ( -17.97082668629999702, 1416.218047894730262, 209.4769668406679841 ) ) ;
#62727 = CARTESIAN_POINT ( 'NONE',  ( 3.394586470828380165, 1484.752177860970050, 220.4731790445629827 ) ) ;
#62728 = CARTESIAN_POINT ( 'NONE',  ( 3.219589608733330000, 1465.067515351920065, 202.8483799685759834 ) ) ;
#62729 = CARTESIAN_POINT ( 'NONE',  ( -2.059804321870000177, 1432.536759692389978, 218.0320281295389861 ) ) ;
#62730 = CIRCLE ( 'NONE', #5535, 4.014131127992580872 ) ;
#62731 = CARTESIAN_POINT ( 'NONE',  ( 2.470955850358427686, 1523.580204110584191, 242.8749759455148478 ) ) ;
#62732 = CARTESIAN_POINT ( 'NONE',  ( 14.92368822464059974, 1409.434207063760141, 209.5555605250399935 ) ) ;
#62733 = CARTESIAN_POINT ( 'NONE',  ( -7.965935579988510540, 1384.902014119069918, 199.4892638029120064 ) ) ;
#62734 = CARTESIAN_POINT ( 'NONE',  ( -89.28323898676370618, 1385.190482965020010, 292.1241280709670036 ) ) ;
#62736 = EDGE_CURVE ( 'NONE', #9292, #104222, #11601, .T. ) ;
#62735 = EDGE_CURVE ( 'NONE', #8045, #22220, #24030, .T. ) ;
#62737 = CARTESIAN_POINT ( 'NONE',  ( -18.01647495410000133, 1424.182360087930192, 192.6480262483979971 ) ) ;
#62738 = FACE_OUTER_BOUND ( 'NONE', #110355, .T. ) ;
#62739 = CARTESIAN_POINT ( 'NONE',  ( 10.93211270434609972, 1490.535788348610140, 207.1035467188879977 ) ) ;
#62740 = ORIENTED_EDGE ( 'NONE', *, *, #109673, .T. ) ;
#62741 = ORIENTED_EDGE ( 'NONE', *, *, #72026, .F. ) ;
#62742 = ADVANCED_FACE ( 'NONE', ( #33984 ), #99237, .F. ) ;
#62743 = CARTESIAN_POINT ( 'NONE',  ( -11.94034776685189847, 1415.658863692659907, 194.9858853494239952 ) ) ;
#62744 = CARTESIAN_POINT ( 'NONE',  ( -3.329590635812200272, 1495.609068625810096, 197.2492212534749854 ) ) ;
#62745 = AXIS2_PLACEMENT_3D ( 'NONE', #15502, #67604, #84919 ) ;
#62746 = CARTESIAN_POINT ( 'NONE',  ( 35.09256191701995675, 1457.673633888417044, 269.5327811216627083 ) ) ;
#62747 = CARTESIAN_POINT ( 'NONE',  ( 12.11032223851909961, 1427.313662735290109, 207.9400900094899782 ) ) ;
#62748 = CARTESIAN_POINT ( 'NONE',  ( 1.171355130469999839, 1396.015413588030015, 220.7560819512980004 ) ) ;
#62749 = CARTESIAN_POINT ( 'NONE',  ( 31.14814639454048262, 1525.697947650488459, 201.5095775078352460 ) ) ;
#62750 = CARTESIAN_POINT ( 'NONE',  ( 0.2101337101240000060, 1457.272896011530293, 183.0700940124980036 ) ) ;
#62751 = CARTESIAN_POINT ( 'NONE',  ( -9.977700672452339603, 1365.292605733889786, 210.6218459616991936 ) ) ;
#62752 = DIRECTION ( 'NONE',  ( 0.9970203751124365743, 0.07713865185920996959, 0.000000000000000000 ) ) ;
#62753 = CARTESIAN_POINT ( 'NONE',  ( -7.338411997524999286, 1517.170512887980067, 206.6372682748769876 ) ) ;
#62754 = B_SPLINE_CURVE_WITH_KNOTS ( 'NONE', 3,
 ( #36665, #106612, #72482, #2541, #104416, #45646, #79786, #21480, #47271, #3091, #81393, #36120, #27709, #19283, #53485, #104970, #5824, #92023, #83609, #90914, #108821, #74688, #14754, #30458, #31555, #100955, #6363, #83072, #40511, #74139, #32117, #66302, #107166, #64642 ),
 .UNSPECIFIED., .F., .F.,
 ( 4, 3, 3, 3, 3, 3, 3, 3, 3, 3, 3, 4 ),
 ( -1.000000000000000000, -0.9332700196348299171, -0.8419690754577389136, -0.7491820742414060375, -0.6555871093692909879, -0.5609708486710199837, -0.4660560511319400412, -0.3711766688345579102, -0.2766611810049399711, -0.1833255963325950422, -0.09105965716530861620, -9.978666077881115370E-07 ),
 .UNSPECIFIED. ) ;
#62755 = CARTESIAN_POINT ( 'NONE',  ( -13.17405550470000186, 1435.081114633759853, 149.9571693888979951 ) ) ;
#62756 = CARTESIAN_POINT ( 'NONE',  ( 1.121350905119999908, 1416.825532216630108, 190.1588586452979825 ) ) ;
#62757 = CARTESIAN_POINT ( 'NONE',  ( -0.3791074914540970009, 1489.809295140069935, 187.8701616902860110 ) ) ;
#62758 = CARTESIAN_POINT ( 'NONE',  ( 2.236830496430000537, 1495.676457072290077, 221.2569898083989699 ) ) ;
#62759 = CARTESIAN_POINT ( 'NONE',  ( 41.61456305172699643, 1444.048090539929944, 136.0122178056329858 ) ) ;
#62760 = ORIENTED_EDGE ( 'NONE', *, *, #102214, .T. ) ;
#62761 = CARTESIAN_POINT ( 'NONE',  ( 38.63859240729999556, 1428.253853516829849, 261.7057271117980122 ) ) ;
#62762 = CARTESIAN_POINT ( 'NONE',  ( -25.57394744089999961, 1488.682087795429879, 201.8621879095979921 ) ) ;
#62764 = CARTESIAN_POINT ( 'NONE',  ( 3.399097891949999726E-14, 1411.680853644829995, 266.9202418608980452 ) ) ;
#62763 = CARTESIAN_POINT ( 'NONE',  ( -2.553569726430000131, 1507.269243784629907, 180.8456350314980057 ) ) ;
#62765 = B_SPLINE_CURVE_WITH_KNOTS ( 'NONE', 3,
 ( #24549, #42476, #76633, #110785, #59853, #93977, #86688 ),
 .UNSPECIFIED., .F., .F.,
 ( 4, 3, 4 ),
 ( -2.813093253849999975, -1.406546626924999988, 0.000000000000000000 ),
 .UNSPECIFIED. ) ;
#62766 = VECTOR ( 'NONE', #24415, 1000.000000000000114 ) ;
#62767 = DIRECTION ( 'NONE',  ( -0.02617694830785676288, 0.9996573249755578150, 1.483054601246242193E-17 ) ) ;
#62768 = CARTESIAN_POINT ( 'NONE',  ( -31.69751081790000313, 1436.813883499979966, 244.1892870165980014 ) ) ;
#62769 = CARTESIAN_POINT ( 'NONE',  ( 19.55529463106600119, 1509.624433752180039, 231.4241880222230066 ) ) ;
#62770 = CARTESIAN_POINT ( 'NONE',  ( 4.046387026569544076, 1446.994266134431655, 154.8289846805161005 ) ) ;
#62771 = CARTESIAN_POINT ( 'NONE',  ( 33.92643251289999995, 1451.728352207130001, 135.1493744902979870 ) ) ;
#62772 = ORIENTED_EDGE ( 'NONE', *, *, #16455, .T. ) ;
#62773 = CARTESIAN_POINT ( 'NONE',  ( -5.377564849545230174, 1430.035755479769932, 154.3918570002599893 ) ) ;
#62774 = CARTESIAN_POINT ( 'NONE',  ( 16.66936639845653900, 1523.382868172864164, 237.7608804993219280 ) ) ;
#62775 = CARTESIAN_POINT ( 'NONE',  ( 16.19087789078229989, 1409.478458302130093, 193.2334102746530107 ) ) ;
#62776 = ORIENTED_EDGE ( 'NONE', *, *, #63941, .T. ) ;
#62777 = ORIENTED_EDGE ( 'NONE', *, *, #81579, .F. ) ;
#62778 = B_SPLINE_CURVE_WITH_KNOTS ( 'NONE', 3,
 ( #26726, #95043, #35680, #19420, #69871, #18312, #96142 ),
 .UNSPECIFIED., .F., .F.,
 ( 4, 3, 4 ),
 ( -9.215058517400001037, -7.151230857792230111, -3.489946704171289937 ),
 .UNSPECIFIED. ) ;
#62779 = CARTESIAN_POINT ( 'NONE',  ( 8.977953201188558552, 1452.688148568789984, 212.1107650675139951 ) ) ;
#62780 = CARTESIAN_POINT ( 'NONE',  ( -23.02675208173420174, 1409.747009289400012, 208.9090590340030076 ) ) ;
#62781 = VERTEX_POINT ( 'NONE', #96100 ) ;
#62782 = CARTESIAN_POINT ( 'NONE',  ( -3.068245697174119879, 1507.352576251979826, 221.6096153556280228 ) ) ;
#62783 = LINE ( 'NONE', #20169, #43809 ) ;
#62784 = AXIS2_PLACEMENT_3D ( 'NONE', #3851, #38512, #30105 ) ;
#62785 = CARTESIAN_POINT ( 'NONE',  ( 0.3570154777189999962, 1451.680777065829943, 183.0662967611979752 ) ) ;
#62786 = CARTESIAN_POINT ( 'NONE',  ( -2.007783359929999900, 1479.773924900330030, 235.8303969823979855 ) ) ;
#62787 = CARTESIAN_POINT ( 'NONE',  ( -113.4000000000000057, 1378.528619065190014, 304.2218459572590064 ) ) ;
#62788 = VERTEX_POINT ( 'NONE', #103377 ) ;
#62789 = CARTESIAN_POINT ( 'NONE',  ( 11.15477664960000048, 1425.160652183429875, 144.1598853320980140 ) ) ;
#62790 = CARTESIAN_POINT ( 'NONE',  ( 19.33983739529999824, 1457.046864427589981, 207.2645132519189985 ) ) ;
#62791 = CARTESIAN_POINT ( 'NONE',  ( 14.41941774000000009, 1474.742523832529969, 225.1206985227979942 ) ) ;
#62792 = ORIENTED_EDGE ( 'NONE', *, *, #41949, .F. ) ;
#62793 = CARTESIAN_POINT ( 'NONE',  ( -7.334328310795000583, 1517.005755693489846, 204.1179978101270081 ) ) ;
#62794 = AXIS2_PLACEMENT_3D ( 'NONE', #50643, #84772, #8070 ) ;
#62795 = ORIENTED_EDGE ( 'NONE', *, *, #5805, .F. ) ;
#62796 = CARTESIAN_POINT ( 'NONE',  ( 11.86283928301630120, 1432.108153224739908, 149.9775622573939984 ) ) ;
#62797 = CARTESIAN_POINT ( 'NONE',  ( 12.75800579317462891, 1444.997181870303393, 186.4738022370279396 ) ) ;
#62798 = EDGE_LOOP ( 'NONE', ( #55338, #96837 ) ) ;
#62799 = ORIENTED_EDGE ( 'NONE', *, *, #71313, .F. ) ;
#62800 = CARTESIAN_POINT ( 'NONE',  ( 31.12456774391174719, 1525.960063244516959, 201.1524202391562710 ) ) ;
#62801 = FACE_OUTER_BOUND ( 'NONE', #26944, .T. ) ;
#62802 = CARTESIAN_POINT ( 'NONE',  ( 5.854932897769000277, 1498.860406282120039, 199.1309772468239885 ) ) ;
#62803 = AXIS2_PLACEMENT_3D ( 'NONE', #34564, #18298, #42979 ) ;
#62804 = CARTESIAN_POINT ( 'NONE',  ( -10.29448394224809959, 1469.837462831460016, 213.9188779471319890 ) ) ;
#62805 = CARTESIAN_POINT ( 'NONE',  ( 19.21825364151619908, 1452.241944181910185, 144.1553783344959925 ) ) ;
#62806 = CARTESIAN_POINT ( 'NONE',  ( 0.9556514315352180322, 1409.785933179500034, 270.0714045367960239 ) ) ;
#62807 = DIRECTION ( 'NONE',  ( 0.8775825618903763115, 0.000000000000000000, 0.4794255386041965106 ) ) ;
#62808 = DIRECTION ( 'NONE',  ( -9.020562075079389318E-14, 0.000000000000000000, 1.000000000000000000 ) ) ;
#62809 = CARTESIAN_POINT ( 'NONE',  ( 9.090063749209999600, 1493.398504240489956, 216.3232041073590040 ) ) ;
#62810 = CARTESIAN_POINT ( 'NONE',  ( 11.16991425404440008, 1478.699414125650037, 205.8835566445779932 ) ) ;
#62811 = CARTESIAN_POINT ( 'NONE',  ( 9.152530698324561342, 1425.159826229013106, 195.6020820322053737 ) ) ;
#62813 = CARTESIAN_POINT ( 'NONE',  ( 14.15593876370000004, 1435.008643399779885, 195.7735139947980088 ) ) ;
#62812 = CARTESIAN_POINT ( 'NONE',  ( -12.76080126299999939, 1502.832725690589996, 208.7536821347480043 ) ) ;
#62814 = CARTESIAN_POINT ( 'NONE',  ( -11.75869035456349998, 1521.951704408389787, 190.9442076542370046 ) ) ;
#62815 =( REPRESENTATION_RELATIONSHIP ('NONE','NONE', #14372, #49395 ) REPRESENTATION_RELATIONSHIP_WITH_TRANSFORMATION ( #9006 )SHAPE_REPRESENTATION_RELATIONSHIP( ) );
#62816 = CIRCLE ( 'NONE', #28803, 2.000000000000003553 ) ;
#62817 = CARTESIAN_POINT ( 'NONE',  ( -9.927113458974829996, 1439.694740119939979, 207.9119407081149973 ) ) ;
#62818 = B_SPLINE_CURVE_WITH_KNOTS ( 'NONE', 5,
 ( #43795, #53890, #704, #77946, #60064, #51650 ),
 .UNSPECIFIED., .F., .F.,
 ( 6, 6 ),
 ( -0.9267553667292389719, 5.517427126029999407 ),
 .UNSPECIFIED. ) ;
#62819 = CARTESIAN_POINT ( 'NONE',  ( -6.911190420815000124, 1512.677556571440164, 201.0605893814370120 ) ) ;
#62820 = EDGE_LOOP ( 'NONE', ( #75391, #32683, #106773, #12710 ) ) ;
#62821 = CARTESIAN_POINT ( 'NONE',  ( 28.02005515429999960, 1437.694013773219922, 248.0989693021979861 ) ) ;
#62822 = CARTESIAN_POINT ( 'NONE',  ( 18.63787275302323465, 1508.244465050627696, 188.4525138201056507 ) ) ;
#62823 = CARTESIAN_POINT ( 'NONE',  ( -66.03229317983959845, 1385.039105777579834, 290.1674623452569790 ) ) ;
#62824 = CARTESIAN_POINT ( 'NONE',  ( -7.445038021963170216, 1508.731359867031642, 214.6352815288127545 ) ) ;
#62825 = CARTESIAN_POINT ( 'NONE',  ( 3.628818059389999906, 1505.602008401590183, 221.3635115024989943 ) ) ;
#62826 = CARTESIAN_POINT ( 'NONE',  ( -14.60558100029999906, 1415.677402203979909, 212.8314178026089962 ) ) ;
#62828 = ORIENTED_EDGE ( 'NONE', *, *, #30904, .F. ) ;
#62827 = CARTESIAN_POINT ( 'NONE',  ( -16.14632490511739960, 1420.004730576690008, 210.0172707792249867 ) ) ;
#62829 = CARTESIAN_POINT ( 'NONE',  ( -15.81740104567429661, 1415.848495208088252, 209.7113497446936776 ) ) ;
#62830 = CIRCLE ( 'NONE', #53868, 2.000000000000003109 ) ;
#62832 = B_SPLINE_CURVE_WITH_KNOTS ( 'NONE', 5,
 ( #102763, #52414, #60254, #87662, #105006, #26628 ),
 .UNSPECIFIED., .F., .F.,
 ( 6, 6 ),
 ( -2.079987011550000098, 0.000000000000000000 ),
 .UNSPECIFIED. ) ;
#62831 = CARTESIAN_POINT ( 'NONE',  ( -10.07154918488590134, 1473.228065907060000, 207.4129428866500007 ) ) ;
#62833 = CARTESIAN_POINT ( 'NONE',  ( -16.11828785200000169, 1416.352749337680279, 209.2475168326350001 ) ) ;
#62835 = ADVANCED_FACE ( 'NONE', ( #27797 ), #109138, .F. ) ;
#62834 = CARTESIAN_POINT ( 'NONE',  ( -16.16632277704758280, 1512.187213306747481, 236.8966194768525497 ) ) ;
#62836 = CARTESIAN_POINT ( 'NONE',  ( 14.49215842413499900, 1514.088841912139969, 225.6376920165670015 ) ) ;
#62837 = DIRECTION ( 'NONE',  ( -1.224646799147350002E-16, 1.836970198721029688E-16, 1.000000000000000000 ) ) ;
#62838 = CARTESIAN_POINT ( 'NONE',  ( 27.28440919872599935, 1509.865850533680032, 222.5516304213150249 ) ) ;
#62839 = DIRECTION ( 'NONE',  ( 0.000000000000000000, 0.000000000000000000, -1.000000000000000000 ) ) ;
#62840 = DIRECTION ( 'NONE',  ( 1.755985294532464991E-16, -1.000000000000000000, 1.338183447452830017E-16 ) ) ;
#62841 = CARTESIAN_POINT ( 'NONE',  ( 14.74268596870000003, 1415.084640305229868, 227.8479518795979857 ) ) ;
#62842 = CARTESIAN_POINT ( 'NONE',  ( -7.980162432014145324, 1424.804287484062115, 210.5240428484218853 ) ) ;
#62843 = CARTESIAN_POINT ( 'NONE',  ( -17.15058533566899968, 1460.897024810804169, 228.2718108823579826 ) ) ;
#62844 = CARTESIAN_POINT ( 'NONE',  ( 4.608021669135000664, 1516.660388280709867, 207.4085285224269910 ) ) ;
#62845 = CARTESIAN_POINT ( 'NONE',  ( 45.27970250219999571, 1434.949994644049866, 268.7737451221979654 ) ) ;
#62846 = CARTESIAN_POINT ( 'NONE',  ( -17.82654646940000021, 1409.700512582729971, 223.9827240008980027 ) ) ;
#62847 = CARTESIAN_POINT ( 'NONE',  ( 15.62192944049999888, 1435.060616691779842, 147.8543328025979804 ) ) ;
#62848 = AXIS2_PLACEMENT_3D ( 'NONE', #19822, #1385, #54029 ) ;
#62849 = CARTESIAN_POINT ( 'NONE',  ( 20.25069675820000015, 1488.587216004930042, 190.8938461704979943 ) ) ;
#62850 = CARTESIAN_POINT ( 'NONE',  ( -16.66259792569089981, 1410.427225285170152, 191.7596848084640158 ) ) ;
#62851 = ADVANCED_FACE ( 'NONE', ( #42772 ), #6231, .T. ) ;
#62852 = CARTESIAN_POINT ( 'NONE',  ( -12.30462497340020001, 1377.683743082049887, 208.6098874196279951 ) ) ;
#62853 = CARTESIAN_POINT ( 'NONE',  ( -18.29970625680000040, 1473.000870360929866, 266.8291869051980143 ) ) ;
#62854 = CARTESIAN_POINT ( 'NONE',  ( -14.91495772972460010, 1417.818891793210014, 203.2118081904590099 ) ) ;
#62855 =( BOUNDED_SURFACE ( )  B_SPLINE_SURFACE ( 3, 2, ( 
 ( #42434, #7728, #8269 ),
 ( #44522, #34035, #101771 ),
 ( #25062, #76592, #100677 ),
 ( #109110, #32390, #52930 ) ),
 .UNSPECIFIED., .F., .F., .T. ) 
 B_SPLINE_SURFACE_WITH_KNOTS ( ( 4, 4 ),
 ( 3, 3 ),
 ( 0.000000000000000000, 0.0002960034161023848936 ),
 ( 0.000000000000000000, 1.000000000000000000 ),
 .UNSPECIFIED. ) 
 GEOMETRIC_REPRESENTATION_ITEM ( )  RATIONAL_B_SPLINE_SURFACE ( (
 ( 1.000000000000000000, 0.8072480644198108957, 1.000000000000000000),
 ( 1.000000000000000000, 0.8072480346917760841, 1.000000000000000000),
 ( 1.000000000000000000, 0.8071723757218336459, 1.000000000000000000),
 ( 1.000000000000000000, 0.8070209408750045332, 1.000000000000000000) ) ) 
 REPRESENTATION_ITEM ( '' )  SURFACE ( )  );
#62856 = PLANE ( 'NONE',  #24118 ) ;
#62857 = DIRECTION ( 'NONE',  ( 1.000000000000000000, -2.740606396879999932E-15, 3.772597702940000410E-15 ) ) ;
#62858 = CARTESIAN_POINT ( 'NONE',  ( -16.31825947160000112, 1416.692283692869978, 208.5165952855510056 ) ) ;
#62859 = CARTESIAN_POINT ( 'NONE',  ( -12.06734954289999884, 1442.226007087160042, 187.2421031291980000 ) ) ;
#62860 = EDGE_CURVE ( 'NONE', #69308, #27986, #29406, .T. ) ;
#62861 = CARTESIAN_POINT ( 'NONE',  ( -27.90835392674980042, 1508.762510115379882, 210.5978890894100175 ) ) ;
#62862 = CARTESIAN_POINT ( 'NONE',  ( 11.87595595069999987, 1433.006363244350268, 146.4341592748980077 ) ) ;
#62863 = CARTESIAN_POINT ( 'NONE',  ( -30.21734179830000144, 1436.028192106169854, 136.4151164768979925 ) ) ;
#62864 = CARTESIAN_POINT ( 'NONE',  ( -15.46337246819999933, 1416.177402202029953, 209.5778879521189992 ) ) ;
#62865 = ORIENTED_EDGE ( 'NONE', *, *, #104723, .F. ) ;
#62866 = CARTESIAN_POINT ( 'NONE',  ( -3.367054167445000079, 1511.558654537720031, 201.2679619493769962 ) ) ;
#62867 = CARTESIAN_POINT ( 'NONE',  ( -5.774656115207120521, 1409.114715822440075, 222.9363759656519903 ) ) ;
#62868 = CARTESIAN_POINT ( 'NONE',  ( 33.14208818188970440, 1524.841055067849311, 197.8283574329067562 ) ) ;
#62869 = CARTESIAN_POINT ( 'NONE',  ( -12.76561250770870082, 1508.446853715159932, 209.6296519742829787 ) ) ;
#62870 = CARTESIAN_POINT ( 'NONE',  ( -37.71859155314457013, 1442.773887286370382, 136.8575361162813238 ) ) ;
#62871 = CARTESIAN_POINT ( 'NONE',  ( -46.05260025390000322, 1446.035358659930125, 266.6770541026980368 ) ) ;
#62872 = CARTESIAN_POINT ( 'NONE',  ( -16.37398935204720019, 1478.527142925449880, 223.3409276542839734 ) ) ;
#62873 = CARTESIAN_POINT ( 'NONE',  ( 0.1601292279041169886, 1420.232911783010195, 183.6671598589649932 ) ) ;
#62874 = CARTESIAN_POINT ( 'NONE',  ( -27.34968394090000032, 1509.645410702830077, 214.2836711016779816 ) ) ;
#62875 = CARTESIAN_POINT ( 'NONE',  ( -84.46369479308390282, 1384.629619117830089, 306.4275599946969919 ) ) ;
#62876 = CARTESIAN_POINT ( 'NONE',  ( -48.75929104102600320, 1385.014805441129965, 223.3784622248080041 ) ) ;
#62877 = STYLED_ITEM ( 'NONE', ( #107750 ), #13206 ) ;
#62878 = CARTESIAN_POINT ( 'NONE',  ( -5.069242052572500157, 1375.174993499499806, 214.7429053951260016 ) ) ;
#62879 = CARTESIAN_POINT ( 'NONE',  ( 16.05891525850000079, 1416.823418193329871, 217.6350310302879905 ) ) ;
#62880 = CARTESIAN_POINT ( 'NONE',  ( 18.11157395349999888, 1509.545530486529969, 186.5307135875980009 ) ) ;
#62881 = FACE_OUTER_BOUND ( 'NONE', #87056, .T. ) ;
#62883 = ORIENTED_EDGE ( 'NONE', *, *, #69860, .F. ) ;
#62882 = CARTESIAN_POINT ( 'NONE',  ( 4.045201229639999951, 1515.528102034789981, 207.6334507866089893 ) ) ;
#62884 = CARTESIAN_POINT ( 'NONE',  ( -3.535396145210000007, 1507.776748965729894, 180.9473349428980100 ) ) ;
#62885 = CARTESIAN_POINT ( 'NONE',  ( -24.02116941819999951, 1411.112860734130209, 208.3416100540740103 ) ) ;
#62887 = EDGE_CURVE ( 'NONE', #94000, #61499, #97435, .T. ) ;
#62886 = AXIS2_PLACEMENT_3D ( 'NONE', #14392, #91666, #101150 ) ;
#62888 = DIRECTION ( 'NONE',  ( 0.7414773880254711402, 0.000000000000000000, 0.6709778558543678662 ) ) ;
#62889 = CARTESIAN_POINT ( 'NONE',  ( -11.41983032799999975, 1415.048591094029916, 195.6129360477979731 ) ) ;
#62890 = CARTESIAN_POINT ( 'NONE',  ( 0.2516559519770019682, 1422.814445642939972, 192.8915334538990010 ) ) ;
#62891 = CARTESIAN_POINT ( 'NONE',  ( 22.42609733799999816, 1409.696196963129978, 212.0712440230379912 ) ) ;
#62892 = CARTESIAN_POINT ( 'NONE',  ( -12.17235240719999823, 1434.042297368109985, 149.7137827380979900 ) ) ;
#62893 = CARTESIAN_POINT ( 'NONE',  ( 10.75633763354679928, 1451.138011284190043, 190.3409219236589820 ) ) ;
#62894 = FACE_OUTER_BOUND ( 'NONE', #37859, .T. ) ;
#62896 = CARTESIAN_POINT ( 'NONE',  ( -11.17264282910000084, 1380.903189564030072, 202.7795052211189955 ) ) ;
#62895 = CARTESIAN_POINT ( 'NONE',  ( -113.4000000000000057, 1309.713060387289943, 304.2218459572590064 ) ) ;
#62897 = CARTESIAN_POINT ( 'NONE',  ( -0.1099389607409999997, 1413.018602985929874, 233.3789693115979844 ) ) ;
#62898 = CARTESIAN_POINT ( 'NONE',  ( 3.074703616360000336, 1441.333178363689967, 218.5515150763889949 ) ) ;
#62899 = CARTESIAN_POINT ( 'NONE',  ( -2201.413669186790685, 11221.53578756870047, 1941.356037698088358 ) ) ;
#62900 = DIRECTION ( 'NONE',  ( -5.980589973904019347E-17, 1.000000000000000000, -1.736889445713099699E-16 ) ) ;
#62901 = CARTESIAN_POINT ( 'NONE',  ( -8.962252599310000178, 1366.920250605820002, 210.6218459616991936 ) ) ;
#62902 = CIRCLE ( 'NONE', #66471, 1.000000000000002442 ) ;
#62903 = CARTESIAN_POINT ( 'NONE',  ( -1.713317447804999949, 1516.660388280709867, 204.5138242629670060 ) ) ;
#62904 = CARTESIAN_POINT ( 'NONE',  ( 13.37364840053160187, 1507.560048672190078, 233.0513862518880046 ) ) ;
#62905 = CARTESIAN_POINT ( 'NONE',  ( -18.13105147114099935, 1486.178406859650067, 188.5764279912840209 ) ) ;
#62906 = CARTESIAN_POINT ( 'NONE',  ( -9.215151402819998339, 1422.993424535609847, 210.2744618676390189 ) ) ;
#62907 = CARTESIAN_POINT ( 'NONE',  ( -10.61736893638143187, 1422.368802841423076, 210.6403487152534240 ) ) ;
#62909 = VERTEX_POINT ( 'NONE', #28176 ) ;
#62908 = CARTESIAN_POINT ( 'NONE',  ( -67.98270077001589584, 1379.746359850080125, 279.4236968873279920 ) ) ;
#62910 = ORIENTED_EDGE ( 'NONE', *, *, #51819, .T. ) ;
#62911 = CARTESIAN_POINT ( 'NONE',  ( 27.73048959930000024, 1508.610947985129997, 212.2558594092780027 ) ) ;
#62912 = ORIENTED_EDGE ( 'NONE', *, *, #90736, .T. ) ;
#62913 = CARTESIAN_POINT ( 'NONE',  ( 0.4444123522354649358, 1457.844269246920703, 199.5878175327990505 ) ) ;
#62914 = CARTESIAN_POINT ( 'NONE',  ( -10.61999665778870039, 1462.990853173620053, 206.0510134237090085 ) ) ;
#62916 = CARTESIAN_POINT ( 'NONE',  ( 15.76697546804739858, 1409.471978965290191, 192.7550041694750007 ) ) ;
#62915 = CARTESIAN_POINT ( 'NONE',  ( -3.677837710089999800E-15, 1426.566393376330097, 144.1938086916980239 ) ) ;
#62917 = CARTESIAN_POINT ( 'NONE',  ( 8.768196648836839913, 1461.433371597579935, 227.1471525255139738 ) ) ;
#62918 = CIRCLE ( 'NONE', #89623, 2.000000000000023537 ) ;
#62919 = CARTESIAN_POINT ( 'NONE',  ( -24.43436514662279890, 1452.059797509780083, 135.9947029744789972 ) ) ;
#62920 = CARTESIAN_POINT ( 'NONE',  ( 10.69300205652376690, 1438.695736345125624, 152.5084499697617559 ) ) ;
#62921 = CARTESIAN_POINT ( 'NONE',  ( 12.52547985540000042, 1410.283479796730035, 228.7537008404979986 ) ) ;
#62922 = PRESENTATION_STYLE_ASSIGNMENT (( #46641 ) ) ;
#62923 = CARTESIAN_POINT ( 'NONE',  ( 3.461047291624999911, 1516.858765657450249, 212.5691103191969944 ) ) ;
#62924 = CARTESIAN_POINT ( 'NONE',  ( 41.46889560158410148, 1441.954934106449855, 134.0999999980859911 ) ) ;
#62925 = CARTESIAN_POINT ( 'NONE',  ( 17.16388877745072605, 1523.678648413191695, 238.6174304775213386 ) ) ;
#62926 = ORIENTED_EDGE ( 'NONE', *, *, #95207, .F. ) ;
#62927 = CARTESIAN_POINT ( 'NONE',  ( 10.37958320015649960, 1453.090533085269954, 190.0119578831939862 ) ) ;
#62928 = CARTESIAN_POINT ( 'NONE',  ( -2.306705840230210303, 1431.167757009700154, 201.0655358790060063 ) ) ;
#62929 = VERTEX_POINT ( 'NONE', #44440 ) ;
#62930 = ORIENTED_EDGE ( 'NONE', *, *, #77871, .F. ) ;
#62931 = VERTEX_POINT ( 'NONE', #10834 ) ;
#62932 = CARTESIAN_POINT ( 'NONE',  ( -8.526415774054999730, 1512.074228085009963, 215.5845765956869968 ) ) ;
#62933 = CARTESIAN_POINT ( 'NONE',  ( 32.85805783624308418, 1523.678648413191695, 217.1983043299902931 ) ) ;
#62934 = CARTESIAN_POINT ( 'NONE',  ( 14.09811198787718389, 1451.182526868617742, 150.3098712486240345 ) ) ;
#62935 = CARTESIAN_POINT ( 'NONE',  ( 0.000000000000000000, 1519.913060387329779, 209.1218459616979999 ) ) ;
#62936 = CARTESIAN_POINT ( 'NONE',  ( 9.739858402530000347, 1462.441346130390002, 208.6777580896069821 ) ) ;
#62937 = VECTOR ( 'NONE', #44347, 1000.000000000000000 ) ;
#62938 = CARTESIAN_POINT ( 'NONE',  ( -19.09790268268400126, 1508.458003811930212, 210.0050661408479868 ) ) ;
#62939 = CARTESIAN_POINT ( 'NONE',  ( -66.35507711686996402, 1379.742713900610170, 275.1017064096059812 ) ) ;
#62940 = CARTESIAN_POINT ( 'NONE',  ( 3.194002131880000039, 1466.133465350190136, 198.9725194175989884 ) ) ;
#62941 = CARTESIAN_POINT ( 'NONE',  ( 1.118067181730000081, 1508.368074802429874, 237.6116800887979821 ) ) ;
#62942 = EDGE_LOOP ( 'NONE', ( #2436, #25936, #13400, #105930 ) ) ;
#62943 = CARTESIAN_POINT ( 'NONE',  ( 6.546039395294999785, 1516.565291103010168, 206.8289057630870218 ) ) ;
#62944 = VERTEX_POINT ( 'NONE', #106533 ) ;
#62945 = CARTESIAN_POINT ( 'NONE',  ( 23.39958255221609917, 1440.913060387330006, 233.3680888324570049 ) ) ;
#62946 = CARTESIAN_POINT ( 'NONE',  ( -16.42304823919999990, 1508.244897181629995, 185.8512656781980183 ) ) ;
#62947 = ORIENTED_EDGE ( 'NONE', *, *, #7744, .F. ) ;
#62948 = CARTESIAN_POINT ( 'NONE',  ( 26.97427084300169753, 1450.930614134690131, 136.4066763474399977 ) ) ;
#62949 = CARTESIAN_POINT ( 'NONE',  ( -14.76096091410000000, 1409.595176565530210, 191.2496112059980078 ) ) ;
#62950 = CARTESIAN_POINT ( 'NONE',  ( -63.28909092007827297, 1379.735398356163614, 271.9840329659873532 ) ) ;
#62952 = CARTESIAN_POINT ( 'NONE',  ( 6.768931359969999839, 1468.810414808390078, 208.2491176551630190 ) ) ;
#62951 = CARTESIAN_POINT ( 'NONE',  ( -24.41204057910000103, 1440.938895779720042, 212.0297384891179888 ) ) ;
#62953 = CARTESIAN_POINT ( 'NONE',  ( -9.115524708650340813, 1437.332156617270130, 212.8456964132400060 ) ) ;
#62954 = CARTESIAN_POINT ( 'NONE',  ( 15.70021604296872830, 1414.913060387330006, 214.2279672958994183 ) ) ;
#62955 = CARTESIAN_POINT ( 'NONE',  ( -1.417434298042890006, 1448.552296757619843, 227.8906923748210147 ) ) ;
#62956 = CARTESIAN_POINT ( 'NONE',  ( 21.04904418909999819, 1494.916427559390058, 209.1218459616989946 ) ) ;
#62957 = CARTESIAN_POINT ( 'NONE',  ( -2.302358205750000053, 1507.635233240290063, 221.1829251670990004 ) ) ;
#62959 = CARTESIAN_POINT ( 'NONE',  ( 8.062587302181759341, 1436.235894220949831, 206.1282943059349861 ) ) ;
#62958 = CARTESIAN_POINT ( 'NONE',  ( 4.477818878069999897, 1465.350087406130115, 234.1438911684979871 ) ) ;
#62960 = CARTESIAN_POINT ( 'NONE',  ( -2.290256301855000398, 1517.170721208160103, 216.0730210990169837 ) ) ;
#62961 = CARTESIAN_POINT ( 'NONE',  ( -2.469061732649111107, 1524.816846803860926, 242.3846597971397330 ) ) ;
#62962 = CARTESIAN_POINT ( 'NONE',  ( 5.730039660753280195, 1510.523965798400013, 216.6735546448169885 ) ) ;
#62963 = LINE ( 'NONE', #78613, #65875 ) ;
#62964 = CARTESIAN_POINT ( 'NONE',  ( 5.786837678925000006, 1517.040132827679827, 212.3790665729270017 ) ) ;
#62965 = CARTESIAN_POINT ( 'NONE',  ( 4.325403553846939531, 1515.219291385629958, 211.4517448047639903 ) ) ;
#62966 = CARTESIAN_POINT ( 'NONE',  ( -9.239806556520379743, 1384.978503770619909, 197.9483252412619834 ) ) ;
#62968 = EDGE_LOOP ( 'NONE', ( #47537, #38455, #17805, #40428 ) ) ;
#62967 = CARTESIAN_POINT ( 'NONE',  ( 3.487586588140600075, 1508.731366866819826, 213.6768007754070027 ) ) ;
#62969 = CARTESIAN_POINT ( 'NONE',  ( -17.59789087267267504, 1524.659148609482827, 237.5602248788992767 ) ) ;
#62970 = CARTESIAN_POINT ( 'NONE',  ( 29.79081509959999607, 1446.796541106770064, 240.1465591158980146 ) ) ;
#62971 = CARTESIAN_POINT ( 'NONE',  ( -11.30248206070000094, 1432.393890462980153, 151.5218268353980022 ) ) ;
#62972 = CARTESIAN_POINT ( 'NONE',  ( -14.56647635000000029, 1415.677402202029953, 205.6923038026590120 ) ) ;
#62973 = CARTESIAN_POINT ( 'NONE',  ( 2.669715429490000069, 1413.149521960129960, 231.7915367626979730 ) ) ;
#62974 = CARTESIAN_POINT ( 'NONE',  ( -19.33162846839999816, 1457.452151859230071, 226.3466835555979912 ) ) ;
#62975 = CIRCLE ( 'NONE', #103996, 1.000000000000000666 ) ;
#62977 = LINE ( 'NONE', #97089, #47956 ) ;
#62976 = CARTESIAN_POINT ( 'NONE',  ( 11.30116471560000058, 1432.303966848209939, 151.5220940858980043 ) ) ;
#62978 = CARTESIAN_POINT ( 'NONE',  ( -8.557209110492459914, 1448.617779613390212, 212.3361752075699940 ) ) ;
#62980 = B_SPLINE_CURVE_WITH_KNOTS ( 'NONE', 5,
 ( #71385, #97643, #56188, #72458, #39384, #4683 ),
 .UNSPECIFIED., .F., .F.,
 ( 6, 6 ),
 ( 0.000000000000000000, 1.000000000000000000 ),
 .UNSPECIFIED. ) ;
#62979 = CARTESIAN_POINT ( 'NONE',  ( -106.7799791470000059, 1379.928168464490000, 308.6026344867590296 ) ) ;
#62981 = ORIENTED_EDGE ( 'NONE', *, *, #47307, .T. ) ;
#62982 = CARTESIAN_POINT ( 'NONE',  ( -3.266349512195000138, 1516.797038924770050, 205.0935381919470046 ) ) ;
#62983 = CARTESIAN_POINT ( 'NONE',  ( 0.7748160517030000527, 1405.993929547030120, 266.9609161638979913 ) ) ;
#62984 = CARTESIAN_POINT ( 'NONE',  ( -0.7508624519220009619, 1515.469918561789882, 213.3394464563290001 ) ) ;
#62985 = CARTESIAN_POINT ( 'NONE',  ( 13.02735688232990086, 1471.728350752560118, 270.3681568976120388 ) ) ;
#62986 = CARTESIAN_POINT ( 'NONE',  ( 2.478578393939999902, 1437.039673764719964, 157.6668020507979975 ) ) ;
#62987 = CARTESIAN_POINT ( 'NONE',  ( 11.60004869885203682, 1423.972964970261728, 135.9380568969748708 ) ) ;
#62988 = AXIS2_PLACEMENT_3D ( 'NONE', #74518, #108649, #73959 ) ;
#62989 = CARTESIAN_POINT ( 'NONE',  ( -38.68338032125110004, 1440.913060393820160, 257.3519283540039737 ) ) ;
#62990 = CARTESIAN_POINT ( 'NONE',  ( 36.00227838366810573, 1442.549544120750170, 137.1411661020360100 ) ) ;
#62991 = CARTESIAN_POINT ( 'NONE',  ( 2.440646991155576373, 1449.387360343648879, 154.4793733419271859 ) ) ;
#62992 = B_SPLINE_CURVE_WITH_KNOTS ( 'NONE', 3,
 ( #1638, #68849, #77780, #27926, #95130, #60440, #1090, #52036, #94558, #10016, #26252, #11674, #71066, #27367, #78326, #86725, #78897, #105188, #35776, #9465, #61549, #2203, #18948, #35216, #20064, #69402, #18392, #70514, #26817, #102951, #53143, #10576, #104072, #44747, #36317, #104629, #17833, #53714, #52591, #69958 ),
 .UNSPECIFIED., .F., .F.,
 ( 4, 2, 2, 2, 1, 1, 2, 2, 2, 2, 1, 1, 1, 2, 2, 2, 2, 1, 1, 1, 2, 2, 2, 4 ),
 ( 0.000000000000000000, 0.1249999999996785072, 0.1874999999995110578, 0.2187499999994365618, 0.2343749999994061695, 0.2421874999993911537, 0.2460937499993812727, 0.2499999999993713917, 0.3749999999997545297, 0.4374999999999461542, 0.4687500000000272005, 0.4843750000000677236, 0.4921875000000839329, 0.4960937500000920375, 0.5000000000001001421, 0.6250000000007530643, 0.6875000000010847989, 0.7187500000012642110, 0.7343750000013491430, 0.7421875000013915535, 0.7460937500014258594, 0.7500000000014600543, 0.8750000000007300827, 1.000000000000000000 ),
 .UNSPECIFIED. ) ;
#62993 = CARTESIAN_POINT ( 'NONE',  ( -0.2087337655829990257, 1432.232251408790034, 200.6786074516889755 ) ) ;
#62994 = CARTESIAN_POINT ( 'NONE',  ( 0.8729611875899290219, 1450.882575902080134, 154.5162442169400094 ) ) ;
#62995 = CARTESIAN_POINT ( 'NONE',  ( 3.035243144599999887, 1506.705827820389914, 220.5430297552989884 ) ) ;
#62996 = DIRECTION ( 'NONE',  ( 0.000000000000000000, 0.7071067811865198172, -0.7071067811865753283 ) ) ;
#62997 =( BOUNDED_SURFACE ( )  B_SPLINE_SURFACE ( 3, 2, ( 
 ( #35066, #76517, #2049 ),
 ( #25543, #397, #87130 ),
 ( #77630, #93853, #68694 ),
 ( #10419, #44589, #102798 ),
 ( #51886, #86022, #78734 ),
 ( #70365, #9323, #941 ),
 ( #69247, #103355, #94981 ),
 ( #18249, #9865, #80940 ),
 ( #21556, #28330, #29418 ),
 ( #11535, #87700, #3158 ),
 ( #45709, #89882, #12073 ),
 ( #62522, #4770, #88242 ),
 ( #71481, #28885, #70925 ),
 ( #20454, #13152, #4238 ) ),
 .UNSPECIFIED., .F., .F., .T. ) 
 B_SPLINE_SURFACE_WITH_KNOTS ( ( 4, 2, 2, 2, 2, 2, 4 ),
 ( 3, 3 ),
 ( 2.840609691912021617E-17, 0.0009443072508236019296, 0.001416460876235388746, 0.001888614501647175453, 0.002360768127058962378, 0.002832921752470748868, 0.003777229003294322283 ),
 ( 0.000000000000000000, 1.000000000000000000 ),
 .UNSPECIFIED. ) 
 GEOMETRIC_REPRESENTATION_ITEM ( )  RATIONAL_B_SPLINE_SURFACE ( (
 ( 1.000000000000000000, 0.9376006582765943342, 1.000000000000000000),
 ( 1.000000000000000000, 0.9283977714735285325, 1.000000000000000000),
 ( 1.000000000000000000, 0.9189750060481984839, 1.000000000000000000),
 ( 1.000000000000000000, 0.9042792056126492950, 1.000000000000000000),
 ( 1.000000000000000000, 0.8992469033843993875, 1.000000000000000000),
 ( 1.000000000000000000, 0.8891280264681499235, 1.000000000000000000),
 ( 1.000000000000000000, 0.8840337471677424119, 1.000000000000000000),
 ( 1.000000000000000000, 0.8736395124161377979, 1.000000000000000000),
 ( 1.000000000000000000, 0.8683406746559806377, 1.000000000000000000),
 ( 1.000000000000000000, 0.8573361860700633441, 1.000000000000000000),
 ( 1.000000000000000000, 0.8516508399499709281, 1.000000000000000000),
 ( 1.000000000000000000, 0.8340914917059080169, 1.000000000000000000),
 ( 1.000000000000000000, 0.8215597275867274618, 1.000000000000000000),
 ( 1.000000000000000000, 0.8070209408750123048, 1.000000000000000000) ) ) 
 REPRESENTATION_ITEM ( '' )  SURFACE ( )  );
#62998 = ORIENTED_EDGE ( 'NONE', *, *, #38623, .F. ) ;
#62999 = CARTESIAN_POINT ( 'NONE',  ( -5.757839681930000175, 1413.763055107629953, 262.6648722463980334 ) ) ;
#63000 = DIRECTION ( 'NONE',  ( 0.000000000000000000, 0.000000000000000000, 1.000000000000000000 ) ) ;
#63001 = CARTESIAN_POINT ( 'NONE',  ( -0.7721454155100000438, 1475.556447494730037, 269.2944986523980333 ) ) ;
#63002 = CARTESIAN_POINT ( 'NONE',  ( -4.282859847165069844, 1446.856630987190101, 156.0743107980160005 ) ) ;
#63003 = CARTESIAN_POINT ( 'NONE',  ( -30.04822308544846621, 1524.382868172804365, 196.4802968571194413 ) ) ;
#63004 = CARTESIAN_POINT ( 'NONE',  ( 7.868158389089999538, 1422.937290482379922, 214.1570520181389838 ) ) ;
#63005 = CARTESIAN_POINT ( 'NONE',  ( -35.75806911936049914, 1384.805942682020031, 235.2916753997550074 ) ) ;
#63006 = VECTOR ( 'NONE', #99383, 1000.000000000000000 ) ;
#63007 = DIRECTION ( 'NONE',  ( -0.9455185755993177343, 0.000000000000000000, 0.3255681544571540909 ) ) ;
#63008 = CARTESIAN_POINT ( 'NONE',  ( 18.72979941119999836, 1454.437773883689943, 204.5413093961989830 ) ) ;
#63009 = CARTESIAN_POINT ( 'NONE',  ( 26.36150907684390177, 1435.617380069360024, 136.0950546535589751 ) ) ;
#63010 = CARTESIAN_POINT ( 'NONE',  ( -7.067966366155039815, 1396.159879213149907, 217.6086540106699942 ) ) ;
#63011 = AXIS2_PLACEMENT_3D ( 'NONE', #50063, #33236, #74166 ) ;
#63012 = CARTESIAN_POINT ( 'NONE',  ( -15.07865052128000016, 1422.394146857109945, 228.4054231139910200 ) ) ;
#63013 = CARTESIAN_POINT ( 'NONE',  ( -16.69321520597850039, 1410.132469723700069, 226.2257568831570040 ) ) ;
#63014 = CARTESIAN_POINT ( 'NONE',  ( -45.63527004870000070, 1440.521702456270077, 268.9748019413980273 ) ) ;
#63015 = VERTEX_POINT ( 'NONE', #20310 ) ;
#63016 = CARTESIAN_POINT ( 'NONE',  ( -11.37293999165238567, 1501.433396541875936, 207.8219951246407504 ) ) ;
#63017 = CARTESIAN_POINT ( 'NONE',  ( -15.69712680692647666, 1415.932051713374676, 208.5727945051003189 ) ) ;
#63018 = FACE_OUTER_BOUND ( 'NONE', #37099, .T. ) ;
#63020 = CARTESIAN_POINT ( 'NONE',  ( -12.53415180646500104, 1512.123798513659949, 192.8669541650669998 ) ) ;
#63019 = CARTESIAN_POINT ( 'NONE',  ( 11.17628604429999939, 1426.885039317430255, 103.4432774836980116 ) ) ;
#63021 = CARTESIAN_POINT ( 'NONE',  ( 3.550311703873260096E-15, 1384.899971913130003, 209.1218459572589836 ) ) ;
#63022 = CARTESIAN_POINT ( 'NONE',  ( -12.37499353609999986, 1442.762691980110048, 205.2217743980949933 ) ) ;
#63023 = ADVANCED_FACE ( 'NONE', ( #36036 ), #24181, .F. ) ;
#63024 = CARTESIAN_POINT ( 'NONE',  ( -0.01010286742719850028, 1516.939452820819952, 201.4022050290969901 ) ) ;
#63025 = CARTESIAN_POINT ( 'NONE',  ( 7.892794852110000647, 1424.253103618490059, 211.9974886484589831 ) ) ;
#63026 = CARTESIAN_POINT ( 'NONE',  ( -5.221955787189999754, 1489.269541098190075, 185.8916489435990229 ) ) ;
#63027 = CARTESIAN_POINT ( 'NONE',  ( 3.211749723379999644, 1507.435849901630036, 181.4459671118979998 ) ) ;
#63028 = CARTESIAN_POINT ( 'NONE',  ( -0.08492873674538491124, 1416.830086716310007, 191.0182577611500108 ) ) ;
#63029 = CARTESIAN_POINT ( 'NONE',  ( -48.44397510641989868, 1379.564747003970069, 243.3357836602579880 ) ) ;
#63030 = CARTESIAN_POINT ( 'NONE',  ( 4.692298114210420756, 1366.846184049853036, 209.6218459617148824 ) ) ;
#63032 = VERTEX_POINT ( 'NONE', #63467 ) ;
#63031 = CARTESIAN_POINT ( 'NONE',  ( -4.487249792034999629, 1509.038615934169911, 205.6342535031670025 ) ) ;
#63033 = ORIENTED_EDGE ( 'NONE', *, *, #24074, .T. ) ;
#63034 = DIRECTION ( 'NONE',  ( 1.755985294532464991E-16, -1.000000000000000000, 1.338183447452830017E-16 ) ) ;
#63035 = CARTESIAN_POINT ( 'NONE',  ( 0.8611642483871809750, 1507.132556045299907, 237.2366988190680104 ) ) ;
#63036 = CARTESIAN_POINT ( 'NONE',  ( 13.15726447020000123, 1414.996442546130083, 197.7616625855980033 ) ) ;
#63037 = CARTESIAN_POINT ( 'NONE',  ( -7.557029945415000505, 1510.729589429620091, 214.2821637710270011 ) ) ;
#63039 = CARTESIAN_POINT ( 'NONE',  ( 12.32904923398311325, 1414.913060387329779, 198.2898876794709224 ) ) ;
#63038 = CARTESIAN_POINT ( 'NONE',  ( -7.543596773550000023, 1384.566397051120020, 219.0776135590490128 ) ) ;
#63040 = CARTESIAN_POINT ( 'NONE',  ( -30.60461244942492343, 1523.621879633028584, 196.4204177336144141 ) ) ;
#63041 = SURFACE_STYLE_FILL_AREA ( #106098 ) ;
#63042 = CARTESIAN_POINT ( 'NONE',  ( -1.842963721827329815, 1515.551704300040001, 205.2922259627210053 ) ) ;
#63043 = CARTESIAN_POINT ( 'NONE',  ( 19.02974267272307074, 1517.151704408390060, 211.0809136819971741 ) ) ;
#63044 = CARTESIAN_POINT ( 'NONE',  ( 3.145663868875199221, 1370.195136005008180, 207.6218459616987673 ) ) ;
#63045 = CARTESIAN_POINT ( 'NONE',  ( 33.93535975524210357, 1435.841728338589974, 135.9422392606320216 ) ) ;
#63046 = CARTESIAN_POINT ( 'NONE',  ( -6.122330375623380228, 1406.076006365369949, 268.4678845349259859 ) ) ;
#63047 = CARTESIAN_POINT ( 'NONE',  ( 41.14740357920000235, 1443.969947807379867, 136.9302553032979972 ) ) ;
#63048 = ORIENTED_EDGE ( 'NONE', *, *, #89984, .F. ) ;
#63049 = CARTESIAN_POINT ( 'NONE',  ( -16.83198307402317440, 1526.000688113712840, 182.3274564795793253 ) ) ;
#63050 = CARTESIAN_POINT ( 'NONE',  ( 11.76268527979999945, 1441.457099483779757, 188.0189021094980149 ) ) ;
#63051 = ORIENTED_EDGE ( 'NONE', *, *, #38611, .T. ) ;
#63052 = ORIENTED_EDGE ( 'NONE', *, *, #98759, .T. ) ;
#63053 = DIRECTION ( 'NONE',  ( 0.9455185755993178454, 0.000000000000000000, -0.3255681544571537578 ) ) ;
#63054 = CARTESIAN_POINT ( 'NONE',  ( -9.178315062050000250, 1363.109187794150102, 207.6218459616989946 ) ) ;
#63055 = CARTESIAN_POINT ( 'NONE',  ( -6.551643424905000401, 1516.807958722750072, 214.9033365145770063 ) ) ;
#63056 = CARTESIAN_POINT ( 'NONE',  ( 2.234922648835000025, 1512.341036949130057, 216.7210731158769761 ) ) ;
#63057 = VERTEX_POINT ( 'NONE', #1900 ) ;
#63058 = CARTESIAN_POINT ( 'NONE',  ( 2.500000000000000000, 1448.437146640389983, 161.5787848790610326 ) ) ;
#63059 = CARTESIAN_POINT ( 'NONE',  ( -94.55573068399999670, 1379.531630663989972, 302.1084921616590009 ) ) ;
#63060 = EDGE_CURVE ( 'NONE', #53857, #86947, #49177, .T. ) ;
#63061 = ADVANCED_FACE ( 'NONE', ( #12473 ), #7218, .F. ) ;
#63062 = EDGE_CURVE ( 'NONE', #106884, #15989, #40126, .T. ) ;
#63063 = CARTESIAN_POINT ( 'NONE',  ( 16.90152335259999816, 1414.971339025629959, 212.5779198278579827 ) ) ;
#63064 = CARTESIAN_POINT ( 'NONE',  ( 7.323974606304999746, 1516.647924054489977, 205.0857262875869935 ) ) ;
#63065 = CARTESIAN_POINT ( 'NONE',  ( -12.22580320763990080, 1490.195274737109912, 209.7895498202320255 ) ) ;
#63066 = ADVANCED_FACE ( 'NONE', ( #49388 ), #16140, .F. ) ;
#63067 = CARTESIAN_POINT ( 'NONE',  ( -92.78054746879999470, 1385.201317530089909, 294.1545524748589742 ) ) ;
#63068 = B_SPLINE_CURVE_WITH_KNOTS ( 'NONE', 3,
 ( #45063, #88705, #80298, #95440, #18704, #78079, #3613, #52900 ),
 .UNSPECIFIED., .F., .F.,
 ( 4, 2, 2, 4 ),
 ( 6.938893903907227607E-18, 0.001073044933456168909, 0.001609567400184250003, 0.002146089866912330880 ),
 .UNSPECIFIED. ) ;
#63069 = CARTESIAN_POINT ( 'NONE',  ( -5.237765362120001100, 1410.471163508729887, 231.7868085280980210 ) ) ;
#63071 = ORIENTED_EDGE ( 'NONE', *, *, #62419, .T. ) ;
#63070 = CARTESIAN_POINT ( 'NONE',  ( -15.96958168569999970, 1519.913060387329779, 191.7668369663979888 ) ) ;
#63072 = CARTESIAN_POINT ( 'NONE',  ( 31.77002005290000142, 1451.803664145230186, 134.7784598387979997 ) ) ;
#63073 = CARTESIAN_POINT ( 'NONE',  ( -26.43364689489139963, 1440.913060452569880, 224.1083565477900095 ) ) ;
#63074 = DIRECTION ( 'NONE',  ( -0.8775825618903703162, 0.000000000000000000, -0.4794255386042076128 ) ) ;
#63075 = DIRECTION ( 'NONE',  ( 0.3892484888175031799, -0.9211327884476211425, 0.000000000000000000 ) ) ;
#63076 = CARTESIAN_POINT ( 'NONE',  ( 35.41142118405590367, 1421.645479188649915, 270.3426747825220104 ) ) ;
#63077 = CARTESIAN_POINT ( 'NONE',  ( -4.997250192034999650, 1516.727068157269969, 212.3866247496169990 ) ) ;
#63078 = CIRCLE ( 'NONE', #80863, 2.000000000000003553 ) ;
#63079 = CARTESIAN_POINT ( 'NONE',  ( -67.45763281530000199, 1379.744713633030187, 277.3665591780590489 ) ) ;
#63080 = CARTESIAN_POINT ( 'NONE',  ( -7.766142847955903150, 1425.761605071012127, 225.8812321164998025 ) ) ;
#63081 = CARTESIAN_POINT ( 'NONE',  ( 12.14778619052680142, 1426.452938115369989, 195.7521405516270079 ) ) ;
#63082 = CARTESIAN_POINT ( 'NONE',  ( 21.04378882164967379, 1411.007238685950597, 200.0432284193734915 ) ) ;
#63083 = CARTESIAN_POINT ( 'NONE',  ( -3.261652325025000021, 1516.939580991450157, 209.1351299096569960 ) ) ;
#63084 = ORIENTED_EDGE ( 'NONE', *, *, #83590, .F. ) ;
#63085 = CARTESIAN_POINT ( 'NONE',  ( 22.79764478813683581, 1411.075395668607598, 207.0126141096596371 ) ) ;
#63087 = ADVANCED_FACE ( 'NONE', ( #24692 ), #17393, .F. ) ;
#63086 = CARTESIAN_POINT ( 'NONE',  ( -2.816706472479999945, 1415.376295151229897, 232.8007527343979746 ) ) ;
#63088 = CARTESIAN_POINT ( 'NONE',  ( -86.93521348900000589, 1384.624802884190103, 307.7215772890590415 ) ) ;
#63089 = VERTEX_POINT ( 'NONE', #33116 ) ;
#63090 = CARTESIAN_POINT ( 'NONE',  ( -30.83205449964789935, 1385.229680719480029, 228.9263574028450137 ) ) ;
#63091 = CARTESIAN_POINT ( 'NONE',  ( -3.118868704080000054, 1430.676437493689946, 201.3658569193489996 ) ) ;
#63092 = EDGE_CURVE ( 'NONE', #75688, #45421, #90893, .T. ) ;
#63093 = CARTESIAN_POINT ( 'NONE',  ( -24.15153490410000359, 1438.063247892820073, 212.1983423404379892 ) ) ;
#63094 = CARTESIAN_POINT ( 'NONE',  ( -24.90943706210489950, 1441.448768262790054, 210.4417431393899847 ) ) ;
#63095 = EDGE_CURVE ( 'NONE', #31476, #56110, #18688, .T. ) ;
#63096 = CARTESIAN_POINT ( 'NONE',  ( 3.487592428935230249, 1508.551704408389924, 214.1089243929580164 ) ) ;
#63097 = CARTESIAN_POINT ( 'NONE',  ( -0.1262818449771200280, 1420.460208507500056, 182.7273227126599977 ) ) ;
#63099 = CARTESIAN_POINT ( 'NONE',  ( 21.83550407203902211, 1523.678648413191695, 183.2743720722707224 ) ) ;
#63098 = CARTESIAN_POINT ( 'NONE',  ( 7.331183090945000203, 1516.882217593000178, 216.0635732225570109 ) ) ;
#63100 = CARTESIAN_POINT ( 'NONE',  ( -3.617573937782270210, 1497.333809982809953, 198.4503636364750037 ) ) ;
#63101 = CARTESIAN_POINT ( 'NONE',  ( 9.939099051061740298, 1468.642790207840108, 207.8814491574680119 ) ) ;
#63102 = ORIENTED_EDGE ( 'NONE', *, *, #8801, .F. ) ;
#63103 = CARTESIAN_POINT ( 'NONE',  ( -11.84669589607570117, 1415.088506334930116, 196.8357868303870077 ) ) ;
#63104 = CARTESIAN_POINT ( 'NONE',  ( -0.7142343592189999146, 1485.913060387329779, 181.6617165099980014 ) ) ;
#63105 = ORIENTED_EDGE ( 'NONE', *, *, #65149, .T. ) ;
#63106 = CARTESIAN_POINT ( 'NONE',  ( 0.3822502236720000113, 1506.811133769929938, 231.1177528848980103 ) ) ;
#63107 = CARTESIAN_POINT ( 'NONE',  ( 11.14671379024469999, 1434.019377051509991, 151.6529839732360188 ) ) ;
#63108 = CARTESIAN_POINT ( 'NONE',  ( -18.86688640473561307, 1511.187213306747708, 237.4611898188522332 ) ) ;
#63109 = CARTESIAN_POINT ( 'NONE',  ( 2.438924525309999591, 1442.537362853589912, 217.7859099704189987 ) ) ;
#63110 = CARTESIAN_POINT ( 'NONE',  ( 16.33841777375469562, 1421.565078431612619, 227.2260880633069178 ) ) ;
#63111 = CARTESIAN_POINT ( 'NONE',  ( -3.653657264520000059, 1446.290935081919997, 168.9981087857980242 ) ) ;
#63112 = CARTESIAN_POINT ( 'NONE',  ( -5.731937517950226990, 1432.353341358200169, 149.9895731141591000 ) ) ;
#63113 = CARTESIAN_POINT ( 'NONE',  ( -15.70342473219999846, 1435.191803117289965, 148.3090083168980016 ) ) ;
#63114 = CARTESIAN_POINT ( 'NONE',  ( -19.53786426058999481, 1511.187213306747708, 236.7197124308268030 ) ) ;
#63115 = DIRECTION ( 'NONE',  ( -0.6742693640212139572, -4.521919481779819710E-17, -0.7384854939282339270 ) ) ;
#63117 = CARTESIAN_POINT ( 'NONE',  ( -18.95277575333325615, 1439.030827722083131, 210.3414025166298131 ) ) ;
#63116 = CARTESIAN_POINT ( 'NONE',  ( -30.51231035492510557, 1526.382868172863937, 218.1578534183722979 ) ) ;
#63118 = CARTESIAN_POINT ( 'NONE',  ( -0.1847390196904469817, 1457.875415826569906, 229.1891656909159849 ) ) ;
#63119 = EDGE_LOOP ( 'NONE', ( #37568, #69777, #14117, #37804 ) ) ;
#63120 = CARTESIAN_POINT ( 'NONE',  ( -103.8895706480000030, 1379.883984609199842, 304.0050191322589512 ) ) ;
#63121 = CARTESIAN_POINT ( 'NONE',  ( -14.24647739600000129, 1508.551704408389924, 215.7238636938289744 ) ) ;
#63122 = CARTESIAN_POINT ( 'NONE',  ( 3.829620113550000315, 1515.551704408389924, 210.9648081929590262 ) ) ;
#63123 = CARTESIAN_POINT ( 'NONE',  ( -24.42533947069999911, 1437.817911553419890, 210.7709913334879843 ) ) ;
#63124 = CARTESIAN_POINT ( 'NONE',  ( 29.66215386746311466, 1526.345556099435726, 216.9909811895615235 ) ) ;
#63125 = CARTESIAN_POINT ( 'NONE',  ( -18.65451768850000036, 1507.632629712929884, 229.7110761578979918 ) ) ;
#63126 = CARTESIAN_POINT ( 'NONE',  ( -2.214868538355918570, 1525.730671215507982, 241.5483252278176565 ) ) ;
#63127 = CARTESIAN_POINT ( 'NONE',  ( 11.46781549567650593, 1434.775379691847320, 151.4529278985016845 ) ) ;
#63128 = CARTESIAN_POINT ( 'NONE',  ( -7.487063421429379417, 1517.051703294439903, 208.6815157772669806 ) ) ;
#63129 = CARTESIAN_POINT ( 'NONE',  ( 5.551017880412060457, 1493.954195658629942, 218.9115059150300056 ) ) ;
#63130 = CARTESIAN_POINT ( 'NONE',  ( -9.512413405997190097, 1489.190735525819946, 215.4037021917559969 ) ) ;
#63131 = PRODUCT_DEFINITION ( 'UNKNOWN', '', #24370, #37868 ) ;
#63132 = CARTESIAN_POINT ( 'NONE',  ( 13.84583145400000070, 1499.900106662689723, 227.7510597354990125 ) ) ;
#63133 = CARTESIAN_POINT ( 'NONE',  ( -82.29609599402139963, 1383.775366892559987, 305.0689505943109907 ) ) ;
#63134 = CARTESIAN_POINT ( 'NONE',  ( -109.4509034362719859, 1384.431620334350100, 311.2553551991560425 ) ) ;
#63135 = LINE ( 'NONE', #50698, #104743 ) ;
#63137 = EDGE_LOOP ( 'NONE', ( #64683, #58694, #69214, #19576 ) ) ;
#63136 = CARTESIAN_POINT ( 'NONE',  ( 22.34603363939999809, 1509.636789321229799, 190.4959359729979838 ) ) ;
#63138 = CARTESIAN_POINT ( 'NONE',  ( -106.6204612740000073, 1379.399477473190018, 303.3336452769589755 ) ) ;
#63139 = CARTESIAN_POINT ( 'NONE',  ( 13.34643004641739950, 1512.594488815719842, 224.4167555860190078 ) ) ;
#63140 = ORIENTED_EDGE ( 'NONE', *, *, #50004, .F. ) ;
#63141 = ORIENTED_EDGE ( 'NONE', *, *, #44818, .F. ) ;
#63142 = CARTESIAN_POINT ( 'NONE',  ( 11.78238356083980065, 1440.882651838439870, 188.1224447589279976 ) ) ;
#63143 = CARTESIAN_POINT ( 'NONE',  ( -109.3492103629999974, 1384.912544404370237, 297.1385189228590207 ) ) ;
#63144 = CARTESIAN_POINT ( 'NONE',  ( 12.57606862101337519, 1442.780661812642620, 169.4711452238722416 ) ) ;
#63146 = CARTESIAN_POINT ( 'NONE',  ( -29.14244563990000003, 1446.680133300080115, 238.0755268643980003 ) ) ;
#63145 = CARTESIAN_POINT ( 'NONE',  ( 29.80102004019969897, 1419.431233126144662, 269.4687009151867301 ) ) ;
#63147 = CARTESIAN_POINT ( 'NONE',  ( -19.71969760489999857, 1491.250796832030119, 189.6734715901979769 ) ) ;
#63148 = CARTESIAN_POINT ( 'NONE',  ( -11.93616985209999903, 1433.496130944540027, 150.0979445124980032 ) ) ;
#63149 = EDGE_CURVE ( 'NONE', #15989, #100706, #38085, .T. ) ;
#63150 = CARTESIAN_POINT ( 'NONE',  ( 26.93106841620000225, 1509.630720109830008, 201.7989744196580091 ) ) ;
#63151 = CARTESIAN_POINT ( 'NONE',  ( -18.97833546889999923, 1485.957402666529788, 189.4643713726979684 ) ) ;
#63152 = CARTESIAN_POINT ( 'NONE',  ( -9.318458176530000969, 1446.292171852890078, 213.7041144372790313 ) ) ;
#63153 = EDGE_CURVE ( 'NONE', #38120, #86906, #98826, .T. ) ;
#63154 = CARTESIAN_POINT ( 'NONE',  ( 4.923253753420000933, 1424.943525846130115, 185.6775012255980073 ) ) ;
#63155 = CARTESIAN_POINT ( 'NONE',  ( 0.5721718498293950628, 1515.139735159980091, 213.4493323049200058 ) ) ;
#63156 = CARTESIAN_POINT ( 'NONE',  ( 6.218421307649999896, 1442.637438617560065, 154.8383831848980208 ) ) ;
#63157 = CARTESIAN_POINT ( 'NONE',  ( -4.856098619647529979, 1477.048158301180138, 219.5765844122289820 ) ) ;
#63158 = CARTESIAN_POINT ( 'NONE',  ( -19.97163517270000099, 1451.785673805730084, 145.5354985206979848 ) ) ;
#63160 = VERTEX_POINT ( 'NONE', #105292 ) ;
#63159 = CARTESIAN_POINT ( 'NONE',  ( 20.12874795999999833, 1473.837606016890049, 209.1218459616989946 ) ) ;
#63161 = VERTEX_POINT ( 'NONE', #54905 ) ;
#63162 = CARTESIAN_POINT ( 'NONE',  ( -11.86392824893790099, 1432.184205469619883, 149.9802395947019988 ) ) ;
#63163 = CARTESIAN_POINT ( 'NONE',  ( 16.52383693655309926, 1494.278885720349990, 193.0549977294350299 ) ) ;
#63164 = CARTESIAN_POINT ( 'NONE',  ( -34.72211068080000018, 1462.213514433730097, 270.0646873488980191 ) ) ;
#63165 = DIRECTION ( 'NONE',  ( -1.156023075842281927E-31, 1.000000000000000000, -1.698192320643030073E-16 ) ) ;
#63166 = CARTESIAN_POINT ( 'NONE',  ( 9.624350592200000776, 1441.605633920840091, 153.1179271311979733 ) ) ;
#63167 = CARTESIAN_POINT ( 'NONE',  ( -15.80679508490000273, 1506.802866820429927, 224.6866773128980128 ) ) ;
#63168 = ADVANCED_FACE ( 'NONE', ( #29133 ), #72261, .F. ) ;
#63169 = DIRECTION ( 'NONE',  ( -0.1070030146457303932, 0.000000000000000000, 0.9942586961433758086 ) ) ;
#63170 = CARTESIAN_POINT ( 'NONE',  ( -12.26257701979999837, 1420.531538507830192, 229.3828047662979941 ) ) ;
#63171 = CARTESIAN_POINT ( 'NONE',  ( -9.077703255249998548, 1460.186802329990087, 213.0212026448490121 ) ) ;
#63172 = CARTESIAN_POINT ( 'NONE',  ( 9.454737631249999552, 1363.431170718789872, 207.6218459616989946 ) ) ;
#63173 = CARTESIAN_POINT ( 'NONE',  ( -45.53644742934309875, 1435.582664252089899, 266.6938170526619842 ) ) ;
#63174 = ORIENTED_EDGE ( 'NONE', *, *, #25483, .T. ) ;
#63175 = CARTESIAN_POINT ( 'NONE',  ( -3.540994294616410354, 1498.936809983509875, 181.3258807172460081 ) ) ;
#63176 = ORIENTED_EDGE ( 'NONE', *, *, #63800, .T. ) ;
#63177 = CARTESIAN_POINT ( 'NONE',  ( 7.338753830235000386, 1517.184383877180153, 211.4127322367170052 ) ) ;
#63178 = CARTESIAN_POINT ( 'NONE',  ( -0.4151546846821903003, 1522.382868172863937, 244.9330574173806951 ) ) ;
#63179 = LINE ( 'NONE', #36833, #51573 ) ;
#63180 = CARTESIAN_POINT ( 'NONE',  ( 4.500000000000000000, 1425.929641636930000, 183.3886486283980162 ) ) ;
#63181 = CARTESIAN_POINT ( 'NONE',  ( -0.4989641633528249520, 1496.333062096209915, 221.4618052869690246 ) ) ;
#63182 = ORIENTED_EDGE ( 'NONE', *, *, #30904, .T. ) ;
#63183 = CARTESIAN_POINT ( 'NONE',  ( -4.026786250540000722, 1415.442497638829991, 163.1427597075980032 ) ) ;
#63184 = EDGE_CURVE ( 'NONE', #31573, #10167, #95681, .T. ) ;
#63185 =( BOUNDED_SURFACE ( )  B_SPLINE_SURFACE ( 3, 2, ( 
 ( #104364, #102276, #54005 ),
 ( #70812, #88137, #45594 ),
 ( #17137, #20347, #19228 ),
 ( #88685, #87582, #10871 ),
 ( #10298, #78619, #27661 ),
 ( #33973, #36072, #79735 ),
 ( #51327, #70257, #25556 ),
 ( #79188, #85462, #3044 ),
 ( #2494, #12514, #71366 ),
 ( #28210, #28767, #62969 ),
 ( #80278, #3592, #97626 ),
 ( #20894, #39918, #13036 ),
 ( #48893, #74087, #30405 ),
 ( #30959, #65684, #32064 ) ),
 .UNSPECIFIED., .F., .F., .T. ) 
 B_SPLINE_SURFACE_WITH_KNOTS ( ( 4, 2, 2, 2, 2, 2, 4 ),
 ( 3, 3 ),
 ( 2.300677010014240409E-16, 0.0009443072508238389362, 0.001416460876235643316, 0.001888614501647447805, 0.002360768127059252076, 0.002832921752471056782, 0.003777229003294665759 ),
 ( 0.000000000000000000, 1.000000000000000000 ),
 .UNSPECIFIED. ) 
 GEOMETRIC_REPRESENTATION_ITEM ( )  RATIONAL_B_SPLINE_SURFACE ( (
 ( 1.000000000000000000, 0.9376006582765984421, 1.000000000000000000),
 ( 1.000000000000000000, 0.9283977714665412329, 1.000000000000000000),
 ( 1.000000000000000000, 0.9189750060575127000, 1.000000000000000000),
 ( 1.000000000000000000, 0.9042792056079913543, 1.000000000000000000),
 ( 1.000000000000000000, 0.8992469033838338399, 1.000000000000000000),
 ( 1.000000000000000000, 0.8891280264687103640, 1.000000000000000000),
 ( 1.000000000000000000, 0.8840337471674056813, 1.000000000000000000),
 ( 1.000000000000000000, 0.8736395124164820780, 1.000000000000000000),
 ( 1.000000000000000000, 0.8683406746559402256, 1.000000000000000000),
 ( 1.000000000000000000, 0.8573361860701106396, 1.000000000000000000),
 ( 1.000000000000000000, 0.8516508399497402237, 1.000000000000000000),
 ( 1.000000000000000000, 0.8340914917063595446, 1.000000000000000000),
 ( 1.000000000000000000, 0.8215597275863861793, 1.000000000000000000),
 ( 1.000000000000000000, 0.8070209408750170788, 1.000000000000000000) ) ) 
 REPRESENTATION_ITEM ( '' )  SURFACE ( )  );
#63186 = EDGE_CURVE ( 'NONE', #91380, #7480, #62783, .T. ) ;
#63187 = CARTESIAN_POINT ( 'NONE',  ( 1.125509850285000280, 1517.203017563489766, 201.7827387294869936 ) ) ;
#63188 = CARTESIAN_POINT ( 'NONE',  ( 6.554685473990000233, 1473.611172115990030, 218.5142022801589974 ) ) ;
#63189 = CARTESIAN_POINT ( 'NONE',  ( -8.567500621095319957, 1439.360189638610109, 206.7715929992849908 ) ) ;
#63190 = ORIENTED_EDGE ( 'NONE', *, *, #74798, .T. ) ;
#63191 = CARTESIAN_POINT ( 'NONE',  ( -13.59643806539980027, 1409.123878638069982, 270.0979091653910018 ) ) ;
#63192 = CARTESIAN_POINT ( 'NONE',  ( -16.33500296837753041, 1517.151704408390060, 204.2067034917001536 ) ) ;
#63193 = CYLINDRICAL_SURFACE ( 'NONE', #8927, 33.13701971169416538 ) ;
#63195 = EDGE_LOOP ( 'NONE', ( #66774, #9580, #93571, #21660, #47876 ) ) ;
#63194 = CARTESIAN_POINT ( 'NONE',  ( -8.962252599310001955, 1366.920250605820002, 207.6218459616989946 ) ) ;
#63196 = ORIENTED_EDGE ( 'NONE', *, *, #101923, .F. ) ;
#63197 = CARTESIAN_POINT ( 'NONE',  ( 44.72660186364661428, 1447.710275772193654, 269.0002519517747714 ) ) ;
#63198 = ADVANCED_FACE ( 'NONE', ( #106392 ), #70077, .F. ) ;
#63199 = CARTESIAN_POINT ( 'NONE',  ( -1.841039239253470017, 1467.896901348140091, 220.0920151498449968 ) ) ;
#63200 = CARTESIAN_POINT ( 'NONE',  ( 3.674553501219381069, 1424.234175143221591, 184.0560900496116972 ) ) ;
#63201 = CARTESIAN_POINT ( 'NONE',  ( -33.44263403534804269, 1416.839417735997131, 266.5283828626972991 ) ) ;
#63202 = EDGE_CURVE ( 'NONE', #45986, #106196, #49463, .T. ) ;
#63203 = DIRECTION ( 'NONE',  ( 1.000000000000000000, 0.000000000000000000, 2.004237160840000101E-13 ) ) ;
#63204 = CARTESIAN_POINT ( 'NONE',  ( 7.333575610579999626, 1455.004670275590115, 216.8632114976190053 ) ) ;
#63205 = CARTESIAN_POINT ( 'NONE',  ( -14.56125758019999950, 1423.490991497129926, 221.7880315116979943 ) ) ;
#63206 = CARTESIAN_POINT ( 'NONE',  ( 11.80119706069999985, 1415.163755984229965, 222.4114065333980079 ) ) ;
#63207 = DIRECTION ( 'NONE',  ( 0.000000000000000000, 6.123233995736769734E-17, 1.000000000000000000 ) ) ;
#63208 = CARTESIAN_POINT ( 'NONE',  ( -5.787477032644999575, 1517.070197312179971, 206.2521524731670013 ) ) ;
#63209 = ORIENTED_EDGE ( 'NONE', *, *, #69383, .T. ) ;
#63210 = PLANE ( 'NONE',  #40203 ) ;
#63211 = CARTESIAN_POINT ( 'NONE',  ( -24.04659120089169733, 1444.796772349889807, 212.0316830080810178 ) ) ;
#63212 = ORIENTED_EDGE ( 'NONE', *, *, #54322, .T. ) ;
#63213 = CARTESIAN_POINT ( 'NONE',  ( 10.48296864959158192, 1455.202037190736291, 226.3317574583255407 ) ) ;
#63214 = CARTESIAN_POINT ( 'NONE',  ( -27.85007289616701698, 1509.193792693449723, 210.7874565944711378 ) ) ;
#63215 = CARTESIAN_POINT ( 'NONE',  ( 19.66678637246580053, 1517.151704408390060, 202.3500283489900085 ) ) ;
#63216 = CARTESIAN_POINT ( 'NONE',  ( -30.11988021650000036, 1389.744009244819836, 222.9251520012589936 ) ) ;
#63217 = CARTESIAN_POINT ( 'NONE',  ( -2.919621720534709919, 1419.522956690290130, 186.2043860719099939 ) ) ;
#63218 = DIRECTION ( 'NONE',  ( 1.755985294532469921E-16, -1.000000000000000000, 1.338183447452831989E-16 ) ) ;
#63219 = CARTESIAN_POINT ( 'NONE',  ( 23.10442914280000082, 1411.095127664230176, 207.3185324329880075 ) ) ;
#63220 = CARTESIAN_POINT ( 'NONE',  ( -0.02516806119179999801, 1415.404723302029879, 233.4400559027980080 ) ) ;
#63221 = CARTESIAN_POINT ( 'NONE',  ( 11.23851827549999882, 1490.487975447490044, 204.0492753133389954 ) ) ;
#63222 = EDGE_CURVE ( 'NONE', #98450, #2901, #15372, .T. ) ;
#63223 = CARTESIAN_POINT ( 'NONE',  ( 0.5501147289262610096, 1452.327375750520105, 183.2609232956120024 ) ) ;
#63224 = CARTESIAN_POINT ( 'NONE',  ( 2.500000000000000000, 1439.569237558239820, 165.5254318433829894 ) ) ;
#63225 = CARTESIAN_POINT ( 'NONE',  ( 5.007588646914999941, 1516.804776704140068, 214.8970827629769644 ) ) ;
#63226 = EDGE_CURVE ( 'NONE', #36010, #104582, #58125, .T. ) ;
#63227 = CARTESIAN_POINT ( 'NONE',  ( 3.317974621678423830, 1524.412455883367784, 241.9116897047633756 ) ) ;
#63228 = ORIENTED_EDGE ( 'NONE', *, *, #23624, .F. ) ;
#63229 = CARTESIAN_POINT ( 'NONE',  ( -19.23853081770000273, 1466.576780668189940, 213.8528554934590034 ) ) ;
#63230 = B_SPLINE_SURFACE_WITH_KNOTS ( 'NONE', 5, 5, ( 
 ( #87603, #26565, #62421, #104943, #18705, #25995 ),
 ( #85930, #87032, #61869, #28234, #78080, #60761 ),
 ( #95987, #94884, #45064, #79207, #96547, #69719 ),
 ( #19820, #103837, #43936, #51790, #14020, #31934 ),
 ( #22403, #24067, #11443, #14577, #58260, #97100 ),
 ( #99124, #81779, #45618, #3065, #23530, #39232 ) ),
 .UNSPECIFIED., .F., .F., .F.,
 ( 6, 6 ),
 ( 6, 6 ),
 ( 6.877177566609999460, 14.96017628310000092 ),
 ( 0.000000000000000000, 2.000000000000000000 ),
 .UNSPECIFIED. ) ;
#63231 = CARTESIAN_POINT ( 'NONE',  ( 22.01290455779448152, 1522.906363951597314, 235.3651141902282689 ) ) ;
#63232 = CARTESIAN_POINT ( 'NONE',  ( -18.16418870590820234, 1416.835419214280137, 209.0763567938479923 ) ) ;
#63233 = CARTESIAN_POINT ( 'NONE',  ( -20.94952978810714228, 1507.788843330700047, 209.4873209303592887 ) ) ;
#63234 = CARTESIAN_POINT ( 'NONE',  ( -39.78974365313739270, 1446.312716817450109, 136.7506402475469827 ) ) ;
#63235 = CARTESIAN_POINT ( 'NONE',  ( 11.60004869885203860, 1425.208448849134129, 137.9974123457472501 ) ) ;
#63236 = DIRECTION ( 'NONE',  ( -0.3090169943749515591, 0.000000000000000000, -0.9510565162951523099 ) ) ;
#63237 = CARTESIAN_POINT ( 'NONE',  ( 41.65772607930001215, 1455.325942033426145, 266.3040522087976569 ) ) ;
#63238 = CARTESIAN_POINT ( 'NONE',  ( 11.59187693560000021, 1433.125071996289989, 151.1000449916980131 ) ) ;
#63239 = CARTESIAN_POINT ( 'NONE',  ( 6.499999980935001531, 1515.051704408389924, 209.1218459511669892 ) ) ;
#63240 = CARTESIAN_POINT ( 'NONE',  ( 24.59498489902570029, 1440.913044926110160, 213.3385239659299941 ) ) ;
#63241 = CARTESIAN_POINT ( 'NONE',  ( -109.5349736409999934, 1385.152114132390125, 297.1296876067589778 ) ) ;
#63242 = CARTESIAN_POINT ( 'NONE',  ( 12.17090612297010033, 1499.730349834240087, 205.6507082230390040 ) ) ;
#63243 = ORIENTED_EDGE ( 'NONE', *, *, #74134, .T. ) ;
#63244 = CARTESIAN_POINT ( 'NONE',  ( -1.906498070525230022E-08, 1509.051704408389924, 216.1347675157070114 ) ) ;
#63245 = CARTESIAN_POINT ( 'NONE',  ( -2.487935123020000194, 1508.551704408389924, 214.1089243778970115 ) ) ;
#63246 = DIRECTION ( 'NONE',  ( -0.2054769195713296304, 0.000000000000000000, -0.9786619618251631847 ) ) ;
#63247 = CARTESIAN_POINT ( 'NONE',  ( 12.53380665967529950, 1445.052233242549846, 186.0874955919830143 ) ) ;
#63248 = CARTESIAN_POINT ( 'NONE',  ( -4.869818399669999742, 1491.215867106689984, 188.8099941780989752 ) ) ;
#63249 = CARTESIAN_POINT ( 'NONE',  ( -16.53175237173161705, 1526.069472839382115, 235.9420435486929364 ) ) ;
#63250 = CARTESIAN_POINT ( 'NONE',  ( -17.56617790150000147, 1509.356465178830149, 231.0161195107979779 ) ) ;
#63251 = CARTESIAN_POINT ( 'NONE',  ( -24.20210390755639907, 1383.848986423020051, 222.9592914590000134 ) ) ;
#63252 = CARTESIAN_POINT ( 'NONE',  ( -21.51339055684400137, 1505.551704076410033, 209.1218459052249727 ) ) ;
#63253 = CARTESIAN_POINT ( 'NONE',  ( 5.407433588731190177, 1422.540975204839924, 131.0095517816550057 ) ) ;
#63254 = CARTESIAN_POINT ( 'NONE',  ( -14.60558113189999929, 1415.677402202029953, 212.8314178170890045 ) ) ;
#63255 = CARTESIAN_POINT ( 'NONE',  ( 1.971096436429999654, 1464.814372936629979, 236.1963158674979866 ) ) ;
#63257 = EDGE_LOOP ( 'NONE', ( #51232, #30150 ) ) ;
#63256 = CARTESIAN_POINT ( 'NONE',  ( 32.36513376976810719, 1523.847233649538339, 216.1093208013068079 ) ) ;
#63258 = CARTESIAN_POINT ( 'NONE',  ( -0.6412295605840000468, 1451.094351508330192, 182.3047427481980094 ) ) ;
#63259 = CARTESIAN_POINT ( 'NONE',  ( -11.15738487964140013, 1390.939238811560017, 203.8452351040699853 ) ) ;
#63260 = CARTESIAN_POINT ( 'NONE',  ( 3.462090701198914822, 1432.317094223078811, 156.5315814253846156 ) ) ;
#63262 = ORIENTED_EDGE ( 'NONE', *, *, #59272, .F. ) ;
#63261 = CARTESIAN_POINT ( 'NONE',  ( -31.62138935264889028, 1525.231887713368678, 216.6630328221493187 ) ) ;
#63263 = CARTESIAN_POINT ( 'NONE',  ( 20.33642002845060048, 1475.138300237510066, 218.0161321312470193 ) ) ;
#63264 = EDGE_LOOP ( 'NONE', ( #77691, #76777 ) ) ;
#63265 = CARTESIAN_POINT ( 'NONE',  ( -13.55712941462900112, 1390.145928966170004, 212.6894278554629807 ) ) ;
#63266 = DIRECTION ( 'NONE',  ( -0.02616798426672899136, -0.9993150019883406676, 0.02616798426434139430 ) ) ;
#63267 = CARTESIAN_POINT ( 'NONE',  ( 11.56380544704854962, 1426.103149140334381, 138.8483449811455159 ) ) ;
#63268 = CARTESIAN_POINT ( 'NONE',  ( 10.99882366966150116, 1470.803487868729917, 192.2106042945659965 ) ) ;
#63269 = ADVANCED_FACE ( 'NONE', ( #21800, #99621 ), #48710, .F. ) ;
#63270 = CARTESIAN_POINT ( 'NONE',  ( 1.124946299140000106, 1430.908435126590120, 217.7868728150889979 ) ) ;
#63271 = CYLINDRICAL_SURFACE ( 'NONE', #20929, 0.5000000000000005551 ) ;
#63272 = CARTESIAN_POINT ( 'NONE',  ( 9.760933975314660671, 1409.253919710149830, 220.4514879604030000 ) ) ;
#63273 = CARTESIAN_POINT ( 'NONE',  ( -7.966180769845361276, 1384.913883566769982, 199.4893105002079778 ) ) ;
#63274 = CARTESIAN_POINT ( 'NONE',  ( -106.3772841639279960, 1385.236231160509988, 297.0206994190789942 ) ) ;
#63275 = CARTESIAN_POINT ( 'NONE',  ( -19.38280343810000161, 1485.637741855729928, 189.8313757130979980 ) ) ;
#63276 = CARTESIAN_POINT ( 'NONE',  ( 10.96892109620000078, 1432.312127152960102, 151.7701099976980004 ) ) ;
#63277 = CARTESIAN_POINT ( 'NONE',  ( 11.86864015205539857, 1492.043074283439864, 209.5973308918830185 ) ) ;
#63278 = EDGE_LOOP ( 'NONE', ( #80458, #87627, #96297, #58620, #109876 ) ) ;
#63279 = ORIENTED_EDGE ( 'NONE', *, *, #56195, .F. ) ;
#63280 = CARTESIAN_POINT ( 'NONE',  ( -7.012524266536320106, 1508.551704613440052, 215.1061919086760099 ) ) ;
#63281 = CARTESIAN_POINT ( 'NONE',  ( -12.06130973530630079, 1415.890045859420070, 194.8674313123640047 ) ) ;
#63282 = CARTESIAN_POINT ( 'NONE',  ( -1.132178478439539893, 1496.267470226739988, 196.8234858163660022 ) ) ;
#63283 = EDGE_CURVE ( 'NONE', #63956, #108856, #64409, .T. ) ;
#63284 = CARTESIAN_POINT ( 'NONE',  ( 35.04437474502410055, 1457.726427851593144, 269.5321128390857552 ) ) ;
#63285 = DIRECTION ( 'NONE',  ( -0.7067700363769180427, 0.03085824620774344287, -0.7067700363772875249 ) ) ;
#63286 = CARTESIAN_POINT ( 'NONE',  ( -14.35646903299999799, 1420.584115152450067, 213.7701001417389932 ) ) ;
#63287 = CARTESIAN_POINT ( 'NONE',  ( 22.15347900851059748, 1496.414301113179818, 209.7169039519030207 ) ) ;
#63288 = CARTESIAN_POINT ( 'NONE',  ( 0.2167502149440000137, 1453.575579519030043, 183.2287056930980214 ) ) ;
#63289 = CARTESIAN_POINT ( 'NONE',  ( -10.02185219039999886, 1364.916310432309956, 207.6218459616989946 ) ) ;
#63290 = CARTESIAN_POINT ( 'NONE',  ( 0.3740406207303079711, 1452.976564550639978, 183.2744760995269928 ) ) ;
#63291 = CARTESIAN_POINT ( 'NONE',  ( -1.718203501584999904, 1516.898441858519845, 207.4215862561470090 ) ) ;
#63292 = CARTESIAN_POINT ( 'NONE',  ( -14.28742066159479940, 1392.367256947369924, 209.8406639845640029 ) ) ;
#63293 = CARTESIAN_POINT ( 'NONE',  ( -3.558358604862239982, 1455.955982659530036, 200.3550966546550001 ) ) ;
#63294 = CARTESIAN_POINT ( 'NONE',  ( 1.121465680670000076, 1416.819759739430083, 190.1591349339979899 ) ) ;
#63295 = CARTESIAN_POINT ( 'NONE',  ( 1.608613766090000174, 1497.503754473789968, 197.5580351143990185 ) ) ;
#63296 = CARTESIAN_POINT ( 'NONE',  ( -19.57991515103069702, 1487.974510678529896, 201.8977438688889947 ) ) ;
#63297 = CARTESIAN_POINT ( 'NONE',  ( 41.36548120546149931, 1444.128165951429992, 136.5310689808069924 ) ) ;
#63298 = ORIENTED_EDGE ( 'NONE', *, *, #66255, .T. ) ;
#63299 = CARTESIAN_POINT ( 'NONE',  ( 42.46017295210000242, 1427.243201938829998, 266.3334799472979739 ) ) ;
#63300 = CARTESIAN_POINT ( 'NONE',  ( -19.72588041030000028, 1469.237837320530161, 193.2706619289980097 ) ) ;
#63302 = CARTESIAN_POINT ( 'NONE',  ( -17.22540132880000030, 1409.514584658930062, 195.8673741195979687 ) ) ;
#63301 = FACE_OUTER_BOUND ( 'NONE', #65039, .T. ) ;
#63303 = CARTESIAN_POINT ( 'NONE',  ( 20.58544670569870760, 1506.578946199305392, 201.0686405472372087 ) ) ;
#63304 = CARTESIAN_POINT ( 'NONE',  ( -31.44036050960000139, 1425.375771789929786, 254.7811623578979834 ) ) ;
#63305 = CARTESIAN_POINT ( 'NONE',  ( 1.951646715579999913, 1485.466892314489996, 220.4400105658989730 ) ) ;
#63306 = EDGE_CURVE ( 'NONE', #36571, #43462, #63514, .T. ) ;
#63307 = CARTESIAN_POINT ( 'NONE',  ( 12.89506042661790097, 1420.989630775050045, 203.4267427568519793 ) ) ;
#63308 = CARTESIAN_POINT ( 'NONE',  ( -22.81026925195165944, 1409.709605436964466, 208.9207937587944741 ) ) ;
#63309 = ORIENTED_EDGE ( 'NONE', *, *, #61635, .F. ) ;
#63310 = LINE ( 'NONE', #36417, #85745 ) ;
#63311 = CARTESIAN_POINT ( 'NONE',  ( 14.78591727178930171, 1514.559393050746394, 225.3792123963893630 ) ) ;
#63312 = EDGE_CURVE ( 'NONE', #17148, #94625, #81357, .T. ) ;
#63313 = DIRECTION ( 'NONE',  ( -1.156023075842281927E-31, 1.000000000000000000, -1.698192320643030073E-16 ) ) ;
#63314 = ORIENTED_EDGE ( 'NONE', *, *, #89359, .F. ) ;
#63315 = EDGE_LOOP ( 'NONE', ( #48628, #15616, #79990, #51586 ) ) ;
#63316 = CARTESIAN_POINT ( 'NONE',  ( 9.160265459600150706, 1451.053466593440135, 210.4056783562319879 ) ) ;
#63317 = CARTESIAN_POINT ( 'NONE',  ( 7.326528841800000080, 1424.652172197859954, 194.6120463040990103 ) ) ;
#63318 = EDGE_CURVE ( 'NONE', #44485, #76097, #909, .T. ) ;
#63319 = ORIENTED_EDGE ( 'NONE', *, *, #57615, .T. ) ;
#63320 = CARTESIAN_POINT ( 'NONE',  ( -0.7235648542570000119, 1417.479220455729774, 184.8026998982980160 ) ) ;
#63321 = CARTESIAN_POINT ( 'NONE',  ( -5.865854492251394880, 1419.522645696713653, 194.8824993499091534 ) ) ;
#63322 = CARTESIAN_POINT ( 'NONE',  ( 19.17592663279999954, 1455.939271352290007, 211.9382291609089748 ) ) ;
#63323 = EDGE_CURVE ( 'NONE', #52311, #108404, #104184, .T. ) ;
#63324 = CARTESIAN_POINT ( 'NONE',  ( -0.2559295722590000377, 1479.777904972630040, 236.1640397496979915 ) ) ;
#63325 = CARTESIAN_POINT ( 'NONE',  ( 5.389719913101400195, 1440.971386073809981, 154.8246291173960003 ) ) ;
#63326 = EDGE_LOOP ( 'NONE', ( #90404, #10566, #9016, #5305 ) ) ;
#63327 = CARTESIAN_POINT ( 'NONE',  ( 46.16774997373190104, 1440.912967117140170, 266.9713874478409821 ) ) ;
#63328 = CARTESIAN_POINT ( 'NONE',  ( -13.15726442949999964, 1415.948532225030021, 221.7037513481980113 ) ) ;
#63329 = CARTESIAN_POINT ( 'NONE',  ( 15.44132444849999786, 1507.624369749529933, 226.1399349509979970 ) ) ;
#63330 = ORIENTED_EDGE ( 'NONE', *, *, #89921, .F. ) ;
#63331 = CARTESIAN_POINT ( 'NONE',  ( 5.000083827734999709, 1516.858456333729919, 204.1129977322069919 ) ) ;
#63332 = ORIENTED_EDGE ( 'NONE', *, *, #57405, .F. ) ;
#63333 = CARTESIAN_POINT ( 'NONE',  ( 11.83960237644440028, 1430.521195547569960, 149.6755224652310119 ) ) ;
#63334 = CARTESIAN_POINT ( 'NONE',  ( 12.90355812175348404, 1444.932587894390736, 186.7378586203405462 ) ) ;
#63335 = ORIENTED_EDGE ( 'NONE', *, *, #84890, .F. ) ;
#63336 = ORIENTED_EDGE ( 'NONE', *, *, #84985, .T. ) ;
#63337 = CARTESIAN_POINT ( 'NONE',  ( 0.4681535437661810684, 1524.397344074319335, 173.8154889443022171 ) ) ;
#63338 = CARTESIAN_POINT ( 'NONE',  ( -2.157742269045689998, 1508.491635936170042, 220.5016648786540259 ) ) ;
#63339 = CARTESIAN_POINT ( 'NONE',  ( -22.57962297529999773, 1409.701558196430142, 208.4161775753709946 ) ) ;
#63340 = CARTESIAN_POINT ( 'NONE',  ( -3.476578636579250148, 1469.245868782419848, 218.7387964245460239 ) ) ;
#63341 = CARTESIAN_POINT ( 'NONE',  ( 19.88079262212649923, 1452.218807810889984, 143.3936228603050154 ) ) ;
#63342 = CARTESIAN_POINT ( 'NONE',  ( 9.209290677350001175, 1421.000200739789989, 196.8939171836989885 ) ) ;
#63343 = EDGE_CURVE ( 'NONE', #110436, #42621, #45510, .T. ) ;
#63344 = DIRECTION ( 'NONE',  ( 5.980589973904019347E-17, -1.000000000000000000, 1.736889445713099699E-16 ) ) ;
#63345 = DIRECTION ( 'NONE',  ( 0.000000000000000000, 0.000000000000000000, 1.000000000000000000 ) ) ;
#63346 = CARTESIAN_POINT ( 'NONE',  ( 4.576312612474012553, 1522.051704408389924, 195.8593501239998318 ) ) ;
#63347 = AXIS2_PLACEMENT_3D ( 'NONE', #13820, #32302, #83802 ) ;
#63348 = CARTESIAN_POINT ( 'NONE',  ( 0.02218773269636665699, 1410.258021740021150, 233.2201378621269896 ) ) ;
#63350 = CARTESIAN_POINT ( 'NONE',  ( -106.1610222967859869, 1391.913060319860051, 304.8404902532309961 ) ) ;
#63349 = CARTESIAN_POINT ( 'NONE',  ( -14.19821127820000051, 1503.588220803689865, 208.7291843775310269 ) ) ;
#63351 = CARTESIAN_POINT ( 'NONE',  ( -67.37805264042475528, 1379.747543260372140, 278.5100200681151819 ) ) ;
#63352 = CARTESIAN_POINT ( 'NONE',  ( -9.740768063862729420, 1440.142023887889991, 206.7831334340250180 ) ) ;
#63353 = ADVANCED_FACE ( 'NONE', ( #73905 ), #93051, .T. ) ;
#63354 = CARTESIAN_POINT ( 'NONE',  ( -7.908505719245000343, 1514.005261957169978, 201.8728991555269943 ) ) ;
#63355 = ORIENTED_EDGE ( 'NONE', *, *, #67067, .F. ) ;
#63356 = CARTESIAN_POINT ( 'NONE',  ( 20.63825565839999854, 1425.387366209430184, 248.0989693021979861 ) ) ;
#63357 = AXIS2_PLACEMENT_3D ( 'NONE', #65308, #39538, #73143 ) ;
#63358 = CARTESIAN_POINT ( 'NONE',  ( -1.331958139231829923E-15, 1375.413060387289988, 209.1218459616989946 ) ) ;
#63359 = CARTESIAN_POINT ( 'NONE',  ( -104.5692869006220036, 1384.935441801240131, 311.1781066240710061 ) ) ;
#63360 = B_SPLINE_SURFACE_WITH_KNOTS ( 'NONE', 5, 5, ( 
 ( #70535, #71089, #28502, #62699, #77613, #16558 ),
 ( #59717, #26076, #94964, #86005, #61391, #85434 ),
 ( #69791, #84887, #59176, #51868, #60838, #102783 ),
 ( #42347, #93296, #35599, #34501, #93834, #50750 ),
 ( #60268, #94387, #924, #101679, #8180, #76502 ),
 ( #27210, #18233, #110651, #95511, #77070, #78154 ),
 ( #69227, #52428, #103910, #18781, #43468, #8732 ),
 ( #44018, #33941, #86554, #68136, #102248, #110105 ),
 ( #17667, #52979, #25527, #9304, #87111, #10401 ),
 ( #68678, #1463, #35048, #9849, #103338, #42914 ),
 ( #75953, #33378, #67574, #24968, #17106, #51297 ),
 ( #380, #26641, #97167, #89868, #87681, #20989 ) ),
 .UNSPECIFIED., .F., .F., .F.,
 ( 6, 3, 3, 6 ),
 ( 6, 6 ),
 ( 52.58344481930000569, 57.38609284729999871, 62.18874087540000062, 65.18198166130000004 ),
 ( 0.000000000000000000, 2.000000000000000000 ),
 .UNSPECIFIED. ) ;
#63361 = CARTESIAN_POINT ( 'NONE',  ( -8.888257569051779328, 1385.312153913200063, 218.6608301139260107 ) ) ;
#63362 = CARTESIAN_POINT ( 'NONE',  ( 4.158039145940000125, 1505.593071592290016, 220.7718859801990163 ) ) ;
#63363 = EDGE_CURVE ( 'NONE', #34173, #52522, #99071, .T. ) ;
#63364 = CARTESIAN_POINT ( 'NONE',  ( 30.48816909598289726, 1414.062251626520037, 269.3695147698609844 ) ) ;
#63366 = ORIENTED_EDGE ( 'NONE', *, *, #98653, .T. ) ;
#63365 = DIRECTION ( 'NONE',  ( -1.000000000000000000, 0.000000000000000000, 0.000000000000000000 ) ) ;
#63367 = CARTESIAN_POINT ( 'NONE',  ( -15.73068931088838340, 1415.766719735401921, 209.6787192454432329 ) ) ;
#63368 = B_SPLINE_CURVE_WITH_KNOTS ( 'NONE', 3,
 ( #104084, #68861, #11683, #26264, #27379, #52601, #96804, #26830, #87294, #61015, #62119, #36327, #95693, #95142, #18959, #9475, #53155, #10588, #60451, #78340, #44759, #62682, #104639, #11150, #27936, #53725, #54268, #45860, #96246, #94571, #17843, #77791, #18403, #1100, #86737, #35228, #10027, #81084, #31233, #63762 ),
 .UNSPECIFIED., .F., .F.,
 ( 4, 3, 3, 3, 3, 3, 3, 3, 3, 3, 3, 3, 3, 4 ),
 ( -1.435063413027759971, -1.364066038576970064, -1.253444982554889897, -1.141100129978610100, -1.027733815200259970, -0.9128813494742499257, -0.7973539268154259396, -0.6814611664271418290, -0.5655430835226159525, -0.4502876605942469634, -0.3358911414603549250, -0.2226055258251640190, -0.1106062959119480382, -2.220446049250313081E-16 ),
 .UNSPECIFIED. ) ;
#63369 = CARTESIAN_POINT ( 'NONE',  ( -24.23120024909999870, 1444.178062262649973, 211.3705830899779983 ) ) ;
#63370 = CARTESIAN_POINT ( 'NONE',  ( -2.096033132107356423, 1450.108388725817122, 154.3469607748115493 ) ) ;
#63371 = CARTESIAN_POINT ( 'NONE',  ( 0.4304708442563399684, 1430.546724899550100, 199.7002147614190051 ) ) ;
#63372 = CARTESIAN_POINT ( 'NONE',  ( 15.09659336983500033, 1514.030803186779849, 224.8374594117669858 ) ) ;
#63373 = CARTESIAN_POINT ( 'NONE',  ( 4.234273392930074209, 1370.421192169647384, 208.5750769448261224 ) ) ;
#63374 = CARTESIAN_POINT ( 'NONE',  ( 27.41738420279390098, 1509.883512505909948, 222.6174317186479925 ) ) ;
#63375 = CARTESIAN_POINT ( 'NONE',  ( 8.185246060965688741, 1459.507010914890088, 203.1833342143360142 ) ) ;
#63376 = CARTESIAN_POINT ( 'NONE',  ( 12.80306059919530171, 1434.672636252922302, 149.2816584392911352 ) ) ;
#63377 = CARTESIAN_POINT ( 'NONE',  ( 2.927772224839999993, 1417.416557252929806, 231.9440355153979851 ) ) ;
#63378 = CARTESIAN_POINT ( 'NONE',  ( -4.526773330479999302, 1476.791184819089949, 219.3260595622990081 ) ) ;
#63379 = CARTESIAN_POINT ( 'NONE',  ( -22.14913372575983175, 1525.402221411349728, 235.6690521037287454 ) ) ;
#63380 = CARTESIAN_POINT ( 'NONE',  ( 0.7352271172030020452, 1516.963431999339946, 207.4067364850470199 ) ) ;
#63381 = CARTESIAN_POINT ( 'NONE',  ( 45.88375197359999902, 1438.918372143629995, 266.4124103407979760 ) ) ;
#63382 = CARTESIAN_POINT ( 'NONE',  ( -18.71691417810000146, 1410.062790051930051, 223.0812584992980021 ) ) ;
#63383 = CARTESIAN_POINT ( 'NONE',  ( 23.46567568339999710, 1436.545700739849963, 140.9406085994980060 ) ) ;
#63384 = CARTESIAN_POINT ( 'NONE',  ( 23.63314310590000034, 1508.007761069829940, 195.0461405673979982 ) ) ;
#63385 = CARTESIAN_POINT ( 'NONE',  ( 21.88687337236331487, 1430.321363104666261, 220.0073771757959378 ) ) ;
#63386 = CARTESIAN_POINT ( 'NONE',  ( -12.55407686808170098, 1378.884881417289989, 208.1735791207040052 ) ) ;
#63387 = CARTESIAN_POINT ( 'NONE',  ( -2.102271589710000388, 1475.801440029330024, 266.9594147012980443 ) ) ;
#63388 = CARTESIAN_POINT ( 'NONE',  ( 12.64521106209990009, 1426.920070115170120, 205.6194074905729963 ) ) ;
#63389 = CARTESIAN_POINT ( 'NONE',  ( -34.87346161656260080, 1436.196920817200180, 136.2719409395089940 ) ) ;
#63390 = CARTESIAN_POINT ( 'NONE',  ( 1.984413551915469975, 1522.051704408389924, 198.9129232538419956 ) ) ;
#63391 = CARTESIAN_POINT ( 'NONE',  ( -14.63963062230000034, 1409.365349618529990, 210.6960423599879846 ) ) ;
#63392 = CARTESIAN_POINT ( 'NONE',  ( 8.454790733525280544, 1428.363638633589972, 213.4109935021670026 ) ) ;
#63393 = CARTESIAN_POINT ( 'NONE',  ( -4.325405441710000076, 1515.219201591190085, 207.2788837304390199 ) ) ;
#63394 = CARTESIAN_POINT ( 'NONE',  ( -22.03465957474533354, 1501.977400791986611, 235.4136513321633117 ) ) ;
#63395 = CARTESIAN_POINT ( 'NONE',  ( 11.87587044680000048, 1433.006446481710100, 146.7587676086979798 ) ) ;
#63396 = CARTESIAN_POINT ( 'NONE',  ( -35.12295699405159866, 1435.816162438429956, 134.0999999976959884 ) ) ;
#63397 = DIRECTION ( 'NONE',  ( -0.9211327884476211425, -0.3892484888175031799, 0.000000000000000000 ) ) ;
#63398 = EDGE_LOOP ( 'NONE', ( #78017, #9599, #51340, #66300 ) ) ;
#63399 = CARTESIAN_POINT ( 'NONE',  ( 5.511665417999469900E-05, 1508.970066526555001, 238.8757070596369942 ) ) ;
#63400 = CARTESIAN_POINT ( 'NONE',  ( -3.860068541672339926, 1409.047856951109907, 223.5979342058130044 ) ) ;
#63401 = CARTESIAN_POINT ( 'NONE',  ( 31.69312280309565821, 1525.713797967456912, 196.3032712708385077 ) ) ;
#63402 = CARTESIAN_POINT ( 'NONE',  ( 4.229167303610000594, 1436.983388288790138, 227.1518914930990150 ) ) ;
#63403 = B_SPLINE_CURVE_WITH_KNOTS ( 'NONE', 5,
 ( #47373, #97211, #98863, #56880, #80426, #107267, #91010, #21590, #39521 ),
 .UNSPECIFIED., .F., .F.,
 ( 6, 3, 6 ),
 ( 0.000000000000000000, 0.5002376165324764479, 1.000000000000000000 ),
 .UNSPECIFIED. ) ;
#63404 = DIRECTION ( 'NONE',  ( -0.000000000000000000, -1.000000000000000000, -0.000000000000000000 ) ) ;
#63405 = CARTESIAN_POINT ( 'NONE',  ( -30.12637356810000355, 1467.407322974130011, 268.6828795483979775 ) ) ;
#63406 = CARTESIAN_POINT ( 'NONE',  ( -30.36939524941901070, 1525.506916460679349, 196.8236333301088337 ) ) ;
#63407 = CARTESIAN_POINT ( 'NONE',  ( -16.66701395081226877, 1523.530870145309109, 237.7590812510466947 ) ) ;
#63408 = CARTESIAN_POINT ( 'NONE',  ( -26.19919347095130036, 1509.827956409970056, 209.1562360456119904 ) ) ;
#63409 = CARTESIAN_POINT ( 'NONE',  ( 7.703229013340137321, 1511.126521620285303, 203.6801736527461628 ) ) ;
#63410 = CARTESIAN_POINT ( 'NONE',  ( -41.29992742285089946, 1384.993104148180009, 214.1677007736450093 ) ) ;
#63411 = CARTESIAN_POINT ( 'NONE',  ( -8.392515761190244561, 1423.425497820198871, 210.5964995326183384 ) ) ;
#63412 = CARTESIAN_POINT ( 'NONE',  ( 15.10946924899999999, 1415.087745006229852, 217.0735260779379701 ) ) ;
#63413 = CARTESIAN_POINT ( 'NONE',  ( 1.110223024630000146E-16, 1435.943783413959864, 155.5249316174979981 ) ) ;
#63414 = CARTESIAN_POINT ( 'NONE',  ( 1.191524307911310254, 1526.382868172864164, 179.0083900503168479 ) ) ;
#63416 = ORIENTED_EDGE ( 'NONE', *, *, #5486, .T. ) ;
#63415 = FACE_OUTER_BOUND ( 'NONE', #92207, .T. ) ;
#63417 = CARTESIAN_POINT ( 'NONE',  ( -109.6576113679999906, 1384.901204824579963, 311.3230521602589533 ) ) ;
#63418 = DIRECTION ( 'NONE',  ( -1.755985294532469921E-16, 1.000000000000000000, -1.338183447452831989E-16 ) ) ;
#63419 = CARTESIAN_POINT ( 'NONE',  ( 7.717505752974999744, 1516.857914730730045, 201.4043401791270185 ) ) ;
#63420 = CARTESIAN_POINT ( 'NONE',  ( 16.66936639845630097, 1523.382868172864164, 180.4828114240739296 ) ) ;
#63421 = CARTESIAN_POINT ( 'NONE',  ( -1.506941832969999950, 1422.391778822009883, 192.9691301536989840 ) ) ;
#63422 = CARTESIAN_POINT ( 'NONE',  ( 23.62603012550000159, 1410.659706541129935, 211.3817606496579913 ) ) ;
#63423 = CARTESIAN_POINT ( 'NONE',  ( -107.1288397327830069, 1391.913060387289988, 306.9725994467550549 ) ) ;
#63424 = CARTESIAN_POINT ( 'NONE',  ( -18.58572048804549937, 1467.426106157030063, 201.0022324237500015 ) ) ;
#63425 = CARTESIAN_POINT ( 'NONE',  ( -5.359903627183280506, 1422.348471699870061, 145.8522681477809897 ) ) ;
#63427 = CARTESIAN_POINT ( 'NONE',  ( -12.17490798859999934, 1378.378576834209980, 206.9930340770689838 ) ) ;
#63426 = CARTESIAN_POINT ( 'NONE',  ( 11.90000415720300175, 1434.913060496859998, 147.6452464505769910 ) ) ;
#63428 = CARTESIAN_POINT ( 'NONE',  ( -5.188149647699999534, 1391.908650341390057, 203.7646307972290174 ) ) ;
#63429 = CARTESIAN_POINT ( 'NONE',  ( -103.5905392011000856, 1377.418846546391933, 309.5807789473911384 ) ) ;
#63430 = DIRECTION ( 'NONE',  ( 0.000000000000000000, 0.000000000000000000, 1.000000000000000000 ) ) ;
#63431 = DIRECTION ( 'NONE',  ( -0.9097196265265821147, 0.3041674008372309834, 0.2826524250387019710 ) ) ;
#63432 = AXIS2_PLACEMENT_3D ( 'NONE', #15370, #7537, #50111 ) ;
#63433 = CARTESIAN_POINT ( 'NONE',  ( -1.153787697646769805, 1420.825136633349985, 183.6905923417640167 ) ) ;
#63434 = CARTESIAN_POINT ( 'NONE',  ( 7.711550677984999602, 1516.630499592039996, 205.0863552195469879 ) ) ;
#63435 = CARTESIAN_POINT ( 'NONE',  ( -18.48452897440000342, 1425.095849964330000, 227.3281627736979829 ) ) ;
#63436 = CARTESIAN_POINT ( 'NONE',  ( -18.68115160533190178, 1485.891698176000091, 189.2421416268200005 ) ) ;
#63437 = CARTESIAN_POINT ( 'NONE',  ( -8.477967594009999885, 1424.852341466620146, 205.3179503978689979 ) ) ;
#63438 = CARTESIAN_POINT ( 'NONE',  ( -4.280709431791439812, 1440.997461520010120, 156.3948438198679867 ) ) ;
#63439 = AXIS2_PLACEMENT_3D ( 'NONE', #109396, #108826, #15835 ) ;
#63441 = VERTEX_POINT ( 'NONE', #13406 ) ;
#63440 = CARTESIAN_POINT ( 'NONE',  ( -67.37805264080000711, 1379.747543260419889, 278.5100200678590454 ) ) ;
#63442 = VERTEX_POINT ( 'NONE', #47594 ) ;
#63443 = CARTESIAN_POINT ( 'NONE',  ( 29.71730764810000025, 1509.987350273330094, 210.0545273362199907 ) ) ;
#63444 = ORIENTED_EDGE ( 'NONE', *, *, #36136, .T. ) ;
#63445 = CARTESIAN_POINT ( 'NONE',  ( -0.4829651199533262496, 1457.465871680693226, 199.6046590496274575 ) ) ;
#63446 = DIRECTION ( 'NONE',  ( -1.755985294532469921E-16, 1.000000000000000000, -1.338183447452831989E-16 ) ) ;
#63448 = CARTESIAN_POINT ( 'NONE',  ( 23.99815499239999994, 1446.810867530319911, 216.6209177652979747 ) ) ;
#63447 = CARTESIAN_POINT ( 'NONE',  ( 15.68557540059999766, 1410.853897593529837, 191.5168599455980143 ) ) ;
#63449 = CARTESIAN_POINT ( 'NONE',  ( 5.386185205460879644, 1432.347042709529887, 154.6076275981190236 ) ) ;
#63450 = CARTESIAN_POINT ( 'NONE',  ( -25.79081092570330114, 1450.963662666099935, 136.8144486713130163 ) ) ;
#63451 = CARTESIAN_POINT ( 'NONE',  ( -105.8048160525020052, 1378.913060387249971, 304.4117408737909614 ) ) ;
#63452 = CARTESIAN_POINT ( 'NONE',  ( 4.388734291479999605, 1410.444832901329846, 231.4150274050980158 ) ) ;
#63454 = EDGE_CURVE ( 'NONE', #94671, #42670, #81720, .T. ) ;
#63453 = DIRECTION ( 'NONE',  ( -0.7414773880254760252, 0.000000000000000000, -0.6709778558543624261 ) ) ;
#63455 = CARTESIAN_POINT ( 'NONE',  ( -5.771797464315000070, 1516.647618671360078, 211.9976960644470125 ) ) ;
#63456 = CARTESIAN_POINT ( 'NONE',  ( 41.02967923190390565, 1440.575676734689978, 134.0999999980680002 ) ) ;
#63457 = FACE_OUTER_BOUND ( 'NONE', #8067, .T. ) ;
#63458 = ORIENTED_EDGE ( 'NONE', *, *, #46825, .F. ) ;
#63459 = CARTESIAN_POINT ( 'NONE',  ( 20.33509144374850308, 1432.834507525260051, 214.7556780039420232 ) ) ;
#63460 = CARTESIAN_POINT ( 'NONE',  ( 9.334683862901423268, 1491.782840251982861, 215.1527950542473491 ) ) ;
#63461 = EDGE_LOOP ( 'NONE', ( #50758, #18314 ) ) ;
#63462 = ORIENTED_EDGE ( 'NONE', *, *, #78836, .T. ) ;
#63463 = ORIENTED_EDGE ( 'NONE', *, *, #9459, .F. ) ;
#63464 = CARTESIAN_POINT ( 'NONE',  ( -6.124171364995000033, 1514.216129015430170, 216.7908301805069868 ) ) ;
#63465 = CARTESIAN_POINT ( 'NONE',  ( 16.52740840709205372, 1514.201209519783333, 194.8160859650000987 ) ) ;
#63466 = CARTESIAN_POINT ( 'NONE',  ( 7.876852879565064747, 1451.393553377243506, 152.9815231998884428 ) ) ;
#63467 = CARTESIAN_POINT ( 'NONE',  ( 1.705087066220000169, 1507.082462650630077, 236.5153987699980007 ) ) ;
#63468 = CARTESIAN_POINT ( 'NONE',  ( 10.05341040150000076, 1462.281908926990127, 210.6545760798489937 ) ) ;
#63469 = AXIS2_PLACEMENT_3D ( 'NONE', #4190, #38323, #45110 ) ;
#63470 = CARTESIAN_POINT ( 'NONE',  ( -14.28029386204369899, 1390.367275669339961, 209.8449220790990069 ) ) ;
#63471 = CARTESIAN_POINT ( 'NONE',  ( -67.48208812431644787, 1379.745290141752776, 277.3802860916713371 ) ) ;
#63472 = CARTESIAN_POINT ( 'NONE',  ( -1.720902727859999981, 1464.150605286389919, 199.3240545488989710 ) ) ;
#63473 = ADVANCED_FACE ( 'NONE', ( #75566 ), #519, .F. ) ;
#63474 = CARTESIAN_POINT ( 'NONE',  ( -0.7347961819880001189, 1487.759023923330005, 231.0371655964979709 ) ) ;
#63475 = CARTESIAN_POINT ( 'NONE',  ( 6.288099950509999481, 1416.823872462129884, 191.8704827068980308 ) ) ;
#63477 = VECTOR ( 'NONE', #63453, 1000.000000000000114 ) ;
#63476 = CARTESIAN_POINT ( 'NONE',  ( -49.39991366742589918, 1384.617024020139752, 224.3629336449129994 ) ) ;
#63478 = ORIENTED_EDGE ( 'NONE', *, *, #54969, .F. ) ;
#63479 = CARTESIAN_POINT ( 'NONE',  ( -2.494758036134999912, 1516.937508036699910, 207.4208181092269854 ) ) ;
#63480 = VERTEX_POINT ( 'NONE', #67165 ) ;
#63481 = CARTESIAN_POINT ( 'NONE',  ( 27.65997673997260264, 1440.913060387330006, 246.7466754288900006 ) ) ;
#63482 = CARTESIAN_POINT ( 'NONE',  ( -15.17209163809999950, 1508.688025133729980, 184.8363905680980110 ) ) ;
#63483 = VERTEX_POINT ( 'NONE', #25118 ) ;
#63484 = CARTESIAN_POINT ( 'NONE',  ( -8.799999999999998934, 1413.913060387329779, 209.1218459616989946 ) ) ;
#63485 = CARTESIAN_POINT ( 'NONE',  ( -14.27950570660000018, 1410.344120410830101, 190.3743234292979878 ) ) ;
#63486 = CARTESIAN_POINT ( 'NONE',  ( -17.34960988009670757, 1508.455927730609119, 212.8242482004856413 ) ) ;
#63487 = CARTESIAN_POINT ( 'NONE',  ( -24.67319088250000192, 1441.246434465200082, 210.6951902311179765 ) ) ;
#63488 = CARTESIAN_POINT ( 'NONE',  ( -6.437876012944840021, 1435.112046181850019, 216.3672298223000041 ) ) ;
#63489 = DIRECTION ( 'NONE',  ( 1.755985294532464991E-16, -1.000000000000000000, 1.338183447452830017E-16 ) ) ;
#63490 = CARTESIAN_POINT ( 'NONE',  ( 0.2153512683669999983, 1405.989301470729970, 266.9611412585979906 ) ) ;
#63491 = DIRECTION ( 'NONE',  ( -0.9455185755993178454, 0.000000000000000000, 0.3255681544571537578 ) ) ;
#63492 = CARTESIAN_POINT ( 'NONE',  ( -5.797231311010000887, 1507.943299984489840, 220.7428112414989982 ) ) ;
#63494 = CARTESIAN_POINT ( 'NONE',  ( -30.31940284292399213, 1512.187213306747481, 222.4933038710547919 ) ) ;
#63493 = CARTESIAN_POINT ( 'NONE',  ( 4.509664962759999618, 1465.693492029729896, 233.9834801382980061 ) ) ;
#63495 = B_SPLINE_SURFACE_WITH_KNOTS ( 'NONE', 5, 5, ( 
 ( #84878, #24422, #84343, #7631, #101671, #24960 ),
 ( #42342, #58607, #76495, #72001, #70898, #97160 ),
 ( #62498, #36159, #106114, #70343, #3133, #87669 ),
 ( #9844, #19886, #44009, #96619, #52421, #61939 ),
 ( #103903, #2024, #61385, #11512, #35594, #95504 ),
 ( #27747, #96058, #46237, #78148, #104455, #20431 ),
 ( #80370, #12053, #1449, #69785, #19327, #27203 ),
 ( #3686, #78711, #18774, #52972, #105015, #105575 ),
 ( #37812, #79826, #87104, #37263, #18226, #79272 ),
 ( #28863, #54093, #28305, #54638, #53529, #88769 ),
 ( #2582, #10958, #29391, #10392, #88218, #44562 ),
 ( #45687, #94956, #36704, #86548, #71461, #63056 ) ),
 .UNSPECIFIED., .F., .F., .F.,
 ( 6, 3, 3, 6 ),
 ( 6, 6 ),
 ( 3.672001930560000016, 6.062162762929999893, 7.801458206499999548, 8.912489289840001661 ),
 ( 0.000000000000000000, 1.000000000000000000 ),
 .UNSPECIFIED. ) ;
#63496 = EDGE_CURVE ( 'NONE', #15990, #81018, #83940, .T. ) ;
#63497 = CARTESIAN_POINT ( 'NONE',  ( -1.708747662384999977, 1517.213554313520035, 216.0740123525270064 ) ) ;
#63498 = CARTESIAN_POINT ( 'NONE',  ( 0.1666560433379990214, 1469.576466606489930, 216.4329724472190151 ) ) ;
#63499 = DIRECTION ( 'NONE',  ( 0.000000000000000000, 0.000000000000000000, -1.000000000000000000 ) ) ;
#63500 = CARTESIAN_POINT ( 'NONE',  ( 18.27523319681197833, 1446.550731797170101, 215.9569883731650748 ) ) ;
#63501 = CARTESIAN_POINT ( 'NONE',  ( 7.724732408895000013, 1517.133889586189980, 212.3822030989969960 ) ) ;
#63502 = CARTESIAN_POINT ( 'NONE',  ( -21.99590692660000002, 1506.811133727630022, 209.5040961443579874 ) ) ;
#63503 =( BOUNDED_CURVE ( )  B_SPLINE_CURVE ( 3, ( #94163, #17433, #43236, #68447 ),
 .UNSPECIFIED., .F., .F. ) 
 B_SPLINE_CURVE_WITH_KNOTS ( ( 4, 4 ),
 ( 1.036305746500566061, 2.105308905912994799 ),
 .UNSPECIFIED. ) 
 CURVE ( )  GEOMETRIC_REPRESENTATION_ITEM ( )  RATIONAL_B_SPLINE_CURVE ( ( 1.000000000000000000, 0.9070150916864841983, 0.9070150916864841983, 1.000000000000000000 ) ) 
 REPRESENTATION_ITEM ( '' )  );
#63504 = ADVANCED_FACE ( 'NONE', ( #76645 ), #59111, .T. ) ;
#63505 = PLANE ( 'NONE',  #88680 ) ;
#63507 = EDGE_LOOP ( 'NONE', ( #88645, #93266, #19863, #61591 ) ) ;
#63506 = CARTESIAN_POINT ( 'NONE',  ( -113.4000000000000057, 1386.785055403669958, 297.3836343121590176 ) ) ;
#63508 = CARTESIAN_POINT ( 'NONE',  ( -18.46505095605026270, 1509.557874174373865, 231.0973782675585255 ) ) ;
#63509 = CARTESIAN_POINT ( 'NONE',  ( 18.33597341320000140, 1458.591204236030080, 232.0308503239980098 ) ) ;
#63510 = CARTESIAN_POINT ( 'NONE',  ( 9.304705586386592842, 1483.500584759331105, 214.3952978072885003 ) ) ;
#63511 = CARTESIAN_POINT ( 'NONE',  ( -15.43898598230000019, 1415.677402227490120, 208.9970960677119933 ) ) ;
#63512 = CARTESIAN_POINT ( 'NONE',  ( -1.480417309695410077, 1508.374054581489872, 237.5951421557219874 ) ) ;
#63513 = FACE_OUTER_BOUND ( 'NONE', #100026, .T. ) ;
#63514 = CIRCLE ( 'NONE', #47413, 1.999999999999999556 ) ;
#63515 = B_SPLINE_CURVE_WITH_KNOTS ( 'NONE', 3,
 ( #59944, #26871, #1137, #103004, #86217, #26301, #53191, #77287, #1688, #34163, #93503, #102455, #52637, #61061, #7852, #60491, #76169, #94612, #67785 ),
 .UNSPECIFIED., .F., .F.,
 ( 4, 2, 2, 2, 1, 1, 1, 2, 2, 2, 4 ),
 ( 0.000000000000000000, 0.2500000000002982059, 0.3750000000004471978, 0.4375000000005346834, 0.4687500000005783707, 0.4843750000006000755, 0.4921875000006109002, 0.4960937500005973555, 0.5000000000005837553, 0.7500000000002919887, 1.000000000000000000 ),
 .UNSPECIFIED. ) ;
#63517 = CARTESIAN_POINT ( 'NONE',  ( 2.500000000000000000, 1419.365153366229833, 145.1079871556979981 ) ) ;
#63516 = CARTESIAN_POINT ( 'NONE',  ( -20.81941094909999990, 1457.442873729829898, 223.8287928082980045 ) ) ;
#63518 = CARTESIAN_POINT ( 'NONE',  ( -9.009356499370060334, 1449.261709350619867, 210.8259634658180062 ) ) ;
#63519 = CARTESIAN_POINT ( 'NONE',  ( -104.7786280602689999, 1380.751497738820035, 308.1052390028799550 ) ) ;
#63520 = ORIENTED_EDGE ( 'NONE', *, *, #103593, .T. ) ;
#63521 = CARTESIAN_POINT ( 'NONE',  ( 2.865911516645000212, 1516.906233342200039, 205.6598507734169914 ) ) ;
#63522 = CARTESIAN_POINT ( 'NONE',  ( 2.086239376750000041, 1406.540766230330064, 269.4971845159980148 ) ) ;
#63523 = VECTOR ( 'NONE', #32061, 1000.000000000000000 ) ;
#63524 = CARTESIAN_POINT ( 'NONE',  ( -0.008608266642480520009, 1515.483924129489878, 213.3566978088589963 ) ) ;
#63525 = CARTESIAN_POINT ( 'NONE',  ( 6.625222801663490202, 1473.589452326439869, 270.3925718229160111 ) ) ;
#63526 = DIRECTION ( 'NONE',  ( -0.5600256381126521577, -0.8284752770339720573, 0.000000000000000000 ) ) ;
#63527 = CARTESIAN_POINT ( 'NONE',  ( 10.23376715243824897, 1422.709367747187798, 137.1241318772909779 ) ) ;
#63528 = B_SPLINE_CURVE_WITH_KNOTS ( 'NONE', 3,
 ( #19944, #87730, #62552, #104510 ),
 .UNSPECIFIED., .F., .F.,
 ( 4, 4 ),
 ( 0.000000000000000000, 0.0002960034161023848394 ),
 .UNSPECIFIED. ) ;
#63529 = CARTESIAN_POINT ( 'NONE',  ( 4.811461131969293703, 1516.551188146008599, 199.9949300312234755 ) ) ;
#63530 = DIRECTION ( 'NONE',  ( -0.04448252661992505713, -0.9990097882110241523, -0.0008648029096898162240 ) ) ;
#63531 = CARTESIAN_POINT ( 'NONE',  ( 0.2719187923920010075, 1432.443060607389953, 200.6707351473390020 ) ) ;
#63532 = CARTESIAN_POINT ( 'NONE',  ( 14.38276615817169635, 1509.537722092532931, 235.4493228184925897 ) ) ;
#63533 = CARTESIAN_POINT ( 'NONE',  ( -14.02570581375069914, 1415.492117401580117, 220.9500074586500205 ) ) ;
#63534 = DIRECTION ( 'NONE',  ( -9.462326934583649054E-47, 1.000000000000000000, -1.836970198721029688E-16 ) ) ;
#63535 = ORIENTED_EDGE ( 'NONE', *, *, #100623, .T. ) ;
#63536 = CARTESIAN_POINT ( 'NONE',  ( -17.26713005559999914, 1428.027535766330175, 234.3916895593979746 ) ) ;
#63537 = CARTESIAN_POINT ( 'NONE',  ( 9.190374286110708724, 1468.398850889019968, 204.6732001591689993 ) ) ;
#63538 = CARTESIAN_POINT ( 'NONE',  ( -0.7691164859940000653, 1475.314785482929892, 269.4984833451979966 ) ) ;
#63539 = FACE_OUTER_BOUND ( 'NONE', #85184, .T. ) ;
#63540 = CARTESIAN_POINT ( 'NONE',  ( -11.97304278378637576, 1513.029508366000300, 192.5452993188944504 ) ) ;
#63541 = CARTESIAN_POINT ( 'NONE',  ( -3.089550218706188733, 1448.274272998623474, 184.5587172890779186 ) ) ;
#63542 = CARTESIAN_POINT ( 'NONE',  ( -41.12117611683139273, 1384.782461838570043, 244.1305867940789938 ) ) ;
#63543 = CARTESIAN_POINT ( 'NONE',  ( 12.06005565936200163, 1491.389938827579954, 206.7797953803130326 ) ) ;
#63544 = DIRECTION ( 'NONE',  ( -0.7071067811865492381, 0.000000000000000000, -0.7071067811865457964 ) ) ;
#63545 = CARTESIAN_POINT ( 'NONE',  ( 26.79919712355280126, 1436.600546571140057, 136.7629453747840103 ) ) ;
#63546 = CIRCLE ( 'NONE', #45639, 1.000000000000001554 ) ;
#63547 = CARTESIAN_POINT ( 'NONE',  ( -10.11703718938549912, 1396.266355110979930, 213.6078271767569845 ) ) ;
#63548 = CARTESIAN_POINT ( 'NONE',  ( -15.03157878520000068, 1422.458659762129855, 229.1221048155979929 ) ) ;
#63549 = CARTESIAN_POINT ( 'NONE',  ( -44.92382433299999889, 1440.723416683769983, 269.6913831256979961 ) ) ;
#63550 = ORIENTED_EDGE ( 'NONE', *, *, #29592, .T. ) ;
#63551 = CARTESIAN_POINT ( 'NONE',  ( -16.81223434880759982, 1414.913060387349788, 207.5743820648510223 ) ) ;
#63552 = CARTESIAN_POINT ( 'NONE',  ( 2.923263585169999956, 1409.521015940530106, 231.4220185117980009 ) ) ;
#63553 = AXIS2_PLACEMENT_3D ( 'NONE', #71717, #10103, #1175 ) ;
#63554 = CARTESIAN_POINT ( 'NONE',  ( 3.829620113920000346, 1515.551704408389924, 211.4519800804890224 ) ) ;
#63556 = CARTESIAN_POINT ( 'NONE',  ( -12.80694037396500029, 1512.080583811389943, 193.5218228818669957 ) ) ;
#63555 = CARTESIAN_POINT ( 'NONE',  ( 10.35419722570000012, 1425.138650036730041, 115.7291061860980079 ) ) ;
#63557 = CARTESIAN_POINT ( 'NONE',  ( -16.14705515586277329, 1409.476923469505209, 225.0742284443501546 ) ) ;
#63558 = CARTESIAN_POINT ( 'NONE',  ( 4.268211237764689692, 1423.922164383429845, 183.9128890805280037 ) ) ;
#63559 = CARTESIAN_POINT ( 'NONE',  ( -4.616861546545000472, 1516.666407245520077, 201.4093549791169835 ) ) ;
#63560 = CARTESIAN_POINT ( 'NONE',  ( 7.996683413600000456, 1427.037929587379949, 212.0417767193789871 ) ) ;
#63561 = CARTESIAN_POINT ( 'NONE',  ( -2.446787376320000096, 1432.353341358199941, 150.2884730787980061 ) ) ;
#63562 = CARTESIAN_POINT ( 'NONE',  ( 1.454856650950000052, 1507.661996469930045, 181.0451578312979848 ) ) ;
#63563 = PLANE ( 'NONE',  #88338 ) ;
#63564 = CARTESIAN_POINT ( 'NONE',  ( -42.03938205346800316, 1377.690944531520017, 233.5611963710439909 ) ) ;
#63565 = CARTESIAN_POINT ( 'NONE',  ( 6.556794880282631688, 1366.140135904955741, 209.6218459617148824 ) ) ;
#63567 = ORIENTED_EDGE ( 'NONE', *, *, #107486, .F. ) ;
#63566 = CARTESIAN_POINT ( 'NONE',  ( -16.66186295847979792, 1379.591909316719921, 212.1494488913359930 ) ) ;
#63568 = EDGE_LOOP ( 'NONE', ( #63105, #65021, #16176, #71336 ) ) ;
#63569 = CARTESIAN_POINT ( 'NONE',  ( -8.264168053159998806, 1396.728728318830008, 199.4337832187279957 ) ) ;
#63570 = CARTESIAN_POINT ( 'NONE',  ( 0.4780929317929359934, 1499.039778920739991, 237.0126458204609889 ) ) ;
#63571 = CARTESIAN_POINT ( 'NONE',  ( -16.53869145193961288, 1435.074985393188399, 146.6152319182869803 ) ) ;
#63572 = CARTESIAN_POINT ( 'NONE',  ( 3.738304505813290657, 1499.328994237659117, 198.3873084196136745 ) ) ;
#63574 = CARTESIAN_POINT ( 'NONE',  ( -21.53299174964140050, 1506.014650851819852, 209.2005993430840078 ) ) ;
#63573 = CARTESIAN_POINT ( 'NONE',  ( -7.553780601869999778, 1384.400324961100068, 219.0644599357090101 ) ) ;
#63575 = B_SPLINE_CURVE_WITH_KNOTS ( 'NONE', 5,
 ( #19440, #104004, #45233, #27301, #2688, #61482 ),
 .UNSPECIFIED., .F., .F.,
 ( 6, 6 ),
 ( -1.999999943015589920, 0.000000000000000000 ),
 .UNSPECIFIED. ) ;
#63576 = CARTESIAN_POINT ( 'NONE',  ( 3.363175565480000184, 1429.769277944529904, 184.9623219864980115 ) ) ;
#63577 = DIRECTION ( 'NONE',  ( 0.8090169943749465631, 0.000000000000000000, -0.5877852522924742473 ) ) ;
#63578 = FACE_OUTER_BOUND ( 'NONE', #5964, .T. ) ;
#63579 = CARTESIAN_POINT ( 'NONE',  ( 40.09012238588890398, 1439.133113879990105, 136.1039124235030044 ) ) ;
#63580 = CARTESIAN_POINT ( 'NONE',  ( 3.969839694839903288, 1370.280274951255933, 210.6218459617030021 ) ) ;
#63581 = CARTESIAN_POINT ( 'NONE',  ( -40.41548887560000480, 1443.621016936120213, 137.1123791864980035 ) ) ;
#63582 = CARTESIAN_POINT ( 'NONE',  ( -6.075257814475249596, 1406.559263763209856, 269.2809304965529691 ) ) ;
#63583 = CARTESIAN_POINT ( 'NONE',  ( 41.66135186410000557, 1443.796891309130160, 135.6885248007979783 ) ) ;
#63584 = EDGE_LOOP ( 'NONE', ( #16493, #88987, #83629, #20432 ) ) ;
#63585 = FACE_OUTER_BOUND ( 'NONE', #27596, .T. ) ;
#63586 = CARTESIAN_POINT ( 'NONE',  ( 11.91277487560000026, 1442.215011169370200, 187.5867736087979836 ) ) ;
#63587 = VERTEX_POINT ( 'NONE', #102929 ) ;
#63588 = ORIENTED_EDGE ( 'NONE', *, *, #56884, .T. ) ;
#63589 = DIRECTION ( 'NONE',  ( -0.9993779840598802089, -0.0009463129492438572803, -0.03525265193161980504 ) ) ;
#63590 = CARTESIAN_POINT ( 'NONE',  ( -13.63106836819999934, 1462.228096604230132, 230.1036610636979844 ) ) ;
#63591 = CARTESIAN_POINT ( 'NONE',  ( -0.7369042090349989804, 1517.080322339569875, 214.1333973382469935 ) ) ;
#63592 = CARTESIAN_POINT ( 'NONE',  ( -14.34382872122290031, 1380.323822069550033, 209.7285467014039853 ) ) ;
#63593 = ORIENTED_EDGE ( 'NONE', *, *, #79156, .F. ) ;
#63594 = CARTESIAN_POINT ( 'NONE',  ( -14.35118438041689970, 1509.480705576550008, 182.9751542011199774 ) ) ;
#63595 = CARTESIAN_POINT ( 'NONE',  ( -70.04184978290001595, 1379.439320607440095, 279.7464857826589650 ) ) ;
#63596 = EDGE_CURVE ( 'NONE', #41404, #6924, #22634, .T. ) ;
#63597 = AXIS2_PLACEMENT_3D ( 'NONE', #2785, #88420, #64336 ) ;
#63598 = CARTESIAN_POINT ( 'NONE',  ( 18.81809407629999953, 1416.219761279530076, 210.6452591561279917 ) ) ;
#63599 = CARTESIAN_POINT ( 'NONE',  ( -4.040527342105000308, 1516.815231249920089, 204.5109077207270047 ) ) ;
#63600 = CARTESIAN_POINT ( 'NONE',  ( -12.09982269103889863, 1489.891875091150041, 210.9072642413369749 ) ) ;
#63601 = EDGE_CURVE ( 'NONE', #23046, #5040, #4489, .T. ) ;
#63602 = B_SPLINE_SURFACE_WITH_KNOTS ( 'NONE', 5, 4, ( 
 ( #64252, #59695, #51848, #41776, #101656 ),
 ( #94365, #50203, #76481, #16000, #24944 ),
 ( #93275, #84328, #110633, #68657, #75404 ),
 ( #33361, #67001, #34482, #355, #67554 ),
 ( #8160, #92182, #25505, #42891, #17647 ),
 ( #85985, #35026, #68113, #9283, #33918 ) ),
 .UNSPECIFIED., .F., .F., .F.,
 ( 6, 6 ),
 ( 5, 5 ),
 ( 0.000000000000000000, 111.1101480259999903 ),
 ( 25.81581217359999769, 39.03307591160000101 ),
 .UNSPECIFIED. ) ;
#63603 = CARTESIAN_POINT ( 'NONE',  ( 11.06154325740661015, 1433.015924775765143, 151.7088343760975704 ) ) ;
#63604 = CARTESIAN_POINT ( 'NONE',  ( -3.069376825600000025, 1409.187778979130144, 231.9248983289979833 ) ) ;
#63606 = ORIENTED_EDGE ( 'NONE', *, *, #24097, .T. ) ;
#63605 = CARTESIAN_POINT ( 'NONE',  ( -7.326859461719999800, 1453.313060387329870, 190.4665504513979783 ) ) ;
#63607 = CARTESIAN_POINT ( 'NONE',  ( -13.85778478534841263, 1434.981447914178034, 148.6210686895626054 ) ) ;
#63608 = DIRECTION ( 'NONE',  ( -0.8796244824232881676, -0.3860830610750210501, -0.2778500312623770063 ) ) ;
#63609 = CARTESIAN_POINT ( 'NONE',  ( -7.020660495122976741, 1374.031200045389824, 205.2864416528653635 ) ) ;
#63610 = CARTESIAN_POINT ( 'NONE',  ( 19.55988977460000200, 1474.636381753090063, 214.0184790771390055 ) ) ;
#63611 = B_SPLINE_CURVE_WITH_KNOTS ( 'NONE', 3,
 ( #449, #9376, #44092, #34570, #78230, #102859, #44651, #69864, #18855, #95586, #53051, #11040, #10481, #79348, #78792, #85507, #2662, #2108, #69306, #86080, #26156, #36234, #27836, #62016, #35124, #60342, #96136, #17737, #51938, #36787, #19415, #70980, #43539, #53616, #26718, #25601, #93913, #77684, #997, #103413, #81523, #11589, #3764, #89935, #20509, #97236, #88295, #12129, #38427, #5386, #46864, #80451, #22152, #80994, #30585, #79902, #4824, #4300, #12684, #82083, #88845, #29476, #46323, #21611 ),
 .UNSPECIFIED., .F., .F.,
 ( 4, 3, 3, 3, 3, 3, 3, 3, 3, 3, 3, 3, 3, 3, 3, 3, 3, 3, 3, 3, 3, 4 ),
 ( -14.97205155145559985, -14.82652002214629938, -14.54016898290000093, -14.44422383253650111, -14.18616176382849936, -13.96389086917469946, -13.75628494548289993, -13.55954878687630050, -13.48778832326109978, -13.41168605665509972, -13.29681976037920066, -13.03955770695989891, -12.77367886414240061, -12.48588961213089910, -12.17406815308810053, -11.81735425579999976, -11.73764647089110014, -11.37242228474149996, -11.02426971002140021, -10.95328097456370031, -10.66065571756510089, -10.38571964170729878 ),
 .UNSPECIFIED. ) ;
#63612 = CARTESIAN_POINT ( 'NONE',  ( 25.61285747430000015, 1414.331920139429940, 270.3573890238980084 ) ) ;
#63613 = CARTESIAN_POINT ( 'NONE',  ( 4.623787969365000805, 1516.947419719950176, 212.5709951659769956 ) ) ;
#63614 = CARTESIAN_POINT ( 'NONE',  ( -68.00907612829999493, 1379.746097695369826, 278.4774409410590010 ) ) ;
#63615 = CARTESIAN_POINT ( 'NONE',  ( 23.43132253519999963, 1410.390761240029860, 207.9091969211580135 ) ) ;
#63616 = CARTESIAN_POINT ( 'NONE',  ( 0.008003304918488279504, 1508.487575044294545, 237.9830183513317365 ) ) ;
#63617 = CARTESIAN_POINT ( 'NONE',  ( 10.93200248603220004, 1426.108105161469894, 194.7599858398060064 ) ) ;
#63619 = CARTESIAN_POINT ( 'NONE',  ( -7.708918532268509871, 1516.529980546400111, 211.4477551148110024 ) ) ;
#63618 = AXIS2_PLACEMENT_3D ( 'NONE', #54280, #54823, #22262 ) ;
#63620 = CARTESIAN_POINT ( 'NONE',  ( -7.332063977575000280, 1516.939491476980038, 209.1325772641960157 ) ) ;
#63621 = VERTEX_POINT ( 'NONE', #45281 ) ;
#63622 = CARTESIAN_POINT ( 'NONE',  ( 4.185430511625449768, 1421.177391087800061, 185.2742621543330017 ) ) ;
#63623 = CARTESIAN_POINT ( 'NONE',  ( -1.332234214539999906, 1417.916672854830040, 233.3009772848979821 ) ) ;
#63624 = CARTESIAN_POINT ( 'NONE',  ( -86.93140579660001777, 1384.976593077780080, 307.7302223600589741 ) ) ;
#63625 = ORIENTED_EDGE ( 'NONE', *, *, #94010, .F. ) ;
#63626 = CARTESIAN_POINT ( 'NONE',  ( -30.52320602891570189, 1385.231135277879957, 228.5881811678719941 ) ) ;
#63627 = DIRECTION ( 'NONE',  ( 0.9510565162951566398, 0.000000000000000000, 0.3090169943749382919 ) ) ;
#63628 = VECTOR ( 'NONE', #30780, 1000.000000000000000 ) ;
#63629 =( BOUNDED_CURVE ( )  B_SPLINE_CURVE ( 3, ( #66181, #100301, #84592, #57776 ),
 .UNSPECIFIED., .F., .T. ) 
 B_SPLINE_CURVE_WITH_KNOTS ( ( 4, 4 ),
 ( 4.146398541727710274, 5.278376838302800245 ),
 .UNSPECIFIED. ) 
 CURVE ( )  GEOMETRIC_REPRESENTATION_ITEM ( )  RATIONAL_B_SPLINE_CURVE ( ( 1.000000000000000000, 0.8960390544622802711, 0.8960390544622802711, 1.000000000000000000 ) ) 
 REPRESENTATION_ITEM ( '' )  );
#63630 = CARTESIAN_POINT ( 'NONE',  ( 4.487249775049700240, 1509.038615934839981, 206.6339108193819811 ) ) ;
#63631 = CARTESIAN_POINT ( 'NONE',  ( -11.60004869885203682, 1411.254281879943164, 135.5999999980979851 ) ) ;
#63632 = CARTESIAN_POINT ( 'NONE',  ( 12.73217514220000091, 1421.428024357469894, 206.3441494772290241 ) ) ;
#63633 = CARTESIAN_POINT ( 'NONE',  ( 0.02358223654491949789, 1420.444546422549820, 182.6733859946079974 ) ) ;
#63635 = CARTESIAN_POINT ( 'NONE',  ( -16.39908139913352869, 1416.805070253819395, 208.0671872555761297 ) ) ;
#63634 = CARTESIAN_POINT ( 'NONE',  ( 4.618119666265000589, 1516.706638732659940, 216.0591847158069925 ) ) ;
#63636 = CARTESIAN_POINT ( 'NONE',  ( 19.34325791780000259, 1509.569025932029945, 187.1036586203979937 ) ) ;
#63637 = CARTESIAN_POINT ( 'NONE',  ( 11.40429614103280187, 1470.873877624120041, 208.7845352330780315 ) ) ;
#63638 = VERTEX_POINT ( 'NONE', #96774 ) ;
#63639 = CARTESIAN_POINT ( 'NONE',  ( -3.454119954834999895, 1516.594591938570147, 201.4112355291069889 ) ) ;
#63640 = CARTESIAN_POINT ( 'NONE',  ( -7.512750246095000861, 1509.038615934239942, 214.6352815282469919 ) ) ;
#63641 = ORIENTED_EDGE ( 'NONE', *, *, #39061, .F. ) ;
#63642 = CARTESIAN_POINT ( 'NONE',  ( 0.08925506140130000376, 1497.012273211330012, 230.7310177360980106 ) ) ;
#63643 = CARTESIAN_POINT ( 'NONE',  ( 4.541133980909999757, 1426.446980476709996, 211.3175313701290179 ) ) ;
#63644 = CARTESIAN_POINT ( 'NONE',  ( 8.133961203403233142, 1424.059811672474325, 195.8560981452540659 ) ) ;
#63645 = CARTESIAN_POINT ( 'NONE',  ( 2.659511198940000209, 1441.714673586189974, 218.2865353327090077 ) ) ;
#63646 = CARTESIAN_POINT ( 'NONE',  ( -26.43747909245940164, 1508.499208940789913, 201.5081742940070058 ) ) ;
#63647 = CARTESIAN_POINT ( 'NONE',  ( -2.710413728979999881, 1447.398499818599930, 159.5173236502980103 ) ) ;
#63648 = CARTESIAN_POINT ( 'NONE',  ( -18.43681981810000181, 1425.072882130230028, 225.4380530597979941 ) ) ;
#63649 = CARTESIAN_POINT ( 'NONE',  ( -18.81929060680000276, 1436.388221856100245, 146.6704585558979943 ) ) ;
#63650 = CARTESIAN_POINT ( 'NONE',  ( 33.92643251289999995, 1451.728352207130001, 135.1493744902979870 ) ) ;
#63651 = CARTESIAN_POINT ( 'NONE',  ( 17.04970435369999748, 1508.515036628130019, 187.9166768603979847 ) ) ;
#63653 = CARTESIAN_POINT ( 'NONE',  ( -18.67271768969374435, 1437.373477116879258, 211.9268211480253683 ) ) ;
#63652 = CARTESIAN_POINT ( 'NONE',  ( 1.137641289866240024, 1410.327604111319943, 232.8584434023429992 ) ) ;
#63654 = CARTESIAN_POINT ( 'NONE',  ( -10.15398179789089994, 1472.533710365230036, 209.9201027492950118 ) ) ;
#63655 = ORIENTED_EDGE ( 'NONE', *, *, #61432, .T. ) ;
#63656 = DIRECTION ( 'NONE',  ( 0.7071093782156816498, -3.166819169022306488E-06, 0.7071041841407837980 ) ) ;
#63657 = CARTESIAN_POINT ( 'NONE',  ( 11.90008666459999986, 1434.920851464509951, 147.6452002888979962 ) ) ;
#63658 = CARTESIAN_POINT ( 'NONE',  ( 11.29267550753220029, 1470.546782610659875, 207.7331957881270057 ) ) ;
#63659 = DIRECTION ( 'NONE',  ( -9.714451465470110893E-14, 0.000000000000000000, 1.000000000000000000 ) ) ;
#63660 = CARTESIAN_POINT ( 'NONE',  ( 8.775825618903722258, 1374.413060387289988, 213.9161013477410336 ) ) ;
#63661 = CARTESIAN_POINT ( 'NONE',  ( -2.485125933802709852, 1524.547873515805350, 242.5340162392059540 ) ) ;
#63662 = CARTESIAN_POINT ( 'NONE',  ( 18.37215797060000000, 1453.313060387329870, 217.1322599118979895 ) ) ;
#63663 = CYLINDRICAL_SURFACE ( 'NONE', #77075, 0.4999999999999449329 ) ;
#63664 = CARTESIAN_POINT ( 'NONE',  ( 4.709068530708940159, 1495.147136111799909, 220.5787748165419941 ) ) ;
#63665 = CARTESIAN_POINT ( 'NONE',  ( 22.24401329409999661, 1475.958617299990010, 209.7631870919539949 ) ) ;
#63666 = CARTESIAN_POINT ( 'NONE',  ( -15.29087862775659978, 1415.677402202089979, 208.7697798501069997 ) ) ;
#63667 = B_SPLINE_CURVE_WITH_KNOTS ( 'NONE', 3,
 ( #14385, #73215, #108466, #107359, #48579, #31749, #30655, #100058, #3836, #72674, #98949, #98404, #54777, #37964, #21676, #56422, #29549, #80519, #81054, #21123, #106263, #55328, #12194, #46387, #63735, #4368, #38497, #55882, #13829, #48016, #82153, #67585, #16034, #77083, #8192, #7652, #42358, #102259, #16569, #23345, #83810, #75437, #58078 ),
 .UNSPECIFIED., .F., .F.,
 ( 4, 3, 3, 3, 3, 3, 3, 3, 3, 3, 3, 3, 3, 3, 4 ),
 ( -8.338949519795640697, -8.327257911908940713, -8.213231001270830944, -8.087512482746008757, -7.836075445696390140, -7.703760222490700471, -7.408891911687140563, -7.099196593615670459, -6.815814698362330226, -6.550724326761839578, -6.491399922859719673, -6.353894249153509755, -6.157064171545170161, -6.019682015367260774, -5.901461776375070301 ),
 .UNSPECIFIED. ) ;
#63668 = AXIS2_PLACEMENT_3D ( 'NONE', #39963, #56221, #23147 ) ;
#63669 = EDGE_CURVE ( 'NONE', #21613, #104968, #44107, .T. ) ;
#63670 = CARTESIAN_POINT ( 'NONE',  ( -109.7600093021320049, 1383.545064258730008, 311.3057984900200381 ) ) ;
#63671 = CARTESIAN_POINT ( 'NONE',  ( 3.959152859930000101, 1428.396642669490120, 216.3690266601789745 ) ) ;
#63673 = ORIENTED_EDGE ( 'NONE', *, *, #105531, .T. ) ;
#63672 = CARTESIAN_POINT ( 'NONE',  ( 13.55421397129999939, 1497.816254223590022, 226.3870761728989862 ) ) ;
#63674 = CARTESIAN_POINT ( 'NONE',  ( -113.4000000000000057, 1380.131807193299892, 307.5349059445590001 ) ) ;
#63675 = EDGE_CURVE ( 'NONE', #73175, #31615, #64806, .T. ) ;
#63676 = CARTESIAN_POINT ( 'NONE',  ( 12.26154099264659969, 1512.129944624190102, 223.9167924943490107 ) ) ;
#63677 = ORIENTED_EDGE ( 'NONE', *, *, #13848, .T. ) ;
#63678 = ORIENTED_EDGE ( 'NONE', *, *, #82224, .F. ) ;
#63679 = CARTESIAN_POINT ( 'NONE',  ( 17.94598849933589690, 1415.434635989099888, 209.7830392791789791 ) ) ;
#63680 = CARTESIAN_POINT ( 'NONE',  ( -109.5347831020000058, 1384.920243598159914, 297.1230830264590281 ) ) ;
#63681 = DIRECTION ( 'NONE',  ( 0.6665120492724808665, 0.000000000000000000, 0.7454942576402571186 ) ) ;
#63683 = CARTESIAN_POINT ( 'NONE',  ( -29.63060422040000219, 1444.770720791339954, 238.0637335945980055 ) ) ;
#63682 = CARTESIAN_POINT ( 'NONE',  ( 32.04160921650328930, 1421.195714791004548, 269.4938129757199476 ) ) ;
#63684 = CARTESIAN_POINT ( 'NONE',  ( -19.88543994140000137, 1484.719660939830192, 190.7434707760979791 ) ) ;
#63685 = CARTESIAN_POINT ( 'NONE',  ( -11.71863204979999828, 1433.641944146899959, 150.9519096011979684 ) ) ;
#63686 = CARTESIAN_POINT ( 'NONE',  ( 26.71146732620000108, 1509.845845380629953, 197.1819887268980267 ) ) ;
#63687 = CARTESIAN_POINT ( 'NONE',  ( -19.52684841499999990, 1485.866921902229933, 190.0057045620980034 ) ) ;
#63688 = CARTESIAN_POINT ( 'NONE',  ( -3.026951662149999667, 1443.662240191790033, 218.7413276925990147 ) ) ;
#63689 = CARTESIAN_POINT ( 'NONE',  ( 5.020440211750000437, 1420.408409142929941, 185.9185919516980334 ) ) ;
#63690 = CARTESIAN_POINT ( 'NONE',  ( -0.3770322115495070014, 1515.150283736280016, 213.4490560809049953 ) ) ;
#63691 = DIRECTION ( 'NONE',  ( 0.9455185755993177343, 0.000000000000000000, -0.3255681544571540909 ) ) ;
#63692 = CARTESIAN_POINT ( 'NONE',  ( -113.4000000000000057, 1379.913060387289988, 304.2218459572590064 ) ) ;
#63693 = B_SPLINE_CURVE_WITH_KNOTS ( 'NONE', 3,
 ( #95407, #35490, #78043, #1923, #70247, #264, #69684 ),
 .UNSPECIFIED., .F., .F.,
 ( 4, 3, 4 ),
 ( -167.5289128729999959, -132.8626999427419833, -78.04659677155639486 ),
 .UNSPECIFIED. ) ;
#63694 = CARTESIAN_POINT ( 'NONE',  ( 33.17484411121986909, 1525.713797967456685, 200.8635405475196762 ) ) ;
#63696 = EDGE_LOOP ( 'NONE', ( #64820, #18805, #26728, #33125 ) ) ;
#63695 = CARTESIAN_POINT ( 'NONE',  ( -7.506254784382560023E-12, 1411.829882030230010, 254.0148294673659848 ) ) ;
#63697 = ORIENTED_EDGE ( 'NONE', *, *, #38800, .F. ) ;
#63698 = CARTESIAN_POINT ( 'NONE',  ( -11.48363738179999949, 1505.551007100490096, 207.2975035741290242 ) ) ;
#63699 = VECTOR ( 'NONE', #60238, 1000.000000000000000 ) ;
#63700 = CARTESIAN_POINT ( 'NONE',  ( -22.17858213466869799, 1484.390483148310068, 216.9702515509989951 ) ) ;
#63701 = CARTESIAN_POINT ( 'NONE',  ( -8.283412045740000451, 1473.335056111630138, 270.2796699741979864 ) ) ;
#63702 = DIRECTION ( 'NONE',  ( -1.744230429721540409E-14, -1.000000000000000000, -3.290755053036525162E-15 ) ) ;
#63703 = CARTESIAN_POINT ( 'NONE',  ( -126.2838827870999836, 1371.894749952190750, 300.9320505736152427 ) ) ;
#63704 = CARTESIAN_POINT ( 'NONE',  ( 38.16624314905799764, 1450.366968005889930, 135.2278820825040100 ) ) ;
#63705 = CARTESIAN_POINT ( 'NONE',  ( 0.3657425961662950087, 1450.911939891260090, 181.4846316853029862 ) ) ;
#63706 = CARTESIAN_POINT ( 'NONE',  ( -11.36250926159999963, 1420.040572322430080, 229.9329963247979833 ) ) ;
#63707 = CARTESIAN_POINT ( 'NONE',  ( -30.24842679174809490, 1524.082582765195411, 222.4736128011820142 ) ) ;
#63708 = EDGE_CURVE ( 'NONE', #43545, #102542, #77779, .T. ) ;
#63709 = CARTESIAN_POINT ( 'NONE',  ( -1.465793917108519917, 1484.360957496709943, 182.4810413606819850 ) ) ;
#63710 = CARTESIAN_POINT ( 'NONE',  ( 8.796059898609998484, 1362.759824263850078, 207.6218459616989946 ) ) ;
#63711 = CARTESIAN_POINT ( 'NONE',  ( -46.00814008725180315, 1437.084982451890028, 267.5989046568349750 ) ) ;
#63712 = EDGE_LOOP ( 'NONE', ( #38578, #3698, #22287, #69109 ) ) ;
#63713 = CARTESIAN_POINT ( 'NONE',  ( -3.535156810759120027, 1493.450694636509979, 181.5593925653629981 ) ) ;
#63714 = ORIENTED_EDGE ( 'NONE', *, *, #86549, .F. ) ;
#63715 = VERTEX_POINT ( 'NONE', #9995 ) ;
#63716 = CARTESIAN_POINT ( 'NONE',  ( -6.548200625775000283, 1516.632821972880038, 210.2524534341069966 ) ) ;
#63717 = DIRECTION ( 'NONE',  ( -0.03489949670247723124, 0.9993908270190966503, 2.775557561563011889E-14 ) ) ;
#63718 = FACE_OUTER_BOUND ( 'NONE', #79694, .T. ) ;
#63719 = CARTESIAN_POINT ( 'NONE',  ( -13.69820349629999967, 1410.401525690029985, 190.0660059053979865 ) ) ;
#63720 = CARTESIAN_POINT ( 'NONE',  ( -16.42379639758739884, 1461.170146474039939, 228.2802429533950033 ) ) ;
#63721 = ORIENTED_EDGE ( 'NONE', *, *, #75552, .F. ) ;
#63722 = CARTESIAN_POINT ( 'NONE',  ( -5.779603138255000161, 1516.738222552470233, 201.4074744291170020 ) ) ;
#63723 = EDGE_CURVE ( 'NONE', #33631, #22102, #65534, .T. ) ;
#63724 = DIRECTION ( 'NONE',  ( 1.000000000000000000, 0.000000000000000000, 0.000000000000000000 ) ) ;
#63725 = CARTESIAN_POINT ( 'NONE',  ( -26.13451554100480223, 1384.547168729040095, 203.7448848093029881 ) ) ;
#63726 = EDGE_LOOP ( 'NONE', ( #71365, #11397, #29482, #8884 ) ) ;
#63727 = CARTESIAN_POINT ( 'NONE',  ( -8.310284128760839550, 1410.978277515770060, 269.3433025615229894 ) ) ;
#63728 = CARTESIAN_POINT ( 'NONE',  ( 1.077847364669999991E-15, 1428.043997280830126, 101.8807690336980016 ) ) ;
#63729 = CARTESIAN_POINT ( 'NONE',  ( 9.281345480445999385, 1435.168664884130294, 207.8114304728740080 ) ) ;
#63731 = ORIENTED_EDGE ( 'NONE', *, *, #88704, .F. ) ;
#63730 = CARTESIAN_POINT ( 'NONE',  ( -8.799096642483785757, 1365.569276427433351, 207.6218459616988241 ) ) ;
#63732 = EDGE_LOOP ( 'NONE', ( #105009, #58380, #92152, #99029 ) ) ;
#63733 = CARTESIAN_POINT ( 'NONE',  ( 44.22871283554869848, 1449.420066736412309, 269.0143090413143909 ) ) ;
#63734 = CARTESIAN_POINT ( 'NONE',  ( 11.18756042069709977, 1471.604168298739978, 211.4504785696180136 ) ) ;
#63735 = CARTESIAN_POINT ( 'NONE',  ( -13.52034949347279991, 1436.166343023079889, 150.4953566056409784 ) ) ;
#63736 = CARTESIAN_POINT ( 'NONE',  ( -19.37374569213963582, 1524.382868172863937, 183.8768763279542213 ) ) ;
#63737 = CARTESIAN_POINT ( 'NONE',  ( -17.74486107192629802, 1415.124054205860148, 207.5653927723479910 ) ) ;
#63738 = CARTESIAN_POINT ( 'NONE',  ( -451.6393500377540136, 1435.141463851319713, 155.5900692994430017 ) ) ;
#63739 = CARTESIAN_POINT ( 'NONE',  ( -13.79270780340000080, 1423.505142977830019, 222.1150309489979691 ) ) ;
#63740 = CARTESIAN_POINT ( 'NONE',  ( 11.27186231780000014, 1414.983773854429955, 222.4323527839979988 ) ) ;
#63741 = CARTESIAN_POINT ( 'NONE',  ( 7.356463438449999614, 1445.970468545179983, 184.4044459342979962 ) ) ;
#63742 = CARTESIAN_POINT ( 'NONE',  ( -3.268859434184999913, 1516.922519270759949, 206.6438591998669949 ) ) ;
#63743 = EDGE_LOOP ( 'NONE', ( #72064, #89154, #32381, #61783 ) ) ;
#63744 = CARTESIAN_POINT ( 'NONE',  ( -7.703846517336140565, 1425.539117803745512, 205.4402351432403862 ) ) ;
#63745 = CARTESIAN_POINT ( 'NONE',  ( -23.65802091397744178, 1447.576292128232353, 214.9099903041857544 ) ) ;
#63746 = VERTEX_POINT ( 'NONE', #4369 ) ;
#63747 = DIRECTION ( 'NONE',  ( 0.0003696129200224610584, 0.001489947240871160403, -0.9999988217210601382 ) ) ;
#63748 = CARTESIAN_POINT ( 'NONE',  ( 11.60004869885203682, 1425.894332500278097, 137.5113157688821275 ) ) ;
#63749 = CARTESIAN_POINT ( 'NONE',  ( -3.913149750709999708, 1414.000033450179899, 206.8545747367489867 ) ) ;
#63750 = CARTESIAN_POINT ( 'NONE',  ( 19.38627076359999890, 1409.590043883829821, 198.4190663087979942 ) ) ;
#63751 = CARTESIAN_POINT ( 'NONE',  ( 20.12133088869999753, 1445.052233488290085, 161.1306464489979930 ) ) ;
#63752 = CARTESIAN_POINT ( 'NONE',  ( -23.69915799640000031, 1435.325095724740095, 137.0907082570979867 ) ) ;
#63753 = CARTESIAN_POINT ( 'NONE',  ( -23.55087667009999919, 1411.110693366829764, 210.4794020521279947 ) ) ;
#63754 = CARTESIAN_POINT ( 'NONE',  ( -110.7672523143288998, 1377.913060387289988, 305.6601225730716465 ) ) ;
#63755 = ADVANCED_FACE ( 'NONE', ( #106800 ), #99491, .F. ) ;
#63756 = CARTESIAN_POINT ( 'NONE',  ( -6.719124544191419801, 1522.051704408389924, 184.2328727701749926 ) ) ;
#63757 = EDGE_CURVE ( 'NONE', #69033, #53641, #21677, .T. ) ;
#63758 = CARTESIAN_POINT ( 'NONE',  ( -4.613762395014999740, 1516.939574742129935, 214.9064842900469898 ) ) ;
#63759 = ORIENTED_EDGE ( 'NONE', *, *, #37278, .T. ) ;
#63760 = CARTESIAN_POINT ( 'NONE',  ( 7.709189683329709553, 1516.540336843770092, 207.3380993366749863 ) ) ;
#63761 = CARTESIAN_POINT ( 'NONE',  ( -6.501109238009999736, 1473.833204323429982, 270.1283629013980203 ) ) ;
#63762 = CARTESIAN_POINT ( 'NONE',  ( -0.2331143941452460122, 1408.921200921389982, 231.7611568498559791 ) ) ;
#63763 = TOROIDAL_SURFACE ( 'NONE', #90508, 14.91144628110000170, 0.5000000000000000000 ) ;
#63764 = DIRECTION ( 'NONE',  ( 9.341989762165448955E-47, -1.000000000000000000, 1.836970198721029688E-16 ) ) ;
#63765 = CARTESIAN_POINT ( 'NONE',  ( -39.76489443428390302, 1446.373445015949983, 136.7410265875109872 ) ) ;
#63766 = LINE ( 'NONE', #47504, #99620 ) ;
#63767 = CARTESIAN_POINT ( 'NONE',  ( 2.051044940784851889, 1417.316251708583195, 233.1624096844531095 ) ) ;
#63768 = CARTESIAN_POINT ( 'NONE',  ( -2.900311661485640347, 1477.802570806589756, 183.6038988494130137 ) ) ;
#63769 = CARTESIAN_POINT ( 'NONE',  ( -12.31060128686659993, 1378.376182493429951, 209.7919535259509871 ) ) ;
#63770 = CARTESIAN_POINT ( 'NONE',  ( -1.511827936991389842, 1475.041441224169830, 269.6439064326379480 ) ) ;
#63771 = CARTESIAN_POINT ( 'NONE',  ( 31.38711126342669999, 1440.913060383769789, 242.4731588227919872 ) ) ;
#63772 = CARTESIAN_POINT ( 'NONE',  ( -20.22596394560000022, 1508.016461165629835, 228.8175828582979818 ) ) ;
#63773 = CIRCLE ( 'NONE', #38727, 7.975189853890007896 ) ;
#63774 = CARTESIAN_POINT ( 'NONE',  ( -30.90487439922565116, 1525.907212628473644, 201.8101144455181952 ) ) ;
#63775 = ORIENTED_EDGE ( 'NONE', *, *, #3777, .F. ) ;
#63776 = CARTESIAN_POINT ( 'NONE',  ( -3.350338079455601026, 1523.604703353109699, 176.1628856388066708 ) ) ;
#63777 = CARTESIAN_POINT ( 'NONE',  ( -19.42349535385465131, 1485.589659117401425, 189.9324232024657135 ) ) ;
#63778 = CARTESIAN_POINT ( 'NONE',  ( -7.260306344532728495, 1509.032998971549432, 202.6015535907291110 ) ) ;
#63779 = CARTESIAN_POINT ( 'NONE',  ( 2.897247639040000156, 1482.822904283830212, 234.8636011151980085 ) ) ;
#63780 = EDGE_CURVE ( 'NONE', #32555, #31391, #4267, .T. ) ;
#63781 = CARTESIAN_POINT ( 'NONE',  ( -17.66471548549609949, 1420.877322952379927, 226.1084292698919853 ) ) ;
#63782 = CARTESIAN_POINT ( 'NONE',  ( -15.36908788890000110, 1507.577581067430174, 231.3915608676979900 ) ) ;
#63783 = CARTESIAN_POINT ( 'NONE',  ( -30.38379501695840190, 1383.841595863670136, 228.2076059929920007 ) ) ;
#63784 = ADVANCED_FACE ( 'NONE', ( #91110 ), #23347, .T. ) ;
#63785 =( BOUNDED_SURFACE ( )  B_SPLINE_SURFACE ( 3, 2, ( 
 ( #80910, #72517, #106645 ),
 ( #55729, #54087, #55178 ),
 ( #79820, #105007, #70337 ),
 ( #104449, #29385, #11506 ),
 ( #71452, #12600, #46778 ),
 ( #64127, #98248, #21518 ),
 ( #13121, #97155, #54630 ),
 ( #88763, #12046, #46229 ),
 ( #80362, #84604, #65223 ),
 ( #107757, #67835, #7896 ),
 ( #17375, #39454, #79 ),
 ( #59437, #90386, #59987 ),
 ( #31040, #5296, #81988 ),
 ( #30493, #85707, #40000 ) ),
 .UNSPECIFIED., .F., .F., .F. ) 
 B_SPLINE_SURFACE_WITH_KNOTS ( ( 4, 2, 2, 2, 2, 2, 4 ),
 ( 3, 3 ),
 ( 2.412349833780247366E-16, 0.0009443072508238468509, 0.001416460876235649605, 0.001888614501647452575, 0.002360768127059255546, 0.002832921752471058083, 0.003777229003294664024 ),
 ( 0.000000000000000000, 1.000000000000000000 ),
 .UNSPECIFIED. ) 
 GEOMETRIC_REPRESENTATION_ITEM ( )  RATIONAL_B_SPLINE_SURFACE ( (
 ( 1.000000000000000000, 0.9376006582765971098, 1.000000000000000000),
 ( 1.000000000000000000, 0.9283977714666437064, 1.000000000000000000),
 ( 1.000000000000000000, 0.9189750060573711465, 1.000000000000000000),
 ( 1.000000000000000000, 0.9042792056080602991, 1.000000000000000000),
 ( 1.000000000000000000, 0.8992469033884697982, 1.000000000000000000),
 ( 1.000000000000000000, 0.8891280264640721853, 1.000000000000000000),
 ( 1.000000000000000000, 0.8840337471674194481, 1.000000000000000000),
 ( 1.000000000000000000, 0.8736395124164607617, 1.000000000000000000),
 ( 1.000000000000000000, 0.8683406746558937073, 1.000000000000000000),
 ( 1.000000000000000000, 0.8573361860701524950, 1.000000000000000000),
 ( 1.000000000000000000, 0.8516508399495845705, 1.000000000000000000),
 ( 1.000000000000000000, 0.8340914917066767353, 1.000000000000000000),
 ( 1.000000000000000000, 0.8215597275861534765, 1.000000000000000000),
 ( 1.000000000000000000, 0.8070209408750069757, 1.000000000000000000) ) ) 
 REPRESENTATION_ITEM ( '' )  SURFACE ( )  );
#63786 = CARTESIAN_POINT ( 'NONE',  ( -21.44637798829759845, 1506.412603150730092, 216.0243673054189912 ) ) ;
#63787 = CARTESIAN_POINT ( 'NONE',  ( 9.547743298340000351, 1407.913147213329921, 218.7935598638979968 ) ) ;
#63788 = CARTESIAN_POINT ( 'NONE',  ( -11.89193436319930086, 1434.276600524120113, 147.6498533934650084 ) ) ;
#63789 = CARTESIAN_POINT ( 'NONE',  ( 1.720386059670000023, 1465.121410839730061, 235.5820274437980117 ) ) ;
#63790 = ADVANCED_FACE ( 'NONE', ( #107908 ), #82265, .T. ) ;
#63792 = VERTEX_POINT ( 'NONE', #78599 ) ;
#63791 = CARTESIAN_POINT ( 'NONE',  ( -5.519906363166400709, 1440.499855196290127, 154.7645174855159951 ) ) ;
#63793 = CARTESIAN_POINT ( 'NONE',  ( -0.5431364122140001083, 1451.469100220230075, 182.8070713969979977 ) ) ;
#63794 = CARTESIAN_POINT ( 'NONE',  ( -9.770253401179999742, 1381.414343185820144, 201.2605876295190228 ) ) ;
#63795 = CARTESIAN_POINT ( 'NONE',  ( 3.856607047088039586, 1508.551704408389924, 204.5415913389130083 ) ) ;
#63797 = EDGE_LOOP ( 'NONE', ( #70368, #101623, #70479, #102254 ) ) ;
#63796 = CARTESIAN_POINT ( 'NONE',  ( -17.36791971707869919, 1414.972329067380088, 207.8825838234459980 ) ) ;
#63798 = CARTESIAN_POINT ( 'NONE',  ( -9.838242193716929762, 1462.268756451870104, 227.9668037484569822 ) ) ;
#63799 = ORIENTED_EDGE ( 'NONE', *, *, #78695, .F. ) ;
#63800 = EDGE_CURVE ( 'NONE', #43874, #95045, #75795, .T. ) ;
#63801 = CARTESIAN_POINT ( 'NONE',  ( -10.62909775710000027, 1390.234991692080030, 215.5537828994590086 ) ) ;
#63802 = CARTESIAN_POINT ( 'NONE',  ( -10.25401551478790196, 1391.808998814714187, 215.0731684536954731 ) ) ;
#63803 = CARTESIAN_POINT ( 'NONE',  ( 4.329791490734999471, 1515.051704408389924, 209.1218459511669892 ) ) ;
#63805 = ADVANCED_FACE ( 'NONE', ( #86437 ), #98329, .F. ) ;
#63804 = CARTESIAN_POINT ( 'NONE',  ( -2.031883580139580037, 1464.998375551469962, 198.3053770173009980 ) ) ;
#63806 = CARTESIAN_POINT ( 'NONE',  ( 4.086314366965700273, 1515.499673594937576, 211.4519800836456795 ) ) ;
#63807 = DIRECTION ( 'NONE',  ( 0.3363363969979655810, -0.9417419115949056119, 0.000000000000000000 ) ) ;
#63808 = CARTESIAN_POINT ( 'NONE',  ( 14.43128343706390027, 1409.417011909710027, 205.2710633763729788 ) ) ;
#63809 = CARTESIAN_POINT ( 'NONE',  ( -7.966081143649218710, 1384.918389534460175, 199.4892681243580057 ) ) ;
#63810 = CARTESIAN_POINT ( 'NONE',  ( -94.44233799117999695, 1385.205980051620145, 294.7441417489620221 ) ) ;
#63811 = CARTESIAN_POINT ( 'NONE',  ( -113.4000000000000057, 1390.939237335599955, 304.2218459572590064 ) ) ;
#63812 = DIRECTION ( 'NONE',  ( 0.8771707529291777883, 0.03063147767459039120, -0.4792005663405778937 ) ) ;
#63813 = EDGE_CURVE ( 'NONE', #60488, #19532, #34772, .T. ) ;
#63814 = CIRCLE ( 'NONE', #71025, 2.000000000000001776 ) ;
#63815 = CARTESIAN_POINT ( 'NONE',  ( -120.0391016774570403, 1390.913060387289988, 305.8779575274093077 ) ) ;
#63816 = ORIENTED_EDGE ( 'NONE', *, *, #41240, .F. ) ;
#63817 = ORIENTED_EDGE ( 'NONE', *, *, #99437, .F. ) ;
#63819 = EDGE_CURVE ( 'NONE', #82691, #96612, #106244, .T. ) ;
#63818 = CARTESIAN_POINT ( 'NONE',  ( 18.15646965371266575, 1522.906363951597314, 238.1669781545271860 ) ) ;
#63820 = CARTESIAN_POINT ( 'NONE',  ( -12.26778636215339979, 1416.765224586759814, 194.6662842786359988 ) ) ;
#63821 =( BOUNDED_CURVE ( )  B_SPLINE_CURVE ( 3, ( #65669, #38789, #89752, #57285 ),
 .UNSPECIFIED., .F., .F. ) 
 B_SPLINE_CURVE_WITH_KNOTS ( ( 4, 4 ),
 ( 4.233974059277724855, 5.191467434861920083 ),
 .UNSPECIFIED. ) 
 CURVE ( )  GEOMETRIC_REPRESENTATION_ITEM ( )  RATIONAL_B_SPLINE_CURVE ( ( 1.000000000000000000, 0.9250486529759208709, 0.9250486529759208709, 1.000000000000000000 ) ) 
 REPRESENTATION_ITEM ( '' )  );
#63822 = CARTESIAN_POINT ( 'NONE',  ( -0.1106396160836400078, 1496.533495305330007, 196.7588328172749925 ) ) ;
#63823 = CARTESIAN_POINT ( 'NONE',  ( 1.685908120830160076E-11, 1466.195288505810140, 242.1879250690809897 ) ) ;
#63824 = CARTESIAN_POINT ( 'NONE',  ( -20.37857258470070221, 1500.692629429460112, 190.5974988396959873 ) ) ;
#63825 = CARTESIAN_POINT ( 'NONE',  ( 6.232532001850000114, 1398.098440471829917, 220.5304192662980256 ) ) ;
#63826 = CARTESIAN_POINT ( 'NONE',  ( 32.06248218118899018, 1524.739915903631754, 202.1338403451020440 ) ) ;
#63827 = ADVANCED_FACE ( 'NONE', ( #87562 ), #89388, .T. ) ;
#63828 = CARTESIAN_POINT ( 'NONE',  ( 13.58268853708210067, 1416.851343896850040, 196.3340833727469885 ) ) ;
#63829 = CARTESIAN_POINT ( 'NONE',  ( -11.83205321494600781, 1365.644012745619875, 208.3718459617010978 ) ) ;
#63830 = CARTESIAN_POINT ( 'NONE',  ( -22.28696231330000188, 1506.798305107829947, 208.8466800722590051 ) ) ;
#63831 = CARTESIAN_POINT ( 'NONE',  ( -22.62861454470000311, 1507.212883763329955, 208.5231287359179930 ) ) ;
#63832 = EDGE_CURVE ( 'NONE', #104688, #50508, #56148, .T. ) ;
#63833 = CARTESIAN_POINT ( 'NONE',  ( 4.997718238375000510, 1516.693851263360102, 207.9888968556769839 ) ) ;
#63834 = CARTESIAN_POINT ( 'NONE',  ( 11.39017366564850242, 1433.914938483480000, 151.4359183571540086 ) ) ;
#63835 = CARTESIAN_POINT ( 'NONE',  ( -13.83305622877970009, 1436.229965305390124, 150.3316969671570007 ) ) ;
#63836 = CARTESIAN_POINT ( 'NONE',  ( -7.544890296849999345, 1384.926148866459926, 219.0875903968589853 ) ) ;
#63837 = CARTESIAN_POINT ( 'NONE',  ( 18.59403002570000041, 1409.562378223829910, 197.6450396516979993 ) ) ;
#63838 = DIRECTION ( 'NONE',  ( -5.980589973904019347E-17, 1.000000000000000000, -1.736889445713099699E-16 ) ) ;
#63839 = CARTESIAN_POINT ( 'NONE',  ( -11.20337388083980201, 1490.156468557539938, 191.3256793942369995 ) ) ;
#63840 = EDGE_CURVE ( 'NONE', #94274, #12190, #39344, .T. ) ;
#63841 = ORIENTED_EDGE ( 'NONE', *, *, #54807, .T. ) ;
#63842 = CARTESIAN_POINT ( 'NONE',  ( 10.82132307049999831, 1413.960774641330090, 250.5360043972979440 ) ) ;
#63843 = CARTESIAN_POINT ( 'NONE',  ( -26.14369035850000245, 1488.683671329329854, 203.4812363805280029 ) ) ;
#63845 = CARTESIAN_POINT ( 'NONE',  ( -17.67654380129999936, 1410.026337406529819, 195.1650949151980114 ) ) ;
#63844 = CARTESIAN_POINT ( 'NONE',  ( -1.542474001980000065, 1502.014794158629911, 181.0193620746979946 ) ) ;
#63846 = CYLINDRICAL_SURFACE ( 'NONE', #49809, 0.4999999999999909517 ) ;
#63847 = CARTESIAN_POINT ( 'NONE',  ( 5.465011822930000053E-09, 1419.727281558630011, 225.2064029046980238 ) ) ;
#63848 = CARTESIAN_POINT ( 'NONE',  ( 0.1259222685549989951, 1487.739371776789994, 219.9965893379989836 ) ) ;
#63849 = PLANE ( 'NONE',  #73165 ) ;
#63850 = CARTESIAN_POINT ( 'NONE',  ( 33.91369266730000476, 1450.440660192670066, 136.2454535554979884 ) ) ;
#63851 = VERTEX_POINT ( 'NONE', #100350 ) ;
#63852 = CARTESIAN_POINT ( 'NONE',  ( 7.620902379277350036, 1398.139480053939906, 197.4921199094770259 ) ) ;
#63853 = CARTESIAN_POINT ( 'NONE',  ( 11.11245944731352964, 1512.836811624652455, 225.1840528857647996 ) ) ;
#63854 = ORIENTED_EDGE ( 'NONE', *, *, #40285, .T. ) ;
#63855 = ORIENTED_EDGE ( 'NONE', *, *, #16691, .T. ) ;
#63856 = CARTESIAN_POINT ( 'NONE',  ( 2.897985082046180327, 1480.124455445799867, 234.7435789289370121 ) ) ;
#63857 = CARTESIAN_POINT ( 'NONE',  ( -22.70984874270769893, 1409.706099204690190, 208.9686739919200136 ) ) ;
#63858 = VERTEX_POINT ( 'NONE', #99226 ) ;
#63859 = CARTESIAN_POINT ( 'NONE',  ( 0.08478249716650000656, 1419.321047202629870, 227.3343309334979949 ) ) ;
#63860 = AXIS2_PLACEMENT_3D ( 'NONE', #49957, #58361, #77366 ) ;
#63861 = CARTESIAN_POINT ( 'NONE',  ( 7.703785732380000084, 1490.746146274789908, 209.8379679705590206 ) ) ;
#63862 = CARTESIAN_POINT ( 'NONE',  ( -3.371383657610000029, 1479.771743941129898, 235.5096298670979991 ) ) ;
#63863 = EDGE_CURVE ( 'NONE', #1004, #109826, #66861, .T. ) ;
#63864 = CARTESIAN_POINT ( 'NONE',  ( 9.146299198640271300, 1461.861878385089767, 205.8341600298289791 ) ) ;
#63865 = VERTEX_POINT ( 'NONE', #107653 ) ;
#63866 = CARTESIAN_POINT ( 'NONE',  ( 46.05252857291980462, 1440.912967510329963, 266.6768989187639818 ) ) ;
#63867 = CARTESIAN_POINT ( 'NONE',  ( -113.3174119514818301, 1391.913060387289988, 300.7228204909004603 ) ) ;
#63868 = EDGE_CURVE ( 'NONE', #98871, #65751, #6292, .T. ) ;
#63869 = CARTESIAN_POINT ( 'NONE',  ( 0.4435022942679999747, 1418.672171181530075, 184.7048927422980000 ) ) ;
#63870 = CARTESIAN_POINT ( 'NONE',  ( -4.620008245204999753, 1516.777260590120022, 203.3472363101570011 ) ) ;
#63871 = ORIENTED_EDGE ( 'NONE', *, *, #29636, .F. ) ;
#63872 = CARTESIAN_POINT ( 'NONE',  ( 7.816109785343320127, 1482.901617154930136, 217.9966951879339945 ) ) ;
#63873 = CARTESIAN_POINT ( 'NONE',  ( 13.08298364061185559, 1443.010872789425321, 187.3424311853700317 ) ) ;
#63874 = EDGE_LOOP ( 'NONE', ( #87936, #78618, #47530, #68919 ) ) ;
#63875 = VERTEX_POINT ( 'NONE', #91945 ) ;
#63876 = CARTESIAN_POINT ( 'NONE',  ( 2.534335827540430852, 1523.982201850120191, 175.6705872193752214 ) ) ;
#63877 = CARTESIAN_POINT ( 'NONE',  ( -3.186928814199029958, 1508.501190230369957, 220.3905975803280057 ) ) ;
#63878 = CARTESIAN_POINT ( 'NONE',  ( -22.30007645030000063, 1409.691796216729927, 207.3274002725380285 ) ) ;
#63879 = CIRCLE ( 'NONE', #40596, 2.000000000000004441 ) ;
#63880 = CARTESIAN_POINT ( 'NONE',  ( -9.262945410020661186, 1470.779016715980106, 213.5645637807399737 ) ) ;
#63881 = CARTESIAN_POINT ( 'NONE',  ( 21.69567490921269837, 1452.155430724869802, 140.9671523504339916 ) ) ;
#63882 = CARTESIAN_POINT ( 'NONE',  ( 9.549927530160001510, 1420.582634806009992, 197.0246874367990131 ) ) ;
#63883 = CARTESIAN_POINT ( 'NONE',  ( -0.2259745478316219913, 1475.391039426699990, 220.5480955931240032 ) ) ;
#63884 = CARTESIAN_POINT ( 'NONE',  ( -6.883305316117739991, 1494.320249002219953, 198.9132838350930115 ) ) ;
#63885 = CARTESIAN_POINT ( 'NONE',  ( -9.724834716106559089E-16, 1374.031200045389824, 209.1218459616989946 ) ) ;
#63886 = CARTESIAN_POINT ( 'NONE',  ( 0.03589260184548991733, 1409.889651789088475, 233.1454190195690330 ) ) ;
#63888 = CARTESIAN_POINT ( 'NONE',  ( -106.4421323744290078, 1391.913060418769874, 306.1278572653080232 ) ) ;
#63887 = CARTESIAN_POINT ( 'NONE',  ( -18.79435929301390118, 1476.960500850449762, 189.8610087135640185 ) ) ;
#63889 = CARTESIAN_POINT ( 'NONE',  ( 11.48916758364780044, 1422.248195443439954, 207.1589471795049917 ) ) ;
#63890 = EDGE_CURVE ( 'NONE', #87917, #80584, #54826, .T. ) ;
#63891 = CARTESIAN_POINT ( 'NONE',  ( -25.01122921334119908, 1509.595256063680154, 222.7800201234539941 ) ) ;
#63892 = CARTESIAN_POINT ( 'NONE',  ( -6.580362948704999937, 1511.382498894319951, 201.8051239266270045 ) ) ;
#63893 = VERTEX_POINT ( 'NONE', #65115 ) ;
#63894 = CARTESIAN_POINT ( 'NONE',  ( 26.42894384599999924, 1421.320559242730042, 262.6648722463980334 ) ) ;
#63895 = CARTESIAN_POINT ( 'NONE',  ( 12.95221149940000060, 1434.756340029210151, 149.1862543735979898 ) ) ;
#63896 = AXIS2_PLACEMENT_3D ( 'NONE', #44112, #102334, #59811 ) ;
#63897 = CARTESIAN_POINT ( 'NONE',  ( -89.21014235648939916, 1384.971367781859726, 308.4434907503709837 ) ) ;
#63898 = CARTESIAN_POINT ( 'NONE',  ( 4.706367361569999908, 1507.026273860589981, 219.8285751887989932 ) ) ;
#63899 = DIRECTION ( 'NONE',  ( -5.980589973904019347E-17, 1.000000000000000000, -1.736889445713099699E-16 ) ) ;
#63901 = VERTEX_POINT ( 'NONE', #83536 ) ;
#63900 = CARTESIAN_POINT ( 'NONE',  ( -16.44718840435429996, 1420.035791990140069, 209.2215304830220077 ) ) ;
#63902 = CARTESIAN_POINT ( 'NONE',  ( -17.01997119704033423, 1417.322295037478625, 207.6226155442043648 ) ) ;
#63903 = CARTESIAN_POINT ( 'NONE',  ( -7.544898852049939819, 1384.902875181250010, 219.0876726591300212 ) ) ;
#63904 = ADVANCED_FACE ( 'NONE', ( #14685 ), #101070, .T. ) ;
#63905 = CARTESIAN_POINT ( 'NONE',  ( -13.58235848260000012, 1416.828044885930012, 221.9087532849979709 ) ) ;
#63906 = CARTESIAN_POINT ( 'NONE',  ( -0.7759192619701910099, 1430.041485328890076, 199.7504914271860059 ) ) ;
#63907 = CARTESIAN_POINT ( 'NONE',  ( 12.93225138353500192, 1513.362623229679912, 226.0086287796669922 ) ) ;
#63908 = CARTESIAN_POINT ( 'NONE',  ( 5.365940947776590697, 1422.323282697306922, 140.6189186885637525 ) ) ;
#63909 = EDGE_CURVE ( 'NONE', #39082, #25053, #97434, .T. ) ;
#63910 = CARTESIAN_POINT ( 'NONE',  ( 1.269517173649849839, 1457.689354814089938, 199.6687979431409872 ) ) ;
#63911 = DIRECTION ( 'NONE',  ( 0.9455185755993178454, 0.000000000000000000, -0.3255681544571537578 ) ) ;
#63912 = CARTESIAN_POINT ( 'NONE',  ( 15.73276775970000330, 1419.767728771030079, 227.5061845221979979 ) ) ;
#63913 = CARTESIAN_POINT ( 'NONE',  ( -22.03465957474530157, 1522.382868172863937, 235.4136513321633117 ) ) ;
#63914 = B_SPLINE_CURVE_WITH_KNOTS ( 'NONE', 3,
 ( #34047, #14476, #109121, #82794, #32400, #66583, #100686, #23970, #6089, #92294 ),
 .UNSPECIFIED., .F., .F.,
 ( 4, 2, 2, 2, 4 ),
 ( 0.000000000000000000, 0.0007189769279725863283, 0.001437953855945172657, 0.002156930783917758877, 0.002875907711890345313 ),
 .UNSPECIFIED. ) ;
#63915 = CARTESIAN_POINT ( 'NONE',  ( 1.700259675955000160, 1516.898441858519845, 207.4036424686470070 ) ) ;
#63916 = CARTESIAN_POINT ( 'NONE',  ( 45.83772369860000140, 1436.897828481359966, 268.5019638271979829 ) ) ;
#63917 = CARTESIAN_POINT ( 'NONE',  ( -17.65294392160000214, 1409.529514773629899, 223.4064738432979880 ) ) ;
#63918 = CARTESIAN_POINT ( 'NONE',  ( 15.86562505229999864, 1435.238789513250140, 148.1955696700979956 ) ) ;
#63919 = CARTESIAN_POINT ( 'NONE',  ( -0.7156054891749999980, 1424.187899035330020, 228.2423996515980207 ) ) ;
#63920 = CARTESIAN_POINT ( 'NONE',  ( 5.385044978479859523, 1432.007840264780043, 154.5986929186840086 ) ) ;
#63921 = CARTESIAN_POINT ( 'NONE',  ( -12.67256029850000054, 1474.517343106330145, 266.8981073570980129 ) ) ;
#63922 = CARTESIAN_POINT ( 'NONE',  ( -14.23398643054899892, 1416.596405885110016, 203.1904536488209772 ) ) ;
#63923 = EDGE_CURVE ( 'NONE', #66318, #3293, #94141, .T. ) ;
#63924 = CARTESIAN_POINT ( 'NONE',  ( -38.69039280719189833, 1437.284833695140151, 135.5234525068720188 ) ) ;
#63925 = CARTESIAN_POINT ( 'NONE',  ( 0.2160969567860719920, 1453.936780232339970, 183.2132073708449980 ) ) ;
#63926 = CARTESIAN_POINT ( 'NONE',  ( -13.88567141579999920, 1409.397958718129985, 203.2213914723980110 ) ) ;
#63927 = CARTESIAN_POINT ( 'NONE',  ( -11.49747567979999907, 1414.913060387329779, 197.9009878688979995 ) ) ;
#63928 = B_SPLINE_CURVE_WITH_KNOTS ( 'NONE', 5,
 ( #73681, #106695, #91563, #107808, #31095, #5348 ),
 .UNSPECIFIED., .F., .F.,
 ( 6, 6 ),
 ( 203.1089678689999971, 212.7664182919999973 ),
 .UNSPECIFIED. ) ;
#63929 = CARTESIAN_POINT ( 'NONE',  ( -4.091836660730000297, 1515.531866980889845, 208.0024180612289797 ) ) ;
#63930 = EDGE_CURVE ( 'NONE', #106529, #85718, #86853, .T. ) ;
#63931 = CARTESIAN_POINT ( 'NONE',  ( -28.35296704552279934, 1509.521797104740017, 211.0041094760910028 ) ) ;
#63932 = CARTESIAN_POINT ( 'NONE',  ( 13.80512448200000009, 1434.979588684790087, 149.6997163784980103 ) ) ;
#63933 = CARTESIAN_POINT ( 'NONE',  ( -38.36650730484889493, 1437.217469519499900, 134.0999999970779868 ) ) ;
#63934 = DIRECTION ( 'NONE',  ( -6.123233995736769734E-17, -1.000000000000000000, 0.000000000000000000 ) ) ;
#63935 = ORIENTED_EDGE ( 'NONE', *, *, #93928, .T. ) ;
#63936 = CARTESIAN_POINT ( 'NONE',  ( -0.9985884068039365680, 1368.656381781917617, 207.8228078564805230 ) ) ;
#63937 = CARTESIAN_POINT ( 'NONE',  ( -8.740751882428300590, 1409.218294169019828, 221.2666971587190119 ) ) ;
#63938 = CARTESIAN_POINT ( 'NONE',  ( -12.25495820260000102, 1490.496248278489702, 208.7368242965009983 ) ) ;
#63939 = B_SPLINE_CURVE_WITH_KNOTS ( 'NONE', 5,
 ( #18878, #45234, #37366, #44677, #35700, #62040, #69890, #53077, #97258 ),
 .UNSPECIFIED., .F., .F.,
 ( 6, 3, 6 ),
 ( 0.000000000000000000, 3.343413285960000092, 6.686826571920000184 ),
 .UNSPECIFIED. ) ;
#63941 = EDGE_CURVE ( 'NONE', #8029, #80761, #76216, .T. ) ;
#63940 = CARTESIAN_POINT ( 'NONE',  ( 3.235048515759559873, 1466.472015849239824, 219.6884157167970102 ) ) ;
#63942 = CARTESIAN_POINT ( 'NONE',  ( 21.05711716160336522, 1526.748660780343471, 233.6123052680174510 ) ) ;
#63943 = AXIS2_PLACEMENT_3D ( 'NONE', #64200, #82067, #71526 ) ;
#63944 = CARTESIAN_POINT ( 'NONE',  ( -37.78661183750000419, 1461.804245060129915, 266.9502806207980257 ) ) ;
#63945 = CARTESIAN_POINT ( 'NONE',  ( -2.500000000000000000, 1425.929641636930000, 172.2701767054979882 ) ) ;
#63946 = DIRECTION ( 'NONE',  ( 0.000000000000000000, 1.000000000000000000, 0.000000000000000000 ) ) ;
#63947 = CARTESIAN_POINT ( 'NONE',  ( -25.16173584180000233, 1509.119668852230234, 220.4671678159979820 ) ) ;
#63948 = CARTESIAN_POINT ( 'NONE',  ( -94.97055395160710134, 1384.610110349949991, 310.0293933350179714 ) ) ;
#63949 = CARTESIAN_POINT ( 'NONE',  ( -31.13530430868299703, 1384.970948276150011, 206.1966052560059950 ) ) ;
#63950 = DIRECTION ( 'NONE',  ( 0.2958906675619759619, 0.3688552201855968549, 0.8811325322512856273 ) ) ;
#63951 = CARTESIAN_POINT ( 'NONE',  ( -9.862951376772540968, 1517.051704408389924, 228.3939896807019920 ) ) ;
#63952 = CARTESIAN_POINT ( 'NONE',  ( -27.03405935059999976, 1451.816840469730096, 135.7882905775979907 ) ) ;
#63953 = ADVANCED_FACE ( 'NONE', ( #103084 ), #84102, .T. ) ;
#63954 = CARTESIAN_POINT ( 'NONE',  ( 1.961418762358043022, 1526.143142182266047, 177.8224660300663515 ) ) ;
#63956 = VERTEX_POINT ( 'NONE', #106953 ) ;
#63955 = CARTESIAN_POINT ( 'NONE',  ( -5.144873395449999443, 1502.885538352589947, 229.8910404859989853 ) ) ;
#63957 = CARTESIAN_POINT ( 'NONE',  ( -109.3075498650000128, 1384.894860980859903, 311.2646804682590300 ) ) ;
#63958 = CARTESIAN_POINT ( 'NONE',  ( -20.92767404034536938, 1512.187213306747481, 182.8548762971666406 ) ) ;
#63959 = CARTESIAN_POINT ( 'NONE',  ( -19.02974267272306719, 1522.051704408389924, 207.1627782414018100 ) ) ;
#63960 = CARTESIAN_POINT ( 'NONE',  ( -12.18103061950000132, 1415.553739809529816, 195.2061824783980342 ) ) ;
#63961 = FACE_OUTER_BOUND ( 'NONE', #57231, .T. ) ;
#63962 = CARTESIAN_POINT ( 'NONE',  ( 22.84076229929999968, 1409.875136994729928, 212.1997148582279920 ) ) ;
#63963 = CARTESIAN_POINT ( 'NONE',  ( 7.201922804036379411, 1423.097602058059920, 196.0540625376380035 ) ) ;
#63964 = CARTESIAN_POINT ( 'NONE',  ( -19.81119127480000230, 1468.787329907190042, 204.4917199178690055 ) ) ;
#63965 = CARTESIAN_POINT ( 'NONE',  ( -3.611923541125130033, 1508.978184271700002, 180.0004877964609875 ) ) ;
#63967 = CARTESIAN_POINT ( 'NONE',  ( -10.44371214979999962, 1379.699184266919929, 202.4842574811590055 ) ) ;
#63966 = CARTESIAN_POINT ( 'NONE',  ( -11.87300260940000030, 1432.863468416260048, 150.3956790681980067 ) ) ;
#63968 = CARTESIAN_POINT ( 'NONE',  ( 24.37269502358340034, 1430.523498792699911, 207.7385376608809793 ) ) ;
#63969 = CARTESIAN_POINT ( 'NONE',  ( -103.0889951380000014, 1378.528619065190014, 304.2218459572590064 ) ) ;
#63970 = CARTESIAN_POINT ( 'NONE',  ( -234.5897387251999930, 11221.53578756869865, 2175.945776423289772 ) ) ;
#63971 = EDGE_CURVE ( 'NONE', #105306, #43307, #74854, .T. ) ;
#63972 = CARTESIAN_POINT ( 'NONE',  ( -1.424810123350000124, 1415.524860511530051, 233.1780344959979914 ) ) ;
#63973 = AXIS2_PLACEMENT_3D ( 'NONE', #41449, #17303, #108643 ) ;
#63974 = CARTESIAN_POINT ( 'NONE',  ( 8.379275254589998667, 1362.454991452510058, 210.6218459616991936 ) ) ;
#63975 = CARTESIAN_POINT ( 'NONE',  ( -1.715361130375000043, 1516.743010792419909, 205.6766444437269854 ) ) ;
#63976 = CARTESIAN_POINT ( 'NONE',  ( -4.340483865352609882, 1484.701310027739964, 183.4883394036949937 ) ) ;
#63977 = ORIENTED_EDGE ( 'NONE', *, *, #91352, .T. ) ;
#63978 = EDGE_CURVE ( 'NONE', #44160, #78578, #99993, .T. ) ;
#63979 = CARTESIAN_POINT ( 'NONE',  ( 11.36217411025890023, 1503.110300770179720, 211.0233484295470134 ) ) ;
#63980 = CARTESIAN_POINT ( 'NONE',  ( 18.88752285780000051, 1416.568813549730066, 210.6689649478780098 ) ) ;
#63983 = ORIENTED_EDGE ( 'NONE', *, *, #40518, .T. ) ;
#63982 = CARTESIAN_POINT ( 'NONE',  ( -68.18659372557320353, 1379.747119388199735, 279.6866116612499695 ) ) ;
#63981 = AXIS2_PLACEMENT_3D ( 'NONE', #51238, #8666, #42844 ) ;
#63984 = ORIENTED_EDGE ( 'NONE', *, *, #43399, .F. ) ;
#63985 = CARTESIAN_POINT ( 'NONE',  ( 28.34445795850000138, 1509.155937278929969, 210.1751191034680062 ) ) ;
#63986 = ORIENTED_EDGE ( 'NONE', *, *, #58492, .F. ) ;
#63987 = CARTESIAN_POINT ( 'NONE',  ( 0.5863727358502109910, 1485.693194848699932, 220.9873588030069982 ) ) ;
#63988 = CARTESIAN_POINT ( 'NONE',  ( 1.556370308520000023, 1414.996442553730049, 191.7142053419979959 ) ) ;
#63990 = CARTESIAN_POINT ( 'NONE',  ( 24.55110742759999809, 1443.479132512090018, 214.0305984285579939 ) ) ;
#63989 = CARTESIAN_POINT ( 'NONE',  ( 2.329729395510000245, 1427.373795049630189, 123.0297916884979941 ) ) ;
#63991 = CARTESIAN_POINT ( 'NONE',  ( 2.494757998004999866, 1516.937508036699910, 210.8228737931069929 ) ) ;
#63992 = CARTESIAN_POINT ( 'NONE',  ( -24.91466702467300109, 1452.043047651259940, 135.6639804502279958 ) ) ;
#63993 = CARTESIAN_POINT ( 'NONE',  ( -105.8258850450579871, 1378.913060387369796, 304.5940478994550062 ) ) ;
#63994 = CARTESIAN_POINT ( 'NONE',  ( 7.280053280969999818, 1410.543619424229973, 230.7511305521980205 ) ) ;
#63995 = CARTESIAN_POINT ( 'NONE',  ( 10.25705989742519897, 1481.638279496849918, 212.3655552129939963 ) ) ;
#63996 = DIRECTION ( 'NONE',  ( 0.000000000000000000, 0.000000000000000000, 1.000000000000000000 ) ) ;
#63997 = CARTESIAN_POINT ( 'NONE',  ( 41.42406817588610579, 1441.754257787119741, 134.0999999980809889 ) ) ;
#63998 = CARTESIAN_POINT ( 'NONE',  ( -7.260870878720000476, 1480.575647549590030, 208.3277293783959863 ) ) ;
#63999 = ORIENTED_EDGE ( 'NONE', *, *, #36144, .T. ) ;
#64000 = CARTESIAN_POINT ( 'NONE',  ( -9.573049153892020158, 1423.428015373189965, 192.3355766873849859 ) ) ;
#64001 = DIRECTION ( 'NONE',  ( 1.000000000000000000, 2.249639673992764790E-32, 1.224646799147350002E-16 ) ) ;
#64002 = VERTEX_POINT ( 'NONE', #24576 ) ;
#64003 = ORIENTED_EDGE ( 'NONE', *, *, #105176, .T. ) ;
#64004 = ORIENTED_EDGE ( 'NONE', *, *, #83012, .T. ) ;
#64005 = CARTESIAN_POINT ( 'NONE',  ( -6.382129857305000264, 1514.500328598809801, 216.9911249345570070 ) ) ;
#64006 = CARTESIAN_POINT ( 'NONE',  ( 16.38124166206986132, 1514.407859675132613, 194.5303642102901165 ) ) ;
#64007 = CARTESIAN_POINT ( 'NONE',  ( 7.867369012536836514, 1451.393875050238648, 152.9843002031269350 ) ) ;
#64008 = CIRCLE ( 'NONE', #106876, 1.999999954377493783 ) ;
#64009 = CARTESIAN_POINT ( 'NONE',  ( -8.862296812249999434, 1384.904551176430004, 218.6851794592490137 ) ) ;
#64010 = CARTESIAN_POINT ( 'NONE',  ( -17.49148533773131931, 1448.272215950228656, 218.1393388027306059 ) ) ;
#64011 = CARTESIAN_POINT ( 'NONE',  ( -65.90777676982870048, 1379.741637275925996, 274.1881090155197285 ) ) ;
#64012 = CARTESIAN_POINT ( 'NONE',  ( 0.06822080563540121323, 1464.084053037690182, 199.2812091259889939 ) ) ;
#64013 = CARTESIAN_POINT ( 'NONE',  ( -8.515581525576479294, 1519.551704408389924, 226.9159523030141372 ) ) ;
#64014 = CARTESIAN_POINT ( 'NONE',  ( 10.26243806819999982, 1415.425644477329797, 194.9508951275979882 ) ) ;
#64015 = CARTESIAN_POINT ( 'NONE',  ( -51.92850933155389725, 1384.628554692669923, 228.3932471100619921 ) ) ;
#64016 = ORIENTED_EDGE ( 'NONE', *, *, #43172, .T. ) ;
#64017 = CARTESIAN_POINT ( 'NONE',  ( -6.950833568235000648, 1517.156142772249950, 206.6378959915070084 ) ) ;
#64018 = ORIENTED_EDGE ( 'NONE', *, *, #56320, .T. ) ;
#64019 = CARTESIAN_POINT ( 'NONE',  ( 23.79195804607689624, 1440.913060387330006, 234.8714593546470155 ) ) ;
#64020 = CARTESIAN_POINT ( 'NONE',  ( -0.002360575507425215300, 1451.791349640477847, 154.0466420352841794 ) ) ;
#64021 = VERTEX_POINT ( 'NONE', #69397 ) ;
#64022 = CARTESIAN_POINT ( 'NONE',  ( -0.2934977098714270372, 1451.161884857989889, 182.5468558900879827 ) ) ;
#64023 = CARTESIAN_POINT ( 'NONE',  ( -16.00480266779999994, 1409.471960401030174, 192.4949821169979884 ) ) ;
#64024 = DIRECTION ( 'NONE',  ( 5.980589973904019347E-17, -1.000000000000000000, 1.736889445713099699E-16 ) ) ;
#64025 = CARTESIAN_POINT ( 'NONE',  ( -24.37563666778019922, 1439.900544325036890, 212.0182502291069682 ) ) ;
#64026 = CARTESIAN_POINT ( 'NONE',  ( -5.855016933008430513, 1434.745513377389898, 216.8132225448020165 ) ) ;
#64027 = CARTESIAN_POINT ( 'NONE',  ( -5.784678387216369622, 1511.501844456730169, 200.3524772839079731 ) ) ;
#64028 = FACE_OUTER_BOUND ( 'NONE', #31172, .T. ) ;
#64029 = CARTESIAN_POINT ( 'NONE',  ( -13.80599399759999990, 1434.979619872719923, 146.4346930356980181 ) ) ;
#64030 = CARTESIAN_POINT ( 'NONE',  ( -21.30823923614832083, 1524.382868172804365, 184.4507411017320919 ) ) ;
#64032 = DIRECTION ( 'NONE',  ( 1.000000000000000000, 7.763588443397869512E-10, 4.457073426249340046E-10 ) ) ;
#64031 = CARTESIAN_POINT ( 'NONE',  ( 4.523181926059999469, 1464.418891312029928, 235.2759163622980054 ) ) ;
#64033 = AXIS2_PLACEMENT_3D ( 'NONE', #30320, #72893, #21891 ) ;
#64034 = CARTESIAN_POINT ( 'NONE',  ( -1.124289693584999972, 1517.184063036290127, 215.6857614941170027 ) ) ;
#64035 = CARTESIAN_POINT ( 'NONE',  ( 11.15490121449999883, 1425.160561550830153, 144.1688093938980160 ) ) ;
#64036 = CARTESIAN_POINT ( 'NONE',  ( -0.1400231725758700196, 1507.707667440369960, 180.7851207917099998 ) ) ;
#64037 = CARTESIAN_POINT ( 'NONE',  ( 19.16976238839742308, 1443.680783661108762, 213.5402241685004299 ) ) ;
#64038 = CARTESIAN_POINT ( 'NONE',  ( 2.492130623175000448, 1516.778761582560037, 212.5675310476169955 ) ) ;
#64039 = CARTESIAN_POINT ( 'NONE',  ( -11.41675697748640061, 1482.775670443970057, 205.7339590229720159 ) ) ;
#64040 = CARTESIAN_POINT ( 'NONE',  ( 29.55269881708366597, 1525.821544997590536, 221.1141083160992764 ) ) ;
#64042 = VERTEX_POINT ( 'NONE', #49826 ) ;
#64041 = CARTESIAN_POINT ( 'NONE',  ( -4.124984636820000716, 1429.048548944989989, 205.3222558022289945 ) ) ;
#64043 = CARTESIAN_POINT ( 'NONE',  ( -1.689251544523377779, 1526.344110814223541, 178.4720708657796138 ) ) ;
#64044 = CARTESIAN_POINT ( 'NONE',  ( 25.18985267180000065, 1440.913060401160010, 217.4969598257980010 ) ) ;
#64045 = FACE_OUTER_BOUND ( 'NONE', #41568, .T. ) ;
#64046 = CARTESIAN_POINT ( 'NONE',  ( -15.53640578200000100, 1415.765361658500069, 208.3984121209330169 ) ) ;
#64047 = CARTESIAN_POINT ( 'NONE',  ( 1.984553072930000051, 1410.354529030129925, 232.0126999757980002 ) ) ;
#64048 = CARTESIAN_POINT ( 'NONE',  ( 16.77192111137855690, 1526.333389947941896, 183.3307103475321185 ) ) ;
#64049 = AXIS2_PLACEMENT_3D ( 'NONE', #17167, #20920, #12541 ) ;
#64050 = CARTESIAN_POINT ( 'NONE',  ( 18.02257621027576917, 1524.382868172863937, 182.8951942368371988 ) ) ;
#64052 = CARTESIAN_POINT ( 'NONE',  ( 5.362073334248089296, 1423.991816925989951, 150.1582991024129967 ) ) ;
#64051 = CARTESIAN_POINT ( 'NONE',  ( -22.30354652620000167, 1470.081838450430041, 222.1003071029979878 ) ) ;
#64053 = CARTESIAN_POINT ( 'NONE',  ( -1.570312491960000001, 1484.305737421829917, 182.5879718789979904 ) ) ;
#64054 = EDGE_LOOP ( 'NONE', ( #97825, #60428, #99628, #58879, #16581 ) ) ;
#64056 = AXIS2_PLACEMENT_3D ( 'NONE', #92552, #59531, #67943 ) ;
#64055 = CARTESIAN_POINT ( 'NONE',  ( -0.01306004006829850073, 1516.939762005280045, 204.5032625402269844 ) ) ;
#64057 = CARTESIAN_POINT ( 'NONE',  ( 2.107306259280000038, 1405.878280305930048, 267.2331469757979789 ) ) ;
#64058 = DIRECTION ( 'NONE',  ( -1.836970198721029688E-16, -1.000000000000000000, 0.000000000000000000 ) ) ;
#64059 = AXIS2_PLACEMENT_3D ( 'NONE', #102558, #16343, #7419 ) ;
#64060 = CARTESIAN_POINT ( 'NONE',  ( 20.81489508609670835, 1427.812437954155030, 220.0757061899427924 ) ) ;
#64061 = CARTESIAN_POINT ( 'NONE',  ( 1.166977143170000009, 1471.376848498290201, 188.9924741841990112 ) ) ;
#64062 = CARTESIAN_POINT ( 'NONE',  ( 21.13483499240000185, 1496.881468811689956, 208.7396410216740037 ) ) ;
#64063 = EDGE_CURVE ( 'NONE', #5861, #18354, #49034, .T. ) ;
#64064 = DIRECTION ( 'NONE',  ( -0.9455185755993178454, 0.000000000000000000, 0.3255681544571539243 ) ) ;
#64065 = DIRECTION ( 'NONE',  ( -1.000000000000000000, 1.836970198721029688E-16, 0.000000000000000000 ) ) ;
#64066 = CARTESIAN_POINT ( 'NONE',  ( -12.89832111469999987, 1444.960415658079910, 186.1351309691980020 ) ) ;
#64067 = EDGE_CURVE ( 'NONE', #58087, #75158, #49253, .T. ) ;
#64068 = CARTESIAN_POINT ( 'NONE',  ( 20.70484064406359437, 1525.907212628473872, 185.0411015109854134 ) ) ;
#64069 = CARTESIAN_POINT ( 'NONE',  ( -1.839380708780000040, 1507.096886517889970, 221.8368464039990045 ) ) ;
#64070 = CARTESIAN_POINT ( 'NONE',  ( -32.85805783624297760, 1523.678648413191695, 217.1983043299907763 ) ) ;
#64071 = CARTESIAN_POINT ( 'NONE',  ( -21.37693747720000204, 1440.913060387330006, 224.8635562088979896 ) ) ;
#64072 = FACE_OUTER_BOUND ( 'NONE', #9378, .T. ) ;
#64073 = CARTESIAN_POINT ( 'NONE',  ( 4.276646838899999636, 1441.052817498070226, 157.0212001317980253 ) ) ;
#64074 = CARTESIAN_POINT ( 'NONE',  ( -0.8892692271930000558, 1476.043852980030124, 268.4834379751979441 ) ) ;
#64076 = AXIS2_PLACEMENT_3D ( 'NONE', #21612, #98338, #80452 ) ;
#64075 = FACE_OUTER_BOUND ( 'NONE', #39889, .T. ) ;
#64077 = DIRECTION ( 'NONE',  ( -0.9993902469236100039, -0.03489947644259129567, 0.001077449766195760121 ) ) ;
#64078 = CARTESIAN_POINT ( 'NONE',  ( -2.884443514848614498, 1448.263804016322638, 184.3271468657659966 ) ) ;
#64079 = CARTESIAN_POINT ( 'NONE',  ( -38.22024519373950113, 1384.795465018370123, 239.1128382243029762 ) ) ;
#64080 = CARTESIAN_POINT ( 'NONE',  ( -4.486733153042460565, 1517.051705360449887, 216.7144192674729766 ) ) ;
#64081 = EDGE_CURVE ( 'NONE', #11098, #15049, #54631, .T. ) ;
#64082 = CARTESIAN_POINT ( 'NONE',  ( -105.2848455000000030, 1379.129118594349848, 302.8293157935589761 ) ) ;
#64083 = CARTESIAN_POINT ( 'NONE',  ( 31.11295621079038654, 1525.790286462508675, 216.3449408200586106 ) ) ;
#64084 = CARTESIAN_POINT ( 'NONE',  ( 0.1681674884180490159, 1420.473121907760060, 182.7464979049940155 ) ) ;
#64085 = CARTESIAN_POINT ( 'NONE',  ( -9.061987881421931235, 1396.229511977310040, 215.4630778420020079 ) ) ;
#64086 = CARTESIAN_POINT ( 'NONE',  ( -15.35035202399999932, 1421.192170133330137, 227.1237052556980132 ) ) ;
#64087 = CARTESIAN_POINT ( 'NONE',  ( 19.74164504280149757, 1455.376031929259852, 226.0788368184279875 ) ) ;
#64088 = ORIENTED_EDGE ( 'NONE', *, *, #43476, .F. ) ;
#64089 = CARTESIAN_POINT ( 'NONE',  ( -6.668618179459999240, 1472.084049029690050, 211.0614949439089969 ) ) ;
#64090 = CARTESIAN_POINT ( 'NONE',  ( 1.408975827199999920, 1408.962262904629824, 231.2047468183979788 ) ) ;
#64091 = CARTESIAN_POINT ( 'NONE',  ( -19.29374783221095768, 1526.349684470114653, 233.1524122426512236 ) ) ;
#64093 = CARTESIAN_POINT ( 'NONE',  ( -11.87063488596499816, 1512.258183966700017, 192.7384874028670083 ) ) ;
#64092 = CARTESIAN_POINT ( 'NONE',  ( 11.51898438939999991, 1425.941348201630035, 135.9196790177979892 ) ) ;
#64094 = CARTESIAN_POINT ( 'NONE',  ( -9859.020463813496463, 54.07981494722837823, 1360.877155230279641 ) ) ;
#64095 = CARTESIAN_POINT ( 'NONE',  ( -9.586136107779999804, 1449.725920977289888, 206.0133221225389946 ) ) ;
#64096 = TOROIDAL_SURFACE ( 'NONE', #92676, 1.000000000000000000, 1.000000000000000000 ) ;
#64097 = CARTESIAN_POINT ( 'NONE',  ( -0.01073133209419849937, 1516.939491476980038, 201.7897819926569980 ) ) ;
#64098 = CARTESIAN_POINT ( 'NONE',  ( 8.220300753029999186, 1427.204169894219831, 212.0038158565590152 ) ) ;
#64099 = CARTESIAN_POINT ( 'NONE',  ( -2.431412526649999961, 1428.647745098929818, 149.4227846719979880 ) ) ;
#64100 = CARTESIAN_POINT ( 'NONE',  ( 2.537844286819999517, 1508.894213628730085, 180.1480057510979975 ) ) ;
#64101 = DIRECTION ( 'NONE',  ( 0.8794237532950536229, -0.3862684439859148666, 0.2782275171889739274 ) ) ;
#64102 = CARTESIAN_POINT ( 'NONE',  ( -69.50772043394130151, 1378.360807531410046, 286.6555711028250357 ) ) ;
#64103 = EDGE_CURVE ( 'NONE', #28737, #71735, #25215, .T. ) ;
#64104 = CARTESIAN_POINT ( 'NONE',  ( 7.233739725823942202, 1366.686151722334898, 210.6218459617142003 ) ) ;
#64106 = ORIENTED_EDGE ( 'NONE', *, *, #11821, .T. ) ;
#64105 = FACE_OUTER_BOUND ( 'NONE', #47728, .T. ) ;
#64107 = EDGE_LOOP ( 'NONE', ( #33669, #30588, #16970, #55495 ) ) ;
#64108 = CARTESIAN_POINT ( 'NONE',  ( -12.02002121700249937, 1447.120365805550136, 187.5076542713389927 ) ) ;
#64109 = CYLINDRICAL_SURFACE ( 'NONE', #99956, 2.500000000000001776 ) ;
#64110 = CARTESIAN_POINT ( 'NONE',  ( 2.688591569480000221, 1509.006950921329917, 238.2845073959980198 ) ) ;
#64111 = CARTESIAN_POINT ( 'NONE',  ( -13.44670203181539492, 1444.308220740991374, 169.3633618578503217 ) ) ;
#64112 = CARTESIAN_POINT ( 'NONE',  ( 7.713339349770000020, 1475.513060387329915, 228.7257818846979944 ) ) ;
#64113 = CARTESIAN_POINT ( 'NONE',  ( -7.572192888655000509, 1511.308638870219966, 211.6864797536570109 ) ) ;
#64116 = ADVANCED_FACE ( 'NONE', ( #88379 ), #78319, .F. ) ;
#64115 = CARTESIAN_POINT ( 'NONE',  ( -1.358297888627590044, 1411.672670050000079, 185.5471854834340206 ) ) ;
#64114 = CARTESIAN_POINT ( 'NONE',  ( -8.697719184660000380, 1384.095450953160025, 218.5750472044589969 ) ) ;
#64117 = CARTESIAN_POINT ( 'NONE',  ( -30.31940284289330734, 1523.456924617338245, 195.7503880522716315 ) ) ;
#64118 = CARTESIAN_POINT ( 'NONE',  ( -2.400179225536239969, 1464.934988852220158, 198.3730454101489897 ) ) ;
#64119 = CARTESIAN_POINT ( 'NONE',  ( -39.13294756354380155, 1449.732214584349776, 134.8601900050019822 ) ) ;
#64120 = CARTESIAN_POINT ( 'NONE',  ( 41.15111780865080249, 1443.645529726370114, 136.9181479281729992 ) ) ;
#64121 = CARTESIAN_POINT ( 'NONE',  ( 8.582644122214238891, 1396.212772926450043, 216.0935766074430262 ) ) ;
#64122 = CARTESIAN_POINT ( 'NONE',  ( -39.08794880019009810, 1436.812182271670054, 136.3558420284400086 ) ) ;
#64123 = FACE_OUTER_BOUND ( 'NONE', #108631, .T. ) ;
#64124 = CYLINDRICAL_SURFACE ( 'NONE', #59047, 0.9999999999999522604 ) ;
#64125 = EDGE_LOOP ( 'NONE', ( #91793, #43031, #48242, #16159, #104162 ) ) ;
#64126 = DIRECTION ( 'NONE',  ( -0.5877852522924629231, 0.000000000000000000, 0.8090169943749548898 ) ) ;
#64127 = CARTESIAN_POINT ( 'NONE',  ( 21.59934095315572478, 1525.137881624885267, 233.5034356062079155 ) ) ;
#64128 = ORIENTED_EDGE ( 'NONE', *, *, #96652, .T. ) ;
#64129 = ORIENTED_EDGE ( 'NONE', *, *, #83766, .F. ) ;
#64130 = CARTESIAN_POINT ( 'NONE',  ( -19.29280426250840108, 1478.092759466889902, 227.9528384731270023 ) ) ;
#64131 = FACE_OUTER_BOUND ( 'NONE', #36794, .T. ) ;
#64132 = AXIS2_PLACEMENT_3D ( 'NONE', #87789, #11071, #28977 ) ;
#64133 = CARTESIAN_POINT ( 'NONE',  ( -13.92379579760000041, 1452.815214893629900, 195.1322242606980240 ) ) ;
#64134 = CARTESIAN_POINT ( 'NONE',  ( 8.881784196999999612E-15, 1441.261220175949802, 126.8032249175980155 ) ) ;
#64135 = CARTESIAN_POINT ( 'NONE',  ( 4.037378256055000669, 1516.688761843659904, 215.6706679112870120 ) ) ;
#64136 = CARTESIAN_POINT ( 'NONE',  ( -14.48029645964409973, 1380.025135367679923, 208.7108227440779729 ) ) ;
#64137 = AXIS2_PLACEMENT_3D ( 'NONE', #98485, #106882, #91741 ) ;
#64138 = ORIENTED_EDGE ( 'NONE', *, *, #60455, .T. ) ;
#64139 = CARTESIAN_POINT ( 'NONE',  ( -11.60004869885202083, 1426.267714527815315, 138.3561744208223274 ) ) ;
#64140 = CARTESIAN_POINT ( 'NONE',  ( 2.500000000000000000, 1448.712186460370049, 157.7132982831409720 ) ) ;
#64141 = CARTESIAN_POINT ( 'NONE',  ( -44.32302097390000029, 1380.083786706710043, 232.1686497034590104 ) ) ;
#64142 = CIRCLE ( 'NONE', #22910, 10.00000000000000000 ) ;
#64143 =( BOUNDED_CURVE ( )  B_SPLINE_CURVE ( 3, ( #70957, #53030, #2084, #88273 ),
 .UNSPECIFIED., .F., .T. ) 
 B_SPLINE_CURVE_WITH_KNOTS ( ( 4, 4 ),
 ( 4.712388980384689674, 6.283185307179586232 ),
 .UNSPECIFIED. ) 
 CURVE ( )  GEOMETRIC_REPRESENTATION_ITEM ( )  RATIONAL_B_SPLINE_CURVE ( ( 1.000000000000000000, 0.8047378541243649375, 0.8047378541243649375, 1.000000000000000000 ) ) 
 REPRESENTATION_ITEM ( '' )  );
#64144 = CARTESIAN_POINT ( 'NONE',  ( 15.71890336570000102, 1414.913060387229962, 214.6699778313279978 ) ) ;
#64145 = CARTESIAN_POINT ( 'NONE',  ( 6.937338745574999521, 1516.706638732659940, 204.5037262658370025 ) ) ;
#64146 = ORIENTED_EDGE ( 'NONE', *, *, #34185, .F. ) ;
#64147 = CARTESIAN_POINT ( 'NONE',  ( -12.06562581462340056, 1489.842093712740052, 211.0982364962250131 ) ) ;
#64148 = CARTESIAN_POINT ( 'NONE',  ( -36.69969584994223766, 1426.055895651937817, 269.5559544832055394 ) ) ;
#64149 = CARTESIAN_POINT ( 'NONE',  ( -8.354921657429999371, 1410.136853626930133, 230.4734767913980136 ) ) ;
#64151 = ORIENTED_EDGE ( 'NONE', *, *, #13319, .F. ) ;
#64150 = CARTESIAN_POINT ( 'NONE',  ( -13.22806383159999832, 1431.113060387329824, 194.5140223583980230 ) ) ;
#64152 = CARTESIAN_POINT ( 'NONE',  ( -0.004457925198051789981, 1451.027869956220002, 181.9225055831719828 ) ) ;
#64153 = CARTESIAN_POINT ( 'NONE',  ( -28.88351707065390173, 1440.913060387269979, 234.5452952734219991 ) ) ;
#64154 = CARTESIAN_POINT ( 'NONE',  ( -25.94071553730000090, 1384.508713631559885, 224.2416845492589914 ) ) ;
#64155 = CARTESIAN_POINT ( 'NONE',  ( 9.600864221749999317, 1470.542902921190034, 212.2537306481789869 ) ) ;
#64156 = VECTOR ( 'NONE', #83504, 1000.000000000000114 ) ;
#64157 = CARTESIAN_POINT ( 'NONE',  ( 25.02520634413389899, 1415.439183875560047, 270.1035392086070033 ) ) ;
#64158 = CARTESIAN_POINT ( 'NONE',  ( -5.772727946874999461, 1516.691414181030041, 212.5791125756269935 ) ) ;
#64159 = CARTESIAN_POINT ( 'NONE',  ( -62.95758008990000576, 1379.733836041129962, 267.9697104864590074 ) ) ;
#64160 = CARTESIAN_POINT ( 'NONE',  ( 23.59717156689999840, 1410.840126738630033, 207.8450998541779882 ) ) ;
#64161 = CYLINDRICAL_SURFACE ( 'NONE', #37436, 2.000000000000003109 ) ;
#64162 = CARTESIAN_POINT ( 'NONE',  ( 9.633401174267049782, 1425.762329347420291, 193.8812324694129927 ) ) ;
#64163 = CARTESIAN_POINT ( 'NONE',  ( -7.717618918966349995, 1516.862251239950183, 209.3707541584199987 ) ) ;
#64164 = CARTESIAN_POINT ( 'NONE',  ( 2.486220101774999858, 1516.939658295650133, 209.1086089184300079 ) ) ;
#64165 = CARTESIAN_POINT ( 'NONE',  ( 4.218374993917859861, 1420.932961763340245, 185.4447900071560014 ) ) ;
#64166 = CARTESIAN_POINT ( 'NONE',  ( -10.34676626709999780, 1420.438686667429920, 229.9603813012979856 ) ) ;
#64167 = CARTESIAN_POINT ( 'NONE',  ( -76.09690353929998707, 1385.004314140359838, 301.2232021421590389 ) ) ;
#64168 = ORIENTED_EDGE ( 'NONE', *, *, #81541, .T. ) ;
#64169 = CARTESIAN_POINT ( 'NONE',  ( -21.27099332670459830, 1385.271245282970085, 221.4929286867449889 ) ) ;
#64170 = CARTESIAN_POINT ( 'NONE',  ( -2.873525832259999913, 1429.447207211989962, 200.9398776307089918 ) ) ;
#64171 = CARTESIAN_POINT ( 'NONE',  ( 0.5260898116900000199, 1417.366494600629949, 235.1724886678979942 ) ) ;
#64172 = CARTESIAN_POINT ( 'NONE',  ( -21.39771622935050033, 1509.704956904690107, 229.7894228794980052 ) ) ;
#64173 = DIRECTION ( 'NONE',  ( -4.336808689942001466E-16, -0.02617694830786544691, -0.9996573249755575929 ) ) ;
#64174 = CARTESIAN_POINT ( 'NONE',  ( 11.23217089400000113, 1422.349028627020061, 203.7645952894689856 ) ) ;
#64175 = CARTESIAN_POINT ( 'NONE',  ( -1.906499846882070084E-08, 1517.051704408389924, 209.1218459511669892 ) ) ;
#64177 = CARTESIAN_POINT ( 'NONE',  ( -3.558358604862239982, 1455.955982659530036, 200.3550966546550001 ) ) ;
#64176 = CARTESIAN_POINT ( 'NONE',  ( 6.942973629204999497, 1516.833844030519913, 216.4505221401170161 ) ) ;
#64178 = FACE_OUTER_BOUND ( 'NONE', #56870, .T. ) ;
#64179 = CARTESIAN_POINT ( 'NONE',  ( 10.46907846689019905, 1470.153368976490128, 208.0239820498049994 ) ) ;
#64180 = VERTEX_POINT ( 'NONE', #28475 ) ;
#64181 = CARTESIAN_POINT ( 'NONE',  ( 2.483949940595000516, 1517.156142772249950, 202.1710124019969896 ) ) ;
#64182 = CARTESIAN_POINT ( 'NONE',  ( -15.87603345926499898, 1512.359593911809952, 220.1461273412669755 ) ) ;
#64183 = EDGE_LOOP ( 'NONE', ( #40392, #77225, #101031, #5525 ) ) ;
#64184 = CARTESIAN_POINT ( 'NONE',  ( 11.60004869885204215, 1426.320646328452540, 137.6121508069457207 ) ) ;
#64185 = CARTESIAN_POINT ( 'NONE',  ( 17.90653978779999989, 1430.488564755489961, 212.6866031076790193 ) ) ;
#64186 = CARTESIAN_POINT ( 'NONE',  ( 7.937878408760115079, 1423.739882246193247, 195.8491950690135468 ) ) ;
#64187 = CARTESIAN_POINT ( 'NONE',  ( 2.390248854959999836, 1443.517510617689823, 217.7159995093989835 ) ) ;
#64188 = CARTESIAN_POINT ( 'NONE',  ( -26.40049011798170042, 1508.358675285229992, 201.5240040975259888 ) ) ;
#64189 = CARTESIAN_POINT ( 'NONE',  ( -2.500000000000000000, 1448.210448412289907, 170.5244215879980061 ) ) ;
#64190 = CARTESIAN_POINT ( 'NONE',  ( -20.35065116390000028, 1427.808792947530037, 223.1463981920979904 ) ) ;
#64191 = CARTESIAN_POINT ( 'NONE',  ( 7.896860026827476453, 1487.333077441552632, 201.7073600637725690 ) ) ;
#64192 = CARTESIAN_POINT ( 'NONE',  ( -105.7922211859999919, 1391.737185282639985, 301.9078056316589596 ) ) ;
#64193 = CARTESIAN_POINT ( 'NONE',  ( 19.87072075760000089, 1498.082836619830005, 189.6522194475979859 ) ) ;
#64195 = CARTESIAN_POINT ( 'NONE',  ( 29.75012120190000076, 1509.993914123429931, 209.6841247587719863 ) ) ;
#64194 = CARTESIAN_POINT ( 'NONE',  ( -107.4307047400000101, 1391.913060387289988, 300.8770155100590387 ) ) ;
#64196 = CARTESIAN_POINT ( 'NONE',  ( 2.534335827540424191, 1523.982201850120191, 242.5731047040208068 ) ) ;
#64197 = ORIENTED_EDGE ( 'NONE', *, *, #17197, .F. ) ;
#64198 = DIRECTION ( 'NONE',  ( 0.000000000000000000, 0.06174578541841399537, -0.9980919085851078787 ) ) ;
#64199 = CARTESIAN_POINT ( 'NONE',  ( -9.487584436799998855, 1508.516108850790033, 218.8016808830589923 ) ) ;
#64200 = CARTESIAN_POINT ( 'NONE',  ( 4.487249753905000027, 1509.038615934239942, 209.1218459511669892 ) ) ;
#64201 = CARTESIAN_POINT ( 'NONE',  ( 11.17215557887869970, 1470.323562617609923, 207.0621806280969963 ) ) ;
#64202 = CARTESIAN_POINT ( 'NONE',  ( -4.205583201319999631, 1483.725063651190112, 199.3005808441589863 ) ) ;
#64203 = CARTESIAN_POINT ( 'NONE',  ( -18.47399050599999626, 1509.320896585530136, 230.4813978294980075 ) ) ;
#64204 = CARTESIAN_POINT ( 'NONE',  ( -2.472529913803020563, 1523.678648413191695, 242.8674788698241400 ) ) ;
#64205 = CARTESIAN_POINT ( 'NONE',  ( -13.25797267067026475, 1444.641804557892556, 186.6667489211167776 ) ) ;
#64206 = CARTESIAN_POINT ( 'NONE',  ( -17.36801837519999836, 1414.983771848829747, 207.7378529488679817 ) ) ;
#64207 = DIRECTION ( 'NONE',  ( -0.1010290445074239624, 0.000000000000000000, 0.9948834766775036531 ) ) ;
#64208 = CIRCLE ( 'NONE', #55330, 419.2957457743311807 ) ;
#64209 = CARTESIAN_POINT ( 'NONE',  ( 24.04366906972200013, 1494.655619859800026, 207.1743914002310021 ) ) ;
#64211 = ADVANCED_FACE ( 'NONE', ( #72161 ), #45295, .T. ) ;
#64210 = CARTESIAN_POINT ( 'NONE',  ( -14.30833984952479909, 1415.677402203010161, 204.8799990442770138 ) ) ;
#64212 = AXIS2_PLACEMENT_3D ( 'NONE', #103378, #51908, #86048 ) ;
#64213 = CARTESIAN_POINT ( 'NONE',  ( -9.658233005175830499, 1460.589625460329898, 208.7565551244479991 ) ) ;
#64214 = CARTESIAN_POINT ( 'NONE',  ( 6.092650983240000429, 1427.361657835570213, 214.7380281929690113 ) ) ;
#64216 = VERTEX_POINT ( 'NONE', #71625 ) ;
#64215 = CARTESIAN_POINT ( 'NONE',  ( 4.511930455219999914, 1492.982136831589969, 216.2205869640490050 ) ) ;
#64217 = CARTESIAN_POINT ( 'NONE',  ( -96.36158319419999430, 1382.338469500439942, 309.9311367202590191 ) ) ;
#64218 = CARTESIAN_POINT ( 'NONE',  ( 14.02477538797010048, 1513.114148093580070, 224.3898003711330205 ) ) ;
#64219 = EDGE_CURVE ( 'NONE', #25603, #91513, #60540, .T. ) ;
#64220 = ORIENTED_EDGE ( 'NONE', *, *, #73258, .T. ) ;
#64221 = VERTEX_POINT ( 'NONE', #36867 ) ;
#64222 = CARTESIAN_POINT ( 'NONE',  ( 26.10691348580380122, 1471.192541839159958, 207.6971073565250094 ) ) ;
#64223 = CARTESIAN_POINT ( 'NONE',  ( 13.53422276719999928, 1509.381727759229989, 234.4599784456980274 ) ) ;
#64224 = CARTESIAN_POINT ( 'NONE',  ( -9.082617507235918097, 1381.499571894695009, 200.6641547696254975 ) ) ;
#64226 = CARTESIAN_POINT ( 'NONE',  ( -34.48978217849999339, 1440.913060389249949, 250.0021841876980488 ) ) ;
#64225 = CARTESIAN_POINT ( 'NONE',  ( 33.44398265167041728, 1422.464213849851376, 269.5109561759928738 ) ) ;
#64227 = CARTESIAN_POINT ( 'NONE',  ( -19.51711174489999934, 1484.705571712129768, 189.8616710270979979 ) ) ;
#64228 = CARTESIAN_POINT ( 'NONE',  ( -11.80297485880000075, 1433.621679574930113, 150.7677425477979796 ) ) ;
#64229 = CARTESIAN_POINT ( 'NONE',  ( 2.470168521978398424, 1523.382868172864164, 242.8787258963054683 ) ) ;
#64230 = CARTESIAN_POINT ( 'NONE',  ( -19.61483391129999987, 1485.816994056529893, 190.1275648953979953 ) ) ;
#64231 = CIRCLE ( 'NONE', #39171, 2.000055272426020991 ) ;
#64232 = DIRECTION ( 'NONE',  ( 1.755985294532464991E-16, -1.000000000000000000, 1.338183447452830017E-16 ) ) ;
#64233 = CARTESIAN_POINT ( 'NONE',  ( -2.057041824809119568, 1523.342713519622521, 244.8463988825372724 ) ) ;
#64234 = CARTESIAN_POINT ( 'NONE',  ( 0.6915095762648889588, 1515.131927850350166, 213.4495367465950153 ) ) ;
#64235 = CARTESIAN_POINT ( 'NONE',  ( 7.878537825433329367, 1522.051704408389924, 200.0586249522280013 ) ) ;
#64236 = CARTESIAN_POINT ( 'NONE',  ( -4.594317082651300232, 1476.940951215450013, 219.6856609997009855 ) ) ;
#64238 = CARTESIAN_POINT ( 'NONE',  ( 1.655301970317450966, 1361.639372583430031, 210.6218459617142003 ) ) ;
#64237 = B_SPLINE_CURVE_WITH_KNOTS ( 'NONE', 5,
 ( #35434, #20274, #61231, #80200, #27044, #27585 ),
 .UNSPECIFIED., .F., .F.,
 ( 6, 6 ),
 ( 0.000000000000000000, 1.000000000000000000 ),
 .UNSPECIFIED. ) ;
#64239 = CARTESIAN_POINT ( 'NONE',  ( 30.51231035492520149, 1526.382868172863937, 200.0858385050239008 ) ) ;
#64241 = ORIENTED_EDGE ( 'NONE', *, *, #69020, .T. ) ;
#64240 = CARTESIAN_POINT ( 'NONE',  ( 2.409488808553320245E-09, 1410.450358379310046, 257.5163489258059712 ) ) ;
#64242 = ORIENTED_EDGE ( 'NONE', *, *, #75729, .T. ) ;
#64243 = CARTESIAN_POINT ( 'NONE',  ( -11.86504885435570067, 1432.262511493439888, 149.9818936695930063 ) ) ;
#64244 = CARTESIAN_POINT ( 'NONE',  ( 16.57070253540619831, 1493.685518685909983, 193.1449767612709820 ) ) ;
#64245 = CARTESIAN_POINT ( 'NONE',  ( -24.70945393470000084, 1465.793440313629844, 269.4189447651980345 ) ) ;
#64246 = CARTESIAN_POINT ( 'NONE',  ( 11.61220494760000044, 1420.579219889470096, 199.3493800206389892 ) ) ;
#64247 = DIRECTION ( 'NONE',  ( 0.1070030146457371656, 0.000000000000000000, -0.9942586961433751425 ) ) ;
#64248 = CARTESIAN_POINT ( 'NONE',  ( 33.92638623454369906, 1450.868589251249887, 136.1710234410380167 ) ) ;
#64249 = CARTESIAN_POINT ( 'NONE',  ( 0.2603518607207219726, 1451.283950821710050, 182.4357641078530037 ) ) ;
#64250 = DIRECTION ( 'NONE',  ( 0.000000000000000000, 0.000000000000000000, 1.000000000000000000 ) ) ;
#64251 = CARTESIAN_POINT ( 'NONE',  ( 1.408274608409999740, 1457.262919913989890, 199.5821060027690237 ) ) ;
#64252 = CARTESIAN_POINT ( 'NONE',  ( -12.54268436849999979, 1408.913060387329779, 196.5791615931979948 ) ) ;
#64253 = CARTESIAN_POINT ( 'NONE',  ( 9.258247136799999666, 1363.198586359130104, 207.6218459616989946 ) ) ;
#64254 = CARTESIAN_POINT ( 'NONE',  ( -33.48176124307740764, 1416.813162719589855, 268.8725262323869742 ) ) ;
#64255 = ORIENTED_EDGE ( 'NONE', *, *, #105614, .F. ) ;
#64256 = CARTESIAN_POINT ( 'NONE',  ( -3.533922947849859941, 1492.310067042970104, 181.6079149013590097 ) ) ;
#64257 = ORIENTED_EDGE ( 'NONE', *, *, #103603, .T. ) ;
#64258 = ORIENTED_EDGE ( 'NONE', *, *, #3657, .F. ) ;
#64259 = CARTESIAN_POINT ( 'NONE',  ( 3.269184908365000197, 1516.940296199220029, 211.4060453336370244 ) ) ;
#64260 = CARTESIAN_POINT ( 'NONE',  ( 4.778748612485856029, 1423.572762554393194, 184.0460358434518469 ) ) ;
#64262 = FILL_AREA_STYLE ('',( #30072 ) ) ;
#64261 = CARTESIAN_POINT ( 'NONE',  ( -4.996642198295000448, 1516.697242742309982, 211.9989590406970024 ) ) ;
#64263 = CARTESIAN_POINT ( 'NONE',  ( -4.345522541100000247, 1440.427655379589851, 185.4586955749979893 ) ) ;
#64264 = VECTOR ( 'NONE', #9195, 999.9999999999998863 ) ;
#64265 = DIRECTION ( 'NONE',  ( 0.4794255386042031719, 0.000000000000000000, 0.8775825618903726477 ) ) ;
#64266 = B_SPLINE_SURFACE_WITH_KNOTS ( 'NONE', 5, 5, ( 
 ( #31639, #99937, #23232, #68035, #18141, #60744, #69135, #94866, #59620 ),
 ( #61305, #52338, #53442, #9214, #69702, #85909, #87587, #95971, #60178 ),
 ( #61852, #86460, #35509, #94295, #44478, #95423, #70261, #34406, #104369 ),
 ( #280, #10876, #17573, #93731, #27665, #19232, #25979, #9751, #45047 ),
 ( #52884, #79192, #17010, #34952, #10304, #1939, #43374, #51773, #25425 ),
 ( #33844, #87012, #77522, #822, #102144, #103239, #26550, #103821, #78624 ),
 ( #51209, #36076, #85339, #8636, #43917, #42811, #78063, #76971, #18686 ),
 ( #68579, #1366, #27120, #102683, #63512, #28214, #88689, #29861, #97630 ),
 ( #11968, #38260, #54555, #21980, #64601, #28773, #46152, #30412, #55097 ) ),
 .UNSPECIFIED., .F., .F., .F.,
 ( 6, 3, 6 ),
 ( 6, 3, 6 ),
 ( 51.29329440469999923, 55.70673016509999798, 65.19347039801400001 ),
 ( -8.782821396822089466E-05, 1.000000000000000000, 2.000000000000000000 ),
 .UNSPECIFIED. ) ;
#64267 = ORIENTED_EDGE ( 'NONE', *, *, #55126, .F. ) ;
#64268 = CARTESIAN_POINT ( 'NONE',  ( -26.79919838190000192, 1436.600005541920154, 136.7628791570980127 ) ) ;
#64269 = B_SPLINE_CURVE_WITH_KNOTS ( 'NONE', 3,
 ( #32959, #67148, #65493, #24545, #40816, #15041, #99603, #58733, #22886, #57096, #74995, #91221, #107464, #32426, #66605, #58186, #15585, #83921, #92870, #99054, #7764, #30759, #73329, #14502, #68266, #17237, #85016, #16687, #50884, #34073, #102373, #60965, #86135, #18357, #69361, #101809, #8310, #33499, #94519, #110782, #25101, #60400, #103471, #77199, #59306, #95640, #104035, #25656, #26778, #502, #8859, #43042, #52551, #9978, #51432 ),
 .UNSPECIFIED., .F., .F.,
 ( 4, 3, 3, 3, 3, 3, 3, 3, 3, 3, 3, 3, 3, 3, 3, 3, 3, 3, 4 ),
 ( 9.902195898180000455, 10.17210527305439882, 10.45530577770670000, 10.70141353110000004, 11.00396970307760114, 11.32322756684139975, 11.52456852350000105, 11.84989040644859948, 12.16242387756629917, 12.38020728900000123, 12.74551463659910056, 13.12275145100690033, 13.53252099859349933, 13.95359103984709925, 14.40783883437189949, 14.91487510439959863, 15.44821056985129992, 15.94145638718300084, 16.40090783169999966 ),
 .UNSPECIFIED. ) ;
#64270 = CARTESIAN_POINT ( 'NONE',  ( -6.942973667334999988, 1516.833844030519913, 201.7931697622170191 ) ) ;
#64271 = AXIS2_PLACEMENT_3D ( 'NONE', #17912, #75656, #50458 ) ;
#64272 = CYLINDRICAL_SURFACE ( 'NONE', #58857, 4.999999999999991118 ) ;
#64273 = CARTESIAN_POINT ( 'NONE',  ( 1.854736326702351557, 1508.995493199552357, 238.6295539663279612 ) ) ;
#64274 =( BOUNDED_CURVE ( )  B_SPLINE_CURVE ( 3, ( #6584, #20205, #74908, #12357 ),
 .UNSPECIFIED., .F., .T. ) 
 B_SPLINE_CURVE_WITH_KNOTS ( ( 4, 4 ),
 ( 4.033485614218559334, 4.137218124529905339 ),
 .UNSPECIFIED. ) 
 CURVE ( )  GEOMETRIC_REPRESENTATION_ITEM ( )  RATIONAL_B_SPLINE_CURVE ( ( 1.000000000000000000, 0.9991034981929989289, 0.9991034981929989289, 1.000000000000000000 ) ) 
 REPRESENTATION_ITEM ( '' )  );
#64275 = CARTESIAN_POINT ( 'NONE',  ( -26.64547680037770405, 1415.060613070530053, 270.3501199617340376 ) ) ;
#64276 = CARTESIAN_POINT ( 'NONE',  ( -26.79413315976150045, 1435.433175095809929, 135.2874648155150226 ) ) ;
#64277 = CARTESIAN_POINT ( 'NONE',  ( 8.559887967433979838, 1437.031052010680014, 207.9845883466809937 ) ) ;
#64279 = VERTEX_POINT ( 'NONE', #54791 ) ;
#64278 = CARTESIAN_POINT ( 'NONE',  ( -7.988138845717701386, 1364.969037029785568, 209.6218459617148824 ) ) ;
#64280 = ORIENTED_EDGE ( 'NONE', *, *, #44202, .T. ) ;
#64281 = CARTESIAN_POINT ( 'NONE',  ( 34.06334320139256988, 1463.667877587127350, 269.2714786605345125 ) ) ;
#64282 = CARTESIAN_POINT ( 'NONE',  ( 11.03771696505579847, 1471.764929341090237, 212.0955496467459795 ) ) ;
#64283 = CARTESIAN_POINT ( 'NONE',  ( -2.500000000000000000, 1419.383100980419840, 144.1003751433630100 ) ) ;
#64284 = CARTESIAN_POINT ( 'NONE',  ( -1.326721101379999990, 1486.243302057330084, 181.7592321280980059 ) ) ;
#64286 = CARTESIAN_POINT ( 'NONE',  ( 5.789394662204999875, 1517.164987839469859, 210.8286437561770299 ) ) ;
#64285 = AXIS2_PLACEMENT_3D ( 'NONE', #107815, #28912, #54687 ) ;
#64287 = CARTESIAN_POINT ( 'NONE',  ( -17.92173952435889817, 1415.219159633810023, 207.5658729395169928 ) ) ;
#64288 = CARTESIAN_POINT ( 'NONE',  ( -7.722580350941189664, 1517.051704403100075, 204.5317855550379988 ) ) ;
#64289 = CIRCLE ( 'NONE', #28462, 2.000000000000003109 ) ;
#64290 = CARTESIAN_POINT ( 'NONE',  ( -14.51195731179999981, 1426.817867355729959, 222.0493599474980044 ) ) ;
#64291 = CARTESIAN_POINT ( 'NONE',  ( 12.30733358380000020, 1416.021639799829927, 223.3557834255979913 ) ) ;
#64292 = CARTESIAN_POINT ( 'NONE',  ( 7.784559201385000016, 1511.207707629420156, 205.1306841488269868 ) ) ;
#64293 = ORIENTED_EDGE ( 'NONE', *, *, #53892, .T. ) ;
#64294 = CARTESIAN_POINT ( 'NONE',  ( 2.477373605864999995, 1516.891731298979948, 206.2406231745169976 ) ) ;
#64295 = ORIENTED_EDGE ( 'NONE', *, *, #5680, .T. ) ;
#64296 = DIRECTION ( 'NONE',  ( -0.6736849260863841948, 0.000000000000000000, 0.7390186874254148774 ) ) ;
#64297 = CARTESIAN_POINT ( 'NONE',  ( -22.44240218647486529, 1451.734269296826824, 219.6387502286748088 ) ) ;
#64298 = ORIENTED_EDGE ( 'NONE', *, *, #104366, .T. ) ;
#64299 = CARTESIAN_POINT ( 'NONE',  ( 0.3722769099684289928, 1457.826255237599980, 228.9731060096619899 ) ) ;
#64300 = CARTESIAN_POINT ( 'NONE',  ( -2.919081270098979441, 1368.383855509380055, 210.4211783971049954 ) ) ;
#64301 = CARTESIAN_POINT ( 'NONE',  ( 13.22475641109999955, 1415.063410489729904, 197.5370647170979623 ) ) ;
#64302 = CARTESIAN_POINT ( 'NONE',  ( -8.838153826319999240, 1416.011808640619847, 204.9871024205990011 ) ) ;
#64303 = CARTESIAN_POINT ( 'NONE',  ( 21.78252905899999803, 1409.837820636329980, 204.8395344835479932 ) ) ;
#64304 = CARTESIAN_POINT ( 'NONE',  ( 28.06188869160000010, 1444.994950788469851, 168.7697867250980153 ) ) ;
#64305 = CARTESIAN_POINT ( 'NONE',  ( 16.03391504160000025, 1409.472977038530189, 225.2054435686980014 ) ) ;
#64306 = CARTESIAN_POINT ( 'NONE',  ( 10.79356334649999916, 1490.085259999289974, 207.2636451086090119 ) ) ;
#64307 = CARTESIAN_POINT ( 'NONE',  ( 2.398688105316478580, 1426.758990796949320, 141.3562649765487436 ) ) ;
#64308 = CARTESIAN_POINT ( 'NONE',  ( 23.32143419377827698, 1449.605800993310140, 217.2891594252025982 ) ) ;
#64309 = CIRCLE ( 'NONE', #14162, 0.9999999999999326095 ) ;
#64310 = CARTESIAN_POINT ( 'NONE',  ( -21.62164173379369814, 1517.151704408390060, 210.2163513719069954 ) ) ;
#64311 = CARTESIAN_POINT ( 'NONE',  ( -4.032397940005000514, 1516.981965530290154, 214.9074288837770155 ) ) ;
#64312 = EDGE_LOOP ( 'NONE', ( #68516, #108318, #51601, #61430 ) ) ;
#64313 = CARTESIAN_POINT ( 'NONE',  ( 7.708916871849369024, 1516.529918593650109, 207.1343159654149986 ) ) ;
#64314 = DIRECTION ( 'NONE',  ( 0.000000000000000000, -6.123233995736769734E-17, -1.000000000000000000 ) ) ;
#64315 = CARTESIAN_POINT ( 'NONE',  ( -2.500000000000000000, 1448.210448412289907, 183.1418046153980015 ) ) ;
#64316 = DIRECTION ( 'NONE',  ( -0.9942586961433764747, 2.969930264099993005E-15, -0.1070030146457249115 ) ) ;
#64317 = CARTESIAN_POINT ( 'NONE',  ( -38.85669708052029847, 1447.921392184620117, 136.5057008105069940 ) ) ;
#64318 = CARTESIAN_POINT ( 'NONE',  ( 11.60004869885203682, 1425.908350318139355, 137.5340513747880777 ) ) ;
#64319 = CARTESIAN_POINT ( 'NONE',  ( 2.493582918933280101, 1417.705059006696047, 233.7388004561698551 ) ) ;
#64320 = AXIS2_PLACEMENT_3D ( 'NONE', #13779, #72620, #82666 ) ;
#64321 = CARTESIAN_POINT ( 'NONE',  ( -1.923670262848290013, 1471.323487510810082, 183.5084292385340063 ) ) ;
#64322 = CARTESIAN_POINT ( 'NONE',  ( 1.608912855160989919, 1456.301673701370191, 198.6631191214040086 ) ) ;
#64323 = CARTESIAN_POINT ( 'NONE',  ( -15.18874088736159855, 1472.514660487180208, 270.0929918628660289 ) ) ;
#64324 = CARTESIAN_POINT ( 'NONE',  ( 28.59384819061660110, 1440.913060387340010, 233.4742120170059820 ) ) ;
#64325 = CARTESIAN_POINT ( 'NONE',  ( -10.88819247137429969, 1470.683299348469973, 210.3143062069100040 ) ) ;
#64326 = FACE_BOUND ( 'NONE', #61484, .T. ) ;
#64327 = ORIENTED_EDGE ( 'NONE', *, *, #11184, .T. ) ;
#64328 = DIRECTION ( 'NONE',  ( -1.755985294532469921E-16, 1.000000000000000000, -1.338183447452831989E-16 ) ) ;
#64329 = LINE ( 'NONE', #4943, #90789 ) ;
#64330 = CARTESIAN_POINT ( 'NONE',  ( -29.06854782859999986, 1509.928156445530021, 211.9488907393379975 ) ) ;
#64331 = CARTESIAN_POINT ( 'NONE',  ( 2.380922373579999807, 1474.722219450530019, 234.6118303102979894 ) ) ;
#64332 = B_SPLINE_CURVE_WITH_KNOTS ( 'NONE', 5,
 ( #32626, #14710, #66259, #100377, #100903, #101448, #23662, #57845, #81911, #39370, #16884, #43782 ),
 .UNSPECIFIED., .F., .F.,
 ( 6, 3, 3, 6 ),
 ( 0.000000000000000000, 0.4215567365674310341, 0.8072018686246260621, 1.000000000000000000 ),
 .UNSPECIFIED. ) ;
#64333 = CARTESIAN_POINT ( 'NONE',  ( -16.73628186595805545, 1526.382868172864164, 234.1845039693045862 ) ) ;
#64334 = CARTESIAN_POINT ( 'NONE',  ( 8.051697842710000330, 1428.206416439490113, 213.2401734540090104 ) ) ;
#64335 = CARTESIAN_POINT ( 'NONE',  ( -37.50821108740120025, 1383.831899505290039, 237.6397739250450059 ) ) ;
#64336 = DIRECTION ( 'NONE',  ( 1.000000000000000000, 0.000000000000000000, 0.000000000000000000 ) ) ;
#64337 = CARTESIAN_POINT ( 'NONE',  ( 6.972733162820000885, 1409.156553594830029, 222.0127823373979936 ) ) ;
#64338 = CARTESIAN_POINT ( 'NONE',  ( -6.009430644317174774, 1511.590044791479613, 200.3317612525653146 ) ) ;
#64339 = CARTESIAN_POINT ( 'NONE',  ( 2.689345562130000200, 1464.716346730230043, 236.9361815678979895 ) ) ;
#64341 = ORIENTED_EDGE ( 'NONE', *, *, #5942, .F. ) ;
#64340 = CARTESIAN_POINT ( 'NONE',  ( -4.987078460856490203, 1508.551704408389924, 212.6094383991630252 ) ) ;
#64342 = CARTESIAN_POINT ( 'NONE',  ( -1.322994767380000214, 1450.726806844560087, 182.2564604496979825 ) ) ;
#64343 = AXIS2_PLACEMENT_3D ( 'NONE', #64767, #23265, #41733 ) ;
#64344 = B_SPLINE_CURVE_WITH_KNOTS ( 'NONE', 5,
 ( #20998, #19346, #37282, #3702, #88237, #78728 ),
 .UNSPECIFIED., .F., .F.,
 ( 6, 6 ),
 ( 0.000000000000000000, 1.000000000000000000 ),
 .UNSPECIFIED. ) ;
#64345 = CARTESIAN_POINT ( 'NONE',  ( -23.02925477460000181, 1382.322973038800001, 221.4483044241590335 ) ) ;
#64346 = CARTESIAN_POINT ( 'NONE',  ( 3.626138226495970063, 1508.551704408389924, 204.4076455118720048 ) ) ;
#64348 = ORIENTED_EDGE ( 'NONE', *, *, #33855, .T. ) ;
#64347 = DIRECTION ( 'NONE',  ( -1.755985294532469921E-16, 1.000000000000000000, -1.338183447452831989E-16 ) ) ;
#64349 = CARTESIAN_POINT ( 'NONE',  ( 18.94655651209840030, 1455.761357035959918, 200.3458043486710380 ) ) ;
#64350 = EDGE_LOOP ( 'NONE', ( #51796, #33402, #62795, #30845, #110056 ) ) ;
#64351 = CARTESIAN_POINT ( 'NONE',  ( -11.13127190274779998, 1388.613762639859942, 216.5227499701169620 ) ) ;
#64352 = CARTESIAN_POINT ( 'NONE',  ( 32.97913964219430483, 1511.187213306747708, 197.9697544589745632 ) ) ;
#64353 = CARTESIAN_POINT ( 'NONE',  ( -9.519358626507830934, 1460.477013633640126, 210.7621351857700063 ) ) ;
#64354 = VECTOR ( 'NONE', #47318, 1000.000000000000114 ) ;
#64355 = CARTESIAN_POINT ( 'NONE',  ( 9.860940659611273418, 1504.635452453244170, 215.2684308639460937 ) ) ;
#64356 = DIRECTION ( 'NONE',  ( 0.3090169943749446757, -0.000000000000000000, -0.9510565162951544194 ) ) ;
#64357 = CARTESIAN_POINT ( 'NONE',  ( 20.06206385248925272, 1509.646645313393947, 187.2373516834030625 ) ) ;
#64358 = CARTESIAN_POINT ( 'NONE',  ( 13.15931087223109941, 1409.372593648980001, 202.0512334247140132 ) ) ;
#64359 = CARTESIAN_POINT ( 'NONE',  ( 4.449807483899999916, 1453.291438929989909, 213.9306864722589978 ) ) ;
#64360 = CARTESIAN_POINT ( 'NONE',  ( 3.410503593230000074, 1419.799443580629941, 185.4204322456980094 ) ) ;
#64361 = CYLINDRICAL_SURFACE ( 'NONE', #98005, 7.799999999999999822 ) ;
#64362 = FACE_OUTER_BOUND ( 'NONE', #71622, .T. ) ;
#64363 = CIRCLE ( 'NONE', #53666, 1.988474534702024066 ) ;
#64364 = CARTESIAN_POINT ( 'NONE',  ( 1.491506560153233352, 1512.187213306747481, 242.6732489767341576 ) ) ;
#64365 = ORIENTED_EDGE ( 'NONE', *, *, #72139, .T. ) ;
#64366 = ORIENTED_EDGE ( 'NONE', *, *, #46758, .F. ) ;
#64367 = CARTESIAN_POINT ( 'NONE',  ( 19.37774363895692886, 1525.878013734321712, 236.8539400710499194 ) ) ;
#64368 = CARTESIAN_POINT ( 'NONE',  ( -11.23669755706080053, 1415.007830323640064, 195.6839844364440069 ) ) ;
#64369 = CARTESIAN_POINT ( 'NONE',  ( -12.50048419760000051, 1435.331243516640143, 150.8675838421980018 ) ) ;
#64370 = CARTESIAN_POINT ( 'NONE',  ( 0.000000000000000000, 1518.913060387330006, 209.1218459616979999 ) ) ;
#64371 = CARTESIAN_POINT ( 'NONE',  ( -20.34485088181780199, 1499.600355960500110, 190.6291793570229913 ) ) ;
#64372 = CARTESIAN_POINT ( 'NONE',  ( -15.83970063559999808, 1420.111466363800218, 210.7068694924290071 ) ) ;
#64373 = CARTESIAN_POINT ( 'NONE',  ( -109.5779934659999952, 1386.007389322860035, 311.2464976022590122 ) ) ;
#64374 = CARTESIAN_POINT ( 'NONE',  ( -0.5583389695640000872, 1486.508398414630165, 181.8176688025980070 ) ) ;
#64375 = CARTESIAN_POINT ( 'NONE',  ( -10.73381386015609174, 1366.619851243301127, 210.6218459617030021 ) ) ;
#64376 = DIRECTION ( 'NONE',  ( 0.000000000000000000, 2.700129756073435379E-15, -1.000000000000000000 ) ) ;
#64377 = CARTESIAN_POINT ( 'NONE',  ( -13.10742788030691663, 1414.941152333605260, 220.2965691509508588 ) ) ;
#64378 = EDGE_CURVE ( 'NONE', #18252, #54175, #18538, .T. ) ;
#64379 = CARTESIAN_POINT ( 'NONE',  ( 6.546001350565000543, 1516.557392317769882, 207.4118413833070065 ) ) ;
#64380 = CARTESIAN_POINT ( 'NONE',  ( -9.004371644888150783, 1448.775058266490078, 210.7636302426640214 ) ) ;
#64381 = CIRCLE ( 'NONE', #16056, 1.999999999999998668 ) ;
#64382 = CARTESIAN_POINT ( 'NONE',  ( 6.232532001951379463, 1407.162969925759853, 220.5304192662420064 ) ) ;
#64383 = CARTESIAN_POINT ( 'NONE',  ( -13.20760688286200057, 1434.870232751160074, 149.1307101172629928 ) ) ;
#64384 = B_SPLINE_CURVE_WITH_KNOTS ( 'NONE', 3,
 ( #59541, #8561, #42733, #102602 ),
 .UNSPECIFIED., .F., .F.,
 ( 4, 4 ),
 ( 0.000000000000000000, 1.000000000000000000 ),
 .UNSPECIFIED. ) ;
#64385 = CARTESIAN_POINT ( 'NONE',  ( -8.579591590190000616, 1385.064761779769924, 218.6660937052890006 ) ) ;
#64386 = B_SPLINE_SURFACE_WITH_KNOTS ( 'NONE', 5, 5, ( 
 ( #93481, #42543, #94040, #17305, #9489, #43655 ),
 ( #45877, #80012, #64331, #62137, #11704, #4418 ),
 ( #63779, #29595, #37459, #96262, #3335, #19538 ),
 ( #21168, #71094, #53745, #98454, #12245, #12799 ),
 ( #21724, #96825, #55376, #55926, #97896, #97356 ),
 ( #27954, #20094, #20625, #46434, #105781, #90046 ) ),
 .UNSPECIFIED., .F., .F., .F.,
 ( 6, 6 ),
 ( 6, 6 ),
 ( 29.77037649420000065, 87.06999293180000166 ),
 ( 0.000000000000000000, 2.000000000000000000 ),
 .UNSPECIFIED. ) ;
#64387 = CARTESIAN_POINT ( 'NONE',  ( -13.58041510073769942, 1508.551704408389924, 210.3416170870220014 ) ) ;
#64388 = CARTESIAN_POINT ( 'NONE',  ( 7.063366770386080518, 1424.901426757719946, 213.0980514803050028 ) ) ;
#64389 = ORIENTED_EDGE ( 'NONE', *, *, #81012, .T. ) ;
#64390 = CARTESIAN_POINT ( 'NONE',  ( 36.92073955249999528, 1428.724883233329820, 259.2254644156980135 ) ) ;
#64392 = CARTESIAN_POINT ( 'NONE',  ( -16.40068023219999915, 1409.485784761229979, 195.3783929211979853 ) ) ;
#64391 = CARTESIAN_POINT ( 'NONE',  ( -0.5262109480990000421, 1494.207478666230145, 181.3805628087980040 ) ) ;
#64393 = CARTESIAN_POINT ( 'NONE',  ( 20.62320342492137470, 1506.569407720647177, 201.1880884098677029 ) ) ;
#64394 = CIRCLE ( 'NONE', #30406, 1.999999999999998668 ) ;
#64395 = CARTESIAN_POINT ( 'NONE',  ( -19.86631883729999970, 1428.969954335329930, 216.3509643007580223 ) ) ;
#64396 = CARTESIAN_POINT ( 'NONE',  ( 0.8430514960859990525, 1485.625134838489885, 221.0008352635990150 ) ) ;
#64397 = CARTESIAN_POINT ( 'NONE',  ( 20.05786438499999846, 1473.530630424389983, 207.1970391306990109 ) ) ;
#64398 = CARTESIAN_POINT ( 'NONE',  ( 30.24135515959999765, 1450.996674463330010, 136.2805541580979991 ) ) ;
#64399 = EDGE_LOOP ( 'NONE', ( #65660, #69780, #37277, #91761 ) ) ;
#64400 = CARTESIAN_POINT ( 'NONE',  ( -0.001991372178490000491, 1395.912990847029960, 197.8078701673980220 ) ) ;
#64401 = CARTESIAN_POINT ( 'NONE',  ( 14.32486855194574105, 1514.214507861885295, 225.6406290981485370 ) ) ;
#64402 = CARTESIAN_POINT ( 'NONE',  ( 2.946467845570000410, 1509.056494393530102, 238.8527705038980002 ) ) ;
#64403 = ORIENTED_EDGE ( 'NONE', *, *, #13025, .T. ) ;
#64404 = EDGE_LOOP ( 'NONE', ( #31515, #80277, #83928, #21945 ) ) ;
#64405 = CARTESIAN_POINT ( 'NONE',  ( -6.354406034210000165, 1384.502204350209922, 199.7451528500290010 ) ) ;
#64406 = CARTESIAN_POINT ( 'NONE',  ( -23.94289775954100108, 1410.422078863890192, 208.8148502979400121 ) ) ;
#64407 = VERTEX_POINT ( 'NONE', #95675 ) ;
#64408 = CARTESIAN_POINT ( 'NONE',  ( 4.491288147733260239, 1508.884219112060009, 205.6342589211700158 ) ) ;
#64409 = LINE ( 'NONE', #82833, #33080 ) ;
#64410 = CARTESIAN_POINT ( 'NONE',  ( -3.874466659299999893, 1479.770995650030045, 235.3786624194979709 ) ) ;
#64411 = CARTESIAN_POINT ( 'NONE',  ( -1.328200906410177184, 1420.347247853201225, 184.8989557469041074 ) ) ;
#64412 = EDGE_LOOP ( 'NONE', ( #78591, #20661, #12749, #99850 ) ) ;
#64413 = EDGE_CURVE ( 'NONE', #94821, #33676, #50768, .T. ) ;
#64414 = CARTESIAN_POINT ( 'NONE',  ( 46.05253185105119229, 1441.852346002359809, 266.6768988155079683 ) ) ;
#64415 = EDGE_CURVE ( 'NONE', #31992, #93336, #18467, .T. ) ;
#64416 = CARTESIAN_POINT ( 'NONE',  ( -11.41805403388689832, 1414.913057862230062, 220.8525437052670100 ) ) ;
#64417 = CARTESIAN_POINT ( 'NONE',  ( -7.098697224140000372, 1427.010778451219949, 204.8644842388889913 ) ) ;
#64418 = CARTESIAN_POINT ( 'NONE',  ( 6.550389432124999800, 1516.755758396839838, 204.1155163507169732 ) ) ;
#64419 = VERTEX_POINT ( 'NONE', #3852 ) ;
#64421 = EDGE_CURVE ( 'NONE', #108102, #82322, #29030, .T. ) ;
#64420 = CARTESIAN_POINT ( 'NONE',  ( 10.26924672323419863, 1481.505245612710041, 214.9441554700569839 ) ) ;
#64422 = AXIS2_PLACEMENT_3D ( 'NONE', #92448, #15722, #15186 ) ;
#64423 = CARTESIAN_POINT ( 'NONE',  ( 13.09408958547385460, 1443.019840760110583, 187.3616399427167494 ) ) ;
#64424 = ORIENTED_EDGE ( 'NONE', *, *, #33659, .T. ) ;
#64425 = ORIENTED_EDGE ( 'NONE', *, *, #47515, .T. ) ;
#64426 = CARTESIAN_POINT ( 'NONE',  ( -10.51530743187480077, 1480.028629462490017, 208.9546532503999856 ) ) ;
#64427 = EDGE_CURVE ( 'NONE', #104141, #19775, #89305, .T. ) ;
#64428 = DIRECTION ( 'NONE',  ( -0.7067700363771036720, 0.03085824620770448792, -0.7067700363771036720 ) ) ;
#64429 = CARTESIAN_POINT ( 'NONE',  ( 2.474966857995990033, 1497.110993154729840, 196.9665763241029879 ) ) ;
#64430 = EDGE_CURVE ( 'NONE', #81429, #4737, #96227, .T. ) ;
#64431 = CARTESIAN_POINT ( 'NONE',  ( -4.370116291996360758, 1424.878943209489535, 185.9531288255872425 ) ) ;
#64432 = CARTESIAN_POINT ( 'NONE',  ( 11.45277010228440062, 1452.513120842550052, 149.9488700328180073 ) ) ;
#64433 = AXIS2_PLACEMENT_3D ( 'NONE', #45130, #91519, #89312 ) ;
#64434 = CARTESIAN_POINT ( 'NONE',  ( 11.29707874440000026, 1420.194464914089849, 198.6147532060990102 ) ) ;
#64435 = CARTESIAN_POINT ( 'NONE',  ( 0.4820566092233740108, 1475.187528322450135, 220.5330728396190239 ) ) ;
#64436 = DIRECTION ( 'NONE',  ( 0.000000000000000000, 1.000000000000000000, 0.000000000000000000 ) ) ;
#64437 = FACE_OUTER_BOUND ( 'NONE', #26925, .T. ) ;
#64438 = DIRECTION ( 'NONE',  ( 1.000000000000000000, 0.000000000000000000, 0.000000000000000000 ) ) ;
#64440 = CARTESIAN_POINT ( 'NONE',  ( -106.4410097957560026, 1391.810857979010052, 306.8924406162939817 ) ) ;
#64439 = CARTESIAN_POINT ( 'NONE',  ( 29.53441971554831724, 1525.651286436460850, 196.5125197345233232 ) ) ;
#64441 = CARTESIAN_POINT ( 'NONE',  ( 11.78015744380379815, 1421.994974570560089, 207.2729246609449945 ) ) ;
#64442 = CARTESIAN_POINT ( 'NONE',  ( -9.600701647585090370, 1440.346316946680190, 206.2437467786620005 ) ) ;
#64443 = CARTESIAN_POINT ( 'NONE',  ( 11.30500403589999792, 1428.976642997429963, 112.4493539157979995 ) ) ;
#64444 = ORIENTED_EDGE ( 'NONE', *, *, #1488, .T. ) ;
#64445 = CARTESIAN_POINT ( 'NONE',  ( 10.05164999069999965, 1426.487183120430245, 224.8635561722979901 ) ) ;
#64446 = TOROIDAL_SURFACE ( 'NONE', #78730, 8.800000000000000711, 1.000000000000000000 ) ;
#64447 = CARTESIAN_POINT ( 'NONE',  ( -11.15489169059993735, 1425.160568487430055, 144.1681086605935604 ) ) ;
#64448 = CARTESIAN_POINT ( 'NONE',  ( -83.69811532344560590, 1384.984538349280001, 306.0467535211649874 ) ) ;
#64449 = CARTESIAN_POINT ( 'NONE',  ( -8.959619814139999860, 1385.213185382589927, 199.9358950396990053 ) ) ;
#64450 =( BOUNDED_CURVE ( )  B_SPLINE_CURVE ( 3, ( #43703, #10658, #9535, #37936 ),
 .UNSPECIFIED., .F., .F. ) 
 B_SPLINE_CURVE_WITH_KNOTS ( ( 4, 4 ),
 ( 5.447131716497383813, 6.315249268839017383 ),
 .UNSPECIFIED. ) 
 CURVE ( )  GEOMETRIC_REPRESENTATION_ITEM ( )  RATIONAL_B_SPLINE_CURVE ( ( 1.000000000000000000, 0.9381775213688714476, 0.9381775213688714476, 1.000000000000000000 ) ) 
 REPRESENTATION_ITEM ( '' )  );
#64451 = FACE_OUTER_BOUND ( 'NONE', #27796, .T. ) ;
#64452 = ADVANCED_FACE ( 'NONE', ( #105746 ), #67141, .F. ) ;
#64454 = VERTEX_POINT ( 'NONE', #21693 ) ;
#64453 = CARTESIAN_POINT ( 'NONE',  ( -17.30417025350569915, 1419.800952382169953, 207.6230020391829783 ) ) ;
#64455 = CARTESIAN_POINT ( 'NONE',  ( 3.947090874974254149, 1427.113278099589934, 137.0999999980980704 ) ) ;
#64456 = CARTESIAN_POINT ( 'NONE',  ( -2.560278795423229781, 1439.616515393840018, 157.6872015775370244 ) ) ;
#64457 = CARTESIAN_POINT ( 'NONE',  ( -14.45771163659999914, 1416.835808398129984, 221.3919539477980152 ) ) ;
#64458 = CARTESIAN_POINT ( 'NONE',  ( 11.93801661799999891, 1433.480575387579847, 150.0148646725980086 ) ) ;
#64459 = CARTESIAN_POINT ( 'NONE',  ( 12.85600963073500047, 1512.300546902530186, 224.3151201823670249 ) ) ;
#64460 = CARTESIAN_POINT ( 'NONE',  ( 13.15726448920050018, 1414.913060387399810, 198.3331475907570223 ) ) ;
#64461 = EDGE_CURVE ( 'NONE', #8198, #68958, #65327, .T. ) ;
#64462 = CARTESIAN_POINT ( 'NONE',  ( 4.163173984530029514, 1457.139433339820016, 199.2031175087780070 ) ) ;
#64463 = CARTESIAN_POINT ( 'NONE',  ( -110.0191722785379653, 1385.664243115142426, 296.9929505227199797 ) ) ;
#64464 = ADVANCED_FACE ( 'NONE', ( #41825 ), #42115, .F. ) ;
#64465 = CARTESIAN_POINT ( 'NONE',  ( 7.459553558550000574, 1422.095603715230027, 231.2386102329980133 ) ) ;
#64466 = DIRECTION ( 'NONE',  ( -1.755985294532469921E-16, 1.000000000000000000, -1.338183447452831989E-16 ) ) ;
#64467 = AXIS2_PLACEMENT_3D ( 'NONE', #110467, #93640, #85248 ) ;
#64468 = CARTESIAN_POINT ( 'NONE',  ( 2.864043418315000089, 1516.811292230880099, 206.8228319013669818 ) ) ;
#64469 = CARTESIAN_POINT ( 'NONE',  ( 3.512785867830420180E-12, 1395.913060387330006, 198.1220674046479928 ) ) ;
#64470 = CARTESIAN_POINT ( 'NONE',  ( -18.41342271589999768, 1409.720851141630192, 222.9148940093980116 ) ) ;
#64471 = CARTESIAN_POINT ( 'NONE',  ( 15.28398915819999893, 1435.448478077710206, 149.0740643685979876 ) ) ;
#64472 = EDGE_CURVE ( 'NONE', #92713, #61077, #31103, .T. ) ;
#64473 = CARTESIAN_POINT ( 'NONE',  ( -1.543830048049999792, 1424.182865445729703, 228.3475006505979934 ) ) ;
#64474 = CARTESIAN_POINT ( 'NONE',  ( 24.46211382750000141, 1438.319209241250064, 213.4123708239580139 ) ) ;
#64475 = CARTESIAN_POINT ( 'NONE',  ( 1.093792492990000031, 1515.225200552689785, 204.7965979425590035 ) ) ;
#64476 = CARTESIAN_POINT ( 'NONE',  ( -14.53046663459189958, 1417.356912740600137, 203.2574546587219970 ) ) ;
#64477 = CARTESIAN_POINT ( 'NONE',  ( -35.82176637796790430, 1436.379724471920099, 136.2603715204670038 ) ) ;
#64478 = CARTESIAN_POINT ( 'NONE',  ( 0.2097987188493439792, 1457.461435332639894, 183.0619989796059883 ) ) ;
#64479 = CARTESIAN_POINT ( 'NONE',  ( -8.191952444756632090, 1407.860267943719919, 219.8961961182280049 ) ) ;
#64480 = CARTESIAN_POINT ( 'NONE',  ( -17.17404474450000151, 1416.216596894529857, 202.8710369035879921 ) ) ;
#64481 = CIRCLE ( 'NONE', #17999, 2.000000000000011102 ) ;
#64482 = CARTESIAN_POINT ( 'NONE',  ( -4.327507137520000491, 1515.138941066290045, 208.4081369698370167 ) ) ;
#64483 = CARTESIAN_POINT ( 'NONE',  ( -28.11107467879419985, 1509.207378190189957, 210.7860757214999978 ) ) ;
#64484 = CARTESIAN_POINT ( 'NONE',  ( 12.06130614719999983, 1433.903343712190235, 147.2729309238979738 ) ) ;
#64485 = CARTESIAN_POINT ( 'NONE',  ( -27.69670551879999820, 1435.466977414309895, 135.6947802121979976 ) ) ;
#64486 = CARTESIAN_POINT ( 'NONE',  ( 8.631780704876279131, 1438.018275767699834, 210.0183142686710198 ) ) ;
#64487 = EDGE_LOOP ( 'NONE', ( #89155, #29253, #43054, #95940 ) ) ;
#64488 = CARTESIAN_POINT ( 'NONE',  ( 2.564256839410000488, 1486.020400378790100, 198.5121203060990354 ) ) ;
#64489 = CARTESIAN_POINT ( 'NONE',  ( 5.270386862360000535, 1477.861965715389942, 199.8733389948390027 ) ) ;
#64490 = CARTESIAN_POINT ( 'NONE',  ( -4.508178739127020940, 1409.070489457920075, 223.4101744795629827 ) ) ;
#64491 = CARTESIAN_POINT ( 'NONE',  ( -11.73701470839999850, 1491.048748728590226, 207.6304560743390084 ) ) ;
#64492 = CARTESIAN_POINT ( 'NONE',  ( -17.00797328670000397, 1417.537217351680056, 207.7155449971589860 ) ) ;
#64493 = CARTESIAN_POINT ( 'NONE',  ( 14.64585795956600123, 1509.424984143169922, 234.5789104686880080 ) ) ;
#64494 = CARTESIAN_POINT ( 'NONE',  ( 5.730844508220573452, 1406.977338306732236, 269.6419569788193940 ) ) ;
#64495 = CARTESIAN_POINT ( 'NONE',  ( 20.51078616439999891, 1453.154034703029993, 210.6541330983779972 ) ) ;
#64496 = CARTESIAN_POINT ( 'NONE',  ( -12.32169722289999925, 1378.992744615490210, 209.8847561567199875 ) ) ;
#64497 = CARTESIAN_POINT ( 'NONE',  ( -84.84750775523609434, 1384.628878466070091, 306.6159466445730004 ) ) ;
#64498 = CARTESIAN_POINT ( 'NONE',  ( -60.37232013571600220, 1385.063171825080190, 244.7907910518410119 ) ) ;
#64499 = CARTESIAN_POINT ( 'NONE',  ( -12.23489732466240021, 1490.237667237379810, 209.6383001084460034 ) ) ;
#64500 = CARTESIAN_POINT ( 'NONE',  ( -4.969384015369690211, 1508.551704408389924, 206.3370868630439929 ) ) ;
#64501 = CARTESIAN_POINT ( 'NONE',  ( -29.34423976567429904, 1509.844966209650011, 208.6282038019159870 ) ) ;
#64503 = VERTEX_POINT ( 'NONE', #33238 ) ;
#64502 = CARTESIAN_POINT ( 'NONE',  ( 0.5007497712181619987, 1414.173381217940005, 184.9066978159829944 ) ) ;
#64504 = DIRECTION ( 'NONE',  ( -0.1837295255851838782, -0.06561766200247082237, -0.9807842697869766369 ) ) ;
#64505 = CARTESIAN_POINT ( 'NONE',  ( 10.02631634006560191, 1469.909548164330090, 210.1023831811019988 ) ) ;
#64506 = CARTESIAN_POINT ( 'NONE',  ( -0.4151546846821903003, 1512.187213306747481, 173.3106345060153046 ) ) ;
#64507 = CARTESIAN_POINT ( 'NONE',  ( -0.1120303467899630145, 1420.419502555939744, 183.1208681730079775 ) ) ;
#64508 = AXIS2_PLACEMENT_3D ( 'NONE', #103437, #26743, #3236 ) ;
#64509 = CARTESIAN_POINT ( 'NONE',  ( 5.864566082395450408, 1517.151704408390060, 226.1537825710409777 ) ) ;
#64510 = CARTESIAN_POINT ( 'NONE',  ( 22.21106947969999723, 1410.183783044429902, 215.0444402526979957 ) ) ;
#64511 = B_SPLINE_SURFACE_WITH_KNOTS ( 'NONE', 4, 5, ( 
 ( #80196, #29239, #28693, #86380, #70183, #3514 ),
 ( #27580, #52254, #1290, #37638, #18602, #62323 ),
 ( #45520, #95891, #2418, #37083, #62897, #10793 ),
 ( #52802, #71287, #53358, #71843, #36535, #95341 ),
 ( #86933, #70732, #105400, #44963, #19727, #97007 ) ),
 .UNSPECIFIED., .F., .F., .F.,
 ( 5, 5 ),
 ( 6, 6 ),
 ( 13.35596682890000153, 21.06373553689999767 ),
 ( 0.000000000000000000, 2.000000835909999886 ),
 .UNSPECIFIED. ) ;
#64512 = DIRECTION ( 'NONE',  ( -1.986951185180850528E-13, 0.03085824620771311644, 0.9995237709234254808 ) ) ;
#64513 = CARTESIAN_POINT ( 'NONE',  ( -19.61848387020800288, 1466.208095908119958, 204.1942870921240001 ) ) ;
#64514 = CARTESIAN_POINT ( 'NONE',  ( -16.46007637289999792, 1423.318218959529986, 228.6067745784980048 ) ) ;
#64516 = CARTESIAN_POINT ( 'NONE',  ( -11.63691600037451401, 1426.763110590993392, 137.0152515069076742 ) ) ;
#64515 = CARTESIAN_POINT ( 'NONE',  ( -2.941312998452541905, 1512.218159651617725, 201.2357107834446026 ) ) ;
#64517 = CARTESIAN_POINT ( 'NONE',  ( 25.47490434202370224, 1449.924909233149947, 207.9936631072650073 ) ) ;
#64518 = CARTESIAN_POINT ( 'NONE',  ( -100.5161172128999993, 1371.894749952190068, 304.2218459572590064 ) ) ;
#64519 = DIRECTION ( 'NONE',  ( 0.000000000000000000, 0.000000000000000000, 1.000000000000000000 ) ) ;
#64520 = CARTESIAN_POINT ( 'NONE',  ( -0.4667865956230000668, 1416.135524792730166, 233.5066666412979828 ) ) ;
#64521 = CARTESIAN_POINT ( 'NONE',  ( -7.173827098680000347, 1361.757975858879945, 210.6218459616991936 ) ) ;
#64522 = EDGE_CURVE ( 'NONE', #45555, #94338, #102088, .T. ) ;
#64523 = CARTESIAN_POINT ( 'NONE',  ( 3.253462060665000433, 1516.874084700499907, 205.6604858388269861 ) ) ;
#64524 = CARTESIAN_POINT ( 'NONE',  ( -4.527446633101839701, 1485.996829922820098, 182.3396792648729843 ) ) ;
#64525 = VERTEX_POINT ( 'NONE', #88631 ) ;
#64526 = AXIS2_PLACEMENT_3D ( 'NONE', #20787, #28103, #96421 ) ;
#64527 = CARTESIAN_POINT ( 'NONE',  ( -4.523944140811339665, 1455.378620635879997, 200.8408219016489795 ) ) ;
#64528 = CARTESIAN_POINT ( 'NONE',  ( -4.262072192076889365, 1441.213750638199826, 159.1103247205799960 ) ) ;
#64530 = ORIENTED_EDGE ( 'NONE', *, *, #52921, .F. ) ;
#64529 = CARTESIAN_POINT ( 'NONE',  ( -68.38904811079750345, 1379.747152134330008, 279.9588836171899970 ) ) ;
#64531 = ORIENTED_EDGE ( 'NONE', *, *, #61831, .T. ) ;
#64532 = CARTESIAN_POINT ( 'NONE',  ( 3.829619994797929916, 1515.551704292389786, 207.2788821832570250 ) ) ;
#64533 = VERTEX_POINT ( 'NONE', #12451 ) ;
#64534 = CARTESIAN_POINT ( 'NONE',  ( 2.707841495209149851, 1485.005101276989990, 220.6627816910599904 ) ) ;
#64535 = CARTESIAN_POINT ( 'NONE',  ( 11.55794785089999976, 1501.267050509989986, 208.2533511322130266 ) ) ;
#64537 = FACE_OUTER_BOUND ( 'NONE', #80076, .T. ) ;
#64536 = CARTESIAN_POINT ( 'NONE',  ( 15.80295874793040056, 1414.899199519979902, 191.3919695463190180 ) ) ;
#64538 = CARTESIAN_POINT ( 'NONE',  ( 4.044319887224999910, 1517.073005577650065, 210.2423896678870108 ) ) ;
#64539 = EDGE_CURVE ( 'NONE', #104987, #105027, #32848, .T. ) ;
#64540 = CARTESIAN_POINT ( 'NONE',  ( -25.34177650560360107, 1450.805395652589823, 137.4212134988369769 ) ) ;
#64541 = CARTESIAN_POINT ( 'NONE',  ( -11.43740528939999912, 1425.481182534629852, 144.1672625331979987 ) ) ;
#64542 = CARTESIAN_POINT ( 'NONE',  ( 11.07372907340000090, 1410.233410434930192, 229.3828206623979895 ) ) ;
#64543 = CARTESIAN_POINT ( 'NONE',  ( 8.680203951845038901, 1482.515033173300026, 217.3319919233640007 ) ) ;
#64544 = DIRECTION ( 'NONE',  ( 1.000000000000000000, 0.000000000000000000, 0.000000000000000000 ) ) ;
#64545 = CARTESIAN_POINT ( 'NONE',  ( 39.18506236152150279, 1437.902641089279996, 134.0999999975959724 ) ) ;
#64546 = VECTOR ( 'NONE', #10089, 1000.000000000000000 ) ;
#64547 = CARTESIAN_POINT ( 'NONE',  ( -31.23437356469455040, 1518.913060387330006, 195.3468678195118287 ) ) ;
#64548 = VERTEX_POINT ( 'NONE', #63449 ) ;
#64549 = CARTESIAN_POINT ( 'NONE',  ( 14.43150070665419982, 1435.522629004720102, 149.5715662318340264 ) ) ;
#64550 = ORIENTED_EDGE ( 'NONE', *, *, #79417, .F. ) ;
#64551 = ORIENTED_EDGE ( 'NONE', *, *, #91819, .T. ) ;
#64552 = CARTESIAN_POINT ( 'NONE',  ( -6.490306558154999905, 1514.605246816799763, 217.1492952416969899 ) ) ;
#64553 = CARTESIAN_POINT ( 'NONE',  ( 5.031477915346656005, 1455.301335138442937, 217.6180370876550114 ) ) ;
#64554 = VECTOR ( 'NONE', #88796, 1000.000000000000000 ) ;
#64555 = CARTESIAN_POINT ( 'NONE',  ( 0.05443591761330000139, 1451.171040272929758, 182.5324322684980132 ) ) ;
#64556 = B_SPLINE_CURVE_WITH_KNOTS ( 'NONE', 5,
 ( #77126, #86608, #9358, #102838, #92801, #42967 ),
 .UNSPECIFIED., .F., .F.,
 ( 6, 6 ),
 ( -157.9969979290000026, -29.50720980500000223 ),
 .UNSPECIFIED. ) ;
#64557 = CARTESIAN_POINT ( 'NONE',  ( -3.380492229449999719, 1485.523073118029970, 182.9528005117980172 ) ) ;
#64558 = CARTESIAN_POINT ( 'NONE',  ( -3.487585887316744238, 1508.611350403811230, 204.4436907818935367 ) ) ;
#64559 = CARTESIAN_POINT ( 'NONE',  ( -68.80955101979490962, 1379.748017775673134, 280.2796398541619851 ) ) ;
#64560 = CARTESIAN_POINT ( 'NONE',  ( 5399.190729149044273, 50.28429875041807406, -8134.791976860689829 ) ) ;
#64561 = EDGE_CURVE ( 'NONE', #65361, #97932, #61507, .T. ) ;
#64562 = CARTESIAN_POINT ( 'NONE',  ( 27.78452742954910093, 1508.000976259739900, 207.7754991261529938 ) ) ;
#64563 = CARTESIAN_POINT ( 'NONE',  ( 8.403208615350001409, 1415.931391677429929, 193.2488689964980040 ) ) ;
#64564 = CARTESIAN_POINT ( 'NONE',  ( -61.65199887796450895, 1384.683307422990083, 247.6074881643829997 ) ) ;
#64565 = ORIENTED_EDGE ( 'NONE', *, *, #34974, .F. ) ;
#64566 = CARTESIAN_POINT ( 'NONE',  ( -1.085894894499999928E-15, 1432.353341358199941, 150.3995506339979897 ) ) ;
#64567 = CARTESIAN_POINT ( 'NONE',  ( -1.133653179125000188, 1516.978425811520083, 208.3843950493249793 ) ) ;
#64568 = VERTEX_POINT ( 'NONE', #95912 ) ;
#64569 = CARTESIAN_POINT ( 'NONE',  ( 40.43917225116809533, 1440.913060387330006, 267.8759699188719878 ) ) ;
#64570 = AXIS2_PLACEMENT_3D ( 'NONE', #103113, #26414, #70128 ) ;
#64571 = CARTESIAN_POINT ( 'NONE',  ( -0.0008084625836226779893, 1451.918325721145493, 154.0009410478433551 ) ) ;
#64572 = ADVANCED_FACE ( 'NONE', ( #61790 ), #85008, .F. ) ;
#64573 = ORIENTED_EDGE ( 'NONE', *, *, #62424, .T. ) ;
#64574 = CARTESIAN_POINT ( 'NONE',  ( -0.05864779970183610358, 1450.911012361030089, 181.2397301690949973 ) ) ;
#64575 = CARTESIAN_POINT ( 'NONE',  ( 7.934673110537849183, 1428.710417030969893, 214.3182389180220184 ) ) ;
#64576 = FACE_OUTER_BOUND ( 'NONE', #69158, .T. ) ;
#64577 = CARTESIAN_POINT ( 'NONE',  ( -9.638453515383760717, 1462.007706823630087, 206.9654734332999908 ) ) ;
#64578 = CARTESIAN_POINT ( 'NONE',  ( 22.49732387063940209, 1410.763224758360138, 206.2063201444890126 ) ) ;
#64579 = CARTESIAN_POINT ( 'NONE',  ( -5.424122872404329776, 1511.219705715099963, 201.2551218106839883 ) ) ;
#64580 = CARTESIAN_POINT ( 'NONE',  ( 9.884505093230000483, 1406.768685218130031, 266.9235441556980390 ) ) ;
#64581 = DIRECTION ( 'NONE',  ( 0.5369043659965772042, -0.4884709562386981840, -0.6878443331779838799 ) ) ;
#64582 = CARTESIAN_POINT ( 'NONE',  ( -22.52214966618224778, 1524.244163922423695, 181.7424121231434810 ) ) ;
#64583 = EDGE_CURVE ( 'NONE', #94550, #80209, #54401, .T. ) ;
#64585 = CARTESIAN_POINT ( 'NONE',  ( 0.000000000000000000, 1508.913060387330006, 224.7618459619980058 ) ) ;
#64584 = CARTESIAN_POINT ( 'NONE',  ( 16.95715696330000100, 1458.910017354530055, 229.2965042560980180 ) ) ;
#64586 = CARTESIAN_POINT ( 'NONE',  ( -6.553524415734999664, 1516.882690742909972, 216.0660777183969969 ) ) ;
#64587 = EDGE_CURVE ( 'NONE', #66446, #36071, #6086, .T. ) ;
#64588 = CARTESIAN_POINT ( 'NONE',  ( -8.716383294119999903, 1450.962816624490188, 203.1307156043189934 ) ) ;
#64589 = CARTESIAN_POINT ( 'NONE',  ( -0.1525074781070819840, 1507.411687413830123, 180.8672947283149881 ) ) ;
#64590 = CARTESIAN_POINT ( 'NONE',  ( 15.11448291366340158, 1451.479646069887622, 221.5393396382719970 ) ) ;
#64591 = CARTESIAN_POINT ( 'NONE',  ( -4.028630622785000170, 1516.812923327049930, 212.5819478221170016 ) ) ;
#64592 = CARTESIAN_POINT ( 'NONE',  ( 4.077242828495350579, 1515.224507406410112, 212.7046838410809926 ) ) ;
#64593 = CARTESIAN_POINT ( 'NONE',  ( 5.923682464646780943, 1522.051704408389924, 194.3813127491490036 ) ) ;
#64595 = VERTEX_POINT ( 'NONE', #80217 ) ;
#64594 = CARTESIAN_POINT ( 'NONE',  ( -109.9987473180000137, 1385.244513981200043, 297.1847073398589600 ) ) ;
#64596 = CARTESIAN_POINT ( 'NONE',  ( -19.28393528680000202, 1507.737928445829994, 229.5896611176980002 ) ) ;
#64597 = CARTESIAN_POINT ( 'NONE',  ( 3.672212372280000192, 1459.726867865030044, 213.1264975034980296 ) ) ;
#64598 = CARTESIAN_POINT ( 'NONE',  ( -11.76451447100000003, 1431.952785265209968, 150.8015324768979895 ) ) ;
#64599 = CARTESIAN_POINT ( 'NONE',  ( -14.67677013559999999, 1415.730435299999954, 205.0458841098590028 ) ) ;
#64600 = CARTESIAN_POINT ( 'NONE',  ( -109.7277482404900013, 1383.460710247889892, 311.2865699025030040 ) ) ;
#64601 = CARTESIAN_POINT ( 'NONE',  ( -0.3285102747869809714, 1508.336848181169898, 237.7487632055650124 ) ) ;
#64602 = EDGE_CURVE ( 'NONE', #22249, #65067, #7777, .T. ) ;
#64603 = CARTESIAN_POINT ( 'NONE',  ( -4.173142725735850433, 1447.222512570230037, 213.8729899181259952 ) ) ;
#64605 = CARTESIAN_POINT ( 'NONE',  ( 5.360003288404429966, 1422.228637084189813, 144.9391265021819777 ) ) ;
#64604 = CARTESIAN_POINT ( 'NONE',  ( -23.82798562378626883, 1411.105473243607321, 207.5387497735277407 ) ) ;
#64606 = CARTESIAN_POINT ( 'NONE',  ( 0.2612701249639999834, 1416.813004075630033, 190.7776225037979714 ) ) ;
#64607 = ORIENTED_EDGE ( 'NONE', *, *, #110208, .F. ) ;
#64608 = CARTESIAN_POINT ( 'NONE',  ( 6.935457925184999262, 1516.627618683580067, 205.6664679548470076 ) ) ;
#64609 = CARTESIAN_POINT ( 'NONE',  ( 3.441247510289999756, 1405.871390642129882, 268.4787024712979928 ) ) ;
#64610 = ADVANCED_FACE ( 'NONE', ( #97028 ), #28712, .F. ) ;
#64611 = CARTESIAN_POINT ( 'NONE',  ( 32.02808312589916540, 1512.187213306747481, 196.2787714533495489 ) ) ;
#64612 = FACE_OUTER_BOUND ( 'NONE', #91397, .T. ) ;
#64613 = CARTESIAN_POINT ( 'NONE',  ( 21.32599293744084434, 1428.684983583262920, 219.2409462215593408 ) ) ;
#64614 = CARTESIAN_POINT ( 'NONE',  ( 4.989246313819999834, 1471.909539260290103, 189.7082128665990126 ) ) ;
#64615 = CARTESIAN_POINT ( 'NONE',  ( 11.60004869885203682, 1423.462011167306855, 135.7646888042274327 ) ) ;
#64616 = CARTESIAN_POINT ( 'NONE',  ( 5.371346801041280372, 1516.551188146539971, 199.4837300725229738 ) ) ;
#64617 = CARTESIAN_POINT ( 'NONE',  ( -0.5697989932908550381, 1450.893162568030220, 155.3351454289200149 ) ) ;
#64618 = CARTESIAN_POINT ( 'NONE',  ( -1.726873275417834197, 1450.480600349099859, 182.9637712753274457 ) ) ;
#64619 = CARTESIAN_POINT ( 'NONE',  ( 1.179291408672469732, 1450.813351935780020, 155.3354828870230051 ) ) ;
#64620 = CARTESIAN_POINT ( 'NONE',  ( -14.27868134598659999, 1415.948038442679945, 221.2079983884039791 ) ) ;
#64621 = DIRECTION ( 'NONE',  ( -0.000000000000000000, -1.000000000000000000, -0.000000000000000000 ) ) ;
#64622 = CARTESIAN_POINT ( 'NONE',  ( -20.63825566599999917, 1425.387366209430184, 248.0989693021979861 ) ) ;
#64623 = CARTESIAN_POINT ( 'NONE',  ( -27.05015830627079865, 1507.998384514670079, 211.3652037525360186 ) ) ;
#64624 = CARTESIAN_POINT ( 'NONE',  ( 3.143814751020000298, 1440.618483647659787, 155.9530253030979736 ) ) ;
#64625 = AXIS2_PLACEMENT_3D ( 'NONE', #32773, #66957, #42841 ) ;
#64626 = CARTESIAN_POINT ( 'NONE',  ( -2.107599154099999872, 1475.947830574629961, 267.2331464721979728 ) ) ;
#64627 = PLANE ( 'NONE',  #6782 ) ;
#64628 = CARTESIAN_POINT ( 'NONE',  ( -17.67071593990000267, 1412.982943450030007, 193.3745006087980016 ) ) ;
#64629 = CARTESIAN_POINT ( 'NONE',  ( 17.60549899623140035, 1410.870509167670207, 224.1774152648420113 ) ) ;
#64630 = CARTESIAN_POINT ( 'NONE',  ( -41.84381950253869320, 1384.779123927429964, 245.4572242766560066 ) ) ;
#64631 = CARTESIAN_POINT ( 'NONE',  ( 7.105427357599999217E-15, 1420.413060387330006, 188.2701767054980166 ) ) ;
#64632 = CARTESIAN_POINT ( 'NONE',  ( 17.01536232022260009, 1507.593738162509908, 193.7118019646590028 ) ) ;
#64633 = CARTESIAN_POINT ( 'NONE',  ( 12.06965614970759937, 1491.404045832239945, 206.8238433162970011 ) ) ;
#64634 = CARTESIAN_POINT ( 'NONE',  ( 31.80537271888414352, 1525.137881624894817, 216.1511922624794693 ) ) ;
#64635 = CARTESIAN_POINT ( 'NONE',  ( 7.953529549975883128, 1511.798530722474197, 205.9061371885316021 ) ) ;
#64636 = CARTESIAN_POINT ( 'NONE',  ( -8.579552460874170450, 1396.212664961330120, 216.0972139694970338 ) ) ;
#64637 = AXIS2_PLACEMENT_3D ( 'NONE', #75859, #31637, #99935 ) ;
#64638 = CARTESIAN_POINT ( 'NONE',  ( -14.60687332829999896, 1422.240656693330038, 229.1148143803980020 ) ) ;
#64639 = CARTESIAN_POINT ( 'NONE',  ( -45.59060096559999664, 1439.350741641819923, 268.9760078171979671 ) ) ;
#64640 = ORIENTED_EDGE ( 'NONE', *, *, #42540, .F. ) ;
#64641 = CARTESIAN_POINT ( 'NONE',  ( -9.758366233290264091, 1410.624983480943683, 229.7348544036108535 ) ) ;
#64642 = CARTESIAN_POINT ( 'NONE',  ( -13.59512407998240135, 1507.703338069740084, 209.3532897553030239 ) ) ;
#64643 = DIRECTION ( 'NONE',  ( 0.000000000000000000, 0.000000000000000000, -1.000000000000000000 ) ) ;
#64644 = AXIS2_PLACEMENT_3D ( 'NONE', #4421, #73267, #48071 ) ;
#64646 = CARTESIAN_POINT ( 'NONE',  ( -13.06501233546500096, 1513.192861445620110, 192.2233964041670049 ) ) ;
#64645 = CARTESIAN_POINT ( 'NONE',  ( 10.30253573629999941, 1425.145685828329988, 112.6579331979979912 ) ) ;
#64647 = B_SPLINE_CURVE_WITH_KNOTS ( 'NONE', 3,
 ( #84030, #74553, #32539, #14620 ),
 .UNSPECIFIED., .F., .F.,
 ( 4, 4 ),
 ( 0.000000000000000000, 1.000000000000000000 ),
 .UNSPECIFIED. ) ;
#64648 = CARTESIAN_POINT ( 'NONE',  ( -16.17746047354429351, 1409.477984536645408, 225.0323634634132759 ) ) ;
#64649 = DIRECTION ( 'NONE',  ( 0.9125304618754024322, 0.000000000000000000, 0.4090087482554191078 ) ) ;
#64650 = ADVANCED_FACE ( 'NONE', ( #10815 ), #51071, .T. ) ;
#64651 = CARTESIAN_POINT ( 'NONE',  ( -3.455378015385000001, 1516.627618683580067, 202.1863880069169852 ) ) ;
#64652 = CARTESIAN_POINT ( 'NONE',  ( 11.44311708778599979, 1501.817457278790016, 208.4257042484660190 ) ) ;
#64653 = CARTESIAN_POINT ( 'NONE',  ( 13.52268460260000005, 1497.923627545689897, 227.8730058995990078 ) ) ;
#64654 = CARTESIAN_POINT ( 'NONE',  ( -3.617573937782270210, 1497.333809982809953, 198.4503636364750037 ) ) ;
#64655 = FACE_BOUND ( 'NONE', #51443, .T. ) ;
#64656 = CARTESIAN_POINT ( 'NONE',  ( -87.43044411833730578, 1379.577971547200150, 299.9734229985630236 ) ) ;
#64657 = AXIS2_PLACEMENT_3D ( 'NONE', #11016, #61997, #12665 ) ;
#64658 = CARTESIAN_POINT ( 'NONE',  ( 4.092070562564425806, 1367.124094438674774, 208.3718459617061285 ) ) ;
#64659 = B_SPLINE_CURVE_WITH_KNOTS ( 'NONE', 3,
 ( #13913, #48098, #66020, #26740, #67669, #60362, #60928, #77165, #102336, #25621, #84447, #33468, #8822, #59813, #94484, #17756, #41352, #93933, #43007, #41894, #35143, #59269, #102877, #26175, #7194, #50320, #95058, #110195, #76597, #76051, #51959, #67118, #101219, #86101 ),
 .UNSPECIFIED., .F., .F.,
 ( 4, 3, 3, 3, 3, 3, 3, 3, 3, 3, 3, 4 ),
 ( -13.43342673250000097, -12.68470386051800070, -11.93598098853600042, -11.14531161610780075, -10.30911549555539963, -9.267678416573820854, -8.124443764497049969, -7.336535162872540816, -6.414797305390919746, -5.580366644398009335, -4.830730724985089708, -4.119224442280000176 ),
 .UNSPECIFIED. ) ;
#64661 = VERTEX_POINT ( 'NONE', #19748 ) ;
#64660 = CARTESIAN_POINT ( 'NONE',  ( 9.247631459069999948, 1454.170661380389902, 214.4254682548290134 ) ) ;
#64662 = VERTEX_POINT ( 'NONE', #53948 ) ;
#64663 = CARTESIAN_POINT ( 'NONE',  ( -9.041387868970000241, 1396.228792609030052, 202.1530002182580006 ) ) ;
#64664 = CARTESIAN_POINT ( 'NONE',  ( -21.45557649069999684, 1410.156571378229728, 216.3485480334879867 ) ) ;
#64665 = CARTESIAN_POINT ( 'NONE',  ( -1.237038659479999803, 1415.048591087029763, 226.6890547777979918 ) ) ;
#64666 = CARTESIAN_POINT ( 'NONE',  ( -13.50348581488808364, 1444.084003877494069, 169.3539515139137279 ) ) ;
#64667 = CARTESIAN_POINT ( 'NONE',  ( -113.4000000000000057, 1305.913060387289988, 304.2218459572590064 ) ) ;
#64668 = CARTESIAN_POINT ( 'NONE',  ( 2.329898843065079994, 1515.219291385629958, 204.7964424078519983 ) ) ;
#64670 = CARTESIAN_POINT ( 'NONE',  ( 16.83667419020000011, 1416.263768433330142, 226.6570821373980209 ) ) ;
#64669 = FACE_OUTER_BOUND ( 'NONE', #73042, .T. ) ;
#64671 = ADVANCED_FACE ( 'NONE', ( #31126 ), #22698, .T. ) ;
#64672 = CARTESIAN_POINT ( 'NONE',  ( 2.709355696829999882, 1410.303802397230129, 185.6373498539979892 ) ) ;
#64673 = CARTESIAN_POINT ( 'NONE',  ( -5.077909815922139636, 1463.916899788050159, 200.2638641301039968 ) ) ;
#64674 = CARTESIAN_POINT ( 'NONE',  ( -40.08938852926480223, 1445.470329989359925, 136.8855892427959873 ) ) ;
#64675 =( LENGTH_UNIT ( ) NAMED_UNIT ( * ) SI_UNIT ( .MILLI., .METRE. ) );
#64676 = CARTESIAN_POINT ( 'NONE',  ( 7.298542379600410079, 1396.167931181390031, 200.8262254698040010 ) ) ;
#64677 = CARTESIAN_POINT ( 'NONE',  ( -28.02579834269999992, 1443.109842421779831, 137.4877371060980238 ) ) ;
#64678 = CARTESIAN_POINT ( 'NONE',  ( 11.76733812390000011, 1426.911783682829991, 146.2965758568979879 ) ) ;
#64679 = CARTESIAN_POINT ( 'NONE',  ( 7.597790773094999395, 1511.735270473989885, 202.7837360344269939 ) ) ;
#64680 = ORIENTED_EDGE ( 'NONE', *, *, #72762, .F. ) ;
#64681 = CARTESIAN_POINT ( 'NONE',  ( 4.408900587259999782, 1425.824676780029904, 185.4670178510979781 ) ) ;
#64682 = CARTESIAN_POINT ( 'NONE',  ( 2.499999996433849070, 1449.068978386697381, 182.3376700388170661 ) ) ;
#64683 = ORIENTED_EDGE ( 'NONE', *, *, #48105, .T. ) ;
#64684 = ORIENTED_EDGE ( 'NONE', *, *, #63780, .T. ) ;
#64685 = CARTESIAN_POINT ( 'NONE',  ( -18.20796897385059765, 1458.243120258429826, 227.9056602949669923 ) ) ;
#64686 = CARTESIAN_POINT ( 'NONE',  ( -15.16833389349999983, 1459.965360397030054, 229.4811956966979949 ) ) ;
#64687 = CARTESIAN_POINT ( 'NONE',  ( -6.232532106187401055, 1407.162969929529936, 197.7132727037109987 ) ) ;
#64688 = DIRECTION ( 'NONE',  ( -1.000000000000000000, -1.947392753017155135E-14, -3.090046365888145414E-15 ) ) ;
#64689 = CARTESIAN_POINT ( 'NONE',  ( -7.328049318385000177, 1516.809497469189864, 215.6772390872569929 ) ) ;
#64690 = CARTESIAN_POINT ( 'NONE',  ( -12.33449316102499971, 1378.995504077259966, 209.6450772243929919 ) ) ;
#64691 = ORIENTED_EDGE ( 'NONE', *, *, #107012, .T. ) ;
#64692 = CARTESIAN_POINT ( 'NONE',  ( -17.69166861870969853, 1508.551704428830135, 211.7662683139330113 ) ) ;
#64693 = CARTESIAN_POINT ( 'NONE',  ( -8.914143057620970367, 1509.305272612319868, 180.3769903018060177 ) ) ;
#64694 = CARTESIAN_POINT ( 'NONE',  ( -59.28197579180000076, 1379.588121118040135, 258.5658342392590043 ) ) ;
#64695 = B_SPLINE_CURVE_WITH_KNOTS ( 'NONE', 5,
 ( #96124, #88282, #69852, #9910, #53040, #79890 ),
 .UNSPECIFIED., .F., .F.,
 ( 6, 6 ),
 ( 0.000000000000000000, 1.000000000000000000 ),
 .UNSPECIFIED. ) ;
#64696 = CARTESIAN_POINT ( 'NONE',  ( 0.1955981716400000125, 1414.913060387329779, 225.1861338294980044 ) ) ;
#64697 = CARTESIAN_POINT ( 'NONE',  ( 1.120543697654999837, 1517.073005577650065, 205.0775260448770041 ) ) ;
#64698 = VERTEX_POINT ( 'NONE', #107287 ) ;
#64699 = CARTESIAN_POINT ( 'NONE',  ( -2.873919040654999701, 1516.940252185109784, 209.1351185066319829 ) ) ;
#64700 = CARTESIAN_POINT ( 'NONE',  ( -9.090368357078379091, 1450.929620059189801, 207.4549948248679812 ) ) ;
#64701 = EDGE_CURVE ( 'NONE', #20783, #17997, #47189, .T. ) ;
#64702 = CARTESIAN_POINT ( 'NONE',  ( -29.83607553919204491, 1419.456892885304342, 269.4690664095026591 ) ) ;
#64703 = CARTESIAN_POINT ( 'NONE',  ( 6.098897513495000311, 1511.444830760690138, 216.7818499078069863 ) ) ;
#64704 = EDGE_CURVE ( 'NONE', #20210, #37975, #57981, .T. ) ;
#64706 = ORIENTED_EDGE ( 'NONE', *, *, #59060, .F. ) ;
#64705 = CARTESIAN_POINT ( 'NONE',  ( 2.225547318884175230, 1525.712830164893376, 176.6706926612863811 ) ) ;
#64707 = CARTESIAN_POINT ( 'NONE',  ( 2.500000000000000000, 1430.041878304429929, 157.3252622477980083 ) ) ;
#64708 = CARTESIAN_POINT ( 'NONE',  ( -35.83479613928479779, 1440.913060387619907, 252.5442945837890250 ) ) ;
#64709 = CARTESIAN_POINT ( 'NONE',  ( -43.09053402079999984, 1384.454438790149879, 247.5006848784589977 ) ) ;
#64710 = CARTESIAN_POINT ( 'NONE',  ( -0.1917209389985229939, 1466.035524394150116, 235.8475842902419970 ) ) ;
#64711 = EDGE_CURVE ( 'NONE', #88321, #65245, #85320, .T. ) ;
#64712 = CIRCLE ( 'NONE', #45049, 6.646318662569999702 ) ;
#64713 = CARTESIAN_POINT ( 'NONE',  ( 42.54895236168549388, 1436.706489006040101, 270.0692006931200240 ) ) ;
#64714 = CARTESIAN_POINT ( 'NONE',  ( 3.266349474065000091, 1516.797038924770050, 213.1501537103870021 ) ) ;
#64715 = CARTESIAN_POINT ( 'NONE',  ( -50.84608916490000041, 1379.691708908819919, 241.2101448141589799 ) ) ;
#64716 = ADVANCED_FACE ( 'NONE', ( #99419 ), #73713, .F. ) ;
#64717 = CARTESIAN_POINT ( 'NONE',  ( 23.02067909570000026, 1409.743111324829897, 209.2425273049379939 ) ) ;
#64718 = CARTESIAN_POINT ( 'NONE',  ( 28.27139721233031722, 1526.382868172864164, 198.6830693683572235 ) ) ;
#64719 = DIRECTION ( 'NONE',  ( -1.000000000000000000, 0.000000000000000000, 0.000000000000000000 ) ) ;
#64720 = CARTESIAN_POINT ( 'NONE',  ( -7.709692149626850011, 1516.559523801380010, 210.7009757622840027 ) ) ;
#64721 = CARTESIAN_POINT ( 'NONE',  ( -5.770820179264999794, 1516.591755933730155, 210.8331571987770019 ) ) ;
#64722 = CARTESIAN_POINT ( 'NONE',  ( 4.196391599596410060, 1421.708143655280082, 184.6451467733209881 ) ) ;
#64723 = CARTESIAN_POINT ( 'NONE',  ( -5.208257314369999946, 1415.371260711229979, 232.0253136197979984 ) ) ;
#64724 = CARTESIAN_POINT ( 'NONE',  ( 8.160856992992099990, 1423.395965121194195, 139.1420365292543408 ) ) ;
#64725 = EDGE_LOOP ( 'NONE', ( #62410, #42075, #103105 ) ) ;
#64727 = AXIS2_PLACEMENT_3D ( 'NONE', #430, #8229, #42396 ) ;
#64726 = CARTESIAN_POINT ( 'NONE',  ( -24.60516260371240094, 1385.257503092070010, 223.4099358821769954 ) ) ;
#64728 = B_SPLINE_CURVE_WITH_KNOTS ( 'NONE', 3,
 ( #41953, #32453, #92894, #7787, #14525, #6131, #66629, #59327, #67170, #82840 ),
 .UNSPECIFIED., .F., .F.,
 ( 4, 2, 2, 2, 4 ),
 ( -0.1063667421838040000, -0.07694718867315308852, -0.05063894887267449824, -0.02539707194426270298, -1.064426199959278563E-09 ),
 .UNSPECIFIED. ) ;
#64729 = CARTESIAN_POINT ( 'NONE',  ( 30.60461244942474224, 1523.621879633028811, 196.4204177336139878 ) ) ;
#64730 = CARTESIAN_POINT ( 'NONE',  ( 1.237116821750000151, 1417.438760711529994, 234.9523517504979964 ) ) ;
#64731 = LINE ( 'NONE', #22106, #100433 ) ;
#64732 = CARTESIAN_POINT ( 'NONE',  ( -24.90078896885400184, 1441.036975948020199, 210.4313365108669984 ) ) ;
#64733 = CARTESIAN_POINT ( 'NONE',  ( 12.20133708979999909, 1421.549213611169989, 205.4486904848489814 ) ) ;
#64734 = CARTESIAN_POINT ( 'NONE',  ( -11.88915037982130052, 1434.057645910959991, 147.6474571075829658 ) ) ;
#64736 = CYLINDRICAL_SURFACE ( 'NONE', #13959, 1.500000000000001332 ) ;
#64735 = CARTESIAN_POINT ( 'NONE',  ( 1.708720984574999768, 1516.531533746980131, 216.4430152012269843 ) ) ;
#64737 = CARTESIAN_POINT ( 'NONE',  ( 11.60004869885203682, 0.000000000000000000, 137.0999999980979851 ) ) ;
#64738 = CARTESIAN_POINT ( 'NONE',  ( 30.79697748855865669, 1526.178928173327449, 221.8439766881941466 ) ) ;
#64739 = EDGE_LOOP ( 'NONE', ( #37789, #99793, #89039, #3821, #92079 ) ) ;
#64740 = CARTESIAN_POINT ( 'NONE',  ( -2.485846037024999955, 1516.545806094630279, 201.8003900583769905 ) ) ;
#64741 = EDGE_CURVE ( 'NONE', #109512, #9799, #34558, .T. ) ;
#64742 = ORIENTED_EDGE ( 'NONE', *, *, #3777, .T. ) ;
#64743 = CONICAL_SURFACE ( 'NONE', #66499, 21.50000000000000355, 0.3430239404209998177 ) ;
#64744 = CARTESIAN_POINT ( 'NONE',  ( 11.60004869885203327, 1426.371423827809394, 136.9558871456979148 ) ) ;
#64745 = CARTESIAN_POINT ( 'NONE',  ( 19.74167487489999928, 1455.375968942129930, 226.0788140436979745 ) ) ;
#64746 = CARTESIAN_POINT ( 'NONE',  ( 7.136348315603505910, 1439.003107248918923, 154.1041582727210368 ) ) ;
#64747 = EDGE_CURVE ( 'NONE', #55319, #31132, #107988, .T. ) ;
#64748 = CARTESIAN_POINT ( 'NONE',  ( 9.292547705917240108, 1425.240615715940748, 195.5975308281553566 ) ) ;
#64749 = VECTOR ( 'NONE', #108273, 1000.000000000000000 ) ;
#64750 = CARTESIAN_POINT ( 'NONE',  ( 1.021942164559999977, 1443.686436469889713, 217.9982604250890006 ) ) ;
#64751 = CARTESIAN_POINT ( 'NONE',  ( 16.36816379095389706, 1421.588183160469725, 227.2088594400390491 ) ) ;
#64752 = CARTESIAN_POINT ( 'NONE',  ( -3.654206553410000335, 1446.297061082940218, 167.4573427789980258 ) ) ;
#64753 = CARTESIAN_POINT ( 'NONE',  ( -19.53863231420000446, 1425.698533139729989, 223.3134001096979944 ) ) ;
#64754 = CARTESIAN_POINT ( 'NONE',  ( -3.061616997868380553E-17, 1389.413060387289988, 209.1218459616989946 ) ) ;
#64755 = CARTESIAN_POINT ( 'NONE',  ( -106.8894869739999933, 1388.082512067059952, 298.5417979983590158 ) ) ;
#64756 = CARTESIAN_POINT ( 'NONE',  ( 17.08559277830000056, 1445.364338547270108, 190.4514208886979816 ) ) ;
#64758 = CARTESIAN_POINT ( 'NONE',  ( 28.83583421379999834, 1509.587522266130009, 209.1233664437740174 ) ) ;
#64757 = CARTESIAN_POINT ( 'NONE',  ( -107.0467961469999949, 1391.913060387289988, 301.5621515082589781 ) ) ;
#64759 = DIRECTION ( 'NONE',  ( -0.002969046283321036261, 0.3161973579630307785, -0.9486887875280103355 ) ) ;
#64760 = ORIENTED_EDGE ( 'NONE', *, *, #109804, .T. ) ;
#64761 = CARTESIAN_POINT ( 'NONE',  ( -103.8942762430000073, 1379.883600127840054, 303.6250335555589572 ) ) ;
#64762 = CARTESIAN_POINT ( 'NONE',  ( -15.65196091179999982, 1508.451915991289980, 214.9530002531589901 ) ) ;
#64763 = DIRECTION ( 'NONE',  ( -1.000000000000000000, 0.000000000000000000, 0.000000000000000000 ) ) ;
#64764 = DIRECTION ( 'NONE',  ( 0.000000000000000000, 1.000000000000000000, 0.000000000000000000 ) ) ;
#64765 = CARTESIAN_POINT ( 'NONE',  ( -5.345848780929999933, 1483.903127912989930, 199.7205304764490279 ) ) ;
#64766 = CARTESIAN_POINT ( 'NONE',  ( 1.451115179245930031, 1504.682986288419897, 181.2193327503090075 ) ) ;
#64767 = CARTESIAN_POINT ( 'NONE',  ( -13.77266209894789917, 1517.051704408389924, 217.0393652727940150 ) ) ;
#64768 = B_SPLINE_CURVE_WITH_KNOTS ( 'NONE', 3,
 ( #105753, #28482, #3858, #88929, #89484, #96796, #46957, #20067, #88386, #11676, #97329, #98428, #109054, #39060, #91132, #73805, #91682, #22797, #57559, #92232, #64308, #15503, #83284, #14957, #90575, #49152, #108490, #48602, #21700, #65408, #23906, #40180, #6027, #74362, #107934, #65960, #31774, #30113, #55905, #40731, #4919, #90023, #74905, #81617, #13300, #47493, #6582, #13855, #98972, #48038, #32340, #30677 ),
 .UNSPECIFIED., .F., .F.,
 ( 4, 2, 2, 1, 1, 1, 2, 2, 2, 2, 1, 1, 1, 1, 1, 2, 2, 2, 2, 1, 1, 1, 1, 1, 2, 2, 2, 2, 1, 1, 1, 2, 2, 4 ),
 ( 0.000000000000000000, 0.1249999999996153077, 0.1874999999994217403, 0.2187499999993249566, 0.2343749999992864319, 0.2421874999992573163, 0.2460937499992527366, 0.2499999999992481570, 0.3749999999992578159, 0.4374999999992638666, 0.4687499999992769673, 0.4843749999992835731, 0.4921874999992881250, 0.4960937499993025024, 0.4980468749993096633, 0.4990234374993119948, 0.4999999999993143263, 0.6249999999997680744, 0.6874999999999948930, 0.7187500000001071365, 0.7343750000001494360, 0.7421875000001550982, 0.7460937500001577627, 0.7480468750001444400, 0.7490234375001525446, 0.7500000000001606493, 0.8125000000005421219, 0.8437500000007338574, 0.8593750000008296697, 0.8671875000008767431, 0.8710937500009010570, 0.8730468750008952838, 0.8750000000008895107, 1.000000000000000000 ),
 .UNSPECIFIED. ) ;
#64769 = CARTESIAN_POINT ( 'NONE',  ( -13.45091335949210176, 1444.296404058437247, 186.9862568266497078 ) ) ;
#64770 = CARTESIAN_POINT ( 'NONE',  ( -33.93019615848939452, 1512.187213306747481, 220.5829544587966211 ) ) ;
#64771 = CARTESIAN_POINT ( 'NONE',  ( -7.828115350939239825, 1507.298737064408897, 235.3518802339874583 ) ) ;
#64772 = DIRECTION ( 'NONE',  ( 0.000000000000000000, 0.02617694830742899742, -0.9996573249755689172 ) ) ;
#64773 = CARTESIAN_POINT ( 'NONE',  ( -103.2908355774439997, 1383.761877798790010, 310.9219936770090271 ) ) ;
#64774 = DIRECTION ( 'NONE',  ( 0.000000000000000000, -1.000000000000000000, 6.123233995736769734E-17 ) ) ;
#64775 = CARTESIAN_POINT ( 'NONE',  ( 7.242271949250000063, 1428.269950913389948, 213.9693205564990137 ) ) ;
#64777 = ORIENTED_EDGE ( 'NONE', *, *, #105628, .F. ) ;
#64776 = CARTESIAN_POINT ( 'NONE',  ( 20.17495212240000058, 1508.361596599530003, 189.3322781249979982 ) ) ;
#64778 = CARTESIAN_POINT ( 'NONE',  ( -109.9987473030000018, 1379.411466190030069, 303.3266014941589788 ) ) ;
#64779 = CARTESIAN_POINT ( 'NONE',  ( -16.56942828594061723, 1526.189892541618974, 235.5982591281702980 ) ) ;
#64780 = ORIENTED_EDGE ( 'NONE', *, *, #5619, .F. ) ;
#64781 = ORIENTED_EDGE ( 'NONE', *, *, #36883, .F. ) ;
#64782 = CARTESIAN_POINT ( 'NONE',  ( -11.92256551290000033, 1502.127826907089911, 209.4204567382010111 ) ) ;
#64783 = CARTESIAN_POINT ( 'NONE',  ( 13.36396446440000041, 1509.377767200929839, 234.5402373753979930 ) ) ;
#64784 = CARTESIAN_POINT ( 'NONE',  ( -10.60205606837675951, 1379.520036171940774, 202.7691692326841633 ) ) ;
#64786 = CARTESIAN_POINT ( 'NONE',  ( 3.980216533449999712E-09, 1468.084175534530004, 248.5896189557980165 ) ) ;
#64785 = CARTESIAN_POINT ( 'NONE',  ( 34.38405749794775801, 1423.397540913143985, 269.5231537529844559 ) ) ;
#64787 = CARTESIAN_POINT ( 'NONE',  ( -19.73850182230000172, 1499.093133259129900, 189.2250669414979996 ) ) ;
#64788 = CARTESIAN_POINT ( 'NONE',  ( -11.83876387009999931, 1433.336427731999947, 150.5404244326980177 ) ) ;
#64789 = B_SPLINE_CURVE_WITH_KNOTS ( 'NONE', 3,
 ( #43644, #54275, #105207, #35794, #95698, #52606, #95148, #18408 ),
 .UNSPECIFIED., .F., .F.,
 ( 4, 2, 2, 4 ),
 ( 3.103167691559091397E-17, 0.001073044933456083041, 0.001609567400184111442, 0.002146089866912140060 ),
 .UNSPECIFIED. ) ;
#64790 = DIRECTION ( 'NONE',  ( -1.000000000000000000, 0.000000000000000000, 0.000000000000000000 ) ) ;
#64791 = CARTESIAN_POINT ( 'NONE',  ( 11.68510097434900175, 1426.730240608209897, 140.4555551319089943 ) ) ;
#64792 = DIRECTION ( 'NONE',  ( -0.8529428551538207337, 0.5214727017401559195, 0.02355222244016309113 ) ) ;
#64793 = LINE ( 'NONE', #22719, #50000 ) ;
#64794 = CARTESIAN_POINT ( 'NONE',  ( 0.6118612315922750122, 1515.137305168469993, 213.4493959364910154 ) ) ;
#64795 = DIRECTION ( 'NONE',  ( -1.000000000000000000, 0.000000000000000000, 0.000000000000000000 ) ) ;
#64796 = CARTESIAN_POINT ( 'NONE',  ( -8.543213252583260697, 1478.735612270709908, 217.0402877408899940 ) ) ;
#64797 = CARTESIAN_POINT ( 'NONE',  ( 3.266939541527484003, 1361.645130185650032, 207.6218459616988241 ) ) ;
#64798 = CARTESIAN_POINT ( 'NONE',  ( -4.852802044422932504, 1509.212694702193176, 238.7485159040689950 ) ) ;
#64800 = ORIENTED_EDGE ( 'NONE', *, *, #9616, .T. ) ;
#64799 = CARTESIAN_POINT ( 'NONE',  ( 1.073572097657399993E-09, 1410.789257220119907, 256.6870931748030102 ) ) ;
#64801 = ORIENTED_EDGE ( 'NONE', *, *, #88419, .T. ) ;
#64802 = CARTESIAN_POINT ( 'NONE',  ( -11.51580851839999831, 1504.609797615890102, 207.7314770397890129 ) ) ;
#64803 = CARTESIAN_POINT ( 'NONE',  ( -21.46486267529380143, 1504.440111944700220, 215.6677449661270032 ) ) ;
#64804 = CARTESIAN_POINT ( 'NONE',  ( -13.58968549449999941, 1472.672770405929896, 270.0972160539979541 ) ) ;
#64805 = CARTESIAN_POINT ( 'NONE',  ( 1.193369943926424703, 1473.153843175627799, 219.2662284112174120 ) ) ;
#64806 =( BOUNDED_CURVE ( )  B_SPLINE_CURVE ( 3, ( #35754, #78303, #88909, #70492 ),
 .UNSPECIFIED., .F., .T. ) 
 B_SPLINE_CURVE_WITH_KNOTS ( ( 4, 4 ),
 ( 0.000000000000000000, 0.7048113239778038830 ),
 .UNSPECIFIED. ) 
 CURVE ( )  GEOMETRIC_REPRESENTATION_ITEM ( )  RATIONAL_B_SPLINE_CURVE ( ( 1.000000000000000000, 0.9590300661663093695, 0.9590300661663093695, 1.000000000000000000 ) ) 
 REPRESENTATION_ITEM ( '' )  );
#64807 = CARTESIAN_POINT ( 'NONE',  ( -123.7110048620000242, 1378.528619065189332, 301.5890141660771064 ) ) ;
#64808 = CARTESIAN_POINT ( 'NONE',  ( 1.997114500746473675, 1519.551704408389924, 188.3688149102297018 ) ) ;
#64809 = AXIS2_PLACEMENT_3D ( 'NONE', #105788, #44784, #37466 ) ;
#64810 = CARTESIAN_POINT ( 'NONE',  ( 0.3919100467378520136, 1450.899374586919976, 181.2708617675390030 ) ) ;
#64811 = CARTESIAN_POINT ( 'NONE',  ( -20.50000000000000000, 1445.052233488290085, 169.0968414572980123 ) ) ;
#64812 = CARTESIAN_POINT ( 'NONE',  ( 10.03610466974719984, 1469.085538504640226, 209.1195785090949926 ) ) ;
#64813 = B_SPLINE_CURVE_WITH_KNOTS ( 'NONE', 3,
 ( #39127, #106887, #29096, #97394 ),
 .UNSPECIFIED., .F., .F.,
 ( 4, 4 ),
 ( 0.000000000000000000, 0.0003467901758445098839 ),
 .UNSPECIFIED. ) ;
#64814 = CARTESIAN_POINT ( 'NONE',  ( -4.329473944230000093, 1458.307963197089975, 218.4835595929489784 ) ) ;
#64815 = CARTESIAN_POINT ( 'NONE',  ( 11.69568758614039083, 1366.517700528763953, 209.6218459617033432 ) ) ;
#64816 = CARTESIAN_POINT ( 'NONE',  ( -24.04206359393009862, 1411.123105596929918, 266.7326845484290061 ) ) ;
#64817 = ORIENTED_EDGE ( 'NONE', *, *, #100705, .F. ) ;
#64818 = CARTESIAN_POINT ( 'NONE',  ( -3.544577584565780093, 1502.375471873259812, 181.1794101401630144 ) ) ;
#64819 = ORIENTED_EDGE ( 'NONE', *, *, #26714, .T. ) ;
#64820 = ORIENTED_EDGE ( 'NONE', *, *, #46780, .T. ) ;
#64821 = CARTESIAN_POINT ( 'NONE',  ( 6.563595869685000750, 1517.154223579619838, 211.4114704024570131 ) ) ;
#64822 = CARTESIAN_POINT ( 'NONE',  ( 4.847717379287757922, 1423.484125437993725, 184.1362136828789176 ) ) ;
#64823 = CARTESIAN_POINT ( 'NONE',  ( 4.624736859184999993, 1516.994127245590107, 211.9896495963369887 ) ) ;
#64824 = CARTESIAN_POINT ( 'NONE',  ( -12.15287379559999970, 1455.446570946329985, 187.1561056955980007 ) ) ;
#64825 = CIRCLE ( 'NONE', #88071, 1.999999999999995559 ) ;
#64826 = CARTESIAN_POINT ( 'NONE',  ( -2.500000000000000444, 1449.021333099697358, 183.0995997157531576 ) ) ;
#64827 = EDGE_LOOP ( 'NONE', ( #30156, #15290, #109079, #38658 ) ) ;
#64828 = CARTESIAN_POINT ( 'NONE',  ( -26.15575153829999877, 1435.490056906990048, 135.8696537409980181 ) ) ;
#64829 = CARTESIAN_POINT ( 'NONE',  ( -3.454119954834999895, 1516.594591938570147, 201.4112355291069889 ) ) ;
#64830 = ADVANCED_FACE ( 'NONE', ( #5937 ), #34066, .F. ) ;
#64831 = CARTESIAN_POINT ( 'NONE',  ( -1.600048698852036821, 1401.254281879943164, 134.0999999980979851 ) ) ;
#64832 = CARTESIAN_POINT ( 'NONE',  ( -20.28517678552929837, 1384.534033518609931, 201.7562538433300006 ) ) ;
#64833 = CARTESIAN_POINT ( 'NONE',  ( -38.60728422249630398, 1426.656195254630120, 270.0188047174270309 ) ) ;
#64834 = CARTESIAN_POINT ( 'NONE',  ( -14.78755727007779974, 1487.414112128270062, 194.1688363173670098 ) ) ;
#64835 = CARTESIAN_POINT ( 'NONE',  ( -4.365829376490000691, 1396.065518508630021, 198.9343448857979979 ) ) ;
#64837 = ORIENTED_EDGE ( 'NONE', *, *, #57084, .F. ) ;
#64836 = CARTESIAN_POINT ( 'NONE',  ( -8.967890654244879300, 1365.210398484327470, 207.6218459616988241 ) ) ;
#64838 = ORIENTED_EDGE ( 'NONE', *, *, #58250, .F. ) ;
#64839 = CARTESIAN_POINT ( 'NONE',  ( -29.16136750932859556, 1526.143142182266047, 220.6593063691003920 ) ) ;
#64840 = CARTESIAN_POINT ( 'NONE',  ( 0.3759925524705069466, 1425.634515328159978, 191.1019336871629832 ) ) ;
#64841 = DIRECTION ( 'NONE',  ( -0.4978433412588729179, 0.000000000000000000, -0.8672669759446635096 ) ) ;
#64842 = CARTESIAN_POINT ( 'NONE',  ( -6.935801299664999142, 1516.621991115350056, 210.2518484644969874 ) ) ;
#64843 = CARTESIAN_POINT ( 'NONE',  ( -68.77190080519999071, 1379.747925807450201, 280.3125203366930123 ) ) ;
#64844 = CARTESIAN_POINT ( 'NONE',  ( 2.953701937874160244, 1440.359118138959957, 157.3263569013780057 ) ) ;
#64845 = EDGE_CURVE ( 'NONE', #68294, #30006, #42290, .T. ) ;
#64846 = CARTESIAN_POINT ( 'NONE',  ( 8.409376565895700040, 1438.261224657589764, 211.4481330912490193 ) ) ;
#64847 = FACE_OUTER_BOUND ( 'NONE', #56417, .T. ) ;
#64848 = CARTESIAN_POINT ( 'NONE',  ( 7.853883982725000656, 1511.558654537720031, 205.7547918027769924 ) ) ;
#64849 = CARTESIAN_POINT ( 'NONE',  ( 7.323390407215000231, 1516.613712827999962, 207.9924597298270044 ) ) ;
#64850 = EDGE_LOOP ( 'NONE', ( #61779, #34536 ) ) ;
#64851 = CARTESIAN_POINT ( 'NONE',  ( -38.81202641437909762, 1450.612734560829949, 135.3761647280269926 ) ) ;
#64852 = CARTESIAN_POINT ( 'NONE',  ( -23.49479895857739464, 1448.333498076887736, 215.7494633260788817 ) ) ;
#64853 = ORIENTED_EDGE ( 'NONE', *, *, #60523, .T. ) ;
#64854 = CARTESIAN_POINT ( 'NONE',  ( -2.157536728407475568, 1397.913060387289988, 210.3005136483574518 ) ) ;
#64856 = EDGE_CURVE ( 'NONE', #17784, #28004, #81356, .T. ) ;
#64855 = LINE ( 'NONE', #12208, #80644 ) ;
#64857 = CARTESIAN_POINT ( 'NONE',  ( 13.76682154080000053, 1416.274718422629803, 196.4072499923979933 ) ) ;
#64858 = B_SPLINE_CURVE_WITH_KNOTS ( 'NONE', 3,
 ( #97892, #4940, #99540, #81098, #57030, #63245 ),
 .UNSPECIFIED., .F., .F.,
 ( 4, 2, 4 ),
 ( 0.000000000000000000, 0.5000000000000000000, 1.000000000000000000 ),
 .UNSPECIFIED. ) ;
#64859 = CARTESIAN_POINT ( 'NONE',  ( -6.273787032870000502, 1415.168582340579860, 205.7307369784189746 ) ) ;
#64860 = CARTESIAN_POINT ( 'NONE',  ( 0.5779273184081717973, 1522.051704408389924, 232.1634304495918002 ) ) ;
#64861 = CARTESIAN_POINT ( 'NONE',  ( 16.40119948470000111, 1409.652464919530075, 226.0181189845979759 ) ) ;
#64862 = CARTESIAN_POINT ( 'NONE',  ( 31.23437356469446868, 1518.913060387330006, 222.8968241038843701 ) ) ;
#64863 = DIRECTION ( 'NONE',  ( -0.9455185755993177343, 0.000000000000000000, 0.3255681544571540909 ) ) ;
#64864 = CARTESIAN_POINT ( 'NONE',  ( 4.255617697982819969, 1441.290921029950141, 160.2176512041789920 ) ) ;
#64865 = DIRECTION ( 'NONE',  ( 0.000000000000000000, 1.000000000000000000, 0.000000000000000000 ) ) ;
#64866 = CARTESIAN_POINT ( 'NONE',  ( 6.556651371285000529, 1516.858146885269889, 215.6747433371770057 ) ) ;
#64867 = ORIENTED_EDGE ( 'NONE', *, *, #8801, .T. ) ;
#64868 = CARTESIAN_POINT ( 'NONE',  ( -17.72676975039999903, 1418.059941342760112, 206.6000183712389742 ) ) ;
#64869 = CARTESIAN_POINT ( 'NONE',  ( -8.322172262500000528, 1473.608514543630008, 270.1222559170979594 ) ) ;
#64870 = DIRECTION ( 'NONE',  ( -0.7071067811865474617, -6.092092863024105611E-16, -0.7071067811865474617 ) ) ;
#64871 = CARTESIAN_POINT ( 'NONE',  ( -6.305026483082059485, 1422.156206029339955, 144.1470533162859908 ) ) ;
#64872 = CARTESIAN_POINT ( 'NONE',  ( -3.118824320620000368, 1475.108726717689933, 218.9463081056090061 ) ) ;
#64873 = ADVANCED_FACE ( 'NONE', ( #17046 ), #106364, .F. ) ;
#64874 = CARTESIAN_POINT ( 'NONE',  ( 11.36480844366392517, 1425.604749195035765, 138.8039940692290486 ) ) ;
#64875 = CARTESIAN_POINT ( 'NONE',  ( 2.290177320370077485, 1417.585464588979448, 233.4942916757924820 ) ) ;
#64876 = CARTESIAN_POINT ( 'NONE',  ( 17.98285126925155808, 1424.103838246010582, 225.5445409078726016 ) ) ;
#64877 = CARTESIAN_POINT ( 'NONE',  ( -2.426602077163350302, 1454.706936359410065, 198.9117694354199841 ) ) ;
#64878 = LINE ( 'NONE', #75479, #43383 ) ;
#64879 = CARTESIAN_POINT ( 'NONE',  ( 33.54441201048500432, 1440.913060383900074, 247.8471729086510038 ) ) ;
#64880 = CARTESIAN_POINT ( 'NONE',  ( -109.5358681720000078, 1384.943159170210265, 297.1231916241590056 ) ) ;
#64881 = DIRECTION ( 'NONE',  ( 1.000000000000000000, 0.000000000000000000, 0.000000000000000000 ) ) ;
#64882 = ORIENTED_EDGE ( 'NONE', *, *, #56465, .T. ) ;
#64883 = ORIENTED_EDGE ( 'NONE', *, *, #102468, .F. ) ;
#64884 = CARTESIAN_POINT ( 'NONE',  ( 13.51610093808349866, 1443.913060387330006, 150.6358704321320090 ) ) ;
#64885 = CARTESIAN_POINT ( 'NONE',  ( -0.4151546846821903003, 1501.977400791986611, 173.3106345060153046 ) ) ;
#64886 = B_SPLINE_CURVE_WITH_KNOTS ( 'NONE', 3,
 ( #38711, #54456, #72886, #46048 ),
 .UNSPECIFIED., .F., .F.,
 ( 4, 4 ),
 ( 0.003723731023023103479, 0.004070443920417508681 ),
 .UNSPECIFIED. ) ;
#64887 = CARTESIAN_POINT ( 'NONE',  ( -29.02628104849999957, 1509.926680457029988, 211.9910930718879740 ) ) ;
#64888 = CARTESIAN_POINT ( 'NONE',  ( 7.886556196039999911, 1423.699161883410170, 195.9191256520989839 ) ) ;
#64889 = DIRECTION ( 'NONE',  ( 1.000000000000000000, 0.000000000000000000, 0.000000000000000000 ) ) ;
#64890 = CARTESIAN_POINT ( 'NONE',  ( 1.997239979113719865, 1508.551704408389924, 219.6740723297500040 ) ) ;
#64891 = CARTESIAN_POINT ( 'NONE',  ( -53.07794406699930079, 1383.806925713539840, 267.6250404484239880 ) ) ;
#64892 = CARTESIAN_POINT ( 'NONE',  ( -5.381312013895000135, 1511.468585915670019, 200.7968825106569852 ) ) ;
#64893 = CARTESIAN_POINT ( 'NONE',  ( -15.02984757429999974, 1489.474306033729817, 193.0520931039979757 ) ) ;
#64894 = CARTESIAN_POINT ( 'NONE',  ( -12.24467222372750008, 1502.437705295270007, 208.9618294917469825 ) ) ;
#64895 = CARTESIAN_POINT ( 'NONE',  ( 2.194850040300000416, 1464.708290688329953, 236.4512987645979933 ) ) ;
#64897 = ORIENTED_EDGE ( 'NONE', *, *, #109085, .F. ) ;
#64896 = CARTESIAN_POINT ( 'NONE',  ( -4.844790491859999548, 1489.192796749890022, 188.8948260823989926 ) ) ;
#64898 = CARTESIAN_POINT ( 'NONE',  ( -0.9007582589660000361, 1450.862954789030027, 181.4326571169980014 ) ) ;
#64899 = CARTESIAN_POINT ( 'NONE',  ( -26.36437929639999922, 1382.323664421269996, 223.7125964019590185 ) ) ;
#64900 = CARTESIAN_POINT ( 'NONE',  ( -3.269263786600000277, 1476.740800597890029, 199.2818572616789936 ) ) ;
#64902 = EDGE_LOOP ( 'NONE', ( #79268, #110413, #83122, #28952 ) ) ;
#64901 = CARTESIAN_POINT ( 'NONE',  ( 1.556370309037290012, 1414.996442620790276, 191.7142051069610034 ) ) ;
#64903 = CARTESIAN_POINT ( 'NONE',  ( 5.076304971681840250, 1469.790025430949981, 187.8425727480230023 ) ) ;
#64904 = ORIENTED_EDGE ( 'NONE', *, *, #37734, .F. ) ;
#64905 = CARTESIAN_POINT ( 'NONE',  ( -12.25820234982129975, 1388.996037939079997, 215.8687775299890177 ) ) ;
#64906 = CARTESIAN_POINT ( 'NONE',  ( -2.329939114882829898, 1515.551844914359890, 205.1381281626180169 ) ) ;
#64907 = LINE ( 'NONE', #39112, #40480 ) ;
#64908 = CARTESIAN_POINT ( 'NONE',  ( -11.60004869884790679, 1426.654320091513227, 134.6710072971295915 ) ) ;
#64909 = APPLICATION_CONTEXT ( 'automotive_design' ) ;
#64910 = FACE_OUTER_BOUND ( 'NONE', #73686, .T. ) ;
#64911 = CARTESIAN_POINT ( 'NONE',  ( 1.313206738690460007, 1408.958918577119903, 194.1820485240640153 ) ) ;
#64912 = CARTESIAN_POINT ( 'NONE',  ( 1.133107404670000040, 1409.891086916829863, 185.2370129161979833 ) ) ;
#64913 = DIRECTION ( 'NONE',  ( 0.7384854939282345931, 0.000000000000000000, -0.6742693640212131800 ) ) ;
#64914 = CARTESIAN_POINT ( 'NONE',  ( -17.51076275510000002, 1437.054563566370007, 191.0009178520979845 ) ) ;
#64915 = CARTESIAN_POINT ( 'NONE',  ( 11.30152483799999885, 1432.323726532349838, 151.5220244154980094 ) ) ;
#64916 = DIRECTION ( 'NONE',  ( -0.2054769195713180285, 0.000000000000000000, 0.9786619618251657382 ) ) ;
#64917 = ORIENTED_EDGE ( 'NONE', *, *, #38900, .T. ) ;
#64918 = ORIENTED_EDGE ( 'NONE', *, *, #107484, .F. ) ;
#64919 = CARTESIAN_POINT ( 'NONE',  ( 18.49724510411089895, 1458.837717710030120, 227.6444223862160072 ) ) ;
#64920 = DIRECTION ( 'NONE',  ( -0.01802056537744943510, 0.000000000000000000, 0.9998376164275263323 ) ) ;
#64921 = FACE_OUTER_BOUND ( 'NONE', #71054, .T. ) ;
#64922 = CARTESIAN_POINT ( 'NONE',  ( -20.48903499640979931, 1504.270597067930112, 190.4936467704999927 ) ) ;
#64923 = CARTESIAN_POINT ( 'NONE',  ( 13.62888593203049936, 1517.051704413129983, 191.9442378289920157 ) ) ;
#64924 = CARTESIAN_POINT ( 'NONE',  ( -108.7465780080000002, 1386.162170843670083, 311.0556125892589421 ) ) ;
#64925 = CARTESIAN_POINT ( 'NONE',  ( -7.679314503873669651, 1511.182265711489890, 215.0124326349510113 ) ) ;
#64926 = CARTESIAN_POINT ( 'NONE',  ( -10.73667021122307297, 1363.210612206614996, 210.6218459617030021 ) ) ;
#64927 = CARTESIAN_POINT ( 'NONE',  ( 1.514120561980000183E-16, 1515.551704408389924, 209.1218459616989946 ) ) ;
#64928 = CARTESIAN_POINT ( 'NONE',  ( -5.432410439472700858, 1391.426148861440197, 203.3415300314919989 ) ) ;
#64929 = CARTESIAN_POINT ( 'NONE',  ( 1.701850457105000158, 1516.908147884120126, 207.9845492812970065 ) ) ;
#64930 = CARTESIAN_POINT ( 'NONE',  ( -9.622749971728280727, 1447.247763375919931, 211.4452405505059858 ) ) ;
#64931 = CARTESIAN_POINT ( 'NONE',  ( 1.430133918726229858, 1408.963001764240062, 224.1218459596319974 ) ) ;
#64932 = CARTESIAN_POINT ( 'NONE',  ( -13.19741843239559920, 1434.958471197750214, 149.6694188718060161 ) ) ;
#64933 = CARTESIAN_POINT ( 'NONE',  ( -8.881957496880000136, 1385.278510013270079, 218.6647829999089936 ) ) ;
#64934 = CARTESIAN_POINT ( 'NONE',  ( -3.968827103576990201, 1517.151704408390060, 229.5396913781519856 ) ) ;
#64935 = CARTESIAN_POINT ( 'NONE',  ( 7.183386785930029994, 1424.944879424049986, 212.8809111208099694 ) ) ;
#64936 = ORIENTED_EDGE ( 'NONE', *, *, #14464, .F. ) ;
#64937 = CARTESIAN_POINT ( 'NONE',  ( 34.21122890170000375, 1429.487523075830040, 254.6787130006979964 ) ) ;
#64938 = CARTESIAN_POINT ( 'NONE',  ( -25.47381561740000322, 1508.124471598029913, 199.2434219609179991 ) ) ;
#64940 = CARTESIAN_POINT ( 'NONE',  ( -17.11609476099999583, 1409.675656833430139, 194.7256359347979924 ) ) ;
#64939 = CARTESIAN_POINT ( 'NONE',  ( -11.70942943321529839, 1491.329393039050046, 206.7632756908639919 ) ) ;
#64941 = CARTESIAN_POINT ( 'NONE',  ( 20.90608034670421489, 1506.501081260929141, 202.1326028675541124 ) ) ;
#64942 = B_SPLINE_CURVE_WITH_KNOTS ( 'NONE', 3,
 ( #68856, #50934, #77245, #24587, #84520, #76674, #110824, #26260, #41976, #25697, #101291, #1096, #59350, #59896, #95138, #16190, #545, #102959, #60447, #17283, #51477, #69411, #85607, #52597 ),
 .UNSPECIFIED., .F., .F.,
 ( 4, 1, 1, 1, 1, 1, 1, 1, 1, 1, 1, 1, 1, 1, 1, 1, 1, 1, 1, 1, 1, 4 ),
 ( 0.000000000000000000, 0.03678250764465099826, 0.07385281888605636780, 0.1111996474769267329, 0.1487830646126913348, 0.1865181366940833751, 0.2243518957215068221, 0.2622984075178853014, 0.3003633763990504746, 0.3385433752522598039, 0.3768295913742388814, 0.4152115393309738778, 0.4536807115451020334, 0.4922340963814919035, 0.5605612547399086987, 0.7446199554937297238, 0.7613094231601892359, 0.7882927121057347053, 0.8256044977319447753, 0.8732899491329376707, 0.9314021484345864632, 1.000000000000000000 ),
 .UNSPECIFIED. ) ;
#64943 = CARTESIAN_POINT ( 'NONE',  ( -27.31509605250000305, 1435.476323111060083, 231.6984297931980166 ) ) ;
#64944 = CARTESIAN_POINT ( 'NONE',  ( 7.683535900364350191, 1517.051704408389924, 209.5573457314510222 ) ) ;
#64945 = CARTESIAN_POINT ( 'NONE',  ( -11.67164634742229978, 1452.505477515639996, 149.8358995112070033 ) ) ;
#64946 = CARTESIAN_POINT ( 'NONE',  ( 22.86388144384979881, 1435.295931049420005, 134.1000000033949959 ) ) ;
#64947 = ORIENTED_EDGE ( 'NONE', *, *, #82259, .T. ) ;
#64948 = CARTESIAN_POINT ( 'NONE',  ( -108.1636966620979905, 1378.913060387289988, 299.7761360902010210 ) ) ;
#64949 = CARTESIAN_POINT ( 'NONE',  ( 16.66701395081591031, 1523.530870145310928, 237.7590812510444493 ) ) ;
#64950 = CARTESIAN_POINT ( 'NONE',  ( 14.36093106826099941, 1421.078536739219999, 228.5629966840699865 ) ) ;
#64951 = ORIENTED_EDGE ( 'NONE', *, *, #56640, .T. ) ;
#64952 = VERTEX_POINT ( 'NONE', #6482 ) ;
#64953 = CARTESIAN_POINT ( 'NONE',  ( 9.380465540465371177, 1451.944138759889938, 210.1274675918040202 ) ) ;
#64954 = CARTESIAN_POINT ( 'NONE',  ( 6.016568497259999759, 1422.672370635280004, 194.9161982602989838 ) ) ;
#64955 = VERTEX_POINT ( 'NONE', #33319 ) ;
#64956 = CARTESIAN_POINT ( 'NONE',  ( 0.2228126134860000107, 1419.322656201930158, 227.2982164590980005 ) ) ;
#64957 = CARTESIAN_POINT ( 'NONE',  ( 20.99949974029999922, 1495.227265342490000, 211.1851663224690014 ) ) ;
#64958 = CARTESIAN_POINT ( 'NONE',  ( -3.370431671830000031, 1507.639056475829875, 236.7514476338979819 ) ) ;
#64959 = CARTESIAN_POINT ( 'NONE',  ( 16.81049281787637639, 1526.143142182265819, 235.5964692618685774 ) ) ;
#64960 = VERTEX_POINT ( 'NONE', #32238 ) ;
#64961 = ADVANCED_FACE ( 'NONE', ( #74805 ), #56131, .F. ) ;
#64962 = CARTESIAN_POINT ( 'NONE',  ( 45.55029481160520533, 1443.690934598179865, 266.1917672049960402 ) ) ;
#64963 = CARTESIAN_POINT ( 'NONE',  ( -13.15726447900050111, 1414.913057819769847, 220.2185343040899852 ) ) ;
#64964 = CARTESIAN_POINT ( 'NONE',  ( 0.01268070879549999981, 1420.208146125329904, 183.8974516564980206 ) ) ;
#64965 = CARTESIAN_POINT ( 'NONE',  ( -0.7560907659159991079, 1516.770163853809890, 204.1215159365669933 ) ) ;
#64966 = VERTEX_POINT ( 'NONE', #42850 ) ;
#64967 = CARTESIAN_POINT ( 'NONE',  ( 10.19012721036619951, 1481.561516676249994, 215.0834239772050012 ) ) ;
#64968 = CARTESIAN_POINT ( 'NONE',  ( 13.14730852243417125, 1443.066035680741606, 187.4537189246333071 ) ) ;
#64969 = ORIENTED_EDGE ( 'NONE', *, *, #18113, .F. ) ;
#64970 = ORIENTED_EDGE ( 'NONE', *, *, #78200, .F. ) ;
#64971 = CARTESIAN_POINT ( 'NONE',  ( -10.70617203047970101, 1481.026974688039900, 208.9677961751969804 ) ) ;
#64972 = CARTESIAN_POINT ( 'NONE',  ( 13.78858221403500117, 1513.492015765619954, 196.0403704991670111 ) ) ;
#64973 = CARTESIAN_POINT ( 'NONE',  ( -12.49443853494850032, 1512.179780174510142, 194.1456554007820330 ) ) ;
#64974 = CARTESIAN_POINT ( 'NONE',  ( 2.364810563598290116, 1452.830479382759904, 152.4381100973169794 ) ) ;
#64975 = CARTESIAN_POINT ( 'NONE',  ( 12.62890211870000101, 1420.357139060750114, 200.3668987843989839 ) ) ;
#64976 = DIRECTION ( 'NONE',  ( 5.569232340736249362E-09, 0.03085823662921604107, -0.9995237712191418211 ) ) ;
#64977 = CARTESIAN_POINT ( 'NONE',  ( 10.98347131258903531, 1433.186512253130104, 151.7693442413542186 ) ) ;
#64978 = DIRECTION ( 'NONE',  ( 1.407418274235009893E-17, 1.000000000000000000, -2.576261870300909820E-17 ) ) ;
#64979 = CARTESIAN_POINT ( 'NONE',  ( 0.03404605193919440359, 1409.337710408478870, 232.7998981013873561 ) ) ;
#64981 = CARTESIAN_POINT ( 'NONE',  ( 17.16792148770000281, 1507.624001450029937, 193.8207119598980057 ) ) ;
#64980 = CARTESIAN_POINT ( 'NONE',  ( 5.009886284249999377, 1430.069699660889910, 217.1776678749689893 ) ) ;
#64982 = CARTESIAN_POINT ( 'NONE',  ( 10.76705900790449988, 1423.512433835739785, 206.7766633243239767 ) ) ;
#64983 = CARTESIAN_POINT ( 'NONE',  ( -24.06019813578369693, 1508.205534045840068, 222.3305738533050260 ) ) ;
#64984 = CARTESIAN_POINT ( 'NONE',  ( 4.852453529149999945, 1427.440084250629980, 147.7756948909979826 ) ) ;
#64985 = ORIENTED_EDGE ( 'NONE', *, *, #48750, .F. ) ;
#64986 = CARTESIAN_POINT ( 'NONE',  ( 19.62446893450000118, 1440.913060387330006, 214.3676144200779845 ) ) ;
#64987 = FACE_OUTER_BOUND ( 'NONE', #43875, .T. ) ;
#64988 = CARTESIAN_POINT ( 'NONE',  ( -98.46611804737121076, 1384.949949166809802, 310.6468918634429883 ) ) ;
#64989 = CARTESIAN_POINT ( 'NONE',  ( -7.988067379700000359, 1385.733169288700083, 199.5350710154689864 ) ) ;
#64990 = CARTESIAN_POINT ( 'NONE',  ( 11.02890202689059862, 1422.198172311190092, 210.7302511592479846 ) ) ;
#64992 = ORIENTED_EDGE ( 'NONE', *, *, #870, .F. ) ;
#64991 = CARTESIAN_POINT ( 'NONE',  ( -16.89965117564359787, 1419.540396951069852, 208.5087401362400215 ) ) ;
#64993 = CARTESIAN_POINT ( 'NONE',  ( 1.865807842320000187, 1429.738386184189949, 217.2385783028290120 ) ) ;
#64994 = CARTESIAN_POINT ( 'NONE',  ( -2.927701378049999713E-15, 1442.756953654919926, 150.7628527808980152 ) ) ;
#64995 = CARTESIAN_POINT ( 'NONE',  ( -16.69591095510000045, 1417.051168577799899, 207.9278418973390217 ) ) ;
#64996 = CARTESIAN_POINT ( 'NONE',  ( 11.93044055110000023, 1433.480854295200061, 150.1316028450980298 ) ) ;
#64997 = CARTESIAN_POINT ( 'NONE',  ( 17.87874079019999840, 1466.750581349630238, 265.6112250856980381 ) ) ;
#64998 = CARTESIAN_POINT ( 'NONE',  ( 13.15726445890019924, 1415.090956648730071, 197.4244024782210261 ) ) ;
#64999 = CARTESIAN_POINT ( 'NONE',  ( 3.776171005225210209, 1457.654323051970096, 199.8439998585350281 ) ) ;
#65000 = CARTESIAN_POINT ( 'NONE',  ( 7.722830810765720422, 1424.481984735209835, 195.1132992968850033 ) ) ;
#65001 = AXIS2_PLACEMENT_3D ( 'NONE', #106741, #4307, #21618 ) ;
#65002 = CARTESIAN_POINT ( 'NONE',  ( 16.78081809529999902, 1422.111771137829919, 226.9773849540979995 ) ) ;
#65003 = CARTESIAN_POINT ( 'NONE',  ( -21.13130013988097389, 1524.397344074317971, 237.4101150494072954 ) ) ;
#65004 = CARTESIAN_POINT ( 'NONE',  ( 0.000000000000000000, 1522.382868172863937, 177.3106345060153046 ) ) ;
#65005 = CARTESIAN_POINT ( 'NONE',  ( -12.27023110815660090, 1416.839692126590080, 194.6640136892829958 ) ) ;
#65006 = CARTESIAN_POINT ( 'NONE',  ( 14.03282286439999993, 1434.988470873060123, 148.9022279828979833 ) ) ;
#65007 = CARTESIAN_POINT ( 'NONE',  ( -1.545334783909999787, 1420.511277924829983, 228.1845102176980049 ) ) ;
#65008 = CARTESIAN_POINT ( 'NONE',  ( 8.800740351439999998, 1452.938977316690170, 191.5447439844990072 ) ) ;
#65009 = CARTESIAN_POINT ( 'NONE',  ( -12.54019733330000008, 1391.397793261360221, 209.7548870936209937 ) ) ;
#65010 = CARTESIAN_POINT ( 'NONE',  ( 1.842962231260000028, 1515.551704408389924, 205.1377642093389966 ) ) ;
#65011 = CARTESIAN_POINT ( 'NONE',  ( -14.35822996286229980, 1417.017622938350087, 203.2444471570910025 ) ) ;
#65012 = FACE_OUTER_BOUND ( 'NONE', #77057, .T. ) ;
#65013 = CARTESIAN_POINT ( 'NONE',  ( 4.602958218326069779E-16, 1426.918876943007945, 134.0999999980979851 ) ) ;
#65014 = CARTESIAN_POINT ( 'NONE',  ( 0.2146574046981659933, 1454.739073199480117, 183.1787909047579888 ) ) ;
#65015 = CARTESIAN_POINT ( 'NONE',  ( -14.97927429840000002, 1409.436148172130061, 207.8035683059279961 ) ) ;
#65016 = CARTESIAN_POINT ( 'NONE',  ( -14.57172186309999873, 1416.216739748630062, 198.5744135584980086 ) ) ;
#65017 = CARTESIAN_POINT ( 'NONE',  ( 1.010561960472377230, 1484.609605269575013, 198.4571475875856663 ) ) ;
#65018 = CARTESIAN_POINT ( 'NONE',  ( 13.50105822729999971, 1434.968970759619879, 148.5019007266980111 ) ) ;
#65019 = CARTESIAN_POINT ( 'NONE',  ( -34.72084050082580120, 1435.748200648189822, 134.0999999979019890 ) ) ;
#65020 = DIRECTION ( 'NONE',  ( 0.4794255386042031719, 0.000000000000000000, 0.8775825618903726477 ) ) ;
#65021 = ORIENTED_EDGE ( 'NONE', *, *, #106934, .T. ) ;
#65022 = CARTESIAN_POINT ( 'NONE',  ( -16.52275002910772272, 1525.042412244735260, 180.9740555130105122 ) ) ;
#65023 = CARTESIAN_POINT ( 'NONE',  ( 2.326513307810000430, 1476.258183369789776, 197.8633931413990013 ) ) ;
#65024 = CARTESIAN_POINT ( 'NONE',  ( -16.79355120555579717, 1420.470915846049820, 203.2250788671829866 ) ) ;
#65025 = CARTESIAN_POINT ( 'NONE',  ( 5.371346801041280372, 1516.551188146539971, 199.4837300725229738 ) ) ;
#65026 = FACE_OUTER_BOUND ( 'NONE', #47443, .T. ) ;
#65027 = CARTESIAN_POINT ( 'NONE',  ( -0.4151546846821903003, 1501.977400791986611, 175.3106345060153046 ) ) ;
#65028 = CARTESIAN_POINT ( 'NONE',  ( 19.73997541995389327, 1410.042412248772507, 269.5249961499508800 ) ) ;
#65029 = CARTESIAN_POINT ( 'NONE',  ( 20.24918891140000099, 1453.165958253830013, 209.7008772832169825 ) ) ;
#65030 = CARTESIAN_POINT ( 'NONE',  ( -12.28044260189999903, 1378.789922127170030, 210.3771987704189996 ) ) ;
#65031 = CARTESIAN_POINT ( 'NONE',  ( 33.36586802512179162, 1512.187213306747481, 216.3367586934468818 ) ) ;
#65032 = CARTESIAN_POINT ( 'NONE',  ( -56.65180216886200526, 1385.045677901099907, 237.0459369986420199 ) ) ;
#65033 = CARTESIAN_POINT ( 'NONE',  ( -12.19432067802980058, 1490.774705066830165, 207.8227360995649917 ) ) ;
#65034 = CARTESIAN_POINT ( 'NONE',  ( -4.985290750076490696, 1508.551704408389924, 206.5066873982580091 ) ) ;
#65035 = CARTESIAN_POINT ( 'NONE',  ( -27.02655812420000103, 1451.969196582630047, 135.3522152283979949 ) ) ;
#65036 = CARTESIAN_POINT ( 'NONE',  ( 1.912903644477788934, 1526.104292489128966, 177.3592290664105349 ) ) ;
#65037 = CARTESIAN_POINT ( 'NONE',  ( -15.84999874720450030, 1409.466461689740072, 225.3744910454719843 ) ) ;
#65039 = EDGE_LOOP ( 'NONE', ( #54920, #69175, #96081, #20390, #78396, #56682, #100888, #63330 ) ) ;
#65038 = DIRECTION ( 'NONE',  ( -0.6736849260863839728, 0.000000000000000000, 0.7390186874254150995 ) ) ;
#65040 = CARTESIAN_POINT ( 'NONE',  ( -109.8254909340000012, 1384.904097876479909, 311.3807978792589779 ) ) ;
#65041 = EDGE_CURVE ( 'NONE', #11721, #88474, #84726, .T. ) ;
#65042 = CARTESIAN_POINT ( 'NONE',  ( 10.15612571795790053, 1470.518962983220035, 210.4951917859000048 ) ) ;
#65043 = EDGE_CURVE ( 'NONE', #33692, #51877, #87676, .T. ) ;
#65044 = CARTESIAN_POINT ( 'NONE',  ( -22.35793875571175704, 1411.052089644072339, 213.2600881478184078 ) ) ;
#65045 = CARTESIAN_POINT ( 'NONE',  ( -109.1111606190000032, 1384.583257063580049, 311.2497810012590094 ) ) ;
#65046 = DIRECTION ( 'NONE',  ( 1.000000000000000000, -0.000000000000000000, -0.000000000000000000 ) ) ;
#65047 = CARTESIAN_POINT ( 'NONE',  ( 0.9807047822899999101, 1465.891021135629899, 235.6257849829979989 ) ) ;
#65048 = EDGE_CURVE ( 'NONE', #51642, #50916, #29213, .T. ) ;
#65049 = CARTESIAN_POINT ( 'NONE',  ( 21.38088874639999659, 1410.581319675330178, 217.4617667072079996 ) ) ;
#65050 = DIRECTION ( 'NONE',  ( -0.02616798426450828510, 0.9993150019883944024, -0.02616798426450858348 ) ) ;
#65051 = EDGE_CURVE ( 'NONE', #33454, #67358, #68692, .T. ) ;
#65052 = CARTESIAN_POINT ( 'NONE',  ( -9.632490594537660655, 1464.050392106980098, 228.1736160443419976 ) ) ;
#65053 = CARTESIAN_POINT ( 'NONE',  ( -17.07859384879999709, 1422.557183082329857, 226.8334922828980211 ) ) ;
#65055 = CARTESIAN_POINT ( 'NONE',  ( 22.06116865624104051, 1506.527232287948436, 209.0797454662948383 ) ) ;
#65054 = CARTESIAN_POINT ( 'NONE',  ( -4.822683201000122821, 1511.395345385124756, 200.6579470351961447 ) ) ;
#65056 = CARTESIAN_POINT ( 'NONE',  ( 24.17539452729910110, 1411.086234962870094, 209.2386321558909685 ) ) ;
#65057 = CARTESIAN_POINT ( 'NONE',  ( -106.4559248862600072, 1358.631207110790001, 304.2218459572590064 ) ) ;
#65058 = CARTESIAN_POINT ( 'NONE',  ( 16.50400130224771544, 1525.907212628473644, 236.2546788475581820 ) ) ;
#65059 = CARTESIAN_POINT ( 'NONE',  ( -0.5401129779459999947, 1417.004128308830104, 234.1403188875979708 ) ) ;
#65060 = CARTESIAN_POINT ( 'NONE',  ( 9.369782510120000296, 1366.497526915279877, 210.6218459616991936 ) ) ;
#65061 = CARTESIAN_POINT ( 'NONE',  ( 7.710285837685000310, 1516.582197289609894, 205.8614676770269796 ) ) ;
#65062 = CARTESIAN_POINT ( 'NONE',  ( -18.11291060900000005, 1424.770096122030054, 227.5276574296979959 ) ) ;
#65063 = EDGE_LOOP ( 'NONE', ( #36045, #37748, #2866, #1728, #16243, #45277, #75941, #3591, #46871, #49913, #34070, #18789, #18643, #60134, #23760, #104935, #54947, #75724, #82214, #95500 ) ) ;
#65064 = DIRECTION ( 'NONE',  ( 0.9510565162951518658, 0.000000000000000000, -0.3090169943749528914 ) ) ;
#65065 = CARTESIAN_POINT ( 'NONE',  ( -4.225717896591520528, 1441.570140337609928, 166.2107877269230016 ) ) ;
#65067 = VERTEX_POINT ( 'NONE', #105941 ) ;
#65066 = CARTESIAN_POINT ( 'NONE',  ( -68.45261304049999751, 1379.747725225370004, 280.0177415624590367 ) ) ;
#65068 = ORIENTED_EDGE ( 'NONE', *, *, #78924, .F. ) ;
#65069 = CARTESIAN_POINT ( 'NONE',  ( -8.325002224603874623, 1381.957443703849094, 218.3429956565692009 ) ) ;
#65070 = ORIENTED_EDGE ( 'NONE', *, *, #34461, .F. ) ;
#65071 = CARTESIAN_POINT ( 'NONE',  ( 2.632747685671115612, 1379.913060387289988, 210.5601225775116063 ) ) ;
#65072 = CARTESIAN_POINT ( 'NONE',  ( 12.61744324630000058, 1500.191175618890156, 207.7465061732789877 ) ) ;
#65074 = CARTESIAN_POINT ( 'NONE',  ( 19.74164504280149757, 1455.376031929259852, 226.0788368184279875 ) ) ;
#65073 = CARTESIAN_POINT ( 'NONE',  ( -20.59664500270120158, 1507.763472350329948, 190.3621299389660066 ) ) ;
#65075 = CARTESIAN_POINT ( 'NONE',  ( -2.284053509485000077, 1516.854133554269993, 210.2586600040969813 ) ) ;
#65076 = EDGE_CURVE ( 'NONE', #63057, #1893, #94643, .T. ) ;
#65077 = CARTESIAN_POINT ( 'NONE',  ( -25.55040591486629964, 1450.975945474709988, 137.0378106854079761 ) ) ;
#65078 = CARTESIAN_POINT ( 'NONE',  ( -10.81518740880000173, 1424.921099675630103, 144.1705347732979874 ) ) ;
#65079 = CARTESIAN_POINT ( 'NONE',  ( -14.37112480107839829, 1379.718463779069907, 208.2713378727540032 ) ) ;
#65080 = CARTESIAN_POINT ( 'NONE',  ( 11.13185944637359803, 1480.405602026969973, 211.3596403160480008 ) ) ;
#65081 = DIRECTION ( 'NONE',  ( 1.000000000000000000, 0.000000000000000000, 0.000000000000000000 ) ) ;
#65082 = EDGE_CURVE ( 'NONE', #74525, #110178, #69291, .T. ) ;
#65083 = CARTESIAN_POINT ( 'NONE',  ( 35.35021333609370231, 1451.550776711799926, 134.0999999984329918 ) ) ;
#65084 = CARTESIAN_POINT ( 'NONE',  ( -39.71338550447469373, 1440.957585935580028, 136.8228776063639884 ) ) ;
#65085 = VERTEX_POINT ( 'NONE', #33059 ) ;
#65086 = CARTESIAN_POINT ( 'NONE',  ( 4.803830733223059646, 1471.771524698999883, 187.6888356675239891 ) ) ;
#65087 = CARTESIAN_POINT ( 'NONE',  ( -16.36071930985236023, 1410.862894828049775, 226.6398529266253945 ) ) ;
#65088 = ORIENTED_EDGE ( 'NONE', *, *, #93993, .F. ) ;
#65089 = VERTEX_POINT ( 'NONE', #67247 ) ;
#65090 = EDGE_CURVE ( 'NONE', #42516, #55064, #99078, .T. ) ;
#65091 = AXIS2_PLACEMENT_3D ( 'NONE', #7903, #42074, #25239 ) ;
#65092 = CARTESIAN_POINT ( 'NONE',  ( 14.74339714404158386, 1410.800272255869004, 227.6397578307206970 ) ) ;
#65093 = DIRECTION ( 'NONE',  ( -0.02616798426500960631, 0.9993150019883683122, -0.02616798426500990815 ) ) ;
#65094 = CARTESIAN_POINT ( 'NONE',  ( 0.08037848105579999125, 1450.910253508570122, 181.8884884461979823 ) ) ;
#65095 = CARTESIAN_POINT ( 'NONE',  ( -21.10721348755030036, 1508.551704408389924, 210.4652812066999843 ) ) ;
#65096 = CARTESIAN_POINT ( 'NONE',  ( -2.500000000000000000, 1439.336915393649861, 160.7446411339429915 ) ) ;
#65097 = AXIS2_PLACEMENT_3D ( 'NONE', #107361, #13280, #72146 ) ;
#65098 = CARTESIAN_POINT ( 'NONE',  ( -63.87186265362610982, 1379.736347229807961, 269.9239848820633370 ) ) ;
#65099 = DIRECTION ( 'NONE',  ( -0.9455185755993178454, 0.000000000000000000, 0.3255681544571537578 ) ) ;
#65100 = CARTESIAN_POINT ( 'NONE',  ( -1.520741264619999811, 1487.753241046729954, 231.1621170213979894 ) ) ;
#65101 =( BOUNDED_SURFACE ( )  B_SPLINE_SURFACE ( 1, 2, ( 
 ( #38306, #4710, #64094 ),
 ( #89270, #29902, #73032 ) ),
 .UNSPECIFIED., .F., .F., .F. ) 
 B_SPLINE_SURFACE_WITH_KNOTS ( ( 2, 2 ),
 ( 3, 3 ),
 ( -10000.00000000000000, 10000.00000000000000 ),
 ( 5.300753508068390296, 6.148747966412170030 ),
 .UNSPECIFIED. ) 
 GEOMETRIC_REPRESENTATION_ITEM ( )  RATIONAL_B_SPLINE_SURFACE ( (
 ( 0.8627701935022100699, 0.8231028658293879641, 0.9541560038375069830),
 ( 0.8627701935022100699, 0.8231028658293879641, 0.9541560038375069830) ) ) 
 REPRESENTATION_ITEM ( '' )  SURFACE ( )  );
#65102 = CARTESIAN_POINT ( 'NONE',  ( 12.50239388149999975, 1416.520646107730045, 196.1087965155979873 ) ) ;
#65103 = CARTESIAN_POINT ( 'NONE',  ( -74.21209275916879733, 1384.762929623529999, 274.0793104329180210 ) ) ;
#65104 = ORIENTED_EDGE ( 'NONE', *, *, #85947, .F. ) ;
#65105 = CARTESIAN_POINT ( 'NONE',  ( 4.035536225084999984, 1517.086065052259983, 201.3983658527070020 ) ) ;
#65106 = CARTESIAN_POINT ( 'NONE',  ( 2.480427254505000345, 1516.872851364150165, 208.3639601402670110 ) ) ;
#65107 = ORIENTED_EDGE ( 'NONE', *, *, #26227, .F. ) ;
#65108 = CARTESIAN_POINT ( 'NONE',  ( 11.01884469525210086, 1414.913527275050001, 222.3009101210830067 ) ) ;
#65109 = CARTESIAN_POINT ( 'NONE',  ( -0.0002367882524984884097, 1452.632826069514067, 153.4248884296770825 ) ) ;
#65110 = ORIENTED_EDGE ( 'NONE', *, *, #25126, .T. ) ;
#65111 = CARTESIAN_POINT ( 'NONE',  ( -0.1807640977892359946, 1452.343039199269924, 183.2709366604759964 ) ) ;
#65112 = EDGE_CURVE ( 'NONE', #60117, #68958, #22993, .T. ) ;
#65113 = CARTESIAN_POINT ( 'NONE',  ( -14.82206140629999958, 1409.430658177129999, 192.2978730262979923 ) ) ;
#65114 = CYLINDRICAL_SURFACE ( 'NONE', #34962, 1.999999999999999556 ) ;
#65115 = CARTESIAN_POINT ( 'NONE',  ( -19.05930086066416607, 1522.051704408389924, 223.0490131529958262 ) ) ;
#65116 = CARTESIAN_POINT ( 'NONE',  ( -8.281161535991449441, 1436.480211923179922, 214.3424743920830053 ) ) ;
#65117 = CARTESIAN_POINT ( 'NONE',  ( -5.718152507175660482, 1511.533951550999973, 200.6987238893559891 ) ) ;
#65118 = CARTESIAN_POINT ( 'NONE',  ( 45.11781007811134003, 1434.982686472060777, 266.2041965797337753 ) ) ;
#65119 = DIRECTION ( 'NONE',  ( 0.6709778558543747495, 0.000000000000000000, 0.7414773880254650340 ) ) ;
#65120 = CARTESIAN_POINT ( 'NONE',  ( -19.37374569213963227, 1526.382868172863937, 183.8768763279542213 ) ) ;
#65122 = CARTESIAN_POINT ( 'NONE',  ( -11.60004869883236900, 1424.991221944704876, 137.7502973972462712 ) ) ;
#65121 = CARTESIAN_POINT ( 'NONE',  ( 15.80576098240000071, 1459.642315333929901, 231.7528682457979983 ) ) ;
#65123 = CARTESIAN_POINT ( 'NONE',  ( -4.999961604102280077, 1422.677871151950740, 184.8425649944229576 ) ) ;
#65124 = AXIS2_PLACEMENT_3D ( 'NONE', #91084, #6537, #47995 ) ;
#65125 = CARTESIAN_POINT ( 'NONE',  ( -1.710012758625000018, 1517.232977404109988, 216.8491730849570160 ) ) ;
#65126 = CARTESIAN_POINT ( 'NONE',  ( -7.405436629479999588, 1451.940595730289942, 201.5764829818989767 ) ) ;
#65127 = CARTESIAN_POINT ( 'NONE',  ( -0.1099879671840549994, 1508.188471773840092, 180.5321450717350160 ) ) ;
#65128 = CARTESIAN_POINT ( 'NONE',  ( 16.68655976294136423, 1449.426786541504725, 219.0859720786843354 ) ) ;
#65129 = CARTESIAN_POINT ( 'NONE',  ( 4.622842844184999578, 1516.901952101700090, 213.1523604828169880 ) ) ;
#65130 = CARTESIAN_POINT ( 'NONE',  ( 18.57349583820000305, 1508.241272126429976, 188.5096420841980205 ) ) ;
#65131 = CARTESIAN_POINT ( 'NONE',  ( -11.60004869885203682, 1426.235585318013136, 138.1668353689006778 ) ) ;
#65133 = ORIENTED_EDGE ( 'NONE', *, *, #7569, .T. ) ;
#65132 = FACE_OUTER_BOUND ( 'NONE', #109991, .T. ) ;
#65134 = CARTESIAN_POINT ( 'NONE',  ( -18.87980335319999625, 1507.654596516530091, 229.6982590054979880 ) ) ;
#65135 = CARTESIAN_POINT ( 'NONE',  ( 2.245848864970000136, 1508.551704888590166, 219.9346363045989960 ) ) ;
#65136 = CARTESIAN_POINT ( 'NONE',  ( -11.84293662189999807, 1430.740907695629858, 149.7515331920980088 ) ) ;
#65137 = CARTESIAN_POINT ( 'NONE',  ( -1.845809110569999856, 1431.027514053989762, 214.5308736330090085 ) ) ;
#65138 = CARTESIAN_POINT ( 'NONE',  ( -4.227481132736940594, 1441.218242348629929, 201.3833600324580289 ) ) ;
#65139 = CARTESIAN_POINT ( 'NONE',  ( 9.364590546472930654, 1429.570614365610027, 153.1245137695219967 ) ) ;
#65140 = CARTESIAN_POINT ( 'NONE',  ( 7.682163124739999738, 1421.658071144350060, 195.7645034974990210 ) ) ;
#65141 = CARTESIAN_POINT ( 'NONE',  ( -18.26024740272439928, 1443.256143005099830, 213.5656067199900008 ) ) ;
#65142 = EDGE_CURVE ( 'NONE', #106529, #74589, #99027, .T. ) ;
#65144 = CARTESIAN_POINT ( 'NONE',  ( -14.30379464810000023, 1503.190943967589874, 209.1271418435919998 ) ) ;
#65143 = CARTESIAN_POINT ( 'NONE',  ( -18.98990496860000121, 1457.449620047930011, 226.8627260498979865 ) ) ;
#65145 = CARTESIAN_POINT ( 'NONE',  ( -2.646145475300000438, 1485.849692937330019, 182.4222346857980313 ) ) ;
#65146 = ORIENTED_EDGE ( 'NONE', *, *, #45919, .T. ) ;
#65147 = CARTESIAN_POINT ( 'NONE',  ( 6.936398355645000180, 1516.667393516340098, 205.0850970932970085 ) ) ;
#65148 = CARTESIAN_POINT ( 'NONE',  ( 9.934322565360000468, 1406.490945014630142, 267.8131979194979522 ) ) ;
#65149 = EDGE_CURVE ( 'NONE', #20110, #102270, #73236, .T. ) ;
#65150 = CARTESIAN_POINT ( 'NONE',  ( 38.64250925720489960, 1443.812098352220119, 137.1879208744120149 ) ) ;
#65151 = DIRECTION ( 'NONE',  ( 0.9942586961433758086, -0.000000000000000000, 0.1070030146457303932 ) ) ;
#65152 = CARTESIAN_POINT ( 'NONE',  ( 24.24851111099502177, 1436.811212231015816, 213.2345827942206427 ) ) ;
#65153 = CARTESIAN_POINT ( 'NONE',  ( 2.587518041203992425, 1464.354613572267681, 199.6306109175279460 ) ) ;
#65154 = CARTESIAN_POINT ( 'NONE',  ( 11.60004869885203682, 1422.719466699653367, 136.9994304497845405 ) ) ;
#65155 = EDGE_CURVE ( 'NONE', #47913, #27899, #23967, .T. ) ;
#65156 = CARTESIAN_POINT ( 'NONE',  ( -1.469498567789999877, 1450.684669993949910, 155.6080925168980116 ) ) ;
#65157 = CARTESIAN_POINT ( 'NONE',  ( -5.881379503709999845, 1428.766218426890191, 203.1321793329989873 ) ) ;
#65158 = CARTESIAN_POINT ( 'NONE',  ( 2.437740546411169884, 1449.518193510780065, 155.3362082612889878 ) ) ;
#65159 = CARTESIAN_POINT ( 'NONE',  ( 2.359533070475779804E-16, 1517.051704408389924, 209.1218459616989946 ) ) ;
#65160 = CARTESIAN_POINT ( 'NONE',  ( -12.48995958559999941, 1501.883328862989856, 211.6213070104490157 ) ) ;
#65161 = CARTESIAN_POINT ( 'NONE',  ( -16.86383896459999931, 1416.370072266829993, 262.6648722463980334 ) ) ;
#65162 = TOROIDAL_SURFACE ( 'NONE', #18606, 2.000000000000000000, 1.000000000000000000 ) ;
#65163 = CARTESIAN_POINT ( 'NONE',  ( 20.00300104875735485, 1507.847453148246132, 229.0979941101246595 ) ) ;
#65164 = CARTESIAN_POINT ( 'NONE',  ( 2.500000000000000000, 1439.162612134750134, 158.2752953368980116 ) ) ;
#65165 = CARTESIAN_POINT ( 'NONE',  ( -6.157771320920000235, 1475.261075526229888, 269.2805908171979468 ) ) ;
#65166 = DIRECTION ( 'NONE',  ( -0.7071067811865475727, 0.000000000000000000, 0.7071067811865475727 ) ) ;
#65167 = CARTESIAN_POINT ( 'NONE',  ( 10.13545575494789830, 1453.511789163979984, 212.2748783515349942 ) ) ;
#65168 = ADVANCED_FACE ( 'NONE', ( #84017 ), #31302, .F. ) ;
#65169 = CARTESIAN_POINT ( 'NONE',  ( 17.95365621164559755, 1414.298405984240162, 223.3003528621370037 ) ) ;
#65170 = CARTESIAN_POINT ( 'NONE',  ( -26.41820922019849860, 1384.841236826930071, 224.7638030708410213 ) ) ;
#65171 = CARTESIAN_POINT ( 'NONE',  ( -31.26701538686457127, 1523.919934424249959, 221.8945625893618683 ) ) ;
#65172 = AXIS2_PLACEMENT_3D ( 'NONE', #21356, #22453, #63430 ) ;
#65173 = CARTESIAN_POINT ( 'NONE',  ( 12.23023785385239925, 1416.449138228889979, 223.5409194945380023 ) ) ;
#65174 = B_SPLINE_SURFACE_WITH_KNOTS ( 'NONE', 5, 1, ( 
 ( #28192, #54533 ),
 ( #79718, #89200 ),
 ( #71344, #99630 ),
 ( #14532, #53985 ),
 ( #22918, #19784 ),
 ( #62952, #105458 ) ),
 .UNSPECIFIED., .F., .F., .F.,
 ( 6, 6 ),
 ( 2, 2 ),
 ( 0.000000000000000000, 3.689078941800000067 ),
 ( 0.000000000000000000, 14.00000000000000000 ),
 .UNSPECIFIED. ) ;
#65175 = CARTESIAN_POINT ( 'NONE',  ( 12.07900496321360073, 1491.418085619319982, 206.8679904804870091 ) ) ;
#65176 = FACE_OUTER_BOUND ( 'NONE', #84001, .T. ) ;
#65177 = CARTESIAN_POINT ( 'NONE',  ( 25.23672735205020956, 1509.794346327565336, 195.3594086562886787 ) ) ;
#65178 = ADVANCED_FACE ( 'NONE', ( #59951 ), #14314, .T. ) ;
#65179 = CARTESIAN_POINT ( 'NONE',  ( -21.29937734410000161, 1409.656851037430215, 203.0292493083479712 ) ) ;
#65180 = EDGE_CURVE ( 'NONE', #50505, #92786, #23888, .T. ) ;
#65181 = CARTESIAN_POINT ( 'NONE',  ( -15.08147747143999950, 1422.395625179872013, 228.4054715315770068 ) ) ;
#65182 = CARTESIAN_POINT ( 'NONE',  ( 19.43004901905829840, 1455.649281546792963, 225.6093494351993058 ) ) ;
#65183 = ORIENTED_EDGE ( 'NONE', *, *, #3636, .T. ) ;
#65184 = B_SPLINE_SURFACE_WITH_KNOTS ( 'NONE', 5, 5, ( 
 ( #41690, #268, #60163, #79728, #20887, #69690, #61294, #71357, #87001 ),
 ( #104357, #3585, #54544, #3037, #45587, #87575, #10289, #88129, #1927 ),
 ( #89212, #18676, #97073, #10862, #44467, #88677, #11955, #45035, #96515 ),
 ( #46141, #36065, #71910, #105471, #52872, #78611, #95412, #11418, #106026 ),
 ( #70250, #37709, #103810, #79180, #95960, #19794, #27109, #70804, #62962 ),
 ( #80270, #12507, #62391, #28758, #27654, #28203, #61840, #53996, #29301 ) ),
 .UNSPECIFIED., .F., .F., .F.,
 ( 6, 6 ),
 ( 6, 3, 6 ),
 ( 4.238752792101460720, 5.659133035218539831 ),
 ( 0.000000000000000000, 0.5000000000000000000, 1.002061266618540003 ),
 .UNSPECIFIED. ) ;
#65185 = CARTESIAN_POINT ( 'NONE',  ( -3.018679138473939094, 1410.395947885577925, 232.5197392892935397 ) ) ;
#65186 = CARTESIAN_POINT ( 'NONE',  ( -7.544470660387704974, 1510.539524133948362, 214.8487628643081848 ) ) ;
#65187 = CARTESIAN_POINT ( 'NONE',  ( -9.609620985028570317, 1464.248423674519927, 228.1966035519590150 ) ) ;
#65189 = CARTESIAN_POINT ( 'NONE',  ( -11.65415826906500030, 1512.679339245399888, 192.6383097548670094 ) ) ;
#65188 = CARTESIAN_POINT ( 'NONE',  ( 11.62665903299999925, 1425.870842608729845, 143.4637069816980102 ) ) ;
#65190 = CARTESIAN_POINT ( 'NONE',  ( 16.64711227027034113, 1523.843271061947917, 237.7438619119893133 ) ) ;
#65191 = CARTESIAN_POINT ( 'NONE',  ( -4.944749881069999908, 1455.119008683790071, 201.0836254654890070 ) ) ;
#65192 = EDGE_CURVE ( 'NONE', #59762, #98761, #103577, .T. ) ;
#65193 = CARTESIAN_POINT ( 'NONE',  ( 5.778372563615000068, 1516.932669162149978, 202.1763558832970205 ) ) ;
#65194 = CARTESIAN_POINT ( 'NONE',  ( 7.786818409689999498, 1426.121526212180015, 211.8122417738590002 ) ) ;
#65195 = CARTESIAN_POINT ( 'NONE',  ( -4.852453529149999945, 1427.440084250629980, 147.7756948909979826 ) ) ;
#65196 = CARTESIAN_POINT ( 'NONE',  ( 16.30040990573499826, 1513.841826332629807, 194.4616504171669931 ) ) ;
#65197 = CARTESIAN_POINT ( 'NONE',  ( -19.06854921284269722, 1419.167091098079936, 205.9066248690829752 ) ) ;
#65198 = CARTESIAN_POINT ( 'NONE',  ( -44.32308149723269963, 1380.083786705709826, 232.1686127967639948 ) ) ;
#65199 = CARTESIAN_POINT ( 'NONE',  ( 7.001358796384309358, 1367.037625826739713, 207.6218459616988241 ) ) ;
#65200 = EDGE_CURVE ( 'NONE', #14800, #70574, #96049, .T. ) ;
#65202 = ORIENTED_EDGE ( 'NONE', *, *, #41297, .F. ) ;
#65201 = CARTESIAN_POINT ( 'NONE',  ( 9.609447197979999800, 1453.954725363390025, 213.7354802858189942 ) ) ;
#65203 = ORIENTED_EDGE ( 'NONE', *, *, #7195, .F. ) ;
#65204 = CARTESIAN_POINT ( 'NONE',  ( -11.13078726520000039, 1396.479398862830067, 203.7609886355280082 ) ) ;
#65205 = CARTESIAN_POINT ( 'NONE',  ( -22.00494421760000208, 1410.601295256730054, 214.9637058440179942 ) ) ;
#65206 = CARTESIAN_POINT ( 'NONE',  ( -1.556370157619999972, 1414.996444526030018, 226.5294865527980051 ) ) ;
#65207 = CARTESIAN_POINT ( 'NONE',  ( -13.02693512829444700, 1444.857299289932826, 169.4172639506946325 ) ) ;
#65208 = CARTESIAN_POINT ( 'NONE',  ( 15.93623140273500027, 1515.958428328729951, 224.2983129015669874 ) ) ;
#65209 = CARTESIAN_POINT ( 'NONE',  ( -7.599227183775000505, 1512.341036949130057, 211.3567686190669974 ) ) ;
#65211 = FACE_OUTER_BOUND ( 'NONE', #77206, .T. ) ;
#65210 = CYLINDRICAL_SURFACE ( 'NONE', #103250, 1.999999999999982014 ) ;
#65212 = AXIS2_PLACEMENT_3D ( 'NONE', #17138, #51328, #13164 ) ;
#65213 = CARTESIAN_POINT ( 'NONE',  ( 4.204230650730000463, 1410.300354822230247, 186.1030492174980111 ) ) ;
#65214 = CARTESIAN_POINT ( 'NONE',  ( -11.74107623939999989, 1415.088275290029969, 195.6245027881980150 ) ) ;
#65215 = CARTESIAN_POINT ( 'NONE',  ( -40.18287292922800447, 1445.042548787329906, 136.9561948773950064 ) ) ;
#65217 = ADVANCED_FACE ( 'NONE', ( #72749 ), #47004, .T. ) ;
#65216 = CARTESIAN_POINT ( 'NONE',  ( 10.37381255510450018, 1396.275321906710133, 205.2617250521719825 ) ) ;
#65218 = CARTESIAN_POINT ( 'NONE',  ( 33.29224916083880004, 1436.556216818010171, 136.5296164106590027 ) ) ;
#65219 = CARTESIAN_POINT ( 'NONE',  ( 10.84999101200000204, 1425.206555810429791, 146.9406714080979839 ) ) ;
#65220 = CARTESIAN_POINT ( 'NONE',  ( 8.502796018205000195, 1512.371933174390051, 202.2779677156470086 ) ) ;
#65221 = ORIENTED_EDGE ( 'NONE', *, *, #43723, .T. ) ;
#65222 = CARTESIAN_POINT ( 'NONE',  ( 3.827442175440000316, 1424.287716995130040, 184.6276801873979991 ) ) ;
#65223 = CARTESIAN_POINT ( 'NONE',  ( 21.51513853577893798, 1524.871836253796118, 234.5521809742263883 ) ) ;
#65224 = ORIENTED_EDGE ( 'NONE', *, *, #8810, .T. ) ;
#65225 = ADVANCED_FACE ( 'NONE', ( #96289 ), #81340, .T. ) ;
#65226 = ORIENTED_EDGE ( 'NONE', *, *, #85613, .T. ) ;
#65227 = CARTESIAN_POINT ( 'NONE',  ( -5.004100793020000104, 1425.392060909700149, 209.0067307068910054 ) ) ;
#65228 = CARTESIAN_POINT ( 'NONE',  ( -109.9855944279999989, 1384.926148861439970, 311.4562326602589906 ) ) ;
#65229 = DIRECTION ( 'NONE',  ( 1.755985294532469921E-16, -1.000000000000000000, 1.338183447452831989E-16 ) ) ;
#65230 = CARTESIAN_POINT ( 'NONE',  ( 1.130002494264999990, 1516.621991115350056, 216.0576472317669925 ) ) ;
#65231 = CARTESIAN_POINT ( 'NONE',  ( -12.31856220172990035, 1378.316865691869907, 209.5864139505719947 ) ) ;
#65232 = EDGE_CURVE ( 'NONE', #66863, #12979, #78956, .T. ) ;
#65233 = ORIENTED_EDGE ( 'NONE', *, *, #65365, .T. ) ;
#65234 = DIRECTION ( 'NONE',  ( 1.000000000000000000, 0.000000000000000000, 0.000000000000000000 ) ) ;
#65235 = CARTESIAN_POINT ( 'NONE',  ( -11.79167011069929849, 1509.456730339710020, 181.3501055891659917 ) ) ;
#65236 = CARTESIAN_POINT ( 'NONE',  ( -37.01195473260000313, 1375.480374498559968, 219.4187096247589750 ) ) ;
#65237 = CARTESIAN_POINT ( 'NONE',  ( 0.3610880125729999390, 1416.520646107730045, 227.1639889635980296 ) ) ;
#65238 = CARTESIAN_POINT ( 'NONE',  ( -0.7574260232259989456, 1516.837969789639828, 205.8660360680970030 ) ) ;
#65239 = VERTEX_POINT ( 'NONE', #2807 ) ;
#65240 = CARTESIAN_POINT ( 'NONE',  ( -2.286472924554999953, 1516.883361325900069, 209.8798303522490016 ) ) ;
#65241 = CARTESIAN_POINT ( 'NONE',  ( -20.07643676080000006, 1508.105275053929972, 229.0283142729980170 ) ) ;
#65242 = CARTESIAN_POINT ( 'NONE',  ( -25.36365838169201226, 1416.527675838791311, 269.4265581229172994 ) ) ;
#65243 = CARTESIAN_POINT ( 'NONE',  ( -1.241688091069999889, 1409.462072764129971, 232.7892660792980166 ) ) ;
#65245 = VERTEX_POINT ( 'NONE', #88981 ) ;
#65244 = CARTESIAN_POINT ( 'NONE',  ( -12.45610846519999981, 1519.913060387329779, 189.3614993990980224 ) ) ;
#65246 = CARTESIAN_POINT ( 'NONE',  ( -0.01303797444059440029, 1452.990214026840022, 183.2388976015689934 ) ) ;
#65247 = CARTESIAN_POINT ( 'NONE',  ( -28.56580625744389934, 1440.913060387279984, 233.3672108470599937 ) ) ;
#65248 = AXIS2_PLACEMENT_3D ( 'NONE', #94021, #53723, #69969 ) ;
#65249 = CARTESIAN_POINT ( 'NONE',  ( -38.49941284300000177, 1384.470821939250072, 239.3076530171589980 ) ) ;
#65250 = CARTESIAN_POINT ( 'NONE',  ( -0.3216917231897860052, 1465.013453958230002, 237.3752535225130202 ) ) ;
#65251 = CARTESIAN_POINT ( 'NONE',  ( 6.266567495659089992, 1410.110873601029880, 270.0731530804650333 ) ) ;
#65252 = VECTOR ( 'NONE', #22521, 1000.000000000000000 ) ;
#65253 = CARTESIAN_POINT ( 'NONE',  ( -6.936398393775000670, 1516.667393516340098, 213.1585948090369698 ) ) ;
#65254 = CARTESIAN_POINT ( 'NONE',  ( -62.92787051930000075, 1379.731629237049901, 267.9834126184589991 ) ) ;
#65255 = VECTOR ( 'NONE', #15805, 1000.000000000000000 ) ;
#65256 = CARTESIAN_POINT ( 'NONE',  ( 23.86480761299999998, 1410.397258296229893, 208.6144169840580105 ) ) ;
#65257 = ADVANCED_FACE ( 'NONE', ( #3908 ), #83059, .T. ) ;
#65258 = CARTESIAN_POINT ( 'NONE',  ( 28.54794148641478913, 1526.382868172864164, 198.4382598900853623 ) ) ;
#65259 = CARTESIAN_POINT ( 'NONE',  ( 12.31397506763359928, 1492.288124162400209, 209.9699710670110164 ) ) ;
#65260 = CARTESIAN_POINT ( 'NONE',  ( -7.709227547919620172, 1516.541781377989992, 210.8861241254419951 ) ) ;
#65261 = CARTESIAN_POINT ( 'NONE',  ( 7.727327114725000001, 1517.232977404109988, 210.8318586907270173 ) ) ;
#65263 = EDGE_CURVE ( 'NONE', #33852, #103208, #41313, .T. ) ;
#65262 = CARTESIAN_POINT ( 'NONE',  ( -107.2061239200703824, 1391.913060387192672, 300.7511740610627839 ) ) ;
#65264 = CARTESIAN_POINT ( 'NONE',  ( -7.217374241420609238, 1424.786834349990158, 212.8040540257917712 ) ) ;
#65265 = CARTESIAN_POINT ( 'NONE',  ( 11.86965601189266728, 1423.326342551363041, 137.0999999980981272 ) ) ;
#65267 = ORIENTED_EDGE ( 'NONE', *, *, #100041, .T. ) ;
#65266 = CARTESIAN_POINT ( 'NONE',  ( -25.90890198950000212, 1386.624726539740095, 203.4658880710290134 ) ) ;
#65268 = CARTESIAN_POINT ( 'NONE',  ( -38.23615600544859916, 1385.191880958569982, 239.1136682615309894 ) ) ;
#65269 = CARTESIAN_POINT ( 'NONE',  ( 18.96298731639999602, 1416.825532216530064, 210.2431968665279953 ) ) ;
#65270 = LINE ( 'NONE', #15919, #98570 ) ;
#65271 = CARTESIAN_POINT ( 'NONE',  ( 5.826428076080000906, 1473.811884028689974, 218.9454251420289950 ) ) ;
#65272 = CARTESIAN_POINT ( 'NONE',  ( 11.06028399019999853, 1425.506596454839837, 205.4898845224990112 ) ) ;
#65273 = CARTESIAN_POINT ( 'NONE',  ( -1.700022450220517012, 1497.975818191871895, 197.9538752838212474 ) ) ;
#65274 = EDGE_CURVE ( 'NONE', #50057, #73846, #9764, .T. ) ;
#65276 = FACE_OUTER_BOUND ( 'NONE', #75842, .T. ) ;
#65275 = CARTESIAN_POINT ( 'NONE',  ( -7.716878941104999612, 1516.833976295079992, 216.4517711926369827 ) ) ;
#65277 = DIRECTION ( 'NONE',  ( 0.000000000000000000, 1.000000000000000000, 0.000000000000000000 ) ) ;
#65278 = CARTESIAN_POINT ( 'NONE',  ( 30.29630067237538071, 1526.329757971584968, 221.7900933993806802 ) ) ;
#65279 = ORIENTED_EDGE ( 'NONE', *, *, #68769, .T. ) ;
#65280 = CARTESIAN_POINT ( 'NONE',  ( 5.003220727074999985, 1516.983995446890049, 202.1750974131470286 ) ) ;
#65281 = CARTESIAN_POINT ( 'NONE',  ( 10.14133495641580041, 1480.626569447219936, 206.2493899992390141 ) ) ;
#65282 = VERTEX_POINT ( 'NONE', #70566 ) ;
#65283 = DIRECTION ( 'NONE',  ( -0.000000000000000000, -1.000000000000000000, -0.000000000000000000 ) ) ;
#65284 = CARTESIAN_POINT ( 'NONE',  ( 24.35915060720000014, 1445.179795648890149, 214.1348656310980232 ) ) ;
#65285 = CARTESIAN_POINT ( 'NONE',  ( 7.873429467257136771, 1438.236320869735664, 153.7470637502197519 ) ) ;
#65286 = CARTESIAN_POINT ( 'NONE',  ( 8.159522702327139498, 1511.384172056590160, 203.7268068870999969 ) ) ;
#65287 = CARTESIAN_POINT ( 'NONE',  ( 2.852546465570000134, 1442.789416142390110, 217.5399594921489950 ) ) ;
#65288 = CARTESIAN_POINT ( 'NONE',  ( -26.63926297338899829, 1508.969960717049844, 201.4257229170909795 ) ) ;
#65289 = EDGE_CURVE ( 'NONE', #60628, #94097, #88444, .T. ) ;
#65290 = CARTESIAN_POINT ( 'NONE',  ( -2.500000004229999906, 1447.770735518889978, 162.7884840773980102 ) ) ;
#65291 = CARTESIAN_POINT ( 'NONE',  ( -19.05289845549999939, 1425.496478449930009, 224.1872183716980089 ) ) ;
#65292 = CARTESIAN_POINT ( 'NONE',  ( -24.92720726409999799, 1436.178261884299900, 137.8894286862980039 ) ) ;
#65293 = CARTESIAN_POINT ( 'NONE',  ( -107.2861855960000099, 1387.769792023699893, 298.2427032543589576 ) ) ;
#65294 = CARTESIAN_POINT ( 'NONE',  ( 19.64936965250000256, 1498.079962482629981, 189.3459704154979875 ) ) ;
#65295 = CARTESIAN_POINT ( 'NONE',  ( -7.512750246095000861, 1509.038615934239942, 209.1218459511669892 ) ) ;
#65296 = AXIS2_PLACEMENT_3D ( 'NONE', #48274, #66188, #82418 ) ;
#65297 = CARTESIAN_POINT ( 'NONE',  ( 26.79413740735880367, 1436.761939593030093, 136.7822073642480234 ) ) ;
#65298 = VERTEX_POINT ( 'NONE', #81127 ) ;
#65300 = ADVANCED_FACE ( 'NONE', ( #4445 ), #72428, .F. ) ;
#65299 = DIRECTION ( 'NONE',  ( -1.755985294532469921E-16, 1.000000000000000000, -1.338183447452831989E-16 ) ) ;
#65301 = DIRECTION ( 'NONE',  ( -0.000000000000000000, -1.000000000000000000, -0.000000000000000000 ) ) ;
#65302 = CARTESIAN_POINT ( 'NONE',  ( 11.19147557906589974, 1422.145537183640045, 210.4506353095700035 ) ) ;
#65303 = CARTESIAN_POINT ( 'NONE',  ( -113.4000000000000057, 1378.813060387289852, 304.2218459572590064 ) ) ;
#65304 = CARTESIAN_POINT ( 'NONE',  ( -0.1245423319220000102, 1416.981664566430027, 234.1917870246980158 ) ) ;
#65305 = CARTESIAN_POINT ( 'NONE',  ( -13.44509113387912613, 1444.312623396357594, 186.9757151702101794 ) ) ;
#65306 = B_SPLINE_SURFACE_WITH_KNOTS ( 'NONE', 3, 5, ( 
 ( #13395, #83368, #6113, #74454, #65499, #6669 ),
 ( #108582, #75000, #109150, #106918, #32434, #107469 ),
 ( #55989, #5013, #99060, #56539, #90667, #13951 ),
 ( #48140, #59312, #49794, #51437, #50893, #51999 ) ),
 .UNSPECIFIED., .F., .F., .F.,
 ( 4, 4 ),
 ( 6, 6 ),
 ( 5.479561967589999583, 5.505632813710000129 ),
 ( 0.000000000000000000, 1.000000000000000000 ),
 .UNSPECIFIED. ) ;
#65307 = CARTESIAN_POINT ( 'NONE',  ( -8.756504656448949930, 1437.746547805949831, 210.1047563292509892 ) ) ;
#65308 = CARTESIAN_POINT ( 'NONE',  ( 7.499999980934999755, 1508.551704408389924, 209.1218459511669892 ) ) ;
#65309 = CARTESIAN_POINT ( 'NONE',  ( 12.53380499174499896, 1442.773887286369927, 169.4755105688890069 ) ) ;
#65310 = CARTESIAN_POINT ( 'NONE',  ( -105.2320395018850121, 1383.760598056300068, 311.0135867326180232 ) ) ;
#65311 = DIRECTION ( 'NONE',  ( 0.9417419115949053898, -0.3363363969979660806, 0.000000000000000000 ) ) ;
#65312 = CARTESIAN_POINT ( 'NONE',  ( -13.17497928872374402, 1443.091744202487234, 169.3947364813658680 ) ) ;
#65315 = ORIENTED_EDGE ( 'NONE', *, *, #85746, .T. ) ;
#65314 = CARTESIAN_POINT ( 'NONE',  ( -14.44229636320000054, 1409.585625700530045, 226.2125909719979973 ) ) ;
#65313 = B_SPLINE_CURVE_WITH_KNOTS ( 'NONE', 3,
 ( #90296, #13029, #81897, #38796, #73531, #98708, #65677, #39357, #13576, #72971, #31496, #56719 ),
 .UNSPECIFIED., .F., .F.,
 ( 4, 2, 1, 1, 2, 2, 4 ),
 ( 0.000000000000000000, 0.2499999999996412869, 0.3749999999994620414, 0.4374999999993723909, 0.4687499999993651745, 0.4999999999993579580, 1.000000000000000000 ),
 .UNSPECIFIED. ) ;
#65316 = B_SPLINE_CURVE_WITH_KNOTS ( 'NONE', 5,
 ( #48604, #58104, #62824, #83835, #97476, #14959 ),
 .UNSPECIFIED., .F., .F.,
 ( 6, 6 ),
 ( 0.000000000000000000, 1.000000000000000000 ),
 .UNSPECIFIED. ) ;
#65317 = CARTESIAN_POINT ( 'NONE',  ( -106.7756679679999934, 1383.435927837959980, 297.1269841571589723 ) ) ;
#65318 = EDGE_CURVE ( 'NONE', #75143, #103585, #835, .T. ) ;
#65319 = CARTESIAN_POINT ( 'NONE',  ( 15.01814799273499901, 1514.214451716350140, 223.8476172842669882 ) ) ;
#65320 = ORIENTED_EDGE ( 'NONE', *, *, #30388, .T. ) ;
#65321 = ORIENTED_EDGE ( 'NONE', *, *, #103887, .F. ) ;
#65322 = DIRECTION ( 'NONE',  ( 0.000000000000000000, 0.000000000000000000, 1.000000000000000000 ) ) ;
#65323 = CARTESIAN_POINT ( 'NONE',  ( -19.92151515271962126, 1526.208281990536307, 233.5199663060418516 ) ) ;
#65325 = CARTESIAN_POINT ( 'NONE',  ( -5.442004251730000242, 1468.737548879730184, 250.5651368667980421 ) ) ;
#65324 = CARTESIAN_POINT ( 'NONE',  ( 4.157308324739999783, 1454.950057953289843, 217.7287963511690236 ) ) ;
#65326 = ADVANCED_FACE ( 'NONE', ( #66019 ), #55427, .F. ) ;
#65327 = B_SPLINE_CURVE_WITH_KNOTS ( 'NONE', 3,
 ( #23363, #91676, #40175, #46950, #82170, #73233, #56438, #107376, #30106, #57553, #5470, #109048, #38513, #98421, #55899, #81610, #4914, #30671, #59204, #75980, #59746, #25554, #49696, #32861, #23901, #68167, #9335, #33971, #93322, #16584, #68708, #100616, #86036, #58641, #102274, #93866, #17135, #110132, #109591, #67052, #102812, #24453, #41282, #26106, #76528, #110680, #51324, #16050, #85460, #84914 ),
 .UNSPECIFIED., .F., .F.,
 ( 4, 2, 2, 2, 1, 2, 2, 2, 2, 1, 1, 2, 2, 2, 2, 2, 1, 1, 2, 2, 2, 2, 1, 1, 1, 2, 2, 2, 4 ),
 ( 0.000000000000000000, 0.06250000000014811763, 0.09375000000033439918, 0.1093750000004250211, 0.1171875000004729828, 0.1210937500004969636, 0.1250000000005209444, 0.1874999999982666643, 0.2187499999971440900, 0.2343749999966805442, 0.2421874999963559427, 0.2460937499961080022, 0.2499999999958600894, 0.3749999999961667885, 0.4374999999963201658, 0.4687499999963219977, 0.4843749999963902209, 0.4921874999964880315, 0.4960937499966067699, 0.4999999999967255082, 0.6249999999975833775, 0.6874999999980123677, 0.7187499999982158716, 0.7343749999983176791, 0.7421874999983686383, 0.7460937499983835153, 0.7499999999983983923, 0.8749999999991993072, 1.000000000000000000 ),
 .UNSPECIFIED. ) ;
#65328 = CARTESIAN_POINT ( 'NONE',  ( 4.329448776040000446, 1515.064792882589927, 206.7917118356089929 ) ) ;
#65329 = CARTESIAN_POINT ( 'NONE',  ( -11.25663278669999912, 1433.724203657259977, 151.5578573542979939 ) ) ;
#65330 = EDGE_CURVE ( 'NONE', #42405, #39998, #88863, .T. ) ;
#65331 = CARTESIAN_POINT ( 'NONE',  ( -18.19590854888121356, 1512.187213306747481, 238.2026672068777202 ) ) ;
#65332 = CARTESIAN_POINT ( 'NONE',  ( 9.345710454894810226, 1422.635914553260136, 212.8840094578699791 ) ) ;
#65333 = CARTESIAN_POINT ( 'NONE',  ( 16.06428792994640276, 1414.913060387329779, 208.9262477894010033 ) ) ;
#65334 = DIRECTION ( 'NONE',  ( 0.7071067811865474617, 5.170588477393925004E-17, 0.7071067811865474617 ) ) ;
#65335 = CARTESIAN_POINT ( 'NONE',  ( 1.179283247357060027, 1515.094876538340031, 213.4505069693209975 ) ) ;
#65336 = FACE_BOUND ( 'NONE', #100070, .T. ) ;
#65337 = CARTESIAN_POINT ( 'NONE',  ( -7.505040120567149309, 1478.213044889750108, 217.9841396579450077 ) ) ;
#65338 = CARTESIAN_POINT ( 'NONE',  ( 3.127224862021169560, 1362.510123982220193, 208.3718459617061285 ) ) ;
#65339 = EDGE_CURVE ( 'NONE', #38113, #26627, #75819, .T. ) ;
#65340 = CARTESIAN_POINT ( 'NONE',  ( -7.587845399210802810, 1509.305955895972602, 238.1603715047018852 ) ) ;
#65342 = ORIENTED_EDGE ( 'NONE', *, *, #2908, .T. ) ;
#65341 = CARTESIAN_POINT ( 'NONE',  ( 7.547424700377989516E-09, 1409.628684922620096, 259.4492681075740279 ) ) ;
#65343 = ORIENTED_EDGE ( 'NONE', *, *, #9225, .F. ) ;
#65344 = CARTESIAN_POINT ( 'NONE',  ( -11.85978036263550095, 1431.894859516819906, 149.9645931322949934 ) ) ;
#65345 = CIRCLE ( 'NONE', #63668, 11.73448142120001059 ) ;
#65346 = CARTESIAN_POINT ( 'NONE',  ( -21.44822655731880090, 1506.215343320510101, 215.9887031352290023 ) ) ;
#65347 = CARTESIAN_POINT ( 'NONE',  ( -6.238302164579999420, 1471.462343947730005, 269.8685151816979442 ) ) ;
#65348 = CARTESIAN_POINT ( 'NONE',  ( -1.609854712855105952, 1474.055975362519348, 219.2485333660200126 ) ) ;
#65349 = CARTESIAN_POINT ( 'NONE',  ( 3.218260492609999801, 1432.346960983880081, 155.4230413404980027 ) ) ;
#65350 = CARTESIAN_POINT ( 'NONE',  ( 33.92637545789110476, 1451.728355673910073, 135.1498132472949862 ) ) ;
#65351 = CARTESIAN_POINT ( 'NONE',  ( 0.2864299555745510317, 1451.125108261750029, 182.1816743638030118 ) ) ;
#65352 = CARTESIAN_POINT ( 'NONE',  ( -8.372579757359998709, 1384.643036033459794, 199.7849846811289751 ) ) ;
#65353 = CARTESIAN_POINT ( 'NONE',  ( -120.2678896395927666, 1378.913060387290216, 304.3291340586740716 ) ) ;
#65354 = CARTESIAN_POINT ( 'NONE',  ( -3.391530762879999994, 1456.859262623989935, 218.0010147046889983 ) ) ;
#65355 = CARTESIAN_POINT ( 'NONE',  ( 10.70668172122111095, 1366.667713169411172, 210.6218459617030021 ) ) ;
#65356 = CARTESIAN_POINT ( 'NONE',  ( -27.50386026148250096, 1412.567279178109857, 267.5294091190150425 ) ) ;
#65357 = ORIENTED_EDGE ( 'NONE', *, *, #85080, .T. ) ;
#65358 = CARTESIAN_POINT ( 'NONE',  ( -3.543960468857640045, 1501.780698723729984, 181.2047494549660200 ) ) ;
#65359 = EDGE_CURVE ( 'NONE', #22619, #75633, #50853, .T. ) ;
#65360 = EDGE_LOOP ( 'NONE', ( #96782, #48010, #23987, #19596 ) ) ;
#65361 = VERTEX_POINT ( 'NONE', #56781 ) ;
#65362 = CARTESIAN_POINT ( 'NONE',  ( 2.882325979385000014, 1516.969638403840008, 210.8235757905769674 ) ) ;
#65363 = CARTESIAN_POINT ( 'NONE',  ( 4.583195184658291232, 1423.744221409726151, 183.8097901654739985 ) ) ;
#65364 = CARTESIAN_POINT ( 'NONE',  ( 41.39923983940850150, 1444.121112939410068, 136.4829021321949938 ) ) ;
#65365 = EDGE_CURVE ( 'NONE', #59464, #61894, #16839, .T. ) ;
#65367 = SURFACE_STYLE_FILL_AREA ( #64262 ) ;
#65366 = CARTESIAN_POINT ( 'NONE',  ( -2.284526496774999860, 1516.956048353049937, 212.5847947667770086 ) ) ;
#65368 = CARTESIAN_POINT ( 'NONE',  ( -16.22390639470000195, 1455.453005806130022, 189.2659189164979807 ) ) ;
#65369 = CARTESIAN_POINT ( 'NONE',  ( -2.182017354322035807, 1449.976583366785462, 182.9105004910145169 ) ) ;
#65370 = ORIENTED_EDGE ( 'NONE', *, *, #34944, .F. ) ;
#65371 = DIRECTION ( 'NONE',  ( 1.000000000000000000, -0.000000000000000000, -0.000000000000000000 ) ) ;
#65372 = AXIS2_PLACEMENT_3D ( 'NONE', #53597, #4282, #30569 ) ;
#65373 = CARTESIAN_POINT ( 'NONE',  ( 2.483949940595000516, 1517.156142772249950, 202.1710124019969896 ) ) ;
#65374 = CARTESIAN_POINT ( 'NONE',  ( -40.60082915980000706, 1447.775075536270379, 135.1193778666983292 ) ) ;
#65376 = CIRCLE ( 'NONE', #20646, 1.000000000000000888 ) ;
#65375 = CARTESIAN_POINT ( 'NONE',  ( -12.36124149779879922, 1384.516177574450012, 200.2720669086149883 ) ) ;
#65377 = CARTESIAN_POINT ( 'NONE',  ( -42.85030160454469694, 1440.913048488810091, 270.2009464246669950 ) ) ;
#65378 = CARTESIAN_POINT ( 'NONE',  ( -33.36586802512168504, 1512.187213306747481, 216.3367586934473366 ) ) ;
#65379 = CARTESIAN_POINT ( 'NONE',  ( -3.412833957800000206, 1396.032239175229961, 198.2233776492980155 ) ) ;
#65381 = EDGE_LOOP ( 'NONE', ( #65657, #67713, #109060, #108025 ) ) ;
#65380 = CARTESIAN_POINT ( 'NONE',  ( -8.726294317499757369, 1364.539843072939220, 210.6218459617142003 ) ) ;
#65382 = ORIENTED_EDGE ( 'NONE', *, *, #93088, .F. ) ;
#65383 = CARTESIAN_POINT ( 'NONE',  ( 17.84338787571943641, 1512.187213306747481, 237.8836641337660467 ) ) ;
#65384 = CARTESIAN_POINT ( 'NONE',  ( 3.747137648998505544, 1425.479684836872821, 185.1860802519873062 ) ) ;
#65385 = CARTESIAN_POINT ( 'NONE',  ( 21.84020450222037724, 1512.187213306747481, 183.2638850454218016 ) ) ;
#65386 = CARTESIAN_POINT ( 'NONE',  ( -2.500000000000000000, 1419.471702562262180, 139.8968355505663794 ) ) ;
#65387 = CARTESIAN_POINT ( 'NONE',  ( -0.03395478378652629775, 1410.184876381479853, 185.0299449505969847 ) ) ;
#65388 = CARTESIAN_POINT ( 'NONE',  ( 4.045182479925000685, 1517.057265928030120, 210.8256255754569963 ) ) ;
#65389 = CARTESIAN_POINT ( 'NONE',  ( 2.143373558913630461, 1458.476679308760822, 199.7396688924466446 ) ) ;
#65390 = CARTESIAN_POINT ( 'NONE',  ( -17.17241001986462123, 1512.187213306747481, 238.6251415217917895 ) ) ;
#65391 = CARTESIAN_POINT ( 'NONE',  ( 3.962577075963499507, 1441.289921133800135, 217.4194056301390106 ) ) ;
#65392 = CARTESIAN_POINT ( 'NONE',  ( 18.80400139965103889, 1425.877415487390863, 225.3118880953776966 ) ) ;
#65393 = CARTESIAN_POINT ( 'NONE',  ( 8.072094028204999105, 1511.572472350439739, 205.5103833285670021 ) ) ;
#65394 = CARTESIAN_POINT ( 'NONE',  ( -7.726331963605000297, 1517.194972660189933, 206.8303316343270239 ) ) ;
#65395 = ORIENTED_EDGE ( 'NONE', *, *, #174, .T. ) ;
#65396 = CARTESIAN_POINT ( 'NONE',  ( -33.91369114127179785, 1451.728768196330066, 134.7398512173020038 ) ) ;
#65397 = CARTESIAN_POINT ( 'NONE',  ( -10.87812260669999986, 1471.332318691390128, 207.6541763658389925 ) ) ;
#65398 = CARTESIAN_POINT ( 'NONE',  ( -23.50846456196114431, 1448.274227622677017, 215.6832531493611782 ) ) ;
#65399 = ORIENTED_EDGE ( 'NONE', *, *, #42522, .F. ) ;
#65400 = CARTESIAN_POINT ( 'NONE',  ( -17.83486663330464950, 1523.678648413191695, 237.8759530894961074 ) ) ;
#65401 = CARTESIAN_POINT ( 'NONE',  ( 25.07770885454710097, 1451.593447514730087, 137.0505554713550112 ) ) ;
#65402 = CARTESIAN_POINT ( 'NONE',  ( 13.57591587739999994, 1415.063410501330054, 197.7477002572979927 ) ) ;
#65403 = CARTESIAN_POINT ( 'NONE',  ( 4.329448776040000446, 1515.064792882589927, 209.0973262533439936 ) ) ;
#65404 = CARTESIAN_POINT ( 'NONE',  ( -10.85852385830536448, 1424.794007418652882, 138.1924915167475660 ) ) ;
#65405 = CARTESIAN_POINT ( 'NONE',  ( -19.68364361505096483, 1517.051704408389924, 221.2357901429078879 ) ) ;
#65406 = CARTESIAN_POINT ( 'NONE',  ( 10.94557456650000127, 1490.490906152089792, 205.6963937967290121 ) ) ;
#65407 = DIRECTION ( 'NONE',  ( 0.5877852522924820189, 0.000000000000000000, 0.8090169943749410120 ) ) ;
#65408 = CARTESIAN_POINT ( 'NONE',  ( 24.20724779095554879, 1446.232668714965484, 214.6598422090904705 ) ) ;
#65409 = CARTESIAN_POINT ( 'NONE',  ( 2.500000000000079936, 1439.283171039279978, 159.9469904227869961 ) ) ;
#65410 = CARTESIAN_POINT ( 'NONE',  ( 9.682514688702729799, 1436.279831273820037, 210.8541350352949735 ) ) ;
#65411 = CARTESIAN_POINT ( 'NONE',  ( -5.777745433405000242, 1516.908489800550115, 215.6797558528670038 ) ) ;
#65412 = VERTEX_POINT ( 'NONE', #66850 ) ;
#65413 = CARTESIAN_POINT ( 'NONE',  ( -17.70265010310000164, 1417.829914391519878, 206.4711793681690040 ) ) ;
#65414 = CARTESIAN_POINT ( 'NONE',  ( -1.476727087160000007, 1474.160226259529963, 270.1373298219979802 ) ) ;
#65415 = CARTESIAN_POINT ( 'NONE',  ( 15.56469051819999905, 1506.798305132829910, 225.0756798403980099 ) ) ;
#65416 = CARTESIAN_POINT ( 'NONE',  ( -31.23437356469425907, 1518.913060387330006, 222.8968241038848248 ) ) ;
#65417 = CIRCLE ( 'NONE', #13580, 26.99999999999999645 ) ;
#65418 = CARTESIAN_POINT ( 'NONE',  ( 1.247885727509999931, 1474.780154000190123, 220.0763491201989837 ) ) ;
#65419 = CARTESIAN_POINT ( 'NONE',  ( 21.61286264580910199, 1509.680930481669975, 229.7181273278760045 ) ) ;
#65420 = CARTESIAN_POINT ( 'NONE',  ( 11.44767209065952684, 1425.800566880429642, 139.0551406208118124 ) ) ;
#65421 = DIRECTION ( 'NONE',  ( 0.08338001035575019759, 5.083217065477059319E-13, 0.9965178241622549837 ) ) ;
#65422 = CARTESIAN_POINT ( 'NONE',  ( -1.730624838930999942, 1477.776000856039900, 183.0333778651980197 ) ) ;
#65423 = CARTESIAN_POINT ( 'NONE',  ( 0.9489938987924170233, 1456.076817772840059, 198.6004356744230108 ) ) ;
#65424 = DIRECTION ( 'NONE',  ( 9.158755289808628626E-47, -1.000000000000000000, 1.836970198721029688E-16 ) ) ;
#65425 = B_SPLINE_SURFACE_WITH_KNOTS ( 'NONE', 5, 5, ( 
 ( #18542, #67892, #7408, #101439, #58926, #93057 ),
 ( #72298, #37573, #89071, #28065, #106429, #37016 ),
 ( #78480, #36468, #96940, #62254, #96381, #20206 ),
 ( #1793, #38117, #3443, #54406, #35930, #53863 ),
 ( #63898, #88538, #12358, #105331, #61701, #11822 ),
 ( #46546, #45992, #3993, #98013, #63362, #10163 ),
 ( #80680, #27515, #79050, #86870, #44337, #29714 ),
 ( #19659, #70114, #95822, #70665, #80123, #53294 ),
 ( #71774, #52736, #104779, #88000, #71210, #62825 ) ),
 .UNSPECIFIED., .F., .F., .F.,
 ( 6, 3, 6 ),
 ( 6, 6 ),
 ( 0.000000000000000000, 1.710105857910000138, 3.420211715829999832 ),
 ( 0.000000000000000000, 2.000000000000000000 ),
 .UNSPECIFIED. ) ;
#65426 = CARTESIAN_POINT ( 'NONE',  ( 30.55220783223240133, 1440.913060385000108, 240.0655027828689754 ) ) ;
#65428 = CARTESIAN_POINT ( 'NONE',  ( -5.478760788770000723, 1476.176840370589844, 217.9931547433689900 ) ) ;
#65427 = CARTESIAN_POINT ( 'NONE',  ( -9.839102621363029044, 1472.123545760580100, 211.7008534868720062 ) ) ;
#65429 = CARTESIAN_POINT ( 'NONE',  ( 13.02322702449999881, 1416.825784017130218, 221.6328457789979893 ) ) ;
#65430 = VERTEX_POINT ( 'NONE', #51139 ) ;
#65431 = ORIENTED_EDGE ( 'NONE', *, *, #30273, .F. ) ;
#65432 = CARTESIAN_POINT ( 'NONE',  ( 11.23388613411650105, 1443.913060387330006, 207.0699376370760092 ) ) ;
#65433 = DIRECTION ( 'NONE',  ( -3.552713678800500929E-15, 0.000000000000000000, 1.000000000000000000 ) ) ;
#65434 = CARTESIAN_POINT ( 'NONE',  ( -1.620287784100000295, 1443.296048881190018, 200.2316306629689677 ) ) ;
#65435 = CARTESIAN_POINT ( 'NONE',  ( 8.260488040129999376, 1424.458407895899882, 195.8858451325990302 ) ) ;
#65436 = CARTESIAN_POINT ( 'NONE',  ( 1.399926847669999974, 1507.072115598929940, 236.8180522793980174 ) ) ;
#65437 = CARTESIAN_POINT ( 'NONE',  ( -10.81507089441019964, 1424.921187596680056, 144.1620444830689962 ) ) ;
#65438 = CARTESIAN_POINT ( 'NONE',  ( -30.61115703707795177, 1523.542365884050923, 221.8239785241903235 ) ) ;
#65439 = CARTESIAN_POINT ( 'NONE',  ( -42.67632043428780264, 1383.823947953480001, 246.6491155685140200 ) ) ;
#65440 = TOROIDAL_SURFACE ( 'NONE', #13526, 3.500000000000000000, 2.000000000000000000 ) ;
#65441 = CARTESIAN_POINT ( 'NONE',  ( -5.385523199825000162, 1511.435001052829875, 200.4690698299770020 ) ) ;
#65442 = CARTESIAN_POINT ( 'NONE',  ( 2.499944985410900156, 1419.419865434090070, 142.4063531947399781 ) ) ;
#65444 =( BOUNDED_CURVE ( )  B_SPLINE_CURVE ( 3, ( #1029, #86658, #68238, #8284 ),
 .UNSPECIFIED., .F., .F. ) 
 B_SPLINE_CURVE_WITH_KNOTS ( ( 4, 4 ),
 ( 3.097740324398939649, 3.109955547998598746 ),
 .UNSPECIFIED. ) 
 CURVE ( )  GEOMETRIC_REPRESENTATION_ITEM ( )  RATIONAL_B_SPLINE_CURVE ( ( 1.000000000000000000, 0.9999875657313538335, 0.9999875657313538335, 1.000000000000000000 ) ) 
 REPRESENTATION_ITEM ( '' )  );
#65443 = CARTESIAN_POINT ( 'NONE',  ( -9.095061913341748294, 1384.893525202921637, 199.9428029920298968 ) ) ;
#65445 = CARTESIAN_POINT ( 'NONE',  ( 2.933761806229999713, 1464.631290085030059, 236.6723689097979673 ) ) ;
#65447 = VERTEX_POINT ( 'NONE', #50585 ) ;
#65446 = CARTESIAN_POINT ( 'NONE',  ( -2.673754402869999769, 1457.395679039389961, 218.6654034043990009 ) ) ;
#65448 = CARTESIAN_POINT ( 'NONE',  ( -1.033934541210000058, 1452.678099303230056, 183.5143811305979966 ) ) ;
#65449 = ADVANCED_FACE ( 'NONE', ( #100425 ), #45532, .T. ) ;
#65450 = CARTESIAN_POINT ( 'NONE',  ( -27.62980858599999578, 1378.955612583270067, 213.6130983169189790 ) ) ;
#65451 = EDGE_CURVE ( 'NONE', #29671, #19743, #54418, .T. ) ;
#65452 = CARTESIAN_POINT ( 'NONE',  ( -4.011846058889999789, 1474.851293822189973, 198.8411774138990040 ) ) ;
#65454 = ORIENTED_EDGE ( 'NONE', *, *, #46604, .T. ) ;
#65453 = CARTESIAN_POINT ( 'NONE',  ( -16.36863935783290103, 1414.913057862230062, 209.3429184488039709 ) ) ;
#65455 = EDGE_LOOP ( 'NONE', ( #54863, #14163, #89307, #2578, #2454 ) ) ;
#65456 = CIRCLE ( 'NONE', #36823, 1.999999999999911182 ) ;
#65457 = CARTESIAN_POINT ( 'NONE',  ( -8.187507831451240392, 1385.403986602129862, 218.7246662665380086 ) ) ;
#65458 = CARTESIAN_POINT ( 'NONE',  ( 35.50394988412039510, 1437.266775526519950, 136.5354948351899793 ) ) ;
#65459 = CARTESIAN_POINT ( 'NONE',  ( -0.5620977654635980203, 1416.851343899799986, 227.7685710128770040 ) ) ;
#65460 = CARTESIAN_POINT ( 'NONE',  ( -11.60004869884791212, 1426.686844843452036, 134.5518989175760396 ) ) ;
#65461 = CARTESIAN_POINT ( 'NONE',  ( -105.6574850370000007, 1379.068304266050063, 301.9655839248590041 ) ) ;
#65462 = DIRECTION ( 'NONE',  ( -4.648609652910299899E-17, -1.000000000000000000, 2.252106476759999926E-16 ) ) ;
#65463 = CARTESIAN_POINT ( 'NONE',  ( -15.07989985220060092, 1508.551704408389924, 214.8207627136849851 ) ) ;
#65464 = CARTESIAN_POINT ( 'NONE',  ( 12.83740251975140012, 1409.361352361609988, 201.4721406717710011 ) ) ;
#65465 = CARTESIAN_POINT ( 'NONE',  ( 18.03151512659999867, 1424.669534113930013, 225.2917716953979834 ) ) ;
#65466 = CYLINDRICAL_SURFACE ( 'NONE', #83954, 4.999999999999997335 ) ;
#65467 = CARTESIAN_POINT ( 'NONE',  ( -19.17357988869999730, 1470.688427666330199, 190.5575023379979882 ) ) ;
#65468 = DIRECTION ( 'NONE',  ( 0.4794255386025446652, -1.809663530140880534E-11, 0.8775825618912787007 ) ) ;
#65469 = ADVANCED_FACE ( 'NONE', ( #50040 ), #32672, .T. ) ;
#65470 = CARTESIAN_POINT ( 'NONE',  ( -2.499996183066730104, 1449.218566323959976, 183.0817960734219696 ) ) ;
#65471 = ORIENTED_EDGE ( 'NONE', *, *, #22650, .T. ) ;
#65472 = CARTESIAN_POINT ( 'NONE',  ( 15.09047375999176843, 1522.051704408389924, 215.6125241866901661 ) ) ;
#65473 = DIRECTION ( 'NONE',  ( 9.230617842401318720E-47, -1.000000000000000000, 1.836970198721029688E-16 ) ) ;
#65474 = CARTESIAN_POINT ( 'NONE',  ( 13.86092937120000101, 1410.765486813630105, 191.1266627561979874 ) ) ;
#65475 = CARTESIAN_POINT ( 'NONE',  ( 2.029578523264960108E-10, 1465.856113608230089, 240.9469248189070072 ) ) ;
#65476 = CARTESIAN_POINT ( 'NONE',  ( -20.28392256243369829, 1497.626837986160126, 190.6863869125700148 ) ) ;
#65477 = CARTESIAN_POINT ( 'NONE',  ( 0.000000000000000000, 1414.913060387329779, 221.6218459616979999 ) ) ;
#65478 = CARTESIAN_POINT ( 'NONE',  ( -109.7495287920000067, 1386.092077302740108, 311.3091851462589830 ) ) ;
#65479 = CARTESIAN_POINT ( 'NONE',  ( -1.212266992759999829, 1483.398284593029985, 182.2695464371980165 ) ) ;
#65480 = CARTESIAN_POINT ( 'NONE',  ( -10.51336953340124758, 1363.224273292747284, 207.6218459616987673 ) ) ;
#65481 = CARTESIAN_POINT ( 'NONE',  ( -46.15015871273919856, 1440.464460849770148, 268.2045569567199550 ) ) ;
#65482 = CARTESIAN_POINT ( 'NONE',  ( 13.39710138444150012, 1508.017386564119988, 233.1392620568510097 ) ) ;
#65483 = CARTESIAN_POINT ( 'NONE',  ( -21.33942536743590068, 1477.920010453090072, 208.5333634439200239 ) ) ;
#65484 = CARTESIAN_POINT ( 'NONE',  ( 2.284053471355000031, 1516.854133554269993, 207.9850318982369970 ) ) ;
#65485 = CARTESIAN_POINT ( 'NONE',  ( 5.082258451441009406, 1407.428259223129999, 221.1577315719200101 ) ) ;
#65486 = EDGE_CURVE ( 'NONE', #99871, #32822, #2603, .T. ) ;
#65487 = CARTESIAN_POINT ( 'NONE',  ( -14.27693757830880017, 1379.587460516140027, 207.9273167693889945 ) ) ;
#65488 = CARTESIAN_POINT ( 'NONE',  ( 7.452937308169480524, 1425.221714708150103, 212.3436467550869793 ) ) ;
#65489 = VERTEX_POINT ( 'NONE', #57892 ) ;
#65490 = CARTESIAN_POINT ( 'NONE',  ( 27.90885394449999879, 1424.419860138930062, 250.2249407727979928 ) ) ;
#65491 = CARTESIAN_POINT ( 'NONE',  ( 10.56407631929999980, 1452.658139941989930, 209.7432180256290053 ) ) ;
#65493 = CARTESIAN_POINT ( 'NONE',  ( -14.79494656225329940, 1512.129944624190102, 221.3833869628849698 ) ) ;
#65492 = CARTESIAN_POINT ( 'NONE',  ( -2.545491131529999951, 1499.389042279630075, 181.1800920301980113 ) ) ;
#65494 = EDGE_CURVE ( 'NONE', #57665, #10690, #31180, .T. ) ;
#65495 = CARTESIAN_POINT ( 'NONE',  ( 1.469929971929456070, 1507.915326702531047, 180.9459708344064666 ) ) ;
#65496 = CARTESIAN_POINT ( 'NONE',  ( -27.70845745580000141, 1431.442878273549923, 238.1060641559980127 ) ) ;
#65497 = CARTESIAN_POINT ( 'NONE',  ( -29.43798506786606950, 1509.956740567253064, 206.0314242323168230 ) ) ;
#65498 = CARTESIAN_POINT ( 'NONE',  ( -10.75854853582960047, 1452.537363593840155, 150.2728578400229935 ) ) ;
#65499 = CARTESIAN_POINT ( 'NONE',  ( -18.79734781009999978, 1416.844618635330107, 208.4088319070980049 ) ) ;
#65500 = VERTEX_POINT ( 'NONE', #49491 ) ;
#65501 = CARTESIAN_POINT ( 'NONE',  ( -107.5342874719949862, 1378.913060387359792, 300.5051711733210595 ) ) ;
#65502 = CARTESIAN_POINT ( 'NONE',  ( 6.480125363573969479E-05, 1410.239966284670118, 269.6149245224239621 ) ) ;
#65503 = CARTESIAN_POINT ( 'NONE',  ( 16.89525345604750228, 1422.350075462329869, 226.9164778485460090 ) ) ;
#65504 = CARTESIAN_POINT ( 'NONE',  ( -4.161595075237580765, 1448.982995846620042, 185.0801961897900298 ) ) ;
#65505 = VERTEX_POINT ( 'NONE', #8562 ) ;
#65506 = ORIENTED_EDGE ( 'NONE', *, *, #88303, .F. ) ;
#65507 = CARTESIAN_POINT ( 'NONE',  ( -25.91358801470000373, 1384.684512614960113, 203.4532549264589818 ) ) ;
#65508 = CARTESIAN_POINT ( 'NONE',  ( -22.93660144289669844, 1409.723673488970007, 209.0949845260039979 ) ) ;
#65509 = ORIENTED_EDGE ( 'NONE', *, *, #14612, .F. ) ;
#65510 = CARTESIAN_POINT ( 'NONE',  ( 0.08461443304019999889, 1416.823634022930037, 227.2251189671980001 ) ) ;
#65511 = CARTESIAN_POINT ( 'NONE',  ( -105.7049770469999999, 1379.426018556420104, 306.8995712054589831 ) ) ;
#65512 = CARTESIAN_POINT ( 'NONE',  ( -2.907264515414449857, 1451.960119877520128, 184.7556101994359778 ) ) ;
#65514 = CIRCLE ( 'NONE', #17174, 8.104319688360000384 ) ;
#65513 = CARTESIAN_POINT ( 'NONE',  ( -1.368191914778909890, 1419.344528075180278, 185.2221190139939893 ) ) ;
#65515 = ORIENTED_EDGE ( 'NONE', *, *, #53839, .T. ) ;
#65516 = VECTOR ( 'NONE', #73290, 1000.000000000000000 ) ;
#65517 = CARTESIAN_POINT ( 'NONE',  ( 41.65757230853200355, 1455.325850625539942, 266.3038443812790206 ) ) ;
#65518 = CARTESIAN_POINT ( 'NONE',  ( -11.80289467576660023, 1415.088012641449950, 221.3076621094219831 ) ) ;
#65519 = CARTESIAN_POINT ( 'NONE',  ( -7.514943502940000464, 1426.327996137909849, 205.9160340660789927 ) ) ;
#65520 = CARTESIAN_POINT ( 'NONE',  ( 7.323974606304999746, 1516.647924054489977, 205.0857262875869935 ) ) ;
#65521 = ORIENTED_EDGE ( 'NONE', *, *, #28902, .F. ) ;
#65522 = CARTESIAN_POINT ( 'NONE',  ( 10.86020916433990102, 1481.036884354570020, 213.7433009987580022 ) ) ;
#65523 = CARTESIAN_POINT ( 'NONE',  ( 19.66678637246580053, 1519.551704408389924, 202.3500283489900085 ) ) ;
#65524 = CARTESIAN_POINT ( 'NONE',  ( 13.28675557712670674, 1443.221090981650377, 187.6942237735384253 ) ) ;
#65525 = ORIENTED_EDGE ( 'NONE', *, *, #27002, .F. ) ;
#65526 = ORIENTED_EDGE ( 'NONE', *, *, #47307, .F. ) ;
#65527 = CARTESIAN_POINT ( 'NONE',  ( -11.41773502901409998, 1481.611637904830104, 209.4132993426249811 ) ) ;
#65528 = LINE ( 'NONE', #37554, #68130 ) ;
#65529 = CARTESIAN_POINT ( 'NONE',  ( -12.67335160806310057, 1512.240709848920005, 194.0399737768200055 ) ) ;
#65530 = CARTESIAN_POINT ( 'NONE',  ( 9.260035559154880858, 1503.457705115180033, 217.8739325455829885 ) ) ;
#65531 = CARTESIAN_POINT ( 'NONE',  ( 12.02531869610000115, 1420.571450649919825, 199.9272147486889821 ) ) ;
#65532 = CARTESIAN_POINT ( 'NONE',  ( 0.1435280708731850041, 1475.283311921460154, 220.5458192635479975 ) ) ;
#65533 = CARTESIAN_POINT ( 'NONE',  ( -108.2677198149262665, 1380.892023996865646, 298.2229625968756750 ) ) ;
#65534 = B_SPLINE_CURVE_WITH_KNOTS ( 'NONE', 3,
 ( #44165, #11655, #54239, #96214, #18373, #105731, #12196, #53692, #86701, #27904, #53123, #104611, #10553, #1616, #79964, #62087, #61530, #95658, #45831, #18925, #19488, #87833, #11121, #56423, #38498, #21124, #5454, #29550, #12754, #3837, #48017, #100059, #13830, #39037, #73216, #48580, #80521, #65936, #72675, #82154, #39613, #46936, #81055, #65387, #90004, #90553 ),
 .UNSPECIFIED., .F., .F.,
 ( 4, 3, 3, 3, 3, 3, 3, 3, 3, 3, 3, 3, 3, 3, 3, 4 ),
 ( 0.000000000000000000, 0.09251053440245410320, 0.1819424025277689982, 0.2703167020720390057, 0.3599760602905189844, 0.4496354185090000177, 0.6562016036042499501, 0.8628455277292459424, 1.069372843309620125, 1.260326837218950002, 1.275900158890000080, 1.435752599818300057, 1.593630893054559960, 1.750171058644690136, 1.905888283666149929, 2.061605508687600175 ),
 .UNSPECIFIED. ) ;
#65535 = CARTESIAN_POINT ( 'NONE',  ( -5.215695737369999918, 1495.379815458989924, 198.7908035812990022 ) ) ;
#65536 = FACE_OUTER_BOUND ( 'NONE', #96877, .T. ) ;
#65538 = LINE ( 'NONE', #89061, #94034 ) ;
#65537 = CARTESIAN_POINT ( 'NONE',  ( -16.79695581410840077, 1415.044791756060022, 191.6206649154599688 ) ) ;
#65539 = CARTESIAN_POINT ( 'NONE',  ( 11.30538286922199909, 1426.159524226919984, 206.5002785976879807 ) ) ;
#65540 = CARTESIAN_POINT ( 'NONE',  ( -24.34259636588380005, 1508.950977677119909, 222.4692572808739897 ) ) ;
#65541 = CARTESIAN_POINT ( 'NONE',  ( -8.041028958794997905, 1514.881364185380107, 203.0257501012370369 ) ) ;
#65542 = VERTEX_POINT ( 'NONE', #42734 ) ;
#65543 = CARTESIAN_POINT ( 'NONE',  ( 5.120453548759999585, 1471.466545119689954, 214.4276395123089856 ) ) ;
#65544 = CARTESIAN_POINT ( 'NONE',  ( -1.347412987175396371, 1395.960113085665398, 201.1218459616979999 ) ) ;
#65545 = CARTESIAN_POINT ( 'NONE',  ( -84.07870740561909884, 1384.983604346920174, 306.2409631616719707 ) ) ;
#65546 = CARTESIAN_POINT ( 'NONE',  ( -8.067891928930000844, 1386.126867263409849, 199.6142371476589972 ) ) ;
#65547 = CARTESIAN_POINT ( 'NONE',  ( 9.517773336257400629, 1423.536455532770105, 209.9636451762389981 ) ) ;
#65549 = ORIENTED_EDGE ( 'NONE', *, *, #108376, .T. ) ;
#65548 = CARTESIAN_POINT ( 'NONE',  ( 11.65242884602639961, 1425.717965413690081, 202.8942723744929992 ) ) ;
#65550 = CARTESIAN_POINT ( 'NONE',  ( 2.398699649889999730, 1429.053736725890076, 217.0724297081890199 ) ) ;
#65551 = CARTESIAN_POINT ( 'NONE',  ( 16.51112239071560950, 1525.159177407155994, 237.1918628954884127 ) ) ;
#65552 = CARTESIAN_POINT ( 'NONE',  ( -4.685705521985438438, 1475.329346039780148, 218.3671617030974801 ) ) ;
#65553 = CARTESIAN_POINT ( 'NONE',  ( 11.77548435589999976, 1433.640636952740124, 150.8383593496980097 ) ) ;
#65554 = CARTESIAN_POINT ( 'NONE',  ( 36.06124926539999365, 1440.913060387330006, 262.6648722463980334 ) ) ;
#65555 = CARTESIAN_POINT ( 'NONE',  ( -31.32995031131208918, 1523.678648413191695, 196.3423562208917872 ) ) ;
#65556 = CARTESIAN_POINT ( 'NONE',  ( 11.81707110430000007, 1430.266231075130008, 147.2485970657980090 ) ) ;
#65557 = CARTESIAN_POINT ( 'NONE',  ( 0.2576823252080000515, 1419.224537961029910, 184.6439154818979773 ) ) ;
#65558 = CARTESIAN_POINT ( 'NONE',  ( 11.40944910055886119, 1511.843510977572350, 224.6458867293904405 ) ) ;
#65559 = CARTESIAN_POINT ( 'NONE',  ( -31.12456774391181469, 1525.960063244516959, 201.1524202391567258 ) ) ;
#65560 = DIRECTION ( 'NONE',  ( 1.000000000000000000, 0.000000000000000000, 0.000000000000000000 ) ) ;
#65561 = CARTESIAN_POINT ( 'NONE',  ( -4.500000000000000000, 1425.929641636930000, 184.1455913746980002 ) ) ;
#65562 = B_SPLINE_CURVE_WITH_KNOTS ( 'NONE', 5,
 ( #105088, #36780, #46315, #106188, #88287, #89929 ),
 .UNSPECIFIED., .F., .F.,
 ( 6, 6 ),
 ( 0.000000000000000000, 1.000000000000000000 ),
 .UNSPECIFIED. ) ;
#65563 = CARTESIAN_POINT ( 'NONE',  ( 5.021037906353149616, 1440.968375784319960, 155.1907003990020257 ) ) ;
#65564 = CARTESIAN_POINT ( 'NONE',  ( 17.78630097849999814, 1455.623587567290087, 200.4657979530790044 ) ) ;
#65565 = CARTESIAN_POINT ( 'NONE',  ( -16.63500958477349911, 1409.493940183780069, 193.4350317777050066 ) ) ;
#65566 = CARTESIAN_POINT ( 'NONE',  ( 0.008453540420540530190, 1515.389376838289991, 204.8287432943390058 ) ) ;
#65567 = CARTESIAN_POINT ( 'NONE',  ( 4.026786250540000722, 1408.413060387330006, 146.1721969590979882 ) ) ;
#65568 = CARTESIAN_POINT ( 'NONE',  ( 2.292469808877632520, 1497.477225423111577, 197.6467893764333326 ) ) ;
#65569 = CARTESIAN_POINT ( 'NONE',  ( -9.612666206359998355, 1414.913060387329779, 222.3789311915979852 ) ) ;
#65570 = CARTESIAN_POINT ( 'NONE',  ( 0.2088027491384900070, 1458.021659680169932, 183.0379629500139913 ) ) ;
#65572 = ORIENTED_EDGE ( 'NONE', *, *, #109978, .F. ) ;
#65571 = CARTESIAN_POINT ( 'NONE',  ( -12.86051124159999937, 1409.184418768930072, 216.3873131214179750 ) ) ;
#65573 = CARTESIAN_POINT ( 'NONE',  ( -32.02808312589930040, 1512.187213306747481, 198.2787714533499752 ) ) ;
#65574 = DIRECTION ( 'NONE',  ( 1.755985294532469921E-16, -1.000000000000000000, 1.338183447452831989E-16 ) ) ;
#65575 = CARTESIAN_POINT ( 'NONE',  ( 13.80544311399999913, 1434.979600114139885, 148.5019818398979794 ) ) ;
#65576 = CARTESIAN_POINT ( 'NONE',  ( -26.80766422789999837, 1435.433722594319988, 135.7240085096979954 ) ) ;
#65577 = CARTESIAN_POINT ( 'NONE',  ( 10.24908546679999866, 1441.239651135290160, 187.1830758738979910 ) ) ;
#65578 = VERTEX_POINT ( 'NONE', #74693 ) ;
#65579 = CARTESIAN_POINT ( 'NONE',  ( -17.26794000855262112, 1525.730671215512757, 181.5864061050555165 ) ) ;
#65580 = CARTESIAN_POINT ( 'NONE',  ( -13.13561839920527063, 1517.151704408390060, 208.3084799397878157 ) ) ;
#65581 = CARTESIAN_POINT ( 'NONE',  ( -105.2473876565402833, 1381.074936998757721, 308.6785104366205132 ) ) ;
#65582 = CARTESIAN_POINT ( 'NONE',  ( -11.14576561989999881, 1491.244072761289999, 209.5089610898519936 ) ) ;
#65583 = DIRECTION ( 'NONE',  ( 0.000000000000000000, -1.000000000000000000, 0.000000000000000000 ) ) ;
#65584 = CARTESIAN_POINT ( 'NONE',  ( 13.37404851082409962, 1507.496393256099964, 233.0472755390670159 ) ) ;
#65585 = CARTESIAN_POINT ( 'NONE',  ( 39.19951531957330104, 1423.398545273861146, 269.1491992711760872 ) ) ;
#65586 = CARTESIAN_POINT ( 'NONE',  ( -13.35310380080168002, 1481.629060506388441, 225.5919806602003064 ) ) ;
#65587 = CARTESIAN_POINT ( 'NONE',  ( 20.32975030060803334, 1508.870389961778528, 189.2250207761221930 ) ) ;
#65588 = CARTESIAN_POINT ( 'NONE',  ( 2.661634141329999537, 1431.451308766379952, 184.1577198843980057 ) ) ;
#65589 = CARTESIAN_POINT ( 'NONE',  ( -58.02100482020349403, 1385.051923325640018, 239.8170954572080120 ) ) ;
#65590 = CARTESIAN_POINT ( 'NONE',  ( -18.10570579381957401, 1525.713797967457140, 238.1210409130250127 ) ) ;
#65591 = CARTESIAN_POINT ( 'NONE',  ( -26.80425587306198310, 1435.467044139958489, 135.6517718923794575 ) ) ;
#65592 = ORIENTED_EDGE ( 'NONE', *, *, #86576, .F. ) ;
#65593 = CARTESIAN_POINT ( 'NONE',  ( -28.49886664254099600, 1509.035040377790210, 208.7883124179550123 ) ) ;
#65594 = CARTESIAN_POINT ( 'NONE',  ( -16.03783333616070195, 1409.473006842159975, 225.3014575052910118 ) ) ;
#65595 = EDGE_CURVE ( 'NONE', #1407, #17543, #41101, .T. ) ;
#65597 = ORIENTED_EDGE ( 'NONE', *, *, #6913, .T. ) ;
#65596 = CARTESIAN_POINT ( 'NONE',  ( 2.023323367690000207, 1501.741525076489779, 230.4104378513989957 ) ) ;
#65598 = CARTESIAN_POINT ( 'NONE',  ( -109.4840107539999963, 1384.898108854659995, 311.2841325702589756 ) ) ;
#65599 = CARTESIAN_POINT ( 'NONE',  ( 10.04076066863449945, 1469.831999276539818, 209.8600323314049945 ) ) ;
#65600 = CARTESIAN_POINT ( 'NONE',  ( 17.83968203154910270, 1430.541692949039998, 212.9271915631379954 ) ) ;
#65601 = CARTESIAN_POINT ( 'NONE',  ( -109.6410173800000081, 1384.508238210969921, 311.3032840212590031 ) ) ;
#65602 = CARTESIAN_POINT ( 'NONE',  ( -11.30241272700000010, 1414.983773852829927, 195.8621715883979846 ) ) ;
#65603 = CARTESIAN_POINT ( 'NONE',  ( 0.4070099242259999639, 1465.094834125830175, 236.9943866744980028 ) ) ;
#65604 = EDGE_CURVE ( 'NONE', #99690, #30233, #58993, .T. ) ;
#65605 = CARTESIAN_POINT ( 'NONE',  ( 23.01300307269999834, 1410.211808750929777, 212.8080261142179666 ) ) ;
#65606 = CYLINDRICAL_SURFACE ( 'NONE', #82055, 1.000000000000001332 ) ;
#65607 = CARTESIAN_POINT ( 'NONE',  ( -9.518190392760001117, 1465.040135640790140, 228.2885054898990234 ) ) ;
#65608 = CARTESIAN_POINT ( 'NONE',  ( -16.55421215910000043, 1423.367941342530003, 228.9006519623980012 ) ) ;
#65610 = CARTESIAN_POINT ( 'NONE',  ( 21.99231067417252206, 1506.446781340372127, 208.8672818357590018 ) ) ;
#65609 = CARTESIAN_POINT ( 'NONE',  ( 5.216723163609201741, 1497.653739079350316, 197.6766713243789013 ) ) ;
#65611 = CARTESIAN_POINT ( 'NONE',  ( 7.015117299519999960, 1480.620769302089911, 206.9956269080190054 ) ) ;
#65612 = CARTESIAN_POINT ( 'NONE',  ( -101.4843241977000474, 1368.558218059090905, 307.2644175748700377 ) ) ;
#65613 = CARTESIAN_POINT ( 'NONE',  ( 13.91344329460000040, 1453.313060387329870, 224.4164659125979995 ) ) ;
#65614 = CARTESIAN_POINT ( 'NONE',  ( -0.7334337980199999718, 1417.382035507929913, 235.1308628909980030 ) ) ;
#65615 = CARTESIAN_POINT ( 'NONE',  ( -5.513264357029999729, 1374.913060387289988, 203.3066656689789795 ) ) ;
#65616 = CARTESIAN_POINT ( 'NONE',  ( 6.547881374914999775, 1516.647534046129977, 205.6658385469270058 ) ) ;
#65617 = CARTESIAN_POINT ( 'NONE',  ( -12.70480096745579957, 1484.837292199019885, 185.9669015828420129 ) ) ;
#65618 = ORIENTED_EDGE ( 'NONE', *, *, #58614, .F. ) ;
#65619 = CARTESIAN_POINT ( 'NONE',  ( -17.05226164202473882, 1516.729020965289237, 195.6302442682282390 ) ) ;
#65621 = B_SPLINE_CURVE_WITH_KNOTS ( 'NONE', 3,
 ( #75334, #83706, #107809, #23240, #57439, #31096, #99390, #56868, #33851, #61312 ),
 .UNSPECIFIED., .F., .F.,
 ( 4, 2, 2, 2, 4 ),
 ( 0.000000000000000000, 0.2500000000000000555, 0.5000000000000001110, 0.7500000000000002220, 1.000000000000000000 ),
 .UNSPECIFIED. ) ;
#65620 = CARTESIAN_POINT ( 'NONE',  ( -4.225202376359490586, 1441.574362862340195, 166.3910519188600006 ) ) ;
#65623 = EDGE_LOOP ( 'NONE', ( #56280, #99259, #14812, #9605 ) ) ;
#65622 = CARTESIAN_POINT ( 'NONE',  ( -68.54965750324760165, 1379.747397323139921, 280.1613699669709945 ) ) ;
#65624 = ORIENTED_EDGE ( 'NONE', *, *, #33357, .F. ) ;
#65625 = CARTESIAN_POINT ( 'NONE',  ( -8.121603995746610849, 1382.367886013207908, 218.5361279351766370 ) ) ;
#65626 = ORIENTED_EDGE ( 'NONE', *, *, #106248, .T. ) ;
#65627 = CARTESIAN_POINT ( 'NONE',  ( -2.848799080821822205, 1456.353470596306806, 200.0717474131963343 ) ) ;
#65628 = CARTESIAN_POINT ( 'NONE',  ( 11.81504872310000032, 1500.768363563890034, 208.0408261944689912 ) ) ;
#65630 = CARTESIAN_POINT ( 'NONE',  ( 15.84154831066869917, 1409.491884921769952, 192.6660917361010092 ) ) ;
#65629 = CARTESIAN_POINT ( 'NONE',  ( -11.44354861750966279, 1425.477604805352030, 144.5838835533737381 ) ) ;
#65631 = CARTESIAN_POINT ( 'NONE',  ( -5.772978316675000166, 1516.659138130710289, 210.2536427808470023 ) ) ;
#65632 = FACE_OUTER_BOUND ( 'NONE', #63315, .T. ) ;
#65633 = CARTESIAN_POINT ( 'NONE',  ( 4.757611653739999724, 1476.697157691990014, 198.4937409947989977 ) ) ;
#65634 = CARTESIAN_POINT ( 'NONE',  ( 16.86259531663306532, 1460.525699792653995, 228.8369507918937700 ) ) ;
#65635 = CARTESIAN_POINT ( 'NONE',  ( 8.921631616102885687, 1502.413060387330006, 225.4527830926159595 ) ) ;
#65636 = CARTESIAN_POINT ( 'NONE',  ( 44.93136303390000563, 1440.913033067569813, 269.6838066906980202 ) ) ;
#65637 = EDGE_LOOP ( 'NONE', ( #14877, #102635, #30772 ) ) ;
#65638 = CARTESIAN_POINT ( 'NONE',  ( -4.354848045695810299, 1481.954746482949986, 231.1149966751839884 ) ) ;
#65639 = CARTESIAN_POINT ( 'NONE',  ( 7.891777514710270225, 1512.314860025949883, 206.1798159824890035 ) ) ;
#65640 = ORIENTED_EDGE ( 'NONE', *, *, #66585, .T. ) ;
#65641 = VERTEX_POINT ( 'NONE', #109937 ) ;
#65642 = CARTESIAN_POINT ( 'NONE',  ( 10.06505727382652715, 1410.639190484854907, 229.7922706876150301 ) ) ;
#65643 = CYLINDRICAL_SURFACE ( 'NONE', #106428, 1.999999999999902967 ) ;
#65644 = CARTESIAN_POINT ( 'NONE',  ( 0.1475592169000000120, 1451.689388021529794, 183.0405803991980065 ) ) ;
#65645 = CARTESIAN_POINT ( 'NONE',  ( -20.35012269109810035, 1508.551704411970150, 210.1667554882619982 ) ) ;
#65646 = LINE ( 'NONE', #100331, #85225 ) ;
#65647 = CIRCLE ( 'NONE', #97757, 0.9999999999999886757 ) ;
#65648 = CARTESIAN_POINT ( 'NONE',  ( -14.51248501049999895, 1379.683207487500113, 208.2417184310789935 ) ) ;
#65649 = CARTESIAN_POINT ( 'NONE',  ( 40.71747595459699909, 1448.637563191980007, 135.6938357208099717 ) ) ;
#65650 = CARTESIAN_POINT ( 'NONE',  ( -5426.659240077532559, 2833.746317950420234, 8449.939303199314963 ) ) ;
#65651 = CARTESIAN_POINT ( 'NONE',  ( 26.64405787239999768, 1440.573177016219915, 137.3591247521979994 ) ) ;
#65652 = DIRECTION ( 'NONE',  ( -0.9786619618251657382, 0.000000000000000000, -0.2054769195713184449 ) ) ;
#65653 = CARTESIAN_POINT ( 'NONE',  ( -69.05319778136079378, 1384.731230461870155, 263.9282964275780046 ) ) ;
#65654 = ORIENTED_EDGE ( 'NONE', *, *, #85543, .F. ) ;
#65655 = CARTESIAN_POINT ( 'NONE',  ( -2.873329398885000163, 1516.572193931679976, 201.7997408644770019 ) ) ;
#65656 = CARTESIAN_POINT ( 'NONE',  ( 5.772978278544999675, 1516.659138130710289, 207.9900491214870044 ) ) ;
#65657 = ORIENTED_EDGE ( 'NONE', *, *, #16601, .T. ) ;
#65658 = CARTESIAN_POINT ( 'NONE',  ( 41.96952434445400115, 1440.913060387330006, 269.5508532369769910 ) ) ;
#65659 = CARTESIAN_POINT ( 'NONE',  ( -0.002355423392913324858, 1451.792606406385175, 154.0462491319130436 ) ) ;
#65660 = ORIENTED_EDGE ( 'NONE', *, *, #12235, .T. ) ;
#65661 = CARTESIAN_POINT ( 'NONE',  ( -0.2565269630447720162, 1450.904102268370025, 181.8958596656970030 ) ) ;
#65662 = DIRECTION ( 'NONE',  ( -0.000000000000000000, -1.000000000000000000, -0.000000000000000000 ) ) ;
#65663 = CARTESIAN_POINT ( 'NONE',  ( -18.92577228117313481, 1508.457812386920523, 210.3413885190254859 ) ) ;
#65664 = CARTESIAN_POINT ( 'NONE',  ( -9.730115140653261108, 1461.904593459310036, 207.4327562979160291 ) ) ;
#65665 = CARTESIAN_POINT ( 'NONE',  ( -4.288575270049999943, 1421.887819494029827, 185.0877211516979912 ) ) ;
#65666 = CARTESIAN_POINT ( 'NONE',  ( -5.890586702848469969, 1511.182265711499895, 201.4425314663570248 ) ) ;
#65667 = CARTESIAN_POINT ( 'NONE',  ( -0.7082213409149999972, 1508.873178418929911, 179.8394376137979975 ) ) ;
#65668 = CARTESIAN_POINT ( 'NONE',  ( -18.51436573157338117, 1512.187213306747481, 237.1421867457408723 ) ) ;
#65669 = CARTESIAN_POINT ( 'NONE',  ( 10.81507089421240053, 1424.921187596799882, 144.1620444706739761 ) ) ;
#65671 = CARTESIAN_POINT ( 'NONE',  ( -11.60004869885203860, 1423.522019188771310, 137.0424394678681210 ) ) ;
#65670 = CARTESIAN_POINT ( 'NONE',  ( 13.76459360349999983, 1460.937369267029908, 231.9016751017979914 ) ) ;
#65672 = CARTESIAN_POINT ( 'NONE',  ( -4.572909471579259311, 1422.074987962655996, 184.6258731943378280 ) ) ;
#65673 = AXIS2_PLACEMENT_3D ( 'NONE', #28608, #36449, #62808 ) ;
#65674 = CARTESIAN_POINT ( 'NONE',  ( -6.554778571775000451, 1516.929962200689943, 216.8412383526069789 ) ) ;
#65675 = ORIENTED_EDGE ( 'NONE', *, *, #17108, .T. ) ;
#65676 = CARTESIAN_POINT ( 'NONE',  ( 18.66420869458043796, 1526.382868172863937, 185.4599087859680537 ) ) ;
#65677 = CARTESIAN_POINT ( 'NONE',  ( -10.34125195379056450, 1480.634459757738796, 207.0903537657474658 ) ) ;
#65678 = CARTESIAN_POINT ( 'NONE',  ( 17.06845921355082041, 1448.846822804656540, 218.4183351126684727 ) ) ;
#65679 = CARTESIAN_POINT ( 'NONE',  ( 6.948321705865000197, 1517.049325831759916, 213.1561268858870051 ) ) ;
#65680 = CARTESIAN_POINT ( 'NONE',  ( 18.60392304109999984, 1508.243836144429906, 188.5101919634980163 ) ) ;
#65681 = CARTESIAN_POINT ( 'NONE',  ( -20.71343476517554905, 1512.187213306747481, 179.9059455038197086 ) ) ;
#65683 = VERTEX_POINT ( 'NONE', #93121 ) ;
#65682 = CARTESIAN_POINT ( 'NONE',  ( -11.28871479695359881, 1500.517265169780103, 210.9741532246169982 ) ) ;
#65684 = CARTESIAN_POINT ( 'NONE',  ( -17.29393938232436057, 1523.621879633028811, 237.3864571009502811 ) ) ;
#65685 = CARTESIAN_POINT ( 'NONE',  ( 11.20759482449999922, 1458.854746706030028, 217.3836589402779964 ) ) ;
#65686 = CARTESIAN_POINT ( 'NONE',  ( -10.94598488280000126, 1430.643605498629995, 151.5761596627980055 ) ) ;
#65687 = CARTESIAN_POINT ( 'NONE',  ( 19.07077998173900113, 1456.927795362189954, 225.2567787181259860 ) ) ;
#65688 = EDGE_CURVE ( 'NONE', #104987, #68277, #48946, .T. ) ;
#65689 = CARTESIAN_POINT ( 'NONE',  ( -109.9643883132849851, 1384.403371867929991, 311.4317840562709989 ) ) ;
#65690 = FACE_OUTER_BOUND ( 'NONE', #85879, .T. ) ;
#65691 = PLANE ( 'NONE',  #143 ) ;
#65692 = CARTESIAN_POINT ( 'NONE',  ( 12.69201959859999995, 1445.029817614240073, 186.3520294606980201 ) ) ;
#65694 = CARTESIAN_POINT ( 'NONE',  ( -10.97569758906830018, 1482.624302103220089, 205.8415845986210115 ) ) ;
#65693 = CARTESIAN_POINT ( 'NONE',  ( -19.37516407789999917, 1457.447849671029871, 226.2756290344979959 ) ) ;
#65696 = CARTESIAN_POINT ( 'NONE',  ( -3.054816022670000297, 1485.996906138130043, 182.1538610966980229 ) ) ;
#65695 = CIRCLE ( 'NONE', #92429, 18.16666666670000296 ) ;
#65697 = VERTEX_POINT ( 'NONE', #16937 ) ;
#65698 = CARTESIAN_POINT ( 'NONE',  ( 4.027697225915000345, 1516.766397346390022, 206.2431526829570032 ) ) ;
#65699 = CARTESIAN_POINT ( 'NONE',  ( 7.002505146659999902, 1406.898447550930086, 269.4815251353980443 ) ) ;
#65700 = CARTESIAN_POINT ( 'NONE',  ( -0.05604939685589999804, 1409.080516226629925, 185.5803113818979853 ) ) ;
#65701 = CARTESIAN_POINT ( 'NONE',  ( 10.93679547204000002, 1490.434980368090010, 209.9321327948960061 ) ) ;
#65702 = CARTESIAN_POINT ( 'NONE',  ( 23.41305660651092424, 1433.448859892850123, 215.2039121327621274 ) ) ;
#65703 = CARTESIAN_POINT ( 'NONE',  ( 2.113994577280214227, 1464.204615851377184, 199.5304910285045992 ) ) ;
#65704 = CARTESIAN_POINT ( 'NONE',  ( 28.19408364699999936, 1508.123162656630029, 209.7484684564449822 ) ) ;
#65705 = CARTESIAN_POINT ( 'NONE',  ( -6.790400283243552160, 1439.837278262902373, 203.5909105148159313 ) ) ;
#65706 = CARTESIAN_POINT ( 'NONE',  ( -2.491511770217889943, 1449.258138113479845, 154.2481093272120063 ) ) ;
#65707 = CARTESIAN_POINT ( 'NONE',  ( -1.641945290704282190, 1450.652787028681360, 183.1941434156354660 ) ) ;
#65708 = CARTESIAN_POINT ( 'NONE',  ( -19.86849070297746067, 1485.435531518196740, 190.6411886671614582 ) ) ;
#65709 = CARTESIAN_POINT ( 'NONE',  ( -14.36283523570150145, 1416.196255300880011, 221.2942896565629951 ) ) ;
#65710 = CARTESIAN_POINT ( 'NONE',  ( -9.234075267490000627, 1498.091069991990025, 216.0247435465689989 ) ) ;
#65711 = CARTESIAN_POINT ( 'NONE',  ( -8.827869491105628796, 1409.221336382960317, 197.0457684614559923 ) ) ;
#65712 = AXIS2_PLACEMENT_3D ( 'NONE', #52343, #61311, #18692 ) ;
#65713 = CARTESIAN_POINT ( 'NONE',  ( 4.363119589138680254, 1423.854801764450031, 183.5697712894070150 ) ) ;
#65714 = CARTESIAN_POINT ( 'NONE',  ( 3.685495795909999650, 1441.157097705729939, 159.2182474352979966 ) ) ;
#65715 = CARTESIAN_POINT ( 'NONE',  ( -3.774051438349999898, 1475.935069928129906, 268.4776602676979564 ) ) ;
#65716 = B_SPLINE_CURVE_WITH_KNOTS ( 'NONE', 5,
 ( #59076, #14280, #57968, #75326, #67479, #90991, #14832, #32200, #42257, #7547, #92103, #15379, #57431, #48471, #66926 ),
 .UNSPECIFIED., .F., .F.,
 ( 6, 3, 3, 3, 6 ),
 ( 0.000000000000000000, 0.1467687781236080569, 0.3860735318475042033, 0.6253782855714004052, 1.000000000000000000 ),
 .UNSPECIFIED. ) ;
#65717 = CARTESIAN_POINT ( 'NONE',  ( -4.240750497009450726, 1446.388360617959961, 162.7103197369740144 ) ) ;
#65718 = CARTESIAN_POINT ( 'NONE',  ( -11.56086350461344203, 1512.916370508231921, 192.7448627781640766 ) ) ;
#65719 = DIRECTION ( 'NONE',  ( -1.755985294532469921E-16, 1.000000000000000000, -1.338183447452831989E-16 ) ) ;
#65720 = CARTESIAN_POINT ( 'NONE',  ( -58.60893540860839579, 1384.701328510650001, 278.5430915364260613 ) ) ;
#65721 = CARTESIAN_POINT ( 'NONE',  ( 2.370878938589389140, 1508.995853304402544, 237.7496061730882673 ) ) ;
#65722 = CIRCLE ( 'NONE', #24520, 7.300000000000009592 ) ;
#65723 = CYLINDRICAL_SURFACE ( 'NONE', #48566, 2.000000000000002220 ) ;
#65724 = CARTESIAN_POINT ( 'NONE',  ( 12.33229080803599942, 1492.071651757490145, 209.1313924691960153 ) ) ;
#65725 = CARTESIAN_POINT ( 'NONE',  ( 31.97162612954836192, 1524.678541297861102, 216.6706125259247244 ) ) ;
#65726 = CARTESIAN_POINT ( 'NONE',  ( 7.892106848066304359, 1512.076549611834707, 206.1384687351585967 ) ) ;
#65727 = CARTESIAN_POINT ( 'NONE',  ( -17.98939367079999840, 1410.465183412730084, 195.2754043712980092 ) ) ;
#65728 = CARTESIAN_POINT ( 'NONE',  ( 12.88825199978909986, 1421.219518988400068, 204.9917899569869917 ) ) ;
#65729 = CARTESIAN_POINT ( 'NONE',  ( -22.40611913229999885, 1411.902937806130012, 270.0285353679980176 ) ) ;
#65730 = ORIENTED_EDGE ( 'NONE', *, *, #20207, .F. ) ;
#65731 = EDGE_CURVE ( 'NONE', #43895, #13558, #8957, .T. ) ;
#65732 = CARTESIAN_POINT ( 'NONE',  ( -1.709547000564935804, 1410.351682048799603, 232.8846474005925415 ) ) ;
#65733 = DIRECTION ( 'NONE',  ( 0.5117323852940359741, 0.8591449038673723004, 0.000000000000000000 ) ) ;
#65734 = CARTESIAN_POINT ( 'NONE',  ( 11.27339694765309908, 1433.557990533659904, 225.8166789516029951 ) ) ;
#65736 = CARTESIAN_POINT ( 'NONE',  ( -15.27973131726499822, 1514.812393650459853, 193.2888744509670005 ) ) ;
#65735 = CARTESIAN_POINT ( 'NONE',  ( 11.64281719679999938, 1426.759312292029790, 137.4371925635979892 ) ) ;
#65737 = FACE_OUTER_BOUND ( 'NONE', #71752, .T. ) ;
#65738 = CARTESIAN_POINT ( 'NONE',  ( -120.4392612185200022, 1309.112692017090239, 300.3762800269190052 ) ) ;
#65739 = CARTESIAN_POINT ( 'NONE',  ( 40.32490366350000244, 1444.177947227670074, 137.1005529477980076 ) ) ;
#65740 = B_SPLINE_CURVE_WITH_KNOTS ( 'NONE', 3,
 ( #57822, #66780, #101986, #84641, #7938, #42107, #51063, #76254, #93583, #85193, #9043, #25824, #42654, #60025 ),
 .UNSPECIFIED., .F., .F.,
 ( 4, 2, 1, 1, 1, 1, 2, 2, 4 ),
 ( 0.000000000000000000, 0.2499999999999296119, 0.3749999999998988587, 0.4374999999998812616, 0.4687499999998721023, 0.4843749999998657740, 0.4921874999998628319, 0.4999999999998597788, 1.000000000000000000 ),
 .UNSPECIFIED. ) ;
#65741 = CARTESIAN_POINT ( 'NONE',  ( 6.552897366944999469, 1516.858146885269889, 202.5651945608169910 ) ) ;
#65742 = CARTESIAN_POINT ( 'NONE',  ( 7.800031391840000161, 1426.737474522780076, 212.0503234373089754 ) ) ;
#65744 = CARTESIAN_POINT ( 'NONE',  ( -13.56343219680000090, 1416.311719779230089, 221.8446948800979897 ) ) ;
#65743 = AXIS2_PLACEMENT_3D ( 'NONE', #39075, #99528, #47505 ) ;
#65745 = CARTESIAN_POINT ( 'NONE',  ( 15.07517727483500103, 1511.972232048389969, 196.8177839844669847 ) ) ;
#65746 = FACE_BOUND ( 'NONE', #17004, .T. ) ;
#65747 = LINE ( 'NONE', #41638, #9002 ) ;
#65748 = CARTESIAN_POINT ( 'NONE',  ( 19.77968988581690013, 1507.818078778149811, 229.2755617519239877 ) ) ;
#65750 = ORIENTED_EDGE ( 'NONE', *, *, #7769, .T. ) ;
#65749 = CARTESIAN_POINT ( 'NONE',  ( -43.31858137841459921, 1379.664109115149813, 233.3688221966910135 ) ) ;
#65751 = VERTEX_POINT ( 'NONE', #102603 ) ;
#65752 = CARTESIAN_POINT ( 'NONE',  ( -10.98463078130000170, 1397.930555569230137, 216.8780141624080215 ) ) ;
#65753 = CARTESIAN_POINT ( 'NONE',  ( -21.49107218889999871, 1409.827664247030043, 214.8354072608880188 ) ) ;
#65754 = ORIENTED_EDGE ( 'NONE', *, *, #50753, .T. ) ;
#65755 = CARTESIAN_POINT ( 'NONE',  ( -13.01504163501136802, 1444.865561423528334, 169.4190877585964472 ) ) ;
#65756 = CARTESIAN_POINT ( 'NONE',  ( 21.64833465062206841, 1509.708313661343936, 229.4903290947612504 ) ) ;
#65757 = CARTESIAN_POINT ( 'NONE',  ( -7.772759728185000938, 1512.089957059379913, 211.9637779886270152 ) ) ;
#65758 =( BOUNDED_SURFACE ( )  B_SPLINE_SURFACE ( 3, 2, ( 
 ( #28550, #70582, #37499 ),
 ( #46476, #71705, #27436 ),
 ( #70038, #12282, #19584 ),
 ( #78403, #2279, #61619 ),
 ( #20136, #87925, #36393 ),
 ( #63826, #3923, #44261 ),
 ( #11212, #79515, #95751 ),
 ( #45375, #19015, #87357 ),
 ( #80608, #88459, #80051 ),
 ( #96867, #104699, #10653 ),
 ( #54330, #36938, #71135 ),
 ( #38053, #54871, #105256 ),
 ( #27994, #62749, #3372 ),
 ( #105823, #72230, #29101 ) ),
 .UNSPECIFIED., .F., .F., .F. ) 
 B_SPLINE_SURFACE_WITH_KNOTS ( ( 4, 2, 2, 2, 2, 2, 4 ),
 ( 3, 3 ),
 ( 0.000000000000000000, 0.0009440840677143907175, 0.001416126101571585968, 0.001888168135428781435, 0.002360210169285976468, 0.002832252203143171936, 0.003776336270857562870 ),
 ( 0.000000000000000000, 1.000000000000000000 ),
 .UNSPECIFIED. ) 
 GEOMETRIC_REPRESENTATION_ITEM ( )  RATIONAL_B_SPLINE_SURFACE ( (
 ( 1.000000000000000000, 0.8070209408750022018, 1.000000000000000000),
 ( 1.000000000000000000, 0.8215603905293340503, 1.000000000000000000),
 ( 1.000000000000000000, 0.8340988699048569321, 1.000000000000000000),
 ( 1.000000000000000000, 0.8516751610464702305, 1.000000000000000000),
 ( 1.000000000000000000, 0.8573697395148289768, 1.000000000000000000),
 ( 1.000000000000000000, 0.8683586635668048004, 1.000000000000000000),
 ( 1.000000000000000000, 0.8736518481710696671, 1.000000000000000000),
 ( 1.000000000000000000, 0.8840377753027998109, 1.000000000000000000),
 ( 1.000000000000000000, 0.8891294171305048621, 1.000000000000000000),
 ( 1.000000000000000000, 0.8992456600575216008, 1.000000000000000000),
 ( 1.000000000000000000, 0.9042785869253413544, 1.000000000000000000),
 ( 1.000000000000000000, 0.9189749222837514386, 1.000000000000000000),
 ( 1.000000000000000000, 0.9283978182349121866, 1.000000000000000000),
 ( 1.000000000000000000, 0.9376006582765940012, 1.000000000000000000) ) ) 
 REPRESENTATION_ITEM ( '' )  SURFACE ( )  );
#65760 = CARTESIAN_POINT ( 'NONE',  ( -14.19446170199559987, 1509.352195767969761, 183.2680670197790107 ) ) ;
#65759 = CARTESIAN_POINT ( 'NONE',  ( -2.253566441613126910E-10, 1426.918876941764893, 134.0999999980980135 ) ) ;
#65761 = CARTESIAN_POINT ( 'NONE',  ( 3.344599308599999876, 1449.236580124219927, 184.0881402263979965 ) ) ;
#65762 = CARTESIAN_POINT ( 'NONE',  ( -4.675548249330949702, 1462.620864918090092, 200.5633472018479893 ) ) ;
#65763 = CARTESIAN_POINT ( 'NONE',  ( 1.362472229929999834, 1423.807295244410170, 191.1810882058989876 ) ) ;
#65764 = CARTESIAN_POINT ( 'NONE',  ( 7.695515934043100081, 1396.181793810000045, 201.1942046015250014 ) ) ;
#65765 = CARTESIAN_POINT ( 'NONE',  ( 0.6414547015549999509, 1416.067629290630066, 190.6212042380979881 ) ) ;
#65766 = CARTESIAN_POINT ( 'NONE',  ( 11.68304837730000045, 1426.648785231629972, 147.7179971800979956 ) ) ;
#65767 = CARTESIAN_POINT ( 'NONE',  ( 8.590023996720262289, 1509.213085694760821, 181.0924370714511440 ) ) ;
#65768 = EDGE_LOOP ( 'NONE', ( #67989, #47592, #19302, #20406 ) ) ;
#65769 = CARTESIAN_POINT ( 'NONE',  ( 12.97954183294099906, 1434.770645735859944, 149.2712075224750095 ) ) ;
#65770 = CARTESIAN_POINT ( 'NONE',  ( 2.500000195207620290, 1448.894380947069976, 182.3534016008459844 ) ) ;
#65771 = ORIENTED_EDGE ( 'NONE', *, *, #25483, .F. ) ;
#65772 = ORIENTED_EDGE ( 'NONE', *, *, #43284, .T. ) ;
#65773 = ADVANCED_FACE ( 'NONE', ( #19730 ), #108204, .T. ) ;
#65774 = CARTESIAN_POINT ( 'NONE',  ( -17.07194142410000026, 1458.267783243329859, 228.1906384420979919 ) ) ;
#65775 = CARTESIAN_POINT ( 'NONE',  ( -13.48270089159999863, 1461.679658884430182, 230.3973540560979814 ) ) ;
#65776 = CIRCLE ( 'NONE', #17443, 9.522913805090002626 ) ;
#65777 = CARTESIAN_POINT ( 'NONE',  ( -109.1276752832161208, 1387.534014296270470, 310.9046063671660249 ) ) ;
#65778 = CARTESIAN_POINT ( 'NONE',  ( 6.555393117025000826, 1516.809497469189864, 216.4498952504870033 ) ) ;
#65779 = CARTESIAN_POINT ( 'NONE',  ( -13.83795085007070114, 1380.065366606389944, 208.6746515825599886 ) ) ;
#65780 = EDGE_LOOP ( 'NONE', ( #27339, #70613, #34025, #46383 ) ) ;
#65781 = CARTESIAN_POINT ( 'NONE',  ( -12.33713420429999985, 1502.629388698589992, 208.8300189963289881 ) ) ;
#65782 = CARTESIAN_POINT ( 'NONE',  ( 2.500000000000000000, 1448.216386378729794, 167.2100391009490181 ) ) ;
#65783 = CARTESIAN_POINT ( 'NONE',  ( -52.12027059030000231, 1375.939285429470146, 241.5351867029590096 ) ) ;
#65784 = ORIENTED_EDGE ( 'NONE', *, *, #9946, .T. ) ;
#65785 = CARTESIAN_POINT ( 'NONE',  ( -2.879956963085000154, 1516.827328999679821, 205.8693153165069702 ) ) ;
#65786 = ORIENTED_EDGE ( 'NONE', *, *, #21486, .F. ) ;
#65787 = CARTESIAN_POINT ( 'NONE',  ( -7.724874651314999952, 1517.139320148880188, 208.3815253650730028 ) ) ;
#65788 = CARTESIAN_POINT ( 'NONE',  ( -20.11539149109999869, 1508.359231761630099, 229.0631537309980104 ) ) ;
#65789 = CARTESIAN_POINT ( 'NONE',  ( -29.98137141540891903, 1419.563817194629792, 269.4706080157307042 ) ) ;
#65790 = CARTESIAN_POINT ( 'NONE',  ( 6.372167600554999645, 1511.069621805459974, 216.5183910133669940 ) ) ;
#65792 = ORIENTED_EDGE ( 'NONE', *, *, #75449, .F. ) ;
#65791 = CARTESIAN_POINT ( 'NONE',  ( -0.3266950887954889748, 1415.429375168339902, 226.7788835740809930 ) ) ;
#65793 = CARTESIAN_POINT ( 'NONE',  ( 24.56509548029999834, 1440.948408367609773, 213.0043227547379843 ) ) ;
#65794 = CARTESIAN_POINT ( 'NONE',  ( -27.22136134539860208, 1440.913060408979845, 227.8408515943710029 ) ) ;
#65796 = CARTESIAN_POINT ( 'NONE',  ( -54.29265189920000267, 1383.804803630430115, 270.2912082677589751 ) ) ;
#65795 = AXIS2_PLACEMENT_3D ( 'NONE', #82198, #72190, #63246 ) ;
#65797 = CARTESIAN_POINT ( 'NONE',  ( -0.4726113425640879884, 1465.085982962939852, 236.9699332437729993 ) ) ;
#65798 = CARTESIAN_POINT ( 'NONE',  ( 8.322172261349999545, 1408.217606231929949, 270.1222559176979416 ) ) ;
#65799 = CARTESIAN_POINT ( 'NONE',  ( -7.324914956285000223, 1516.685667699390024, 213.7393364370070117 ) ) ;
#65800 = CONICAL_SURFACE ( 'NONE', #40691, 0.9999999999999910072, 0.7853981633970000820 ) ;
#65801 = CARTESIAN_POINT ( 'NONE',  ( 24.10111531969999987, 1410.845843824029998, 208.8643776631820117 ) ) ;
#65802 = CARTESIAN_POINT ( 'NONE',  ( 29.61692403810791419, 1526.104292489129193, 197.4873780791076001 ) ) ;
#65803 = CARTESIAN_POINT ( 'NONE',  ( 2.634457758659999538, 1441.548974666690128, 218.6895019696289921 ) ) ;
#65804 = VECTOR ( 'NONE', #70776, 1000.000000000000000 ) ;
#65806 = ADVANCED_FACE ( 'NONE', ( #99171 ), #37641, .F. ) ;
#65805 = CARTESIAN_POINT ( 'NONE',  ( -7.709335680692180226, 1516.545910801970194, 210.8355061257960017 ) ) ;
#65807 = CARTESIAN_POINT ( 'NONE',  ( 4.044319887224999910, 1517.073005577650065, 210.2423896678870108 ) ) ;
#65808 = EDGE_CURVE ( 'NONE', #22289, #71455, #106555, .T. ) ;
#65809 = CARTESIAN_POINT ( 'NONE',  ( 9.658808656759559241, 1434.868392548590009, 207.4898433114610157 ) ) ;
#65810 = CARTESIAN_POINT ( 'NONE',  ( 0.4542301007209999519, 1418.679722665129930, 184.7067504190980003 ) ) ;
#65811 = CARTESIAN_POINT ( 'NONE',  ( 10.97799415081370000, 1432.849868510099896, 151.7696862706320076 ) ) ;
#65812 = EDGE_CURVE ( 'NONE', #74706, #95667, #61577, .T. ) ;
#65814 = ORIENTED_EDGE ( 'NONE', *, *, #16467, .F. ) ;
#65813 = CARTESIAN_POINT ( 'NONE',  ( -41.51449232029999337, 1389.658647050520131, 237.5849401716589853 ) ) ;
#65815 = CARTESIAN_POINT ( 'NONE',  ( -53.14043027547860021, 1385.103307817649920, 268.1312696023829858 ) ) ;
#65816 = FACE_OUTER_BOUND ( 'NONE', #107355, .T. ) ;
#65817 = EDGE_CURVE ( 'NONE', #14716, #46630, #15094, .T. ) ;
#65818 = CARTESIAN_POINT ( 'NONE',  ( -3.743571413909633439, 1370.323971799861056, 208.2444943395997825 ) ) ;
#65819 = ADVANCED_FACE ( 'NONE', ( #37085 ), #22545, .F. ) ;
#65820 = LINE ( 'NONE', #7548, #29446 ) ;
#65821 = CARTESIAN_POINT ( 'NONE',  ( 12.72079913470000001, 1426.539370631579914, 203.1228655698189982 ) ) ;
#65822 = CARTESIAN_POINT ( 'NONE',  ( 17.71193101166619854, 1517.151704408390060, 196.6727161458730109 ) ) ;
#65823 = EDGE_CURVE ( 'NONE', #108510, #91781, #105963, .T. ) ;
#65825 = CARTESIAN_POINT ( 'NONE',  ( -7.545064089280000275, 1384.907233277360092, 219.0876311325589825 ) ) ;
#65824 = CARTESIAN_POINT ( 'NONE',  ( -4.034280953785000179, 1517.049325831759916, 216.0701676760970145 ) ) ;
#65826 = CARTESIAN_POINT ( 'NONE',  ( -29.31378141421994599, 1450.601296382764986, 136.3806906879467249 ) ) ;
#65827 = FACE_OUTER_BOUND ( 'NONE', #38255, .T. ) ;
#65828 = VECTOR ( 'NONE', #20637, 1000.000000000000000 ) ;
#65829 = VERTEX_POINT ( 'NONE', #46620 ) ;
#65830 = CARTESIAN_POINT ( 'NONE',  ( 3.259101798884999734, 1517.102359858469754, 202.1722709844570147 ) ) ;
#65831 = CARTESIAN_POINT ( 'NONE',  ( -14.72576942166499947, 1512.123542805230272, 221.3115653187670091 ) ) ;
#65832 = CARTESIAN_POINT ( 'NONE',  ( 0.08771972261379999691, 1467.621255356930078, 229.4461896818980051 ) ) ;
#65833 = DIRECTION ( 'NONE',  ( -0.000000000000000000, -1.000000000000000000, -0.000000000000000000 ) ) ;
#65834 = CARTESIAN_POINT ( 'NONE',  ( 10.93915268089999948, 1461.376312761390182, 209.8459655709470155 ) ) ;
#65835 = CARTESIAN_POINT ( 'NONE',  ( 8.462050346931258460, 1424.499487015235445, 195.8146675219503265 ) ) ;
#65836 = ADVANCED_FACE ( 'NONE', ( #80750 ), #29784, .T. ) ;
#65837 = CARTESIAN_POINT ( 'NONE',  ( 25.97508195616575577, 1450.776908619160849, 136.7573643306957933 ) ) ;
#65838 = CARTESIAN_POINT ( 'NONE',  ( 15.21669680536202485, 1420.730405204549470, 227.8538932186329191 ) ) ;
#65839 = CARTESIAN_POINT ( 'NONE',  ( 40.26396420611710170, 1444.186530323160014, 137.1012295353969819 ) ) ;
#65840 = CARTESIAN_POINT ( 'NONE',  ( -19.52413277859999852, 1426.414269502929756, 225.5212833970979887 ) ) ;
#65841 = CARTESIAN_POINT ( 'NONE',  ( 8.324709289579081073, 1487.559664528698477, 202.1769454163824946 ) ) ;
#65842 = CARTESIAN_POINT ( 'NONE',  ( -108.6690692859999956, 1387.662519259070223, 297.7628581251590276 ) ) ;
#65843 = CARTESIAN_POINT ( 'NONE',  ( 18.72056918370000034, 1488.305367430329852, 189.2161702103979906 ) ) ;
#65844 = CARTESIAN_POINT ( 'NONE',  ( 20.70484064406364766, 1525.907212628473872, 185.0411015109854134 ) ) ;
#65845 = EDGE_CURVE ( 'NONE', #7591, #19696, #68781, .T. ) ;
#65846 = CARTESIAN_POINT ( 'NONE',  ( -29.77122833299150173, 1462.416651616063064, 269.4683881299069412 ) ) ;
#65847 = ORIENTED_EDGE ( 'NONE', *, *, #18037, .T. ) ;
#65848 = CARTESIAN_POINT ( 'NONE',  ( -9.157162863174900025, 1440.811664631680060, 204.9830593813619828 ) ) ;
#65849 = CARTESIAN_POINT ( 'NONE',  ( 10.26696809936899513, 1506.473666147782524, 189.6435125623585520 ) ) ;
#65850 = EDGE_CURVE ( 'NONE', #31132, #55319, #56209, .T. ) ;
#65851 = CARTESIAN_POINT ( 'NONE',  ( 31.12456774391174719, 1525.960063244516959, 201.1524202391562710 ) ) ;
#65852 = CARTESIAN_POINT ( 'NONE',  ( -5.164876290100000489, 1519.913060387329779, 231.9023197776979828 ) ) ;
#65853 = DIRECTION ( 'NONE',  ( -1.755985294532469921E-16, 1.000000000000000000, -1.338183447452831989E-16 ) ) ;
#65854 = CARTESIAN_POINT ( 'NONE',  ( -12.63725134787329196, 1442.793345748885940, 186.0969688226275593 ) ) ;
#65855 = CARTESIAN_POINT ( 'NONE',  ( -8.783092974434230982, 1437.856998031400053, 209.9037047230029884 ) ) ;
#65856 = CARTESIAN_POINT ( 'NONE',  ( -3.582837879391600033, 1515.224507406410112, 213.1990887901850158 ) ) ;
#65857 = EDGE_CURVE ( 'NONE', #34471, #23280, #51826, .T. ) ;
#65858 = CARTESIAN_POINT ( 'NONE',  ( 0.000000000000000000, 1518.913060387330006, 209.1218459616979999 ) ) ;
#65859 = CARTESIAN_POINT ( 'NONE',  ( -15.17835049509060141, 1415.677402202029953, 208.2345230821440225 ) ) ;
#65860 = CARTESIAN_POINT ( 'NONE',  ( 18.27452169968656293, 1424.830735475889469, 227.7277621568871098 ) ) ;
#65861 = B_SPLINE_CURVE_WITH_KNOTS ( 'NONE', 5,
 ( #27267, #20496, #96691, #12118, #78780, #104527, #11026, #36775, #26703, #36223, #87178, #61450 ),
 .UNSPECIFIED., .F., .F.,
 ( 6, 3, 3, 6 ),
 ( 0.000000000000000000, 0.2059268257605248176, 0.6177804772432864411, 1.000000000000000000 ),
 .UNSPECIFIED. ) ;
#65862 = CARTESIAN_POINT ( 'NONE',  ( -13.14393378692782299, 1443.063090240467091, 169.3993137622184690 ) ) ;
#65864 = ORIENTED_EDGE ( 'NONE', *, *, #60452, .T. ) ;
#65863 = CARTESIAN_POINT ( 'NONE',  ( 18.02077237764099849, 1424.321284042770003, 225.1939596517550228 ) ) ;
#65865 = CARTESIAN_POINT ( 'NONE',  ( -0.2707663694140940436, 1415.088012641449950, 192.1592658664270061 ) ) ;
#65866 = CARTESIAN_POINT ( 'NONE',  ( 21.91509308718912763, 1509.516311612268055, 226.8168978660500841 ) ) ;
#65867 = ORIENTED_EDGE ( 'NONE', *, *, #99821, .T. ) ;
#65868 = VERTEX_POINT ( 'NONE', #107043 ) ;
#65869 = CARTESIAN_POINT ( 'NONE',  ( 16.20819593131900049, 1414.913060387399810, 209.7580636464409736 ) ) ;
#65870 = CARTESIAN_POINT ( 'NONE',  ( -8.862456919400310440, 1384.912279086194303, 218.6852231908899569 ) ) ;
#65872 = CARTESIAN_POINT ( 'NONE',  ( -21.29700444710000085, 1453.723742755830017, 225.2777522932979934 ) ) ;
#65871 = CARTESIAN_POINT ( 'NONE',  ( 3.067487128190000245, 1454.793378140790082, 218.0351595015090140 ) ) ;
#65873 = B_SPLINE_CURVE_WITH_KNOTS ( 'NONE', 5,
 ( #40543, #83642, #99879, #57379, #90942, #6937, #91506, #74718, #100449, #23732, #32145, #41094 ),
 .UNSPECIFIED., .F., .F.,
 ( 6, 3, 3, 6 ),
 ( 22.07912247049999976, 24.05556723879999836, 24.39387767419999875, 25.37426196462180172 ),
 .UNSPECIFIED. ) ;
#65874 = CARTESIAN_POINT ( 'NONE',  ( -2.707190781069999996, 1444.178722878989902, 218.0787341613589945 ) ) ;
#65875 = VECTOR ( 'NONE', #70251, 1000.000000000000000 ) ;
#65876 = CARTESIAN_POINT ( 'NONE',  ( -11.17646686400000000, 1433.232109516899982, 151.6158427537980060 ) ) ;
#65877 = CARTESIAN_POINT ( 'NONE',  ( 12.68801352610000066, 1500.413650637289948, 208.6561538998189747 ) ) ;
#65878 = CARTESIAN_POINT ( 'NONE',  ( 9.674883418626309961, 1463.833330980269920, 210.7190143815600152 ) ) ;
#65879 = CIRCLE ( 'NONE', #17557, 1.999994602259498100 ) ;
#65880 = CARTESIAN_POINT ( 'NONE',  ( -25.39849853130000312, 1438.598112496549902, 138.1525938156979976 ) ) ;
#65881 = CARTESIAN_POINT ( 'NONE',  ( -24.88010259380000022, 1440.326081558280066, 210.4197093850879980 ) ) ;
#65882 = FACE_BOUND ( 'NONE', #15591, .T. ) ;
#65883 = CARTESIAN_POINT ( 'NONE',  ( -11.54258847144769895, 1481.005615187450076, 211.6768298937909947 ) ) ;
#65884 = VECTOR ( 'NONE', #109365, 999.9999999999998863 ) ;
#65885 = CARTESIAN_POINT ( 'NONE',  ( 8.796059898617141215, 1362.759824263836208, 210.6218459616987957 ) ) ;
#65886 = CARTESIAN_POINT ( 'NONE',  ( 32.92528853941135480, 1523.611961620354123, 201.0067946816160713 ) ) ;
#65887 = EDGE_CURVE ( 'NONE', #27055, #18369, #15674, .T. ) ;
#65889 = ORIENTED_EDGE ( 'NONE', *, *, #83766, .T. ) ;
#65888 = CARTESIAN_POINT ( 'NONE',  ( 1.509834891803940062E-08, 1407.459576716519905, 264.1073148544030005 ) ) ;
#65890 = ORIENTED_EDGE ( 'NONE', *, *, #45419, .T. ) ;
#65891 = CARTESIAN_POINT ( 'NONE',  ( -11.78481361938159999, 1427.587923050230074, 147.3447378541869739 ) ) ;
#65892 = TOROIDAL_SURFACE ( 'NONE', #83772, 32.13701971169416538, 1.000000000000000000 ) ;
#65893 = ADVANCED_FACE ( 'NONE', ( #16260 ), #48259, .F. ) ;
#65894 = CARTESIAN_POINT ( 'NONE',  ( 13.65193357110329941, 1498.714159422929924, 227.8242311217019846 ) ) ;
#65895 = CARTESIAN_POINT ( 'NONE',  ( -4.259181586709999578, 1473.442099373829933, 270.3898288651980124 ) ) ;
#65896 = DIRECTION ( 'NONE',  ( 0.4794255386042040601, 0.000000000000000000, 0.8775825618903722036 ) ) ;
#65897 = CARTESIAN_POINT ( 'NONE',  ( -124.1574587856573828, 1375.179104070688027, 298.3450194382638756 ) ) ;
#65898 = CARTESIAN_POINT ( 'NONE',  ( -13.71487111490000110, 1452.409042808630147, 223.1592556243980141 ) ) ;
#65899 = CARTESIAN_POINT ( 'NONE',  ( 0.2795316912186849856, 1451.161107430230004, 182.2471984510860068 ) ) ;
#65900 = CARTESIAN_POINT ( 'NONE',  ( -20.22049527400000102, 1484.072692924690045, 213.0524004518590004 ) ) ;
#65901 = DIRECTION ( 'NONE',  ( -0.9455185755993178454, 0.000000000000000000, 0.3255681544571537578 ) ) ;
#65902 = CARTESIAN_POINT ( 'NONE',  ( -3.840466235669999673, 1457.048098735890107, 217.8269071805590045 ) ) ;
#65903 = CARTESIAN_POINT ( 'NONE',  ( 10.75464559463706671, 1366.583021909888885, 210.6218459617030021 ) ) ;
#65904 = CARTESIAN_POINT ( 'NONE',  ( -28.99670781314710055, 1413.665506641640150, 266.8891590342930158 ) ) ;
#65905 = VERTEX_POINT ( 'NONE', #82402 ) ;
#65906 = CARTESIAN_POINT ( 'NONE',  ( -4.328976357965290234, 1515.082833801179959, 210.4724564393140156 ) ) ;
#65907 = VERTEX_POINT ( 'NONE', #50463 ) ;
#65908 = ORIENTED_EDGE ( 'NONE', *, *, #20676, .T. ) ;
#65909 = CARTESIAN_POINT ( 'NONE',  ( 6.950833530105000158, 1517.156142772249950, 211.6057959108269984 ) ) ;
#65910 = ADVANCED_FACE ( 'NONE', ( #33079 ), #13382, .T. ) ;
#65911 = CARTESIAN_POINT ( 'NONE',  ( 34.00753574056176376, 1443.913060387329097, 154.9193549732159454 ) ) ;
#65912 = CARTESIAN_POINT ( 'NONE',  ( 41.43280085394450651, 1444.114101214960101, 136.4350172471320093 ) ) ;
#65913 = CIRCLE ( 'NONE', #47993, 32.13701971169416538 ) ;
#65915 = CARTESIAN_POINT ( 'NONE',  ( -3.869313214925711897, 1441.524545288032868, 170.5363236963821123 ) ) ;
#65914 = CARTESIAN_POINT ( 'NONE',  ( -5.772403812434999892, 1516.676340709600026, 212.3853678745870184 ) ) ;
#65916 = CARTESIAN_POINT ( 'NONE',  ( -17.59820799470000097, 1455.456540126329855, 190.1371769522980060 ) ) ;
#65917 = CARTESIAN_POINT ( 'NONE',  ( -2.230120725627048994, 1449.898333919053584, 182.9323432209308464 ) ) ;
#65918 = ORIENTED_EDGE ( 'NONE', *, *, #43865, .F. ) ;
#65919 = CARTESIAN_POINT ( 'NONE',  ( -26.79956309869999842, 1435.440280005279874, 135.4702187632980213 ) ) ;
#65920 = CARTESIAN_POINT ( 'NONE',  ( 2.289624432225000117, 1517.154223579619838, 202.5582500624169882 ) ) ;
#65921 = B_SPLINE_CURVE_WITH_KNOTS ( 'NONE', 3,
 ( #17448, #68461, #33718, #43790, #76847, #18015 ),
 .UNSPECIFIED., .F., .F.,
 ( 4, 2, 4 ),
 ( 0.000000000000000000, 0.5000000000000000000, 1.000000000000000000 ),
 .UNSPECIFIED. ) ;
#65922 = ADVANCED_FACE ( 'NONE', ( #108138 ), #34015, .T. ) ;
#65923 = CARTESIAN_POINT ( 'NONE',  ( -32.02808312589908013, 1511.187213306747708, 219.9649204700466782 ) ) ;
#65924 = CARTESIAN_POINT ( 'NONE',  ( -10.93176275610840165, 1384.512863483779938, 200.1239762818750023 ) ) ;
#65925 = CARTESIAN_POINT ( 'NONE',  ( -42.28242862210569797, 1440.913046154859785, 269.8809742447210169 ) ) ;
#65926 = DIRECTION ( 'NONE',  ( 1.755985294532464991E-16, -1.000000000000000000, 1.338183447452830017E-16 ) ) ;
#65927 = CARTESIAN_POINT ( 'NONE',  ( -4.487375328049999723, 1396.069762987030117, 198.6459191643980091 ) ) ;
#65928 = EDGE_CURVE ( 'NONE', #67449, #15423, #12040, .T. ) ;
#65930 = ORIENTED_EDGE ( 'NONE', *, *, #72276, .F. ) ;
#65929 = CARTESIAN_POINT ( 'NONE',  ( -9.832966357650001044, 1364.062280235949856, 207.6218459616989946 ) ) ;
#65931 = ORIENTED_EDGE ( 'NONE', *, *, #78971, .F. ) ;
#65932 = CARTESIAN_POINT ( 'NONE',  ( 0.4061596876509999676, 1451.157747844730238, 182.5691048874980140 ) ) ;
#65933 = CARTESIAN_POINT ( 'NONE',  ( -4.993214560040000194, 1391.653934889589891, 203.5347113830289913 ) ) ;
#65934 = CARTESIAN_POINT ( 'NONE',  ( 10.75296554538699922, 1460.440714502600031, 207.1959050312180182 ) ) ;
#65935 = LINE ( 'NONE', #90003, #15294 ) ;
#65936 = CARTESIAN_POINT ( 'NONE',  ( -0.03698025251986000739, 1409.854707136450088, 185.1104546373300082 ) ) ;
#65937 = CARTESIAN_POINT ( 'NONE',  ( -5.770820179264999794, 1516.591755933730155, 210.8331571987770019 ) ) ;
#65938 = CARTESIAN_POINT ( 'NONE',  ( 8.852952242565432783, 1461.582927576305110, 205.0540815658535507 ) ) ;
#65939 = CARTESIAN_POINT ( 'NONE',  ( -10.10004869885203682, 1411.254281879943164, 137.0999999980979851 ) ) ;
#65940 = CARTESIAN_POINT ( 'NONE',  ( 4.948204956154519607, 1440.721229042110053, 216.9276863776850064 ) ) ;
#65941 = DIRECTION ( 'NONE',  ( 5.980589973904019347E-17, -1.000000000000000000, 1.736889445713099699E-16 ) ) ;
#65942 = EDGE_CURVE ( 'NONE', #47384, #81952, #25004, .T. ) ;
#65943 = CARTESIAN_POINT ( 'NONE',  ( 11.75111438890000137, 1446.815402695709963, 187.7955925520979861 ) ) ;
#65944 = CARTESIAN_POINT ( 'NONE',  ( 4.995623452895000760, 1516.636036526019780, 207.4092012159470073 ) ) ;
#65945 = EDGE_LOOP ( 'NONE', ( #27467, #37688, #91104, #103610 ) ) ;
#65946 = CARTESIAN_POINT ( 'NONE',  ( -38.81202644819489933, 1450.612734570859857, 134.4203407196499995 ) ) ;
#65947 = FACE_OUTER_BOUND ( 'NONE', #17541, .T. ) ;
#65948 = CARTESIAN_POINT ( 'NONE',  ( -8.743364905860000036, 1385.034306932410118, 218.5834041657990099 ) ) ;
#65949 = VERTEX_POINT ( 'NONE', #71988 ) ;
#65950 = CARTESIAN_POINT ( 'NONE',  ( -29.61076903484010003, 1526.107876515966609, 197.4926634013643252 ) ) ;
#65951 = EDGE_CURVE ( 'NONE', #51216, #94817, #97357, .T. ) ;
#65952 = CARTESIAN_POINT ( 'NONE',  ( 12.89586781552239891, 1434.724716683040242, 149.2198538527470077 ) ) ;
#65953 = B_SPLINE_SURFACE_WITH_KNOTS ( 'NONE', 5, 5, ( 
 ( #36361, #1680, #86766, #35821, #61588, #87326, #10622, #95721, #69444 ),
 ( #18986, #96275, #105231, #26863, #19553, #53759, #28519, #62719, #80026 ),
 ( #37471, #96840, #61051, #95173, #18429, #88966, #71674, #29075, #97369 ),
 ( #43669, #52629, #63794, #57049, #31819, #38557, #107970, #23412, #55389 ),
 ( #91175, #81653, #82217, #56485, #72736, #73280, #106861, #47532, #14454 ),
 ( #100128, #12811, #82775, #66007, #90616, #97908, #98466, #31267, #3894 ),
 ( #55938, #90058, #5520, #21179, #4959, #80579, #48648, #30153, #39102 ),
 ( #40221, #29609, #73843, #22843, #65450, #13896, #13340, #64345, #57605 ),
 ( #74402, #38024, #72203, #107417, #30714, #89519, #99559, #64899, #46990 ),
 ( #81114, #4431, #99007, #22283, #21736, #106326, #39676, #48083, #6068 ),
 ( #46447, #108528, #12257, #33452, #109637, #25605, #76032, #102318, #34022 ),
 ( #6619, #26160, #92824, #58144, #8256, #32379, #16098, #51378, #66561 ),
 ( #453, #7177, #76580, #102863, #23947, #49744, #59797, #50303, #50833 ),
 ( #93917, #85512, #110732, #14997, #84431, #100664, #93370, #8808, #68214 ),
 ( #92275, #84964, #67653, #16637, #42422, #7716, #41876, #17184, #40773 ),
 ( #42991, #110180, #68759, #101761, #15544, #77149, #25050, #34574, #91723 ),
 ( #59252, #49196, #41333, #83324, #83872, #74950, #109099, #101205, #75503 ),
 ( #32910, #67103, #24501, #58691, #78797, #45770, #86631, #53621, #1001 ),
 ( #36792, #69869, #70984, #51943, #104544, #9925, #10485, #44096, #95590 ),
 ( #9380, #37346, #60914, #19978, #79906, #27840, #35128, #35679, #45213 ),
 ( #69310, #103985, #27281, #87763, #103417, #53055, #17742, #28390, #78234 ),
 ( #2112, #61464, #19419, #3219, #87193, #86086, #44656, #95042, #18859 ),
 ( #43543, #11044, #79353, #52502, #36238, #26724, #77688, #71544, #18311 ),
 ( #2666, #105100, #96708, #96140, #62020, #105666, #70425, #1547, #60346 ),
 ( #94468, #62591, #54172, #88298, #11592, #73721, #13214, #39546, #82086 ),
 ( #20512, #54721, #74272, #30024, #106197, #56356, #80455, #64217, #99428 ),
 ( #107844, #48514, #55268, #13763, #40090, #72083, #97786, #31133, #98341 ),
 ( #3767, #65317, #22706, #47947, #63138, #21614, #37902, #30590, #56904 ),
 ( #38430, #29479, #22155, #81526, #64778, #98888, #55819, #89938, #5389 ),
 ( #82653, #91037, #47404, #5945, #4828, #63674, #14324, #28949, #97239 ) ),
 .UNSPECIFIED., .F., .F., .F.,
 ( 6, 3, 3, 3, 3, 3, 3, 3, 3, 6 ),
 ( 6, 3, 6 ),
 ( -3.552713678800000397E-15, 15.39383910899999997, 27.58084801740000103, 41.39509552349999666, 65.53909258059999843, 90.91108773649999364, 117.6367619669999982, 132.4493970709999928, 144.8160795070000120, 161.8240513320000105 ),
 ( 2.092690777440000094, 17.86261146360000041, 33.63253214979999939 ),
 .UNSPECIFIED. ) ;
#65954 = CARTESIAN_POINT ( 'NONE',  ( 13.38213216230000135, 1415.140114695929924, 197.3646947084980070 ) ) ;
#65955 = CARTESIAN_POINT ( 'NONE',  ( -1.517310924280000028, 1507.186118470329802, 180.8246499599979984 ) ) ;
#65956 = CARTESIAN_POINT ( 'NONE',  ( 2.461716435160000049, 1435.943783413959864, 150.4083956814980070 ) ) ;
#65957 = CARTESIAN_POINT ( 'NONE',  ( 3.491631218259470426, 1450.859992781919573, 184.0578325456160655 ) ) ;
#65958 = CARTESIAN_POINT ( 'NONE',  ( 7.646098387520000372, 1488.620979909889911, 200.2919901690490008 ) ) ;
#65959 = CARTESIAN_POINT ( 'NONE',  ( -4.958564224928870168, 1476.141795758730041, 200.0452580833139962 ) ) ;
#65960 = CARTESIAN_POINT ( 'NONE',  ( 24.34104170635332665, 1445.460888148215190, 214.1669348561839001 ) ) ;
#65961 = EDGE_CURVE ( 'NONE', #66906, #57154, #81150, .T. ) ;
#65962 = CARTESIAN_POINT ( 'NONE',  ( 41.52362078918107358, 1442.051295106819907, 135.5055851492039380 ) ) ;
#65963 = CIRCLE ( 'NONE', #94537, 11.71219856409999949 ) ;
#65964 = PLANE ( 'NONE',  #53167 ) ;
#65965 = CARTESIAN_POINT ( 'NONE',  ( 1.130002494264999990, 1516.621991115350056, 216.0576472317669925 ) ) ;
#65966 = ORIENTED_EDGE ( 'NONE', *, *, #93216, .T. ) ;
#65967 = CARTESIAN_POINT ( 'NONE',  ( 7.714047019527109583, 1516.725831029360052, 208.3892583435649897 ) ) ;
#65968 = CARTESIAN_POINT ( 'NONE',  ( -5.402393449050000740, 1473.936434490630063, 270.1311850751980046 ) ) ;
#65969 = CIRCLE ( 'NONE', #14049, 1.999999999999993117 ) ;
#65970 = CARTESIAN_POINT ( 'NONE',  ( 0.1115023623899999983, 1420.227194636330069, 183.9075503089979975 ) ) ;
#65971 = EDGE_CURVE ( 'NONE', #50244, #90113, #37152, .T. ) ;
#65972 = ADVANCED_FACE ( 'NONE', ( #36409 ), #38421, .T. ) ;
#65973 = CIRCLE ( 'NONE', #15887, 2.000006069085131344 ) ;
#65974 = CARTESIAN_POINT ( 'NONE',  ( -14.09074480600290080, 1508.447712472369858, 216.3025742391060078 ) ) ;
#65975 = CARTESIAN_POINT ( 'NONE',  ( -2.405152095979999682, 1474.348779541090153, 219.1148944409090120 ) ) ;
#65976 = CARTESIAN_POINT ( 'NONE',  ( 30.54124909559969936, 1510.057079062230059, 213.7077286667680198 ) ) ;
#65977 = CARTESIAN_POINT ( 'NONE',  ( 3.835404308833624043, 1405.413060387330006, 216.1425064568209677 ) ) ;
#65978 = CARTESIAN_POINT ( 'NONE',  ( -3.811293930937523111, 1508.139652414328793, 220.7071210997668516 ) ) ;
#65979 = CARTESIAN_POINT ( 'NONE',  ( 17.90582816991177495, 1423.855356620343855, 225.8115124795609745 ) ) ;
#65980 = CARTESIAN_POINT ( 'NONE',  ( -109.1665242455550100, 1385.079937276020019, 297.1361710942769605 ) ) ;
#65981 = CARTESIAN_POINT ( 'NONE',  ( -22.08523867432538879, 1523.530870145311610, 184.4211813602715893 ) ) ;
#65982 = CARTESIAN_POINT ( 'NONE',  ( 33.88603162083069975, 1440.913060384309802, 248.6081570316809746 ) ) ;
#65983 = B_SPLINE_CURVE_WITH_KNOTS ( 'NONE', 3,
 ( #40517, #74695, #108827, #55699, #94787, #102067 ),
 .UNSPECIFIED., .F., .F.,
 ( 4, 2, 4 ),
 ( -1.131363979617638733E-05, 0.001067788114096024149, 0.002146889867988224614 ),
 .UNSPECIFIED. ) ;
#65985 = CARTESIAN_POINT ( 'NONE',  ( 4.327308595631699895, 1515.146523075020013, 208.6641484814759906 ) ) ;
#65984 = CARTESIAN_POINT ( 'NONE',  ( -10.81513955013129902, 1470.571292273900099, 210.8385438386609962 ) ) ;
#65986 = CARTESIAN_POINT ( 'NONE',  ( 12.88143820049999810, 1419.885573380330015, 222.2329351837979914 ) ) ;
#65987 = VERTEX_POINT ( 'NONE', #8589 ) ;
#65988 = ORIENTED_EDGE ( 'NONE', *, *, #65812, .T. ) ;
#65989 = CARTESIAN_POINT ( 'NONE',  ( 10.53557798318139938, 1481.859448200410043, 210.2581152848169950 ) ) ;
#65990 = CARTESIAN_POINT ( 'NONE',  ( -19.63429367885367682, 1485.335955380609221, 190.2453589707047286 ) ) ;
#65991 = CARTESIAN_POINT ( 'NONE',  ( -28.17856942739999937, 1509.667335739730106, 211.1330165365179994 ) ) ;
#65992 = FACE_OUTER_BOUND ( 'NONE', #54343, .T. ) ;
#65993 = MECHANICAL_DESIGN_GEOMETRIC_PRESENTATION_REPRESENTATION (  '', ( #99919 ), #83860 ) ;
#65994 = CARTESIAN_POINT ( 'NONE',  ( -18.19590854888121356, 1522.382868172863937, 238.2026672068777202 ) ) ;
#65995 = EDGE_CURVE ( 'NONE', #53764, #3178, #97222, .T. ) ;
#65996 = CARTESIAN_POINT ( 'NONE',  ( 20.29103523386016050, 1509.739352328666428, 231.2885314561093253 ) ) ;
#65997 = CARTESIAN_POINT ( 'NONE',  ( -16.81611548244467258, 1526.382868172864164, 234.5451076435288371 ) ) ;
#65998 = CARTESIAN_POINT ( 'NONE',  ( -1.995807793896930082, 1508.551704408389924, 220.0704850252740243 ) ) ;
#65999 = CARTESIAN_POINT ( 'NONE',  ( -47.66019703560549914, 1383.815780539829802, 256.5296040942980085 ) ) ;
#66000 = FACE_OUTER_BOUND ( 'NONE', #41676, .T. ) ;
#66001 = CARTESIAN_POINT ( 'NONE',  ( 5.361946547511959871, 1422.281156908029971, 142.4701046725139975 ) ) ;
#66002 = CARTESIAN_POINT ( 'NONE',  ( -12.12616446094680001, 1502.349690982020093, 208.9415299542270077 ) ) ;
#66003 = CARTESIAN_POINT ( 'NONE',  ( 10.86502470147939903, 1490.656646050969812, 210.7146857633749732 ) ) ;
#66005 = ORIENTED_EDGE ( 'NONE', *, *, #34619, .T. ) ;
#66004 = CARTESIAN_POINT ( 'NONE',  ( 0.4663913465019989824, 1455.963574820090116, 218.7208018874689799 ) ) ;
#66006 = CARTESIAN_POINT ( 'NONE',  ( -1.676216080179999901, 1450.511945511729891, 182.4451616703979937 ) ) ;
#66007 = CARTESIAN_POINT ( 'NONE',  ( -21.97707892889999926, 1380.247610671960047, 205.6383942844589967 ) ) ;
#66008 = CARTESIAN_POINT ( 'NONE',  ( -3.076050021859999983, 1475.159716099690058, 198.5224445511989870 ) ) ;
#66009 = ORIENTED_EDGE ( 'NONE', *, *, #22780, .T. ) ;
#66010 = VERTEX_POINT ( 'NONE', #15865 ) ;
#66011 = CARTESIAN_POINT ( 'NONE',  ( -8.348311995175087930, 1386.164425872750144, 218.5824697249680071 ) ) ;
#66012 = CARTESIAN_POINT ( 'NONE',  ( -4.259777688362290426, 1515.374151772610048, 206.1850293956469784 ) ) ;
#66013 = CARTESIAN_POINT ( 'NONE',  ( 18.19590854888146580, 1522.382868172863937, 180.0410247165184217 ) ) ;
#66014 = CARTESIAN_POINT ( 'NONE',  ( -9.234136244889999290, 1461.205488667689906, 206.1827751366290045 ) ) ;
#66015 = CARTESIAN_POINT ( 'NONE',  ( -104.9457213230000008, 1380.324877816590060, 300.8469997012589943 ) ) ;
#66016 = FACE_OUTER_BOUND ( 'NONE', #97842, .T. ) ;
#66017 = CARTESIAN_POINT ( 'NONE',  ( -13.01051159769479959, 1508.551704408389924, 216.5695640764339771 ) ) ;
#66018 = CARTESIAN_POINT ( 'NONE',  ( 7.067760138535259529, 1409.159872009930041, 195.9246175589510131 ) ) ;
#66019 = FACE_OUTER_BOUND ( 'NONE', #47345, .T. ) ;
#66020 = CARTESIAN_POINT ( 'NONE',  ( -1.862709314156860030, 1485.677233011570252, 197.3688579391329938 ) ) ;
#66021 = LINE ( 'NONE', #67119, #90822 ) ;
#66022 = CARTESIAN_POINT ( 'NONE',  ( -3.655277279608119656, 1441.526510731130202, 166.9096038968010021 ) ) ;
#66023 = AXIS2_PLACEMENT_3D ( 'NONE', #110318, #58823, #67241 ) ;
#66024 = CARTESIAN_POINT ( 'NONE',  ( -3.827327156165859723, 1424.046157831530081, 184.1455916618039907 ) ) ;
#66025 = ORIENTED_EDGE ( 'NONE', *, *, #39427, .F. ) ;
#66026 = CARTESIAN_POINT ( 'NONE',  ( -1.608351468689999786, 1426.598937817530214, 144.1938086916980239 ) ) ;
#66027 = CARTESIAN_POINT ( 'NONE',  ( 18.65411303873779758, 1457.703406872730056, 227.4352212818459975 ) ) ;
#66028 = CARTESIAN_POINT ( 'NONE',  ( -12.19455143910000139, 1434.284752744940079, 150.5224356719979824 ) ) ;
#66029 = CIRCLE ( 'NONE', #28443, 0.5000016051842596232 ) ;
#66030 = CARTESIAN_POINT ( 'NONE',  ( -3.063324380877089998E-10, 1466.672023398390138, 243.8770760458830011 ) ) ;
#66031 = CARTESIAN_POINT ( 'NONE',  ( -31.81407709660758698, 1522.382868172863937, 221.9534378623334305 ) ) ;
#66032 = CARTESIAN_POINT ( 'NONE',  ( -15.09297716350000051, 1420.200853339370269, 212.5836862043790063 ) ) ;
#66033 = CARTESIAN_POINT ( 'NONE',  ( -109.0087032940000000, 1387.252923815580061, 310.8549776262589717 ) ) ;
#66034 = CARTESIAN_POINT ( 'NONE',  ( -8.795269478359751147, 1511.561753607920082, 215.0949048348660142 ) ) ;
#66035 = B_SPLINE_CURVE_WITH_KNOTS ( 'NONE', 3,
 ( #95760, #80060, #47031, #87368, #79524, #106906, #89560 ),
 .UNSPECIFIED., .F., .F.,
 ( 4, 3, 4 ),
 ( -89.03555611550000037, -57.33326531478269317, -17.24302739680000229 ),
 .UNSPECIFIED. ) ;
#66036 = CARTESIAN_POINT ( 'NONE',  ( -9.701269302676793771, 1361.953484705324172, 210.6218459617030021 ) ) ;
#66037 = FACE_OUTER_BOUND ( 'NONE', #69351, .T. ) ;
#66038 = CARTESIAN_POINT ( 'NONE',  ( 13.48944867574859963, 1508.549640178079926, 233.3847123851280116 ) ) ;
#66039 = CARTESIAN_POINT ( 'NONE',  ( -10.22078022364619976, 1448.827725899079724, 207.2905427559460065 ) ) ;
#66040 = CARTESIAN_POINT ( 'NONE',  ( -4.623892098755000291, 1517.066898074209803, 208.3852847535989952 ) ) ;
#66041 = CARTESIAN_POINT ( 'NONE',  ( 6.825986730469999486, 1409.091027440530070, 221.7399762292980085 ) ) ;
#66042 = SURFACE_STYLE_FILL_AREA ( #5564 ) ;
#66043 = CARTESIAN_POINT ( 'NONE',  ( 5.553848058839999879, 1423.191816860230119, 91.03168606369779070 ) ) ;
#66044 = CARTESIAN_POINT ( 'NONE',  ( 7.455126725186649317, 1425.226345695840109, 212.3390874243399935 ) ) ;
#66045 = VECTOR ( 'NONE', #104205, 1000.000000000000000 ) ;
#66046 = VERTEX_POINT ( 'NONE', #50069 ) ;
#66047 = AXIS2_PLACEMENT_3D ( 'NONE', #73731, #15432, #6500 ) ;
#66048 = CARTESIAN_POINT ( 'NONE',  ( 23.87826881430000014, 1432.672873845370077, 221.5017660107979793 ) ) ;
#66049 = CARTESIAN_POINT ( 'NONE',  ( 0.5086982323670009576, 1417.713718859019764, 204.0301965041890071 ) ) ;
#66051 = CARTESIAN_POINT ( 'NONE',  ( -16.63178664779999849, 1409.493855175129966, 194.4517206995979848 ) ) ;
#66050 = CARTESIAN_POINT ( 'NONE',  ( -1.515746652750000312, 1478.158358440429765, 182.0299493565979958 ) ) ;
#66052 = CARTESIAN_POINT ( 'NONE',  ( -19.53786426058999481, 1511.187213306747708, 236.7197124308268030 ) ) ;
#66053 = CARTESIAN_POINT ( 'NONE',  ( -24.09667674930000203, 1426.479304371029912, 238.1639134735980008 ) ) ;
#66054 = CARTESIAN_POINT ( 'NONE',  ( -4.640277423280045888, 1378.166137044523111, 214.4725589679636641 ) ) ;
#66055 = EDGE_CURVE ( 'NONE', #33528, #55613, #90155, .T. ) ;
#66056 = CARTESIAN_POINT ( 'NONE',  ( -22.24479823131389722, 1452.136254915900054, 140.1071540872370065 ) ) ;
#66057 = DIRECTION ( 'NONE',  ( -1.000000000000000000, 0.000000000000000000, 0.000000000000000000 ) ) ;
#66058 = VERTEX_POINT ( 'NONE', #7495 ) ;
#66059 = CARTESIAN_POINT ( 'NONE',  ( -2.500000000000000000, 1422.798905948130141, 153.2868469301980099 ) ) ;
#66060 = CARTESIAN_POINT ( 'NONE',  ( 13.95553492442098431, 1416.818673872114459, 196.3353044460132537 ) ) ;
#66061 = PLANE ( 'NONE',  #22137 ) ;
#66062 = CARTESIAN_POINT ( 'NONE',  ( 11.10442532319999920, 1501.746131285089859, 206.2421527516889626 ) ) ;
#66063 = VERTEX_POINT ( 'NONE', #59023 ) ;
#66064 = ORIENTED_EDGE ( 'NONE', *, *, #82880, .T. ) ;
#66065 = CARTESIAN_POINT ( 'NONE',  ( -37.21633441560000222, 1384.983113612510124, 210.1703949109789846 ) ) ;
#66066 = CARTESIAN_POINT ( 'NONE',  ( -22.77796388237689840, 1409.708471313090058, 209.3294552566549669 ) ) ;
#66067 = ORIENTED_EDGE ( 'NONE', *, *, #68632, .T. ) ;
#66068 = DIRECTION ( 'NONE',  ( 0.9455185755993177343, 0.000000000000000000, -0.3255681544571540909 ) ) ;
#66069 = CIRCLE ( 'NONE', #19513, 2.000012855935070721 ) ;
#66070 = DIRECTION ( 'NONE',  ( -0.9455185755993178454, 0.000000000000000000, 0.3255681544571537578 ) ) ;
#66071 = DIRECTION ( 'NONE',  ( -0.03489949673788425577, -0.9993908270178603059, 4.843886099300351310E-10 ) ) ;
#66072 = CARTESIAN_POINT ( 'NONE',  ( -19.53416072559999961, 1415.852625093730012, 222.3903674702980027 ) ) ;
#66073 = CARTESIAN_POINT ( 'NONE',  ( 42.12374111126599985, 1455.597911166439872, 267.7355564021549412 ) ) ;
#66074 = CARTESIAN_POINT ( 'NONE',  ( -4.678149174004739841, 1508.611352721110052, 205.6342598901590009 ) ) ;
#66075 = CARTESIAN_POINT ( 'NONE',  ( -5.731568358319999668, 1428.367353358390119, 203.0107280175789981 ) ) ;
#66076 = CARTESIAN_POINT ( 'NONE',  ( 0.7360974386200019870, 1517.045004075700035, 205.0794574309270217 ) ) ;
#66077 = VERTEX_POINT ( 'NONE', #25377 ) ;
#66078 = CARTESIAN_POINT ( 'NONE',  ( -2.500000000000000000, 1411.429641636930000, 146.1721969575970093 ) ) ;
#66079 = CARTESIAN_POINT ( 'NONE',  ( 15.10840964654390106, 1512.260118274579781, 196.3980101966029963 ) ) ;
#66080 = CARTESIAN_POINT ( 'NONE',  ( 13.18440430809449460, 1443.101454830199145, 187.5179277441473005 ) ) ;
#66081 = ORIENTED_EDGE ( 'NONE', *, *, #36574, .F. ) ;
#66082 = CARTESIAN_POINT ( 'NONE',  ( -10.55763132505339996, 1480.395020916429985, 210.7122116074530140 ) ) ;
#66083 = ADVANCED_FACE ( 'NONE', ( #40891 ), #74261, .T. ) ;
#66084 = CARTESIAN_POINT ( 'NONE',  ( 26.75523174175490126, 1451.912001146919920, 135.4172217544110026 ) ) ;
#66085 = CARTESIAN_POINT ( 'NONE',  ( -4.363123796622770278, 1423.854800546939941, 184.2546035468919854 ) ) ;
#66086 = CARTESIAN_POINT ( 'NONE',  ( 10.53235956273399943, 1452.545262286839943, 150.3730426087770127 ) ) ;
#66087 = EDGE_CURVE ( 'NONE', #49285, #24021, #110515, .T. ) ;
#66088 = CARTESIAN_POINT ( 'NONE',  ( 7.423896801969999792, 1422.288457550600015, 195.6224997975990334 ) ) ;
#66090 = B_SPLINE_SURFACE_WITH_KNOTS ( 'NONE', 5, 1, ( 
 ( #60856, #18800 ),
 ( #8196, #34516 ),
 ( #77089, #52445 ),
 ( #85450, #26657 ),
 ( #44033, #8748 ),
 ( #52996, #68155 ) ),
 .UNSPECIFIED., .F., .F., .F.,
 ( 6, 6 ),
 ( 2, 2 ),
 ( -8.364788202518770371E-05, 17.30286250248200020 ),
 ( 0.000000000000000000, 14.00008364788200055 ),
 .UNSPECIFIED. ) ;
#66089 = CARTESIAN_POINT ( 'NONE',  ( -0.1950599852922330069, 1431.910904562789938, 218.6163528922420198 ) ) ;
#66091 = CARTESIAN_POINT ( 'NONE',  ( -9.389251474311459233, 1493.203009381459879, 201.1804961733769801 ) ) ;
#66092 = CARTESIAN_POINT ( 'NONE',  ( 10.29233424086269899, 1479.549769955249985, 205.9985512849049769 ) ) ;
#66093 = CARTESIAN_POINT ( 'NONE',  ( 13.04207810306199988, 1409.368499790489750, 192.3005055522939983 ) ) ;
#66095 = CARTESIAN_POINT ( 'NONE',  ( 22.08622291482331335, 1523.382868172864164, 184.4183880513174927 ) ) ;
#66094 = CARTESIAN_POINT ( 'NONE',  ( -13.07075687411459874, 1434.811948465909836, 149.1083925370589895 ) ) ;
#66096 = CARTESIAN_POINT ( 'NONE',  ( 10.86483302107700055, 1425.362906770059908, 206.5122574745630004 ) ) ;
#66097 = EDGE_CURVE ( 'NONE', #44736, #28853, #24041, .T. ) ;
#66098 = CARTESIAN_POINT ( 'NONE',  ( -11.78930676389999910, 1378.156676306969985, 212.7700627114790279 ) ) ;
#66099 = CARTESIAN_POINT ( 'NONE',  ( 9.534219445089998857, 1428.030197386430018, 144.1938086916980239 ) ) ;
#66100 = ORIENTED_EDGE ( 'NONE', *, *, #34757, .F. ) ;
#66101 = CARTESIAN_POINT ( 'NONE',  ( 2.331468351709999880E-15, 1427.913060387330006, 209.1218459616979999 ) ) ;
#66102 = AXIS2_PLACEMENT_3D ( 'NONE', #14544, #48733, #31905 ) ;
#66103 = CARTESIAN_POINT ( 'NONE',  ( -0.09233079908728399066, 1424.283549355850027, 227.6553671107380126 ) ) ;
#66104 = CARTESIAN_POINT ( 'NONE',  ( 31.29224604902393381, 1525.661275128775515, 201.9587785200654650 ) ) ;
#66105 = ADVANCED_FACE ( 'NONE', ( #102852 ), #47657, .F. ) ;
#66106 = B_SPLINE_SURFACE_WITH_KNOTS ( 'NONE', 5, 5, ( 
 ( #17765, #69336, #79377, #44681, #18334, #60938, #70449, #2693, #51969 ),
 ( #95067, #102886, #78826, #86110, #78259, #34600, #36817, #9404, #102347 ),
 ( #26183, #2137, #19446, #25630, #43566, #104569, #59822, #93942, #77717 ),
 ( #44124, #17208, #60372, #85536, #86657, #87219, #27864, #95616, #1028 ),
 ( #35152, #27306, #62044, #103444, #8831, #52525, #51404, #26749, #69894 ),
 ( #96170, #9952, #18883, #43016, #77173, #53081, #35705, #36260, #53644 ),
 ( #1572, #104009, #476, #61487, #87788, #10509, #11070, #68786, #94493 ),
 ( #45239, #63164, #106763, #98913, #21640, #38460, #81554, #105693, #97811 ),
 ( #11619, #21090, #3245, #89967, #56383, #4330, #28976, #30054, #55845 ),
 ( #55293, #13241, #13790, #96734, #72110, #47431, #39001, #46350, #64245 ),
 ( #72634, #89423, #97265, #98367, #20541, #37371, #12713, #4856, #22185 ),
 ( #62617, #20005, #73178, #106224, #107322, #46897, #30617, #105128, #5413 ),
 ( #64804, #90515, #47974, #81021, #82114, #71007, #28419, #54745, #54199 ),
 ( #88875, #45796, #79929, #29508, #12160, #80479, #88324, #71572, #3797 ),
 ( #37928, #63701, #66452, #73745, #91064, #100565, #82677, #58587, #24937 ),
 ( #108427, #75395, #24403, #22733, #56935, #5968, #14348, #6515, #40113 ),
 ( #84321, #15993, #91622, #50195, #109534, #49637, #65347, #23846, #59149 ),
 ( #7068, #41224, #108985, #66993, #32808, #31157, #99455, #41768, #101103 ),
 ( #40668, #92175, #74841, #92717, #58037, #93270, #33353, #48539, #32270 ),
 ( #75925, #74296, #65895, #15446, #16533, #7612, #83774, #110078, #67548 ),
 ( #100012, #31709, #101650, #23302, #50724, #57497, #84855, #14898, #39572 ),
 ( #49089, #83225, #107869, #17079, #25499, #61917, #102220, #69198, #94934 ),
 ( #51274, #60809, #19305, #77040, #59690, #103305, #103882, #87084, #1428 ),
 ( #26046, #17638, #43989, #10368, #51840, #93802, #895, #8155, #85977 ),
 ( #86526, #78124, #27182, #27729, #77588, #69765, #35019, #26613, #68650 ),
 ( #85406, #44542, #35570, #2003, #8705, #33911, #34475, #42883, #348 ),
 ( #18206, #102751, #60239, #96034, #94358, #52403, #9820, #9277, #61365 ) ),
 .UNSPECIFIED., .F., .F., .F.,
 ( 6, 3, 3, 3, 3, 3, 3, 3, 6 ),
 ( 6, 3, 6 ),
 ( 24.02324320159999971, 42.68733206409999781, 75.98967771649999747, 109.6146260670000032, 126.4768870990000096, 132.7991108720000000, 135.9602227580000147, 139.1213346450000188, 143.3324205490000054 ),
 ( 0.000000000000000000, 1.000000000000000000, 2.000000000000000000 ),
 .UNSPECIFIED. ) ;
#66107 = CARTESIAN_POINT ( 'NONE',  ( -8.257938479109999008, 1385.286773756459979, 199.7059428756689954 ) ) ;
#66108 = CARTESIAN_POINT ( 'NONE',  ( 10.31893549361520002, 1422.402437340219876, 211.7674958658010098 ) ) ;
#66109 =( BOUNDED_CURVE ( )  B_SPLINE_CURVE ( 3, ( #16660, #57070, #75525, #91197 ),
 .UNSPECIFIED., .F., .T. ) 
 B_SPLINE_CURVE_WITH_KNOTS ( ( 4, 4 ),
 ( 2.768156387931280271, 3.267547937231884969 ),
 .UNSPECIFIED. ) 
 CURVE ( )  GEOMETRIC_REPRESENTATION_ITEM ( )  RATIONAL_B_SPLINE_CURVE ( ( 1.000000000000000000, 0.9793250956183989775, 0.9793250956183989775, 1.000000000000000000 ) ) 
 REPRESENTATION_ITEM ( '' )  );
#66110 = CARTESIAN_POINT ( 'NONE',  ( 12.02395472744730043, 1421.496668670510189, 203.4303483181410002 ) ) ;
#66111 = CARTESIAN_POINT ( 'NONE',  ( 16.81223226430000039, 1414.913060387329779, 210.6693098017280192 ) ) ;
#66112 = CARTESIAN_POINT ( 'NONE',  ( 16.57542919120497515, 1524.538768545233779, 237.5505425563592041 ) ) ;
#66113 = AXIS2_PLACEMENT_3D ( 'NONE', #77944, #71234, #35390 ) ;
#66114 = CARTESIAN_POINT ( 'NONE',  ( -8.079136863727587325, 1477.137875895455636, 215.6487954345820128 ) ) ;
#66115 = CARTESIAN_POINT ( 'NONE',  ( 11.88903768390000160, 1433.614055813610094, 150.5325803792979968 ) ) ;
#66116 = CARTESIAN_POINT ( 'NONE',  ( 10.79382269979189957, 1414.913060387349788, 222.1041130917409987 ) ) ;
#66117 = B_SPLINE_SURFACE_WITH_KNOTS ( 'NONE', 5, 5, ( 
 ( #32241, #83740, #73148, #99980, #83197, #15417, #108396, #107291, #106731, #98884, #14320, #82649 ),
 ( #22151, #31129, #56352, #90484, #13759, #99424, #74266, #22702, #56900, #91033, #23272, #48510 ),
 ( #5940, #57469, #94333, #8675, #85380, #16507, #50166, #17050, #41740, #50696, #18182, #58558 ),
 ( #84827, #15963, #33325, #84294, #17611, #103279, #67520, #26586, #51813, #102724, #75366, #60215 ),
 ( #43412, #8128, #102189, #110600, #60783, #66965, #51247, #24373, #101075, #101621, #85953, #321 ),
 ( #24909, #9254, #867, #52377, #92687, #34446, #77562, #94908, #77015, #75899, #7037, #59117 ),
 ( #42855, #34992, #41195, #42294, #110051, #109505, #7585, #32781, #68622, #93241, #76446, #33883 ),
 ( #68077, #25469, #59663, #69173, #93771, #26018, #54045, #96005, #18723, #96568, #10340, #19274 ),
 ( #27156, #105521, #53479, #52920, #97116, #63009, #87622, #104962, #88172, #20385, #44513, #80317 ),
 ( #10909, #2534, #28251, #19840, #3632, #62443, #61341, #79225, #3084, #11463, #36655, #45638 ),
 ( #70852, #45083, #78660, #71406, #79777, #1977, #43958, #37211, #28810, #95461, #54587, #104409 ),
 ( #88723, #12005, #46186, #37762, #71955, #86497, #106066, #27702, #87053, #29346, #63545, #97661 ) ),
 .UNSPECIFIED., .F., .F., .F.,
 ( 6, 3, 3, 6 ),
 ( 6, 3, 3, 6 ),
 ( 12.92362791200000061, 14.22782209820000077, 16.13066607289999865, 17.24295068607450077 ),
 ( 0.000000000000000000, 0.3306909445339999976, 0.9920728336020000482, 1.580619590369999994 ),
 .UNSPECIFIED. ) ;
#66118 = CARTESIAN_POINT ( 'NONE',  ( 1.168363032481170016, 1450.780489601989984, 181.5091470336249984 ) ) ;
#66119 = CARTESIAN_POINT ( 'NONE',  ( -29.00779973304138437, 1526.382868172864164, 200.9494832830839073 ) ) ;
#66120 = AXIS2_PLACEMENT_3D ( 'NONE', #103896, #77055, #77600 ) ;
#66121 = CARTESIAN_POINT ( 'NONE',  ( -108.0197652269449407, 1389.258088431015722, 298.4547169909268405 ) ) ;
#66122 = CARTESIAN_POINT ( 'NONE',  ( 0.000000000000000000, 1397.913060387289988, 209.1218459616989946 ) ) ;
#66123 = CARTESIAN_POINT ( 'NONE',  ( -5.360152366205530150, 1422.242722016050038, 144.1549655170190078 ) ) ;
#66124 = CARTESIAN_POINT ( 'NONE',  ( 3.955903661833950036, 1474.305422501160137, 219.8349303349459944 ) ) ;
#66125 = CARTESIAN_POINT ( 'NONE',  ( -16.48212676430000201, 1409.488628936830082, 224.5375981998979853 ) ) ;
#66126 = EDGE_CURVE ( 'NONE', #23318, #36047, #39709, .T. ) ;
#66127 = VECTOR ( 'NONE', #158, 1000.000000000000000 ) ;
#66128 = CARTESIAN_POINT ( 'NONE',  ( -0.7143255590409999245, 1420.516258837929854, 228.0808124483980066 ) ) ;
#66129 = CARTESIAN_POINT ( 'NONE',  ( -32.38845791999490586, 1512.187213306747481, 216.1254071228449902 ) ) ;
#66130 = CARTESIAN_POINT ( 'NONE',  ( -1.393816646507350487, 1512.187213306747481, 243.1385343369520342 ) ) ;
#66131 = CARTESIAN_POINT ( 'NONE',  ( -3.172147559474420109E-06, 1406.917453532339778, 196.1218398979460176 ) ) ;
#66132 = CARTESIAN_POINT ( 'NONE',  ( 12.70077814543349959, 1426.512147001669973, 202.9361290949429986 ) ) ;
#66133 = CARTESIAN_POINT ( 'NONE',  ( -19.86622903098490056, 1443.388331107859813, 213.1207024752020232 ) ) ;
#66134 = ADVANCED_FACE ( 'NONE', ( #95030 ), #87182, .F. ) ;
#66135 = CARTESIAN_POINT ( 'NONE',  ( -11.22085809270000034, 1414.913060387329779, 220.6193216414980043 ) ) ;
#66136 = CARTESIAN_POINT ( 'NONE',  ( 0.1840937434512019966, 1472.115685549119917, 182.4330042628529895 ) ) ;
#66138 = ORIENTED_EDGE ( 'NONE', *, *, #62424, .F. ) ;
#66137 = CARTESIAN_POINT ( 'NONE',  ( 8.769621322867079627, 1467.226126602908835, 204.3312691679350905 ) ) ;
#66139 = CARTESIAN_POINT ( 'NONE',  ( -16.90742463042001376, 1444.994950788469623, 162.4348201727408991 ) ) ;
#66140 = CARTESIAN_POINT ( 'NONE',  ( -27.95614485608019706, 1508.896726002669993, 210.6431370344629954 ) ) ;
#66141 = CARTESIAN_POINT ( 'NONE',  ( 11.87916569230000086, 1433.311660768669981, 149.4775962793980000 ) ) ;
#66142 = CARTESIAN_POINT ( 'NONE',  ( -41.66188030070000536, 1443.681299836830021, 134.0999999982049928 ) ) ;
#66143 = CARTESIAN_POINT ( 'NONE',  ( -2.594026038730000039, 1450.364277435190161, 190.1050478246989996 ) ) ;
#66144 = ORIENTED_EDGE ( 'NONE', *, *, #59143, .F. ) ;
#66145 = CARTESIAN_POINT ( 'NONE',  ( -17.19754479272735637, 1524.059663615499630, 180.8698486848230971 ) ) ;
#66146 = DIRECTION ( 'NONE',  ( 0.000000000000000000, -1.000000000000000000, 0.000000000000000000 ) ) ;
#66147 = CARTESIAN_POINT ( 'NONE',  ( -104.4180155810560535, 1380.492968669763968, 307.4335991971175872 ) ) ;
#66148 = DIRECTION ( 'NONE',  ( -0.6736849260863839728, 0.000000000000000000, 0.7390186874254150995 ) ) ;
#66149 = CARTESIAN_POINT ( 'NONE',  ( 1.877783507969999821, 1464.338560063190016, 202.3121933697890142 ) ) ;
#66150 = CARTESIAN_POINT ( 'NONE',  ( 31.97075719519320458, 1416.524385823295688, 269.3163262971341396 ) ) ;
#66151 = VECTOR ( 'NONE', #23288, 1000.000000000000114 ) ;
#66152 = CARTESIAN_POINT ( 'NONE',  ( 4.500000000000000000, 1439.615672362369878, 182.7715282920979973 ) ) ;
#66153 = B_SPLINE_CURVE_WITH_KNOTS ( 'NONE', 3,
 ( #83964, #57695, #58232, #40309, #23503, #15089, #40861, #15628, #7264, #41427 ),
 .UNSPECIFIED., .F., .F.,
 ( 4, 2, 2, 2, 4 ),
 ( 0.000000000000000000, 0.2500000000000000000, 0.5000000000000000000, 0.7500000000000000000, 1.000000000000000000 ),
 .UNSPECIFIED. ) ;
#66154 = CARTESIAN_POINT ( 'NONE',  ( -14.23129321600000097, 1380.257846505089901, 210.5264815996590073 ) ) ;
#66155 = CARTESIAN_POINT ( 'NONE',  ( 2.500000000000000000, 1428.667732478729931, 183.2651393807979900 ) ) ;
#66156 = CARTESIAN_POINT ( 'NONE',  ( -61.95008448870819961, 1385.071029117499847, 248.2449222687090185 ) ) ;
#66157 = CARTESIAN_POINT ( 'NONE',  ( 12.87618670774100060, 1416.835419214280137, 196.3099906520550064 ) ) ;
#66158 = CARTESIAN_POINT ( 'NONE',  ( -4.987078423031819696, 1508.551704408389924, 206.6198795153389938 ) ) ;
#66159 = EDGE_LOOP ( 'NONE', ( #97913, #73340, #18434, #54983, #99709 ) ) ;
#66160 = CARTESIAN_POINT ( 'NONE',  ( -28.70934402958750198, 1509.343126753840124, 208.7447959780810152 ) ) ;
#66161 = CARTESIAN_POINT ( 'NONE',  ( -15.93050487141630178, 1409.571762620169920, 225.8570170024219976 ) ) ;
#66163 = ORIENTED_EDGE ( 'NONE', *, *, #51073, .F. ) ;
#66162 = CARTESIAN_POINT ( 'NONE',  ( 2.980039776149999931, 1507.572950449990003, 217.5187685084390239 ) ) ;
#66164 = CARTESIAN_POINT ( 'NONE',  ( 4.322866002579999645, 1473.654522927490007, 218.8408954872590186 ) ) ;
#66165 = CARTESIAN_POINT ( 'NONE',  ( 10.21480549290979845, 1470.289156061989843, 209.7505692248130060 ) ) ;
#66166 = CARTESIAN_POINT ( 'NONE',  ( -18.96565013588459792, 1410.937324021512723, 223.0483911484982400 ) ) ;
#66167 = CARTESIAN_POINT ( 'NONE',  ( -109.2887680899999907, 1384.559956795920016, 311.2476293452589857 ) ) ;
#66168 = CARTESIAN_POINT ( 'NONE',  ( -0.1424279854816119795, 1419.609337117080031, 184.3401574130290044 ) ) ;
#66169 = CIRCLE ( 'NONE', #17741, 2.000000000000003553 ) ;
#66170 = CARTESIAN_POINT ( 'NONE',  ( 17.84692647500000007, 1410.032952999730014, 222.8512867949980318 ) ) ;
#66171 = CARTESIAN_POINT ( 'NONE',  ( -0.4151546846821903003, 1511.187213306747708, 243.9330574173806951 ) ) ;
#66172 = CARTESIAN_POINT ( 'NONE',  ( -17.64168070010000022, 1423.919165630929911, 226.5634843356980070 ) ) ;
#66173 = CARTESIAN_POINT ( 'NONE',  ( -3.965320971343086143, 1511.478961035300472, 200.9376376759473146 ) ) ;
#66174 = CARTESIAN_POINT ( 'NONE',  ( 2.500000000000000000, 1428.667732465049994, 183.2651393814149969 ) ) ;
#66175 = CARTESIAN_POINT ( 'NONE',  ( -118.9277976642162855, 1311.832804576488797, 294.9031044600987457 ) ) ;
#66176 = CARTESIAN_POINT ( 'NONE',  ( -3.005276066430516035, 1369.205039411270036, 210.6218459616991936 ) ) ;
#66177 = CARTESIAN_POINT ( 'NONE',  ( 9.984115569229999210, 1365.258395869460173, 210.6218459616991936 ) ) ;
#66178 = B_SPLINE_CURVE_WITH_KNOTS ( 'NONE', 3,
 ( #77268, #8935, #15653, #25169, #92381, #101318, #51502, #7832, #42546, #10, #566, #85086, #33573, #49858, #35249, #94590, #50959, #59373, #110297, #102437, #17869 ),
 .UNSPECIFIED., .F., .F.,
 ( 4, 2, 1, 1, 1, 2, 2, 2, 1, 1, 2, 2, 4 ),
 ( 0.000000000000000000, 0.1250000000002345901, 0.1875000000003518852, 0.2187500000004230782, 0.2343750000004451162, 0.2421875000004429790, 0.2500000000004408141, 0.3750000000004406475, 0.4375000000004405365, 0.4687500000004408696, 0.4843750000004405920, 0.5000000000004402034, 1.000000000000000000 ),
 .UNSPECIFIED. ) ;
#66179 = CARTESIAN_POINT ( 'NONE',  ( -3.267291643295000103, 1516.842852731759876, 205.6749038603869906 ) ) ;
#66180 = CARTESIAN_POINT ( 'NONE',  ( -6.954065720117950100, 1517.551704408389924, 183.5505540514350002 ) ) ;
#66181 = CARTESIAN_POINT ( 'NONE',  ( -2.031883580139580037, 1464.998375551469962, 198.3053770173009980 ) ) ;
#66182 = DIRECTION ( 'NONE',  ( -0.3363363969979660806, -0.9417419115949053898, 0.000000000000000000 ) ) ;
#66184 = ORIENTED_EDGE ( 'NONE', *, *, #20659, .F. ) ;
#66183 = CARTESIAN_POINT ( 'NONE',  ( -68.66299202070430852, 1379.747740319620107, 280.2603170350629966 ) ) ;
#66185 = ORIENTED_EDGE ( 'NONE', *, *, #63363, .F. ) ;
#66186 = CARTESIAN_POINT ( 'NONE',  ( -9.362891644902104460, 1380.380461215845344, 217.2234689991179550 ) ) ;
#66187 = ORIENTED_EDGE ( 'NONE', *, *, #25860, .T. ) ;
#66188 = DIRECTION ( 'NONE',  ( 0.4090087482554252696, 0.000000000000000000, -0.9125304618753996566 ) ) ;
#66189 = CARTESIAN_POINT ( 'NONE',  ( -22.66911695520000336, 1410.908238445129882, 203.8386702287579908 ) ) ;
#66191 = CARTESIAN_POINT ( 'NONE',  ( 15.86082858073990032, 1410.114303850130000, 191.7269226526290140 ) ) ;
#66190 = CARTESIAN_POINT ( 'NONE',  ( -11.63809698065658438, 1425.864003583440081, 144.2671358013096778 ) ) ;
#66192 = CARTESIAN_POINT ( 'NONE',  ( 2.882325979385000014, 1516.969638403840008, 210.8235757905769674 ) ) ;
#66193 = CARTESIAN_POINT ( 'NONE',  ( 41.49264608937420462, 1443.127563515339943, 136.5039589477979973 ) ) ;
#66194 = AXIS2_PLACEMENT_3D ( 'NONE', #42224, #92069, #16977 ) ;
#66195 = CARTESIAN_POINT ( 'NONE',  ( -10.81512807170000023, 1424.921141247430114, 144.1662922870979742 ) ) ;
#66196 = FACE_OUTER_BOUND ( 'NONE', #15190, .T. ) ;
#66197 = CARTESIAN_POINT ( 'NONE',  ( 12.68863146979170153, 1500.713416596689967, 209.8116292722930041 ) ) ;
#66198 = DIRECTION ( 'NONE',  ( 0.000000000000000000, 0.000000000000000000, 1.000000000000000000 ) ) ;
#66199 = CARTESIAN_POINT ( 'NONE',  ( 35.54866228602229938, 1451.502040174259946, 134.0999999984919668 ) ) ;
#66200 = B_SPLINE_CURVE_WITH_KNOTS ( 'NONE', 3,
 ( #86234, #85125, #60509, #70575 ),
 .UNSPECIFIED., .F., .F.,
 ( 4, 4 ),
 ( 0.000000000000000000, 1.000000000000000000 ),
 .UNSPECIFIED. ) ;
#66201 = LINE ( 'NONE', #109286, #84717 ) ;
#66202 = CARTESIAN_POINT ( 'NONE',  ( -12.04602610249999906, 1481.198043686990104, 227.9689298191989622 ) ) ;
#66203 = CIRCLE ( 'NONE', #60845, 1.000002393159192371 ) ;
#66204 = CARTESIAN_POINT ( 'NONE',  ( -3.994937574034520100, 1430.106198372560129, 201.8091617894969829 ) ) ;
#66205 = ORIENTED_EDGE ( 'NONE', *, *, #98178, .F. ) ;
#66206 = VERTEX_POINT ( 'NONE', #78786 ) ;
#66207 = DIRECTION ( 'NONE',  ( 0.000000000000000000, 1.000000000000000000, -1.836970198721029688E-16 ) ) ;
#66208 = CARTESIAN_POINT ( 'NONE',  ( -16.19492410612830113, 1409.478599598990058, 194.0661808939520085 ) ) ;
#66209 = CARTESIAN_POINT ( 'NONE',  ( 19.19535387687943029, 1456.080104641030175, 225.8939609127118047 ) ) ;
#66210 = CARTESIAN_POINT ( 'NONE',  ( -20.35522600081170097, 1508.452240834250006, 209.8847156256999824 ) ) ;
#66211 = DIRECTION ( 'NONE',  ( -0.9455185755993178454, 0.000000000000000000, 0.3255681544571537578 ) ) ;
#66212 = AXIS2_PLACEMENT_3D ( 'NONE', #43440, #11495, #28285 ) ;
#66213 = CARTESIAN_POINT ( 'NONE',  ( 4.324479010949999314, 1515.254596385190098, 209.8453191605230188 ) ) ;
#66214 = CARTESIAN_POINT ( 'NONE',  ( -3.487585001760570069, 1508.551704408610021, 204.2892291422272422 ) ) ;
#66215 = CARTESIAN_POINT ( 'NONE',  ( 33.91369120209999721, 1435.681798817170147, 134.0999984767980209 ) ) ;
#66216 = CARTESIAN_POINT ( 'NONE',  ( 9.803834995107230554, 1517.051704408389924, 221.6221720662910002 ) ) ;
#66217 = CARTESIAN_POINT ( 'NONE',  ( 26.46046307870000192, 1441.626270307079949, 137.7338459176980336 ) ) ;
#66218 = CARTESIAN_POINT ( 'NONE',  ( -10.91416569499999945, 1391.310101084879989, 214.8368661670989752 ) ) ;
#66219 = CARTESIAN_POINT ( 'NONE',  ( -73.07052337915050089, 1384.756188251220010, 271.9861327822499675 ) ) ;
#66220 = ORIENTED_EDGE ( 'NONE', *, *, #108387, .T. ) ;
#66221 = CARTESIAN_POINT ( 'NONE',  ( 1.124894050234999998, 1517.194816588360027, 202.1703287997270309 ) ) ;
#66222 = CARTESIAN_POINT ( 'NONE',  ( 2.477975315464999717, 1516.839862955080207, 207.9852983471170091 ) ) ;
#66223 = ORIENTED_EDGE ( 'NONE', *, *, #90507, .F. ) ;
#66224 = CARTESIAN_POINT ( 'NONE',  ( 41.87718344479209520, 1440.913060387330006, 269.4528669971400063 ) ) ;
#66225 = CARTESIAN_POINT ( 'NONE',  ( -0.0002536599424906319715, 1452.586836000080439, 153.4883541576832329 ) ) ;
#66226 = ORIENTED_EDGE ( 'NONE', *, *, #104640, .T. ) ;
#66227 = LINE ( 'NONE', #67869, #66045 ) ;
#66228 = ADVANCED_FACE ( 'NONE', ( #18299 ), #3209, .F. ) ;
#66229 = DIRECTION ( 'NONE',  ( 0.7071067811865492381, 0.000000000000000000, 0.7071067811865457964 ) ) ;
#66230 = CARTESIAN_POINT ( 'NONE',  ( 0.000000000000000000, 1511.187213306747708, 209.1218459616979999 ) ) ;
#66231 = CARTESIAN_POINT ( 'NONE',  ( -9.234024398008379819, 1461.205035371770009, 206.1824885990050120 ) ) ;
#66232 = DIRECTION ( 'NONE',  ( 0.8090169943749465631, -0.000000000000000000, -0.5877852522924742473 ) ) ;
#66233 = CARTESIAN_POINT ( 'NONE',  ( 10.28237718578049886, 1469.669003181509879, 207.2474476084789785 ) ) ;
#66234 = CARTESIAN_POINT ( 'NONE',  ( -8.233416563630001406, 1473.844808855489873, 202.6267445639990115 ) ) ;
#66235 = CARTESIAN_POINT ( 'NONE',  ( -5.593955164791184487, 1510.491946807396744, 201.5711409828585943 ) ) ;
#66236 = CARTESIAN_POINT ( 'NONE',  ( 26.40325702796710061, 1497.690506021000147, 206.2288011628740207 ) ) ;
#66238 = CARTESIAN_POINT ( 'NONE',  ( -10.85852385072151449, 1424.794007429657313, 138.1924915429941905 ) ) ;
#66237 = CARTESIAN_POINT ( 'NONE',  ( 17.37740683730000057, 1460.085864807530015, 228.4865696861979814 ) ) ;
#66239 = CARTESIAN_POINT ( 'NONE',  ( -4.632166985597920394, 1422.117103908413128, 184.6589626825009418 ) ) ;
#66240 = B_SPLINE_SURFACE_WITH_KNOTS ( 'NONE', 5, 5, ( 
 ( #72834, #73933, #39204, #108063, #47084, #31359, #91815, #6710, #66651 ),
 ( #100753, #106968, #94569, #93460, #24040, #109729, #51479, #17285, #42517 ),
 ( #77247, #60449, #59898, #16731, #41432, #7811, #75599, #26262, #58236 ),
 ( #52044, #110826, #43637, #17841, #25147, #547, #67193, #49839, #68858 ),
 ( #7268, #33547, #68309, #102417, #76129, #67745, #69413, #9473, #50394 ),
 ( #34671, #101854, #92360, #85609, #15632, #83968, #33007, #59352, #101293 ) ),
 .UNSPECIFIED., .F., .F., .F.,
 ( 6, 6 ),
 ( 6, 3, 6 ),
 ( 0.4666582265090000181, 2.797885342447860246 ),
 ( -1.082961785764040044E-05, 1.000000000000000000, 2.000000000000000000 ),
 .UNSPECIFIED. ) ;
#66241 = CARTESIAN_POINT ( 'NONE',  ( 4.035490712554999249, 1516.630499592039996, 216.8333966482170183 ) ) ;
#66242 = ORIENTED_EDGE ( 'NONE', *, *, #6974, .T. ) ;
#66243 = CARTESIAN_POINT ( 'NONE',  ( -1.210324586182019546, 1486.266221086842961, 181.7930448816870523 ) ) ;
#66244 = DIRECTION ( 'NONE',  ( 0.4770263929453174567, 0.7067418228236591604, 0.5224574779878943254 ) ) ;
#66245 = EDGE_CURVE ( 'NONE', #27633, #46347, #59749, .T. ) ;
#66246 = CARTESIAN_POINT ( 'NONE',  ( 0.4409583776298362512, 1516.806451497312082, 216.8380041110111733 ) ) ;
#66247 = CARTESIAN_POINT ( 'NONE',  ( -2.866857931135000204, 1516.951766529250108, 213.1652121904069759 ) ) ;
#66248 = CARTESIAN_POINT ( 'NONE',  ( 3.912777227685470205, 1515.493283046529996, 212.5869276274669915 ) ) ;
#66249 = FACE_OUTER_BOUND ( 'NONE', #37841, .T. ) ;
#66251 = ORIENTED_EDGE ( 'NONE', *, *, #16504, .F. ) ;
#66250 = CARTESIAN_POINT ( 'NONE',  ( 4.364191146503010543, 1509.032029208890208, 213.2377284900549910 ) ) ;
#66252 = CYLINDRICAL_SURFACE ( 'NONE', #79986, 2.000000000000022204 ) ;
#66253 = AXIS2_PLACEMENT_3D ( 'NONE', #68512, #16397, #42189 ) ;
#66254 = CARTESIAN_POINT ( 'NONE',  ( 2.727892099239999979, 1508.551704408389924, 219.8158444027990015 ) ) ;
#66255 = EDGE_CURVE ( 'NONE', #42031, #65361, #58061, .T. ) ;
#66256 = CARTESIAN_POINT ( 'NONE',  ( -11.86004383289999886, 1431.913113693130072, 149.9670089978980059 ) ) ;
#66257 = CARTESIAN_POINT ( 'NONE',  ( -15.69795926999090163, 1519.551704408389924, 195.4758181584410011 ) ) ;
#66258 = CARTESIAN_POINT ( 'NONE',  ( -109.9685895047820026, 1384.440684789770103, 311.4348663963149306 ) ) ;
#66259 = CARTESIAN_POINT ( 'NONE',  ( 27.02366939970098159, 1451.038188054575812, 136.3589578157976803 ) ) ;
#66260 = B_SPLINE_CURVE_WITH_KNOTS ( 'NONE', 3,
 ( #107141, #108242, #13061, #66279, #98739, #31532, #4687, #5801, #100395, #74663, #30433, #82500, #107699, #91991, #47246, #83581, #99273, #5235, #74112, #65708, #90889, #6880, #100922, #39390, #73566, #75213, #99830, #48918 ),
 .UNSPECIFIED., .F., .F.,
 ( 4, 2, 1, 1, 1, 2, 2, 2, 1, 1, 2, 2, 1, 1, 1, 2, 2, 4 ),
 ( 0.000000000000000000, 0.1249999999971333209, 0.1874999999956837582, 0.2187499999949452933, 0.2343749999945753670, 0.2421874999943897933, 0.2499999999942042195, 0.3749999999947117857, 0.4374999999949656382, 0.4687499999949767404, 0.4843749999949823470, 0.4999999999949878982, 0.6249999999956661334, 0.6874999999958667507, 0.7187499999961025621, 0.7343749999962204678, 0.7499999999963383734, 1.000000000000000000 ),
 .UNSPECIFIED. ) ;
#66261 = DIRECTION ( 'NONE',  ( 1.835183309750130004E-16, 1.000000000000000000, 1.599799320660000123E-19 ) ) ;
#66262 = CARTESIAN_POINT ( 'NONE',  ( 12.86833609579999838, 1444.979730008290062, 187.1048578417980082 ) ) ;
#66264 = CARTESIAN_POINT ( 'NONE',  ( -5.940831854492779840, 1420.421544355079959, 137.0999999980978430 ) ) ;
#66263 = CARTESIAN_POINT ( 'NONE',  ( -26.86204968839999907, 1508.007394745430020, 212.0120969969080136 ) ) ;
#66265 = CARTESIAN_POINT ( 'NONE',  ( -16.12806753298000473, 1459.080126285580036, 229.9878173539649993 ) ) ;
#66266 = EDGE_LOOP ( 'NONE', ( #88076, #60220, #81080, #99756 ) ) ;
#66267 = CARTESIAN_POINT ( 'NONE',  ( -0.7572979743539989261, 1516.829948096479939, 205.6721984920870057 ) ) ;
#66268 = CARTESIAN_POINT ( 'NONE',  ( 14.57541043219999999, 1407.789481095929887, 268.9619740390979814 ) ) ;
#66269 = CARTESIAN_POINT ( 'NONE',  ( 38.62063633891679615, 1443.662372577139877, 137.1803698152800166 ) ) ;
#66270 = CARTESIAN_POINT ( 'NONE',  ( 10.82854844483479972, 1489.698305903909841, 207.5992399318249966 ) ) ;
#66271 = CARTESIAN_POINT ( 'NONE',  ( 22.07708618635539466, 1430.125185735898640, 217.9172516584410744 ) ) ;
#66272 = CARTESIAN_POINT ( 'NONE',  ( -8.571699234208210783, 1388.295717325432861, 218.1000065865680710 ) ) ;
#66273 = CARTESIAN_POINT ( 'NONE',  ( 27.70972759929999896, 1508.058934375229910, 212.2396871123379753 ) ) ;
#66274 = ADVANCED_FACE ( 'NONE', ( #103975 ), #21422, .T. ) ;
#66275 = CARTESIAN_POINT ( 'NONE',  ( 13.99649777436419917, 1443.814619143300206, 195.5016475565269900 ) ) ;
#66276 = AXIS2_PLACEMENT_3D ( 'NONE', #100432, #23715, #102075 ) ;
#66277 = CARTESIAN_POINT ( 'NONE',  ( -0.8736373970091440011, 1450.882552293999879, 154.7893752771190066 ) ) ;
#66278 = CARTESIAN_POINT ( 'NONE',  ( -12.03594224589999939, 1445.662096867079981, 187.0019513043980055 ) ) ;
#66279 = CARTESIAN_POINT ( 'NONE',  ( -19.69953526152687928, 1486.120311317603864, 190.0890748500791290 ) ) ;
#66280 = CARTESIAN_POINT ( 'NONE',  ( -8.631581796184160993, 1437.055567594220065, 209.4405929349389908 ) ) ;
#66281 = FACE_OUTER_BOUND ( 'NONE', #85918, .T. ) ;
#66282 = CARTESIAN_POINT ( 'NONE',  ( -19.00000000000000000, 1440.913060387330006, 209.1218459616979999 ) ) ;
#66283 = CARTESIAN_POINT ( 'NONE',  ( 20.10171188468166292, 1507.852758503362338, 228.9948063811727934 ) ) ;
#66284 = CARTESIAN_POINT ( 'NONE',  ( 3.134096205239999655, 1440.879545174999976, 159.2386616682979934 ) ) ;
#66285 = CARTESIAN_POINT ( 'NONE',  ( -2.077244269789999986, 1475.014520942230092, 269.6487028165980178 ) ) ;
#66286 = CARTESIAN_POINT ( 'NONE',  ( -11.45157208071476695, 1425.808262388908815, 139.1344810667301601 ) ) ;
#66287 = CARTESIAN_POINT ( 'NONE',  ( -14.47444372044108540, 1514.320539547600902, 192.6747587196877021 ) ) ;
#66288 = DIRECTION ( 'NONE',  ( 0.9455185755993178454, 0.000000000000000000, -0.3255681544571537578 ) ) ;
#66289 = CARTESIAN_POINT ( 'NONE',  ( -50.80134176948489966, 1384.736217744079795, 263.3871381538430114 ) ) ;
#66290 = CARTESIAN_POINT ( 'NONE',  ( -106.4627743365379899, 1391.913060387289988, 303.3857292504940233 ) ) ;
#66291 = AXIS2_PLACEMENT_3D ( 'NONE', #93413, #16680, #8302 ) ;
#66292 = DIRECTION ( 'NONE',  ( -0.6736849260863837507, 0.000000000000000000, 0.7390186874254154326 ) ) ;
#66293 = CARTESIAN_POINT ( 'NONE',  ( -24.27560546558390087, 1444.785062312789933, 211.2846025609280218 ) ) ;
#66294 = CARTESIAN_POINT ( 'NONE',  ( 30.95751052620450494, 1525.821544997590081, 216.7905424461071675 ) ) ;
#66295 = CARTESIAN_POINT ( 'NONE',  ( 8.003677881822152784, 1511.683950138178034, 205.7359720134772090 ) ) ;
#66296 = CARTESIAN_POINT ( 'NONE',  ( -20.91134631659999599, 1409.807790057629745, 201.0288384400980135 ) ) ;
#66297 = B_SPLINE_CURVE_WITH_KNOTS ( 'NONE', 3,
 ( #45637, #70296, #79224, #27155, #10339, #12004, #2533, #78659, #46185, #80316 ),
 .UNSPECIFIED., .F., .F.,
 ( 4, 3, 3, 4 ),
 ( 2.231733318449370174, 2.693712400684689978, 2.992882853181570102, 3.155691482920000013 ),
 .UNSPECIFIED. ) ;
#66298 = CARTESIAN_POINT ( 'NONE',  ( -15.03850872322399823, 1422.463411162540069, 228.7611157286099797 ) ) ;
#66299 = DIRECTION ( 'NONE',  ( 0.9858563016923833633, 0.000000000000000000, 0.1675928173085483863 ) ) ;
#66300 = ORIENTED_EDGE ( 'NONE', *, *, #44902, .F. ) ;
#66301 = LINE ( 'NONE', #56775, #23065 ) ;
#66302 = CARTESIAN_POINT ( 'NONE',  ( -13.59488878742559947, 1507.788032636909975, 209.3690985338880068 ) ) ;
#66303 = CARTESIAN_POINT ( 'NONE',  ( -19.34950487613039627, 1446.106571107670106, 200.0047943255200096 ) ) ;
#66305 = CARTESIAN_POINT ( 'NONE',  ( -14.92730992206499785, 1514.452905717119847, 192.9094359382670234 ) ) ;
#66304 = CARTESIAN_POINT ( 'NONE',  ( 11.72729116660000059, 1426.702026288230172, 143.4717466479980033 ) ) ;
#66306 = CARTESIAN_POINT ( 'NONE',  ( 16.88555899345125866, 1525.556089352344316, 236.5668029769053931 ) ) ;
#66307 = CARTESIAN_POINT ( 'NONE',  ( -1.600048698852036821, 1401.254281879943164, 135.5999999980979851 ) ) ;
#66308 = CARTESIAN_POINT ( 'NONE',  ( 19.37374569213924502, 1524.382868172863937, 183.8768763279539655 ) ) ;
#66309 = CIRCLE ( 'NONE', #105618, 2.000000000000001776 ) ;
#66310 = CARTESIAN_POINT ( 'NONE',  ( 6.553524377605000062, 1516.882690742909972, 202.1776141839370098 ) ) ;
#66311 = CARTESIAN_POINT ( 'NONE',  ( 11.54436744337454002, 1432.352362330610049, 151.3410663384053976 ) ) ;
#66312 = DIRECTION ( 'NONE',  ( 1.988618688120850357E-13, 0.03085824620771311644, -0.9995237709234254808 ) ) ;
#66313 = CARTESIAN_POINT ( 'NONE',  ( 16.25489176703500149, 1512.123798513659949, 196.5876941637669688 ) ) ;
#66314 = CARTESIAN_POINT ( 'NONE',  ( -19.96805577914620144, 1418.682940182010043, 207.2801514309879849 ) ) ;
#66315 = CYLINDRICAL_SURFACE ( 'NONE', #66276, 2.000000000000001776 ) ;
#66316 = CARTESIAN_POINT ( 'NONE',  ( 21.68605459302450100, 1509.621532965099959, 228.4776040847019942 ) ) ;
#66318 = VERTEX_POINT ( 'NONE', #59920 ) ;
#66317 = CARTESIAN_POINT ( 'NONE',  ( -56.82419418675780776, 1379.716300530480112, 259.5363713978089777 ) ) ;
#66319 = ORIENTED_EDGE ( 'NONE', *, *, #70627, .T. ) ;
#66320 = CARTESIAN_POINT ( 'NONE',  ( 12.02669875993479920, 1433.747065677280034, 149.9298205679299940 ) ) ;
#66321 = CARTESIAN_POINT ( 'NONE',  ( -4.661545375210000230, 1396.075845138829891, 219.5353638017980131 ) ) ;
#66322 = CARTESIAN_POINT ( 'NONE',  ( -20.28107068739999974, 1410.981495019129852, 220.2339880788979940 ) ) ;
#66323 = VERTEX_POINT ( 'NONE', #86197 ) ;
#66324 = CARTESIAN_POINT ( 'NONE',  ( -13.36916045171295053, 1444.478176240853372, 169.3716993028445472 ) ) ;
#66325 = CARTESIAN_POINT ( 'NONE',  ( 22.51756156282889876, 1509.699390964210124, 227.9212218486820234 ) ) ;
#66326 = CARTESIAN_POINT ( 'NONE',  ( -0.1613635714646410035, 1507.107001889669846, 180.9028745560509890 ) ) ;
#66328 = CARTESIAN_POINT ( 'NONE',  ( -13.70772824027479864, 1507.648153509909889, 184.2587339175119894 ) ) ;
#66327 = CARTESIAN_POINT ( 'NONE',  ( 0.2941023281940010059, 1444.784487645989884, 199.4356807887090213 ) ) ;
#66329 = CIRCLE ( 'NONE', #75189, 1.999994602351848672 ) ;
#66330 = CARTESIAN_POINT ( 'NONE',  ( 7.083309374099999722, 1468.699157173630056, 184.4250794663979889 ) ) ;
#66331 = CARTESIAN_POINT ( 'NONE',  ( -4.885459850415359462, 1463.524421287130053, 200.4816849840370026 ) ) ;
#66332 = DIRECTION ( 'NONE',  ( 0.000000000000000000, -6.123233995736769734E-17, -1.000000000000000000 ) ) ;
#66333 = SURFACE_SIDE_STYLE ('',( #30486 ) ) ;
#66334 = CARTESIAN_POINT ( 'NONE',  ( 9.833610268327619863, 1396.256457636480036, 204.0482078523459677 ) ) ;
#66335 = CARTESIAN_POINT ( 'NONE',  ( 0.7890062529840000671, 1416.021639796329964, 190.5012297770979899 ) ) ;
#66336 = CARTESIAN_POINT ( 'NONE',  ( 10.91629673539999956, 1428.582341354329856, 150.7594233110980042 ) ) ;
#66337 = CARTESIAN_POINT ( 'NONE',  ( 7.960834073489841067, 1509.191483305627116, 180.8814468251773064 ) ) ;
#66338 = ORIENTED_EDGE ( 'NONE', *, *, #100084, .F. ) ;
#66339 = CARTESIAN_POINT ( 'NONE',  ( 13.29115197908729940, 1435.192795144800129, 149.9986224416759910 ) ) ;
#66340 = EDGE_LOOP ( 'NONE', ( #35549, #90487, #12179, #84633 ) ) ;
#66341 = ORIENTED_EDGE ( 'NONE', *, *, #89147, .T. ) ;
#66342 = CARTESIAN_POINT ( 'NONE',  ( 12.92773491524689078, 1444.920201159182170, 169.4324473822623816 ) ) ;
#66343 = CARTESIAN_POINT ( 'NONE',  ( -9.049861655339999089, 1463.472726760930072, 233.4465893264980139 ) ) ;
#66344 = CARTESIAN_POINT ( 'NONE',  ( -12.86077854309999857, 1416.823634022829992, 196.3807302971979993 ) ) ;
#66345 = CARTESIAN_POINT ( 'NONE',  ( -5.777745433405000242, 1516.908489800550115, 215.6797558528670038 ) ) ;
#66346 = CARTESIAN_POINT ( 'NONE',  ( -8.374266313531483874, 1511.401872466645500, 213.6732156279371679 ) ) ;
#66347 = EDGE_LOOP ( 'NONE', ( #71317, #44248, #21369, #91941 ) ) ;
#66348 = CARTESIAN_POINT ( 'NONE',  ( -11.34379066580000028, 1503.466875535689951, 207.0254393924689964 ) ) ;
#66349 = CARTESIAN_POINT ( 'NONE',  ( 2.500000000000000000, 1448.203020940240094, 169.6834909796610020 ) ) ;
#66350 = CARTESIAN_POINT ( 'NONE',  ( -57.70298350590000069, 1377.436376805819918, 252.0908766120590201 ) ) ;
#66351 = EDGE_LOOP ( 'NONE', ( #28889, #75420, #28222, #42420 ) ) ;
#66352 = CARTESIAN_POINT ( 'NONE',  ( -3.461047329755000401, 1516.858765657450249, 205.6745815831370123 ) ) ;
#66353 = ORIENTED_EDGE ( 'NONE', *, *, #9946, .F. ) ;
#66354 = CARTESIAN_POINT ( 'NONE',  ( -3.261652325025000021, 1516.939580991450157, 209.1351299096569960 ) ) ;
#66355 = CARTESIAN_POINT ( 'NONE',  ( -20.25110114130000127, 1509.046039793229966, 229.4394552683979782 ) ) ;
#66356 = CARTESIAN_POINT ( 'NONE',  ( -20.74384221371932924, 1414.376127513459551, 269.3942681799695151 ) ) ;
#66357 = CARTESIAN_POINT ( 'NONE',  ( 6.998420849865000015, 1512.696049264760177, 217.3137064069569817 ) ) ;
#66359 = VERTEX_POINT ( 'NONE', #69431 ) ;
#66358 = CARTESIAN_POINT ( 'NONE',  ( -0.05152562430163110108, 1416.529254608160045, 227.2755757173690085 ) ) ;
#66360 = CARTESIAN_POINT ( 'NONE',  ( 2.500000000000000000, 1425.201036443130079, 155.3321294796979828 ) ) ;
#66361 = CARTESIAN_POINT ( 'NONE',  ( -27.45330484456810183, 1440.913060400619997, 228.8604962196139923 ) ) ;
#66362 = CARTESIAN_POINT ( 'NONE',  ( -43.23635582379999676, 1383.823167092340100, 247.4293989253590098 ) ) ;
#66363 = CARTESIAN_POINT ( 'NONE',  ( -14.42498423343375791, 1415.918606729107523, 214.3962734341573366 ) ) ;
#66364 = CARTESIAN_POINT ( 'NONE',  ( 14.88997449063399969, 1411.680983156579941, 270.0818248018620693 ) ) ;
#66366 = CARTESIAN_POINT ( 'NONE',  ( 0.7568986996720019622, 1516.805675336850072, 213.1530147380969993 ) ) ;
#66365 = CIRCLE ( 'NONE', #62784, 2.000000000000003553 ) ;
#66367 = CARTESIAN_POINT ( 'NONE',  ( 24.12740820519999829, 1411.115144176130116, 208.8584871057929888 ) ) ;
#66368 = CARTESIAN_POINT ( 'NONE',  ( -20.13638283970000131, 1507.886205248129954, 189.0953426691980042 ) ) ;
#66369 = CARTESIAN_POINT ( 'NONE',  ( 3.039942922830000338, 1441.350710123290128, 218.5632362648489959 ) ) ;
#66370 = CARTESIAN_POINT ( 'NONE',  ( 7.203708765649230017, 1508.728101229370168, 215.8474698634739752 ) ) ;
#66371 = CARTESIAN_POINT ( 'NONE',  ( 3.462835627365000057, 1517.038650117239968, 210.2415636864969883 ) ) ;
#66372 = CARTESIAN_POINT ( 'NONE',  ( -20.27427188162092975, 1517.151704408390060, 208.7383139970561672 ) ) ;
#66373 = CARTESIAN_POINT ( 'NONE',  ( 0.1114963473639999925, 1420.227192211030115, 183.9075558398980093 ) ) ;
#66374 = AXIS2_PLACEMENT_3D ( 'NONE', #78603, #45028, #12498 ) ;
#66375 = CARTESIAN_POINT ( 'NONE',  ( -8.473904872574415492, 1486.003588610487441, 183.3063149312824294 ) ) ;
#66377 = ORIENTED_EDGE ( 'NONE', *, *, #20676, .F. ) ;
#66376 = CARTESIAN_POINT ( 'NONE',  ( -50.36169832019999859, 1389.574744497710071, 254.8962280555589928 ) ) ;
#66378 = CARTESIAN_POINT ( 'NONE',  ( -45.19369995658139771, 1385.151324122020014, 251.9073361886829900 ) ) ;
#66379 = CARTESIAN_POINT ( 'NONE',  ( 30.61115703708031432, 1523.542365884047740, 196.4197133992099396 ) ) ;
#66380 = CARTESIAN_POINT ( 'NONE',  ( -4.118752830811812871, 1370.397247303622407, 209.7672875607871958 ) ) ;
#66381 = CIRCLE ( 'NONE', #68141, 8.013264357029999729 ) ;
#66382 = CARTESIAN_POINT ( 'NONE',  ( 0.3578367916707796414, 1494.301120918491051, 220.2517076097725806 ) ) ;
#66383 = CARTESIAN_POINT ( 'NONE',  ( 7.885640402109895142, 1473.211498812089985, 217.4524272520788486 ) ) ;
#66384 = CARTESIAN_POINT ( 'NONE',  ( -23.40333288369999920, 1448.250072204309845, 217.2337772597779804 ) ) ;
#66385 = CARTESIAN_POINT ( 'NONE',  ( 1.744489195120649150, 1498.886263367861602, 197.9188166206191113 ) ) ;
#66387 = FACE_OUTER_BOUND ( 'NONE', #32711, .T. ) ;
#66386 = CARTESIAN_POINT ( 'NONE',  ( 5.779603100124999671, 1516.738222552470233, 216.8362174732170047 ) ) ;
#66388 = CARTESIAN_POINT ( 'NONE',  ( -25.32446257976238968, 1450.806899494430354, 137.4427265456963880 ) ) ;
#66389 = CARTESIAN_POINT ( 'NONE',  ( 30.31404213106236512, 1524.330813522192102, 221.7920027509178169 ) ) ;
#66390 = EDGE_LOOP ( 'NONE', ( #37293, #97832, #96706, #26977 ) ) ;
#66391 = CARTESIAN_POINT ( 'NONE',  ( -7.718763544034999313, 1516.905946377369901, 202.1794916586869988 ) ) ;
#66392 = CARTESIAN_POINT ( 'NONE',  ( -16.74824993986500132, 1512.868709057589967, 222.4423585103670007 ) ) ;
#66393 = CARTESIAN_POINT ( 'NONE',  ( -27.02655704100176592, 1451.108971386630174, 136.3738572239980158 ) ) ;
#66394 = CARTESIAN_POINT ( 'NONE',  ( 20.06570944619999963, 1454.764211563430081, 224.8152366716980168 ) ) ;
#66395 = CARTESIAN_POINT ( 'NONE',  ( 10.78248285070100110, 1461.894572756529897, 211.1626650880500051 ) ) ;
#66396 = CARTESIAN_POINT ( 'NONE',  ( -7.727640881871497669, 1461.842851176162412, 203.2269185635026076 ) ) ;
#66397 = CARTESIAN_POINT ( 'NONE',  ( -1.466944312100000092, 1443.753574183790079, 218.3055266773990013 ) ) ;
#66398 = DIRECTION ( 'NONE',  ( 0.000000000000000000, 0.000000000000000000, -1.000000000000000000 ) ) ;
#66399 = AXIS2_PLACEMENT_3D ( 'NONE', #69720, #63530, #3616 ) ;
#66400 = CARTESIAN_POINT ( 'NONE',  ( -105.4624709189999834, 1391.255327103129957, 304.2078109453590287 ) ) ;
#66401 = CARTESIAN_POINT ( 'NONE',  ( -23.63309344749999852, 1435.875959318670084, 212.1442856114379936 ) ) ;
#66402 = CARTESIAN_POINT ( 'NONE',  ( 9.275324149480784541, 1488.103561708918050, 203.3811522517966068 ) ) ;
#66403 = CARTESIAN_POINT ( 'NONE',  ( -105.5788448139999929, 1390.041791431060119, 301.0601375796589991 ) ) ;
#66404 = CARTESIAN_POINT ( 'NONE',  ( -16.56636285579999779, 1413.296451893629865, 226.6997547370980044 ) ) ;
#66405 = CARTESIAN_POINT ( 'NONE',  ( 20.07149347155336372, 1526.186458717542791, 185.1794229323649290 ) ) ;
#66406 = AXIS2_PLACEMENT_3D ( 'NONE', #96265, #104107, #2236 ) ;
#66407 = CARTESIAN_POINT ( 'NONE',  ( -30.00386682649119763, 1462.246334517119067, 269.4708284355384080 ) ) ;
#66408 = ORIENTED_EDGE ( 'NONE', *, *, #76451, .T. ) ;
#66409 = CARTESIAN_POINT ( 'NONE',  ( 2.439001525050000119, 1430.488531030629929, 150.2249694046979869 ) ) ;
#66410 = CARTESIAN_POINT ( 'NONE',  ( -42.06510204283767962, 1427.649616927324587, 269.0740259319668439 ) ) ;
#66411 = ADVANCED_FACE ( 'NONE', ( #52616 ), #64386, .T. ) ;
#66412 = CARTESIAN_POINT ( 'NONE',  ( -4.534010781284650626, 1508.610336716400070, 213.3588268743650076 ) ) ;
#66413 = CARTESIAN_POINT ( 'NONE',  ( -0.9756374909739999879, 1431.113060387329824, 228.8047907271979966 ) ) ;
#66414 = CARTESIAN_POINT ( 'NONE',  ( -0.1798688738929999642, 1417.261861208530263, 235.9169760632979944 ) ) ;
#66415 = CARTESIAN_POINT ( 'NONE',  ( -13.46697063184865151, 1444.247415097991052, 187.0159000695805673 ) ) ;
#66416 = CARTESIAN_POINT ( 'NONE',  ( -16.66700976312950644, 1523.530935881284904, 180.4846138748687281 ) ) ;
#66417 = CARTESIAN_POINT ( 'NONE',  ( 2.236820334746699945, 1495.676459233159903, 221.2569916761739819 ) ) ;
#66418 = CIRCLE ( 'NONE', #18104, 17.74083438352840503 ) ;
#66419 = CARTESIAN_POINT ( 'NONE',  ( -1.906531099660209973E-08, 1509.038615934239942, 204.6345961781970004 ) ) ;
#66420 = CARTESIAN_POINT ( 'NONE',  ( -15.07584010957818954, 1451.149360461914966, 149.6732302036660656 ) ) ;
#66421 = CARTESIAN_POINT ( 'NONE',  ( -9.659635694953360385, 1460.543239006349950, 208.9236336851400040 ) ) ;
#66422 =( BOUNDED_CURVE ( )  B_SPLINE_CURVE ( 3, ( #40932, #25766, #32541, #77307 ),
 .UNSPECIFIED., .F., .F. ) 
 B_SPLINE_CURVE_WITH_KNOTS ( ( 4, 4 ),
 ( 1.555588359660764919, 1.573006934440774884 ),
 .UNSPECIFIED. ) 
 CURVE ( )  GEOMETRIC_REPRESENTATION_ITEM ( )  RATIONAL_B_SPLINE_CURVE ( ( 1.000000000000000000, 0.9999747162642045328, 0.9999747162642045328, 1.000000000000000000 ) ) 
 REPRESENTATION_ITEM ( '' )  );
#66423 = CARTESIAN_POINT ( 'NONE',  ( -12.60679465157404167, 1442.786628925963214, 169.4683254417570026 ) ) ;
#66425 = VERTEX_POINT ( 'NONE', #38545 ) ;
#66424 = CARTESIAN_POINT ( 'NONE',  ( -14.33610927549999836, 1409.413688348330197, 225.7799880264979890 ) ) ;
#66426 = CARTESIAN_POINT ( 'NONE',  ( -0.09392264339291689357, 1415.426561690370136, 191.6203292375940066 ) ) ;
#66427 = CARTESIAN_POINT ( 'NONE',  ( 22.01759343194246910, 1509.573295641457435, 226.9000235256352767 ) ) ;
#66428 = ORIENTED_EDGE ( 'NONE', *, *, #68530, .F. ) ;
#66429 = EDGE_LOOP ( 'NONE', ( #16301, #67012 ) ) ;
#66430 = CARTESIAN_POINT ( 'NONE',  ( 16.98743823132990016, 1415.088136167450102, 209.1445283149309944 ) ) ;
#66431 = CARTESIAN_POINT ( 'NONE',  ( 6.218727018272192986, 1516.719877041854261, 204.9285666176960206 ) ) ;
#66433 = CARTESIAN_POINT ( 'NONE',  ( -24.18530732099999980, 1444.140951279559886, 212.0278258309579940 ) ) ;
#66432 = CARTESIAN_POINT ( 'NONE',  ( 4.573885314059999985, 1455.617763203289996, 218.2506144138390027 ) ) ;
#66434 = CARTESIAN_POINT ( 'NONE',  ( -3.499767445780000319, 1444.082658218989764, 218.1757574250489995 ) ) ;
#66435 = CARTESIAN_POINT ( 'NONE',  ( -11.75646471859999842, 1433.433141379730159, 150.8109742706980114 ) ) ;
#66436 = CARTESIAN_POINT ( 'NONE',  ( -4.487357219411578946, 1509.034509700538365, 212.2379894419900381 ) ) ;
#66437 = CARTESIAN_POINT ( 'NONE',  ( 251.6799247787360230, 1855.634424228300077, 173.9675981348009941 ) ) ;
#66438 = CARTESIAN_POINT ( 'NONE',  ( 7.190134108680000580, 1424.106784181189823, 213.0072132442990096 ) ) ;
#66439 = CARTESIAN_POINT ( 'NONE',  ( -14.32882045604760357, 1429.651770908837989, 222.2483748908982761 ) ) ;
#66440 = FACE_BOUND ( 'NONE', #30375, .T. ) ;
#66441 = LINE ( 'NONE', #24929, #57322 ) ;
#66442 =( GEOMETRIC_REPRESENTATION_CONTEXT ( 3 ) GLOBAL_UNCERTAINTY_ASSIGNED_CONTEXT ( ( #24471 ) ) GLOBAL_UNIT_ASSIGNED_CONTEXT ( ( #64675, #14786, #89842 ) ) REPRESENTATION_CONTEXT ( 'NONE', 'WORKASPACE' ) );
#66443 = CARTESIAN_POINT ( 'NONE',  ( 8.476942927299997876, 1362.523913559720086, 207.6218459616989946 ) ) ;
#66444 = CARTESIAN_POINT ( 'NONE',  ( -28.97640022888837663, 1510.035890305760176, 216.8925410192303218 ) ) ;
#66446 = VERTEX_POINT ( 'NONE', #106846 ) ;
#66445 = CARTESIAN_POINT ( 'NONE',  ( -4.858360422201509543, 1508.551704408389469, 205.6342535009236485 ) ) ;
#66447 = ORIENTED_EDGE ( 'NONE', *, *, #87716, .T. ) ;
#66448 = CARTESIAN_POINT ( 'NONE',  ( -11.75158851103499913, 1426.771919862610048, 145.1867488865719906 ) ) ;
#66449 = EDGE_CURVE ( 'NONE', #101372, #36895, #38370, .T. ) ;
#66450 = EDGE_CURVE ( 'NONE', #89981, #66046, #104657, .T. ) ;
#66451 = CARTESIAN_POINT ( 'NONE',  ( -21.43713612259999834, 1507.398797767890073, 216.2026692569289992 ) ) ;
#66452 = CARTESIAN_POINT ( 'NONE',  ( -8.240145092400000593, 1473.030649236130103, 270.3822351584980197 ) ) ;
#66453 = CARTESIAN_POINT ( 'NONE',  ( -2.338275166668102756, 1474.327831861476170, 219.1154912885318709 ) ) ;
#66455 = VECTOR ( 'NONE', #104892, 1000.000000000000000 ) ;
#66454 = CARTESIAN_POINT ( 'NONE',  ( -105.5311032031419956, 1320.102705746889569, 317.4872039844588016 ) ) ;
#66456 = EDGE_CURVE ( 'NONE', #6446, #77864, #99785, .T. ) ;
#66457 = CARTESIAN_POINT ( 'NONE',  ( 37.85868654299600422, 1450.015328435070160, 136.0234584287910025 ) ) ;
#66459 = EDGE_CURVE ( 'NONE', #20723, #110373, #56937, .T. ) ;
#66458 = CARTESIAN_POINT ( 'NONE',  ( 18.70730727500000157, 1431.113060387329824, 209.1218459615069776 ) ) ;
#66460 = CARTESIAN_POINT ( 'NONE',  ( -8.847783283049999170, 1384.881200138800068, 199.9249094011889838 ) ) ;
#66461 = EDGE_CURVE ( 'NONE', #43603, #15017, #94416, .T. ) ;
#66462 = CARTESIAN_POINT ( 'NONE',  ( -5.257080573758877939, 1522.051704408389924, 199.2452589303538275 ) ) ;
#66463 = CARTESIAN_POINT ( 'NONE',  ( -4.468118146560000170, 1458.475370017489922, 218.8772509106790096 ) ) ;
#66464 = CARTESIAN_POINT ( 'NONE',  ( 9.704582620010000937, 1366.001145740639913, 207.6218459616989946 ) ) ;
#66465 = CARTESIAN_POINT ( 'NONE',  ( -43.77342332416050397, 1429.948824217480023, 266.7521212402160131 ) ) ;
#66466 = ORIENTED_EDGE ( 'NONE', *, *, #41772, .T. ) ;
#66467 = CARTESIAN_POINT ( 'NONE',  ( -4.327620191588679610, 1515.134623705510194, 209.7786229697130125 ) ) ;
#66468 = ORIENTED_EDGE ( 'NONE', *, *, #100925, .F. ) ;
#66469 = ORIENTED_EDGE ( 'NONE', *, *, #77703, .F. ) ;
#66470 = CARTESIAN_POINT ( 'NONE',  ( 1.136547584984999970, 1516.839862955080207, 211.5998212856970042 ) ) ;
#66471 = AXIS2_PLACEMENT_3D ( 'NONE', #95184, #1142, #41480 ) ;
#66472 = CARTESIAN_POINT ( 'NONE',  ( 4.619879510139068834, 1423.718273955572158, 183.8526073848954638 ) ) ;
#66473 = CARTESIAN_POINT ( 'NONE',  ( 22.03465957474552539, 1522.382868172863937, 182.8300405912328301 ) ) ;
#66475 = DIRECTION ( 'NONE',  ( -0.6736849260863839728, 0.000000000000000000, 0.7390186874254150995 ) ) ;
#66474 = CARTESIAN_POINT ( 'NONE',  ( -6.547881413045000265, 1516.647534046129977, 212.5778533554070293 ) ) ;
#66476 = CARTESIAN_POINT ( 'NONE',  ( -16.58606811730000175, 1455.453783750930143, 189.4873228618979795 ) ) ;
#66477 = DIRECTION ( 'NONE',  ( -0.6736849260863841948, 0.000000000000000000, 0.7390186874254148774 ) ) ;
#66478 = ORIENTED_EDGE ( 'NONE', *, *, #98695, .F. ) ;
#66479 = CARTESIAN_POINT ( 'NONE',  ( -26.29948081250000058, 1435.416034970859982, 135.3926350979980100 ) ) ;
#66480 = EDGE_CURVE ( 'NONE', #68857, #61100, #52618, .T. ) ;
#66481 = CARTESIAN_POINT ( 'NONE',  ( -5.006329619514999330, 1516.755758396839838, 202.5714564999769891 ) ) ;
#66482 = AXIS2_PLACEMENT_3D ( 'NONE', #15543, #49743, #75501 ) ;
#66483 = CARTESIAN_POINT ( 'NONE',  ( 9.877435263969999824, 1471.593449360889963, 212.9802648889690033 ) ) ;
#66484 = EDGE_CURVE ( 'NONE', #81651, #13362, #31256, .T. ) ;
#66485 = CARTESIAN_POINT ( 'NONE',  ( -35.17588676205760123, 1384.569143118210150, 208.8585631465319921 ) ) ;
#66486 = CARTESIAN_POINT ( 'NONE',  ( -33.74129728029610220, 1421.399541067400150, 269.9732882242340111 ) ) ;
#66487 = DIRECTION ( 'NONE',  ( -0.7067700464262639537, 0.03085823069700149510, -0.7067700270051548994 ) ) ;
#66488 = CARTESIAN_POINT ( 'NONE',  ( -1.143643780430000145, 1395.952997308129852, 197.8013073227980101 ) ) ;
#66490 = ORIENTED_EDGE ( 'NONE', *, *, #46868, .F. ) ;
#66489 = DIRECTION ( 'NONE',  ( -0.6736849260863841948, 0.000000000000000000, 0.7390186874254148774 ) ) ;
#66491 = VERTEX_POINT ( 'NONE', #39087 ) ;
#66493 = EDGE_CURVE ( 'NONE', #9890, #9209, #68390, .T. ) ;
#66492 = DIRECTION ( 'NONE',  ( 0.000000000000000000, 0.000000000000000000, 1.000000000000000000 ) ) ;
#66494 = CARTESIAN_POINT ( 'NONE',  ( -28.49879435372385572, 1526.382868173645647, 219.8425395114961702 ) ) ;
#66495 = CARTESIAN_POINT ( 'NONE',  ( -10.36756237719999874, 1382.682511944280122, 200.8304498154890041 ) ) ;
#66496 = CARTESIAN_POINT ( 'NONE',  ( -25.11421028039999825, 1436.601945934859941, 137.7221587483980159 ) ) ;
#66497 = CARTESIAN_POINT ( 'NONE',  ( -24.49558118859999922, 1441.433152052330115, 211.0117683613680128 ) ) ;
#66498 = CARTESIAN_POINT ( 'NONE',  ( 2.493699768634999536, 1516.858326417339867, 211.5985794462469869 ) ) ;
#66499 = AXIS2_PLACEMENT_3D ( 'NONE', #37850, #107802, #82036 ) ;
#66500 = CARTESIAN_POINT ( 'NONE',  ( -68.77575455639998836, 1379.747977220560188, 280.2449803406589695 ) ) ;
#66501 = CARTESIAN_POINT ( 'NONE',  ( -2.293592999468180071, 1484.254952969489977, 183.1434726039850034 ) ) ;
#66502 = CARTESIAN_POINT ( 'NONE',  ( 4.010670133484330435, 1440.993182668509917, 217.7599716824630036 ) ) ;
#66503 = CARTESIAN_POINT ( 'NONE',  ( -13.15471227499809892, 1414.913526845469960, 220.1561254705790134 ) ) ;
#66504 = CARTESIAN_POINT ( 'NONE',  ( -6.952166420425000659, 1517.213554313520035, 207.4130983078469797 ) ) ;
#66505 = VERTEX_POINT ( 'NONE', #58676 ) ;
#66506 = CARTESIAN_POINT ( 'NONE',  ( -2.907264515414449857, 1451.960119877520128, 184.7556101994359778 ) ) ;
#66507 = CARTESIAN_POINT ( 'NONE',  ( -8.663672900706190561, 1438.058509006810027, 208.5115941168539848 ) ) ;
#66508 = CARTESIAN_POINT ( 'NONE',  ( -3.078458293620000230, 1385.190530866809922, 218.5645787212890241 ) ) ;
#66509 = ORIENTED_EDGE ( 'NONE', *, *, #80952, .F. ) ;
#66511 = B_SPLINE_CURVE_WITH_KNOTS ( 'NONE', 3,
 ( #94189, #17458, #51658, #85797, #9095, #105369, #35961, #88574, #11317, #11857, #37050, #69587, #53898, #36504, #61194, #79629 ),
 .UNSPECIFIED., .F., .F.,
 ( 4, 2, 2, 1, 1, 1, 1, 2, 2, 4 ),
 ( 0.000000000000000000, 0.2499999999999679146, 0.3749999999999507616, 0.4374999999999422129, 0.4687499999999449329, 0.4843749999999474865, 0.4921874999999487632, 0.4960937499999555356, 0.4999999999999622524, 1.000000000000000000 ),
 .UNSPECIFIED. ) ;
#66510 = CARTESIAN_POINT ( 'NONE',  ( -9.724834716106559089E-16, 1374.031200045389824, 209.1218459616989946 ) ) ;
#66512 = CARTESIAN_POINT ( 'NONE',  ( -22.64739172320458849, 1509.725407825014599, 228.2189809371752460 ) ) ;
#66513 = CARTESIAN_POINT ( 'NONE',  ( 18.22865577494500045, 1459.310763497099970, 227.8759328773050186 ) ) ;
#66514 = CARTESIAN_POINT ( 'NONE',  ( 17.19739463999625784, 1525.960063244516959, 181.9833109756548595 ) ) ;
#66515 = CARTESIAN_POINT ( 'NONE',  ( 12.62835224979999893, 1416.067629290630066, 222.6573521500980064 ) ) ;
#66516 = CARTESIAN_POINT ( 'NONE',  ( 2.830001175615096454, 1451.807281766560891, 183.8374670539779174 ) ) ;
#66517 = CARTESIAN_POINT ( 'NONE',  ( 4.747050408260000687, 1486.851065980389876, 199.2547198969290037 ) ) ;
#66518 = CARTESIAN_POINT ( 'NONE',  ( -3.269259737218870310, 1476.740802116999930, 199.2818558394819775 ) ) ;
#66519 = CARTESIAN_POINT ( 'NONE',  ( 4.278374243669960109, 1441.027869772839949, 156.7540461662579787 ) ) ;
#66520 = CARTESIAN_POINT ( 'NONE',  ( -1.842963787330039960, 1515.551704393028331, 205.1635077660893387 ) ) ;
#66521 = DIRECTION ( 'NONE',  ( -2.513978196838388281E-18, -0.7071067811865475727, -0.7071067811865475727 ) ) ;
#66522 = CARTESIAN_POINT ( 'NONE',  ( 5.780861236055000241, 1516.783701990830195, 216.0610654530370027 ) ) ;
#66523 = ORIENTED_EDGE ( 'NONE', *, *, #7521, .T. ) ;
#66524 = CARTESIAN_POINT ( 'NONE',  ( -12.77825866169999891, 1416.543503932829935, 195.9645815386980132 ) ) ;
#66525 = CARTESIAN_POINT ( 'NONE',  ( 16.16926794620007257, 1409.477699224023809, 193.1978555737975682 ) ) ;
#66526 = CARTESIAN_POINT ( 'NONE',  ( 2.250225901099999870, 1421.216712495730008, 183.8152323106979793 ) ) ;
#66527 = CARTESIAN_POINT ( 'NONE',  ( -0.2610938271800009591, 1474.054394607790073, 219.3955652254989843 ) ) ;
#66528 = DIRECTION ( 'NONE',  ( -0.8672669759446596238, 0.000000000000000000, 0.4978433412588795792 ) ) ;
#66529 = CARTESIAN_POINT ( 'NONE',  ( -11.18513414810809969, 1471.346656141509811, 206.8404382864960098 ) ) ;
#66530 = CARTESIAN_POINT ( 'NONE',  ( -33.36586802512168504, 1523.382868172864164, 216.3367586934473366 ) ) ;
#66531 = CARTESIAN_POINT ( 'NONE',  ( 18.76751273909999895, 1416.021639799829927, 210.4841606299879970 ) ) ;
#66532 = CARTESIAN_POINT ( 'NONE',  ( 0.3799711347515690174, 1455.871197009739944, 198.5797350333110103 ) ) ;
#66533 = CARTESIAN_POINT ( 'NONE',  ( -1.984413551915469975, 1517.051704408389924, 219.3307686695569885 ) ) ;
#66534 = CARTESIAN_POINT ( 'NONE',  ( 1.393816646507350709, 1511.187213306747708, 175.1051575864439656 ) ) ;
#66536 = DIRECTION ( 'NONE',  ( -1.755985294532469921E-16, 1.000000000000000000, -1.338183447452831989E-16 ) ) ;
#66535 = CARTESIAN_POINT ( 'NONE',  ( -10.10799952816689995, 1471.968561594289895, 210.1976632032360044 ) ) ;
#66537 = CARTESIAN_POINT ( 'NONE',  ( -3.179847367899999888, 1481.779546599790137, 229.4457135908990040 ) ) ;
#66538 = VERTEX_POINT ( 'NONE', #49728 ) ;
#66539 = ORIENTED_EDGE ( 'NONE', *, *, #49364, .T. ) ;
#66540 = CARTESIAN_POINT ( 'NONE',  ( 10.47512669263509899, 1482.041014330849976, 210.7459474806360049 ) ) ;
#66541 = ADVANCED_FACE ( 'NONE', ( #65992 ), #73266, .F. ) ;
#66542 = CARTESIAN_POINT ( 'NONE',  ( 16.34617637888406705, 1409.483876603966110, 193.1367303227071659 ) ) ;
#66543 = AXIS2_PLACEMENT_3D ( 'NONE', #59155, #110086, #16538 ) ;
#66544 = CARTESIAN_POINT ( 'NONE',  ( -3.061334144399999957, 1442.717432058590020, 200.6190578008389878 ) ) ;
#66545 = DIRECTION ( 'NONE',  ( -0.9996573249755574819, 0.02617694830786558916, 0.000000000000000000 ) ) ;
#66546 = EDGE_CURVE ( 'NONE', #43885, #53799, #100114, .T. ) ;
#66547 = CARTESIAN_POINT ( 'NONE',  ( 207.7471169361000136, -8387.357407334289746, -1761.517333167069864 ) ) ;
#66548 = DIRECTION ( 'NONE',  ( 0.000000000000000000, -1.000000000000000000, 6.123233995736769734E-17 ) ) ;
#66549 = CARTESIAN_POINT ( 'NONE',  ( -1.561041872522580087, 1508.551704408389924, 220.0816520586899969 ) ) ;
#66550 = CARTESIAN_POINT ( 'NONE',  ( 16.68062049856701989, 1524.382868172863937, 181.4122394607862816 ) ) ;
#66551 = CARTESIAN_POINT ( 'NONE',  ( -48.47771611847429796, 1383.814425808469878, 258.2089094142469889 ) ) ;
#66552 = CARTESIAN_POINT ( 'NONE',  ( -4.678143775780629454, 1508.611354794059935, 206.6339233318589947 ) ) ;
#66553 = CARTESIAN_POINT ( 'NONE',  ( -13.85509113240000012, 1453.154616238129847, 193.9807013630980066 ) ) ;
#66554 = CARTESIAN_POINT ( 'NONE',  ( -27.44229999310290680, 1509.334241622238778, 212.0840502660885249 ) ) ;
#66555 = CARTESIAN_POINT ( 'NONE',  ( 10.82590729831830068, 1491.268289583239948, 211.1351721366039840 ) ) ;
#66557 = ORIENTED_EDGE ( 'NONE', *, *, #46707, .T. ) ;
#66556 = CARTESIAN_POINT ( 'NONE',  ( -11.16717556649999921, 1414.661898229710005, 212.7267128011690147 ) ) ;
#66558 = CARTESIAN_POINT ( 'NONE',  ( 33.52308185467592239, 1525.402221411349501, 217.5800527287148043 ) ) ;
#66559 = AXIS2_PLACEMENT_3D ( 'NONE', #87884, #71664, #45335 ) ;
#66560 = ADVANCED_FACE ( 'NONE', ( #7161 ), #47394, .F. ) ;
#66561 = CARTESIAN_POINT ( 'NONE',  ( -36.25797752260000095, 1383.833857111379984, 235.3800711337590030 ) ) ;
#66562 = CARTESIAN_POINT ( 'NONE',  ( 4.889439660094519802, 1508.551704408389924, 205.9425365203790079 ) ) ;
#66563 = ORIENTED_EDGE ( 'NONE', *, *, #61940, .F. ) ;
#66564 = ORIENTED_EDGE ( 'NONE', *, *, #83101, .F. ) ;
#66565 =( BOUNDED_CURVE ( )  B_SPLINE_CURVE ( 3, ( #58202, #50366, #42488, #84492 ),
 .UNSPECIFIED., .F., .T. ) 
 B_SPLINE_CURVE_WITH_KNOTS ( ( 4, 4 ),
 ( 5.330947148644519906, 5.979513181285929235 ),
 .UNSPECIFIED. ) 
 CURVE ( )  GEOMETRIC_REPRESENTATION_ITEM ( )  RATIONAL_B_SPLINE_CURVE ( ( 1.000000000000000000, 0.9652529480040055176, 0.9652529480040055176, 1.000000000000000000 ) ) 
 REPRESENTATION_ITEM ( '' )  );
#66566 = CARTESIAN_POINT ( 'NONE',  ( -8.464911085096829879, 1385.365015953710099, 218.6689375795459966 ) ) ;
#66567 = CARTESIAN_POINT ( 'NONE',  ( 35.81700442754009828, 1437.367486095130062, 136.5363678219200096 ) ) ;
#66569 = CARTESIAN_POINT ( 'NONE',  ( -9.833393186232900263, 1517.151704408390060, 212.5077547680540135 ) ) ;
#66568 = CARTESIAN_POINT ( 'NONE',  ( -111.9617233841873940, 1306.413060387289988, 301.5890982715878863 ) ) ;
#66570 = CARTESIAN_POINT ( 'NONE',  ( -9.457585828349998280, 1462.148799080189974, 206.2711936052490103 ) ) ;
#66571 = CARTESIAN_POINT ( 'NONE',  ( -105.7409752579999918, 1381.140865015730242, 299.3151906013590065 ) ) ;
#66572 = CARTESIAN_POINT ( 'NONE',  ( 2.765840199879999961, 1444.819550273290133, 203.5022050372989781 ) ) ;
#66573 = CARTESIAN_POINT ( 'NONE',  ( -9.088471267427010503, 1508.551704408389924, 218.6183512830809832 ) ) ;
#66574 = DIRECTION ( 'NONE',  ( -1.000000000000000000, 0.000000000000000000, 0.000000000000000000 ) ) ;
#66575 = CARTESIAN_POINT ( 'NONE',  ( 0.5133706386020000512, 1410.311097227529899, 185.0719932622980082 ) ) ;
#66576 = CARTESIAN_POINT ( 'NONE',  ( -13.33054336736499934, 1520.551704408390151, 207.1218459511669892 ) ) ;
#66577 = CARTESIAN_POINT ( 'NONE',  ( 7.311196690888119853, 1433.969857655230044, 203.9080805087000101 ) ) ;
#66578 = CARTESIAN_POINT ( 'NONE',  ( 11.76945428880000044, 1432.334073542720034, 150.8119095935979885 ) ) ;
#66579 = AXIS2_PLACEMENT_3D ( 'NONE', #35632, #46282, #87148 ) ;
#66580 = CARTESIAN_POINT ( 'NONE',  ( -2.101005067686500194, 1450.237514968539699, 183.4561686731089765 ) ) ;
#66581 = VERTEX_POINT ( 'NONE', #44081 ) ;
#66582 = EDGE_CURVE ( 'NONE', #51456, #48164, #50685, .T. ) ;
#66583 = CARTESIAN_POINT ( 'NONE',  ( -21.83117874278453741, 1524.760046179776054, 184.6256242011980930 ) ) ;
#66584 = CARTESIAN_POINT ( 'NONE',  ( 18.24783257861880159, 1458.395086229769959, 227.8518626438460046 ) ) ;
#66585 = EDGE_CURVE ( 'NONE', #63161, #12743, #22421, .T. ) ;
#66586 = DIRECTION ( 'NONE',  ( 0.8236474686107847498, 0.5669078173018529121, 0.01484500364079605582 ) ) ;
#66587 = CARTESIAN_POINT ( 'NONE',  ( -1.634883190284829911E-09, 1471.268413604999978, 257.2557666294709975 ) ) ;
#66588 = CARTESIAN_POINT ( 'NONE',  ( 16.96608709051594488, 1436.324541078401126, 148.2478660041307990 ) ) ;
#66589 = PLANE ( 'NONE',  #1768 ) ;
#66590 = CARTESIAN_POINT ( 'NONE',  ( -109.8314448029999966, 1386.134759465500110, 311.3488533982589388 ) ) ;
#66591 = CARTESIAN_POINT ( 'NONE',  ( -0.9064963533630000514, 1486.513385844430104, 181.9403208173980033 ) ) ;
#66592 = CARTESIAN_POINT ( 'NONE',  ( -10.56256883942626068, 1363.309231799455802, 207.6218459616987673 ) ) ;
#66593 = DIRECTION ( 'NONE',  ( -1.000000000000000000, 0.000000000000000000, 0.000000000000000000 ) ) ;
#66594 = CARTESIAN_POINT ( 'NONE',  ( 13.97271228624649986, 1509.364740696860054, 234.5129875352629938 ) ) ;
#66595 = CARTESIAN_POINT ( 'NONE',  ( -7.969533265219999940, 1425.156681655810189, 206.0885952228989879 ) ) ;
#66596 = ADVANCED_FACE ( 'NONE', ( #17169 ), #110167, .F. ) ;
#66597 = CARTESIAN_POINT ( 'NONE',  ( 1.122033391945000069, 1516.972341476009888, 208.3659064338399673 ) ) ;
#66598 = DIRECTION ( 'NONE',  ( 0.000000000000000000, -1.000000000000000000, 0.000000000000000000 ) ) ;
#66599 = CARTESIAN_POINT ( 'NONE',  ( -14.30024709372010072, 1379.589079739520002, 207.9540921923399708 ) ) ;
#66600 = CARTESIAN_POINT ( 'NONE',  ( 7.457299212086079265, 1425.231075921110005, 212.3345666727680054 ) ) ;
#66601 = EDGE_CURVE ( 'NONE', #64966, #31041, #72005, .T. ) ;
#66602 = ORIENTED_EDGE ( 'NONE', *, *, #34965, .T. ) ;
#66603 = CARTESIAN_POINT ( 'NONE',  ( 28.07850872979999934, 1439.094797578370162, 231.9053043656980151 ) ) ;
#66605 = CARTESIAN_POINT ( 'NONE',  ( -15.13257544217990080, 1512.281672892730057, 221.8969035856549965 ) ) ;
#66604 = CARTESIAN_POINT ( 'NONE',  ( -2.531548701460000217, 1486.446787100029951, 181.7283458845979851 ) ) ;
#66606 = CARTESIAN_POINT ( 'NONE',  ( -6.338357687459999390, 1461.235457266589947, 207.8854984423689984 ) ) ;
#66607 = CARTESIAN_POINT ( 'NONE',  ( -5.432410439650000811, 1391.426148861440197, 214.9021618825790085 ) ) ;
#66608 = CARTESIAN_POINT ( 'NONE',  ( -28.81229682350082300, 1509.921425474858097, 203.0494097711116410 ) ) ;
#66609 = DIRECTION ( 'NONE',  ( -5.980589973904019347E-17, 1.000000000000000000, -1.736889445713099699E-16 ) ) ;
#66610 = CARTESIAN_POINT ( 'NONE',  ( 9859.020463722770728, 54.07981494723821925, 1360.877155955070066 ) ) ;
#66611 = EDGE_LOOP ( 'NONE', ( #7484, #107275, #94835, #33923 ) ) ;
#66612 = CARTESIAN_POINT ( 'NONE',  ( -5.370353317006889782, 1427.592827902419913, 153.4505299550590109 ) ) ;
#66613 = CARTESIAN_POINT ( 'NONE',  ( 13.58235846979999906, 1416.828040475229955, 196.3349388281980055 ) ) ;
#66614 = CARTESIAN_POINT ( 'NONE',  ( 14.59153218112539996, 1421.962858571700053, 230.0979270886319910 ) ) ;
#66615 = CARTESIAN_POINT ( 'NONE',  ( 10.14394188820000053, 1461.870444916690076, 209.6790091569899914 ) ) ;
#66616 = EDGE_LOOP ( 'NONE', ( #65624, #63677, #107058, #2847, #46095, #20833, #70570, #110142, #14609, #95631 ) ) ;
#66617 = ORIENTED_EDGE ( 'NONE', *, *, #106213, .F. ) ;
#66618 = EDGE_CURVE ( 'NONE', #36010, #33249, #51362, .T. ) ;
#66619 = CARTESIAN_POINT ( 'NONE',  ( -31.91391880200000131, 1384.560375756019766, 206.3213236589990061 ) ) ;
#66620 = CARTESIAN_POINT ( 'NONE',  ( -22.71590553989589978, 1409.706312905169852, 209.0156571623660113 ) ) ;
#66621 = EDGE_LOOP ( 'NONE', ( #31439, #94692, #93739, #71027, #28415 ) ) ;
#66622 = CARTESIAN_POINT ( 'NONE',  ( -113.4000000000000057, 1305.714868215269917, 304.2218459572590064 ) ) ;
#66623 = CARTESIAN_POINT ( 'NONE',  ( -4.496878417739999634, 1428.155750001629940, 101.8807690336980016 ) ) ;
#66624 = EDGE_CURVE ( 'NONE', #62944, #39452, #28372, .T. ) ;
#66625 = CARTESIAN_POINT ( 'NONE',  ( -0.4200920693160000163, 1507.643922758529925, 237.3276516554979878 ) ) ;
#66626 = CARTESIAN_POINT ( 'NONE',  ( 3.747941686733399891, 1508.879013277289914, 213.3683127840300244 ) ) ;
#66627 = ORIENTED_EDGE ( 'NONE', *, *, #11981, .F. ) ;
#66628 = CARTESIAN_POINT ( 'NONE',  ( 44.13469765186309957, 1449.794459338159868, 269.0171759414279791 ) ) ;
#66629 = CARTESIAN_POINT ( 'NONE',  ( -1.210427285455619950, 1424.150940588480125, 228.3852517110850044 ) ) ;
#66630 = CARTESIAN_POINT ( 'NONE',  ( -0.3973369724709999717, 1418.672808243929921, 184.7148013090980214 ) ) ;
#66631 = CARTESIAN_POINT ( 'NONE',  ( 2.285487581364999965, 1517.001127920769704, 205.0775242521070254 ) ) ;
#66632 = ORIENTED_EDGE ( 'NONE', *, *, #95252, .F. ) ;
#66633 = CARTESIAN_POINT ( 'NONE',  ( 18.94672925339437342, 1457.565180153704205, 226.7986852134035871 ) ) ;
#66634 = CARTESIAN_POINT ( 'NONE',  ( 14.72577158086200022, 1514.214451999800076, 194.1036973123569851 ) ) ;
#66635 = CARTESIAN_POINT ( 'NONE',  ( 17.69622990075129820, 1430.679836004809886, 213.5595397380919849 ) ) ;
#66636 = ORIENTED_EDGE ( 'NONE', *, *, #18001, .T. ) ;
#66637 = LINE ( 'NONE', #16715, #37413 ) ;
#66638 = CARTESIAN_POINT ( 'NONE',  ( 26.79276161880000018, 1451.726218324329693, 135.7942559489979999 ) ) ;
#66639 = CARTESIAN_POINT ( 'NONE',  ( -12.22498602940789958, 1512.125809830880144, 194.3608099058220091 ) ) ;
#66640 = CARTESIAN_POINT ( 'NONE',  ( 0.3648627223273580023, 1452.900319100310071, 152.5217687494670145 ) ) ;
#66641 = CARTESIAN_POINT ( 'NONE',  ( 7.474305816439999361, 1422.145197690320174, 195.6519535563990075 ) ) ;
#66642 = CARTESIAN_POINT ( 'NONE',  ( 16.87240902346729854, 1409.502257893559772, 222.1138755377239988 ) ) ;
#66643 = CARTESIAN_POINT ( 'NONE',  ( -5.094674989349999628, 1496.284763139690085, 199.1200413041989918 ) ) ;
#66644 = CARTESIAN_POINT ( 'NONE',  ( 12.20337053245270020, 1409.339211476720038, 191.6948814310479747 ) ) ;
#66646 = CARTESIAN_POINT ( 'NONE',  ( -11.22085813611739979, 1414.913060387329779, 220.6193216859199993 ) ) ;
#66645 = CARTESIAN_POINT ( 'NONE',  ( -13.11275527770450111, 1434.829963905530121, 149.0799834946710121 ) ) ;
#66647 = CARTESIAN_POINT ( 'NONE',  ( 10.68158499005449968, 1423.994661768180094, 206.6794003566110121 ) ) ;
#66648 = CARTESIAN_POINT ( 'NONE',  ( -12.24671249760000080, 1378.552623650770101, 211.6779590913389768 ) ) ;
#66649 = CARTESIAN_POINT ( 'NONE',  ( -7.962346614255001676, 1514.830240247470101, 203.0623562961069979 ) ) ;
#66650 = ORIENTED_EDGE ( 'NONE', *, *, #73820, .F. ) ;
#66651 = CARTESIAN_POINT ( 'NONE',  ( 12.78776258890000150, 1416.851343897030119, 222.2791103843980238 ) ) ;
#66652 = CARTESIAN_POINT ( 'NONE',  ( -30.25425994617014780, 1526.382868172863937, 199.2916410102373277 ) ) ;
#66653 = CARTESIAN_POINT ( 'NONE',  ( -108.2120120822389850, 1384.926448218169980, 311.2629986585570236 ) ) ;
#66654 = CARTESIAN_POINT ( 'NONE',  ( -10.17260142399999978, 1386.954104889990049, 200.6847011332289981 ) ) ;
#66655 = CARTESIAN_POINT ( 'NONE',  ( 9.784730986437239153, 1426.272936423899864, 209.3148760698660169 ) ) ;
#66656 = CARTESIAN_POINT ( 'NONE',  ( 11.35995302351660108, 1425.310403992989905, 202.9730432884799995 ) ) ;
#66657 = B_SPLINE_CURVE_WITH_KNOTS ( 'NONE', 3,
 ( #59475, #60027, #25274, #24717, #42109, #49959, #50519, #25826, #94145, #101425, #34249, #17416, #103089, #92489, #41561, #669, #8482, #109322, #68988, #93045, #34800, #126, #109862, #84095 ),
 .UNSPECIFIED., .F., .F.,
 ( 4, 2, 2, 1, 1, 1, 1, 1, 1, 2, 2, 2, 2, 2, 4 ),
 ( 0.000000000000000000, 0.2499999999998854805, 0.3749999999998297473, 0.4374999999998017697, 0.4687499999997883360, 0.4843749999997818412, 0.4921874999997785660, 0.4960937499997771227, 0.4980468749997753464, 0.4990234374997746247, 0.4999999999997739586, 0.7499999999998890887, 0.8124999999999159561, 0.8749999999999427125, 1.000000000000000000 ),
 .UNSPECIFIED. ) ;
#66658 = FACE_OUTER_BOUND ( 'NONE', #15150, .T. ) ;
#66659 = CARTESIAN_POINT ( 'NONE',  ( -2.451271202390000070, 1433.447543843880112, 150.3250444719979839 ) ) ;
#66660 = CARTESIAN_POINT ( 'NONE',  ( -21.95659415135585846, 1509.539901157007534, 191.3931345191016931 ) ) ;
#66661 = CARTESIAN_POINT ( 'NONE',  ( -12.87561223598270033, 1428.667272998819954, 222.5140706137790119 ) ) ;
#66662 = CARTESIAN_POINT ( 'NONE',  ( 29.75208676419999776, 1462.665512622030064, 268.3665355201979992 ) ) ;
#66663 = CARTESIAN_POINT ( 'NONE',  ( 13.15726442270000085, 1416.851343897030119, 196.3340833727979771 ) ) ;
#66664 = CARTESIAN_POINT ( 'NONE',  ( 1.213697692988580545, 1466.857525291594811, 235.2505294708204246 ) ) ;
#66665 = CARTESIAN_POINT ( 'NONE',  ( -9.202936508599998788, 1519.913060387329779, 230.3262217860979888 ) ) ;
#66666 = CARTESIAN_POINT ( 'NONE',  ( 5.275783403443830899, 1466.070747001820109, 217.9942205468059910 ) ) ;
#66667 = EDGE_CURVE ( 'NONE', #53940, #98249, #87747, .T. ) ;
#66668 = CARTESIAN_POINT ( 'NONE',  ( -19.61825196109999681, 1486.333718774929821, 189.8690818786980117 ) ) ;
#66669 = CYLINDRICAL_SURFACE ( 'NONE', #19908, 2.000000000000009770 ) ;
#66670 = CARTESIAN_POINT ( 'NONE',  ( 17.54299231450000107, 1415.063410489729904, 210.2814835228880099 ) ) ;
#66671 = CARTESIAN_POINT ( 'NONE',  ( 23.70212955589999737, 1410.915617627129905, 211.1403328626279858 ) ) ;
#66672 = CARTESIAN_POINT ( 'NONE',  ( -0.2024664826940029971, 1479.235308103189936, 229.5453557735989989 ) ) ;
#66673 = CARTESIAN_POINT ( 'NONE',  ( -3.246772394788719929, 1512.187213306747481, 241.0944358625217774 ) ) ;
#66674 = CARTESIAN_POINT ( 'NONE',  ( 12.45642912959999826, 1416.822692871130130, 223.4763060122980107 ) ) ;
#66675 = CARTESIAN_POINT ( 'NONE',  ( -0.6235920161070115375, 1525.878013734321257, 175.2961586039431552 ) ) ;
#66676 = CARTESIAN_POINT ( 'NONE',  ( 3.217370148928750062, 1424.184623195729955, 188.9579834054289904 ) ) ;
#66677 = CARTESIAN_POINT ( 'NONE',  ( -11.41806921110000062, 1414.913060387329779, 220.8525480562979908 ) ) ;
#66678 = CARTESIAN_POINT ( 'NONE',  ( 0.2023891958416690062, 1461.642228596550012, 182.8826039181769829 ) ) ;
#66680 = ORIENTED_EDGE ( 'NONE', *, *, #32316, .F. ) ;
#66679 = CARTESIAN_POINT ( 'NONE',  ( -5.619561408211779963, 1407.449627137000107, 221.3655341017839930 ) ) ;
#66681 = CARTESIAN_POINT ( 'NONE',  ( 2.385013337802738498, 1526.073434386619056, 177.7125070007693353 ) ) ;
#66682 = EDGE_CURVE ( 'NONE', #109192, #91565, #91862, .T. ) ;
#66683 = CARTESIAN_POINT ( 'NONE',  ( -15.17700602440057622, 1445.095295946591477, 196.7536451946974410 ) ) ;
#66684 = CARTESIAN_POINT ( 'NONE',  ( 11.87905392670000104, 1433.311775745339901, 149.9804763676980031 ) ) ;
#66685 = CARTESIAN_POINT ( 'NONE',  ( -41.63323805074259809, 1443.027121606309947, 134.0999999981200119 ) ) ;
#66686 = DIRECTION ( 'NONE',  ( -0.7067700477543440440, -0.03085664260726115465, 0.7067700950127487891 ) ) ;
#66687 = ORIENTED_EDGE ( 'NONE', *, *, #59018, .F. ) ;
#66688 = CARTESIAN_POINT ( 'NONE',  ( -0.5111327314519990006, 1484.634848108790038, 198.3940791051990118 ) ) ;
#66689 = CARTESIAN_POINT ( 'NONE',  ( 9.831955598149999531, 1479.326580839289818, 204.9319913846790087 ) ) ;
#66690 = CARTESIAN_POINT ( 'NONE',  ( -105.8150085967258605, 1381.470779566475130, 309.3040015815146830 ) ) ;
#66691 = DIRECTION ( 'NONE',  ( -6.123233995736769734E-17, -1.000000000000000000, 0.000000000000000000 ) ) ;
#66692 = EDGE_CURVE ( 'NONE', #65245, #46100, #72070, .T. ) ;
#66693 = FACE_OUTER_BOUND ( 'NONE', #46760, .T. ) ;
#66694 = CARTESIAN_POINT ( 'NONE',  ( -108.2287821362297251, 1381.019133052909638, 310.1919587077548499 ) ) ;
#66695 = CARTESIAN_POINT ( 'NONE',  ( -16.96581893389999962, 1420.808731266319910, 208.6966097274290064 ) ) ;
#66696 = CARTESIAN_POINT ( 'NONE',  ( 3.500000000000000000, 1420.857604035629947, 170.3256330572980062 ) ) ;
#66697 = CARTESIAN_POINT ( 'NONE',  ( 2.662604276420000193, 1436.925442033910031, 183.9139560369979733 ) ) ;
#66698 = CARTESIAN_POINT ( 'NONE',  ( -54.33537259569690292, 1385.035685468000111, 232.6071117302159905 ) ) ;
#66699 = CARTESIAN_POINT ( 'NONE',  ( -18.88880210472915877, 1524.667648926078755, 238.8296805722607417 ) ) ;
#66700 = CARTESIAN_POINT ( 'NONE',  ( 11.73186578479040065, 1421.919406218840095, 207.6102233476609911 ) ) ;
#66701 = CARTESIAN_POINT ( 'NONE',  ( -30.93305786360000198, 1450.544576909440138, 136.3330928348979967 ) ) ;
#66702 = CARTESIAN_POINT ( 'NONE',  ( -15.91753217932039632, 1410.856834153720001, 226.7185307615260115 ) ) ;
#66704 = ORIENTED_EDGE ( 'NONE', *, *, #28127, .F. ) ;
#66703 = CARTESIAN_POINT ( 'NONE',  ( 11.60004869885203682, 1428.983126981193436, 137.0999999980966777 ) ) ;
#66705 = CARTESIAN_POINT ( 'NONE',  ( -109.1309838760000019, 1384.924126712679936, 311.2646841762590384 ) ) ;
#66706 = CARTESIAN_POINT ( 'NONE',  ( 10.51937569161310115, 1470.762630565469863, 209.9255540597749814 ) ) ;
#66707 = B_SPLINE_CURVE_WITH_KNOTS ( 'NONE', 3,
 ( #68137, #84889, #33379, #26078, #51298, #75955 ),
 .UNSPECIFIED., .F., .F.,
 ( 4, 2, 4 ),
 ( 0.000000000000000000, 0.5000000000000001110, 1.000000000000000000 ),
 .UNSPECIFIED. ) ;
#66708 = CARTESIAN_POINT ( 'NONE',  ( -20.22565842890162813, 1410.979628444421451, 220.3650596930099823 ) ) ;
#66709 = CARTESIAN_POINT ( 'NONE',  ( -109.8184593100000086, 1384.563165728690137, 311.3672836522590046 ) ) ;
#66710 = CARTESIAN_POINT ( 'NONE',  ( -0.3936502047466580168, 1418.683933865910149, 184.7134515189369779 ) ) ;
#66711 = B_SPLINE_CURVE_WITH_KNOTS ( 'NONE', 5,
 ( #11820, #15506, #7136, #14412, #31228, #20746 ),
 .UNSPECIFIED., .F., .F.,
 ( 6, 6 ),
 ( 0.000000000000000000, 3.472809815250000209 ),
 .UNSPECIFIED. ) ;
#66712 = EDGE_CURVE ( 'NONE', #16710, #92713, #25885, .T. ) ;
#66713 = CARTESIAN_POINT ( 'NONE',  ( 21.48911905780000353, 1409.663476963630046, 214.7487920242479902 ) ) ;
#66714 = CARTESIAN_POINT ( 'NONE',  ( 14.84895960065126275, 1511.957228877181251, 197.0446257365507563 ) ) ;
#66715 = CARTESIAN_POINT ( 'NONE',  ( -17.36099134979999903, 1423.305661865730144, 226.7048953899980006 ) ) ;
#66716 = CARTESIAN_POINT ( 'NONE',  ( -10.96878236979999954, 1432.307827591499972, 151.7701597093980013 ) ) ;
#66717 = CARTESIAN_POINT ( 'NONE',  ( 9.549998141239999683, 1451.222071590189898, 207.5451647913689897 ) ) ;
#66718 = CARTESIAN_POINT ( 'NONE',  ( -96.14154407968888449, 1340.114449826970031, 304.2218459572590064 ) ) ;
#66719 = ADVANCED_FACE ( 'NONE', ( #97774 ), #107285, .T. ) ;
#66720 = CARTESIAN_POINT ( 'NONE',  ( -3.942352636383586795, 1370.082171903791277, 207.6218459616987673 ) ) ;
#66721 = B_SPLINE_CURVE_WITH_KNOTS ( 'NONE', 5,
 ( #36133, #62470, #28276, #88192, #11485, #77583, #10363, #61910, #61361, #17631, #79246, #28835, #18747, #9272, #70318 ),
 .UNSPECIFIED., .F., .F.,
 ( 6, 3, 3, 3, 6 ),
 ( 0.000000000000000000, 0.3593463541239135250, 0.6253129843951757971, 0.8912796146636228212, 1.000000000000000000 ),
 .UNSPECIFIED. ) ;
#66722 = CARTESIAN_POINT ( 'NONE',  ( -2.514213374330000139, 1455.572514118689924, 199.8771817507590072 ) ) ;
#66723 = EDGE_CURVE ( 'NONE', #52165, #12260, #95610, .T. ) ;
#66724 = CARTESIAN_POINT ( 'NONE',  ( -1.135460355084999762, 1516.790374942449944, 205.8685445508469911 ) ) ;
#66725 = CARTESIAN_POINT ( 'NONE',  ( 2.500000000000000000, 1448.197706736549890, 167.4845663187979881 ) ) ;
#66726 = ORIENTED_EDGE ( 'NONE', *, *, #17858, .T. ) ;
#66727 = CARTESIAN_POINT ( 'NONE',  ( -107.2902847454959954, 1391.913060387289988, 307.3027153792770036 ) ) ;
#66728 = CARTESIAN_POINT ( 'NONE',  ( -4.226271147029579289, 1441.565518713930032, 166.0303910921570036 ) ) ;
#66730 = ORIENTED_EDGE ( 'NONE', *, *, #31936, .F. ) ;
#66729 = CARTESIAN_POINT ( 'NONE',  ( -68.49156254684720579, 1379.747260696060039, 280.0978574668839656 ) ) ;
#66731 = EDGE_CURVE ( 'NONE', #73174, #100464, #77000, .T. ) ;
#66732 = CARTESIAN_POINT ( 'NONE',  ( -11.18760872067141321, 1378.375624679992598, 214.3033515264987727 ) ) ;
#66733 = ORIENTED_EDGE ( 'NONE', *, *, #58323, .F. ) ;
#66734 = CARTESIAN_POINT ( 'NONE',  ( -15.90990515426090113, 1514.921193439799936, 224.3246443988719818 ) ) ;
#66735 = CARTESIAN_POINT ( 'NONE',  ( 12.20582139389999909, 1500.450892145889839, 208.0634134494790146 ) ) ;
#66737 = CARTESIAN_POINT ( 'NONE',  ( 16.01538719336489791, 1409.574438585999815, 192.4055768128030195 ) ) ;
#66736 = CARTESIAN_POINT ( 'NONE',  ( -11.44511274162072922, 1425.476693466300048, 144.6899562955641727 ) ) ;
#66738 = CARTESIAN_POINT ( 'NONE',  ( -3.251611363945000388, 1516.779243033999819, 211.4202154400570066 ) ) ;
#66739 = CARTESIAN_POINT ( 'NONE',  ( 41.33979271583219628, 1441.992233827169912, 136.3820788539130149 ) ) ;
#66740 = CARTESIAN_POINT ( 'NONE',  ( -106.6028128171490010, 1378.913060387289988, 306.5905933178560190 ) ) ;
#66741 = CARTESIAN_POINT ( 'NONE',  ( -31.23437356469425907, 1518.913060387330006, 221.8968241038848248 ) ) ;
#66742 = CARTESIAN_POINT ( 'NONE',  ( 16.20733605427863466, 1461.062281268581728, 229.2672831881708646 ) ) ;
#66743 = SHAPE_DEFINITION_REPRESENTATION ( #36561, #83713 ) ;
#66744 = B_SPLINE_CURVE_WITH_KNOTS ( 'NONE', 3,
 ( #28871, #96626, #105022, #63065, #72533, #106124, #11519, #29399, #63600, #64147, #98266, #46247, #88777, #97718, #12615, #19336, #55749, #10965, #44570 ),
 .UNSPECIFIED., .F., .F.,
 ( 4, 3, 3, 3, 3, 3, 4 ),
 ( -7.661770161623569386, -7.428136132220500620, -6.292251436735150527, -5.400505869387740354, -4.641385543154090243, -3.845608395895360410, -3.139241426659999945 ),
 .UNSPECIFIED. ) ;
#66745 = CARTESIAN_POINT ( 'NONE',  ( 35.94635777376459629, 1451.396212934409959, 134.0999999986040052 ) ) ;
#66746 = DIRECTION ( 'NONE',  ( -0.000000000000000000, -1.000000000000000000, -0.000000000000000000 ) ) ;
#66747 = ORIENTED_EDGE ( 'NONE', *, *, #59412, .F. ) ;
#66748 = CARTESIAN_POINT ( 'NONE',  ( 22.14279730899999876, 1473.984189751590065, 210.1089390466149780 ) ) ;
#66749 = EDGE_CURVE ( 'NONE', #102658, #1876, #2687, .T. ) ;
#66750 = CARTESIAN_POINT ( 'NONE',  ( 4.500000000000000000, 1417.575542696430148, 161.0097146498980010 ) ) ;
#66751 = ORIENTED_EDGE ( 'NONE', *, *, #110155, .T. ) ;
#66752 = EDGE_LOOP ( 'NONE', ( #236, #82196, #100471, #80676 ) ) ;
#66753 = CARTESIAN_POINT ( 'NONE',  ( -29.73446499118736241, 1509.991171415641929, 209.9271895720580119 ) ) ;
#66754 = CARTESIAN_POINT ( 'NONE',  ( 10.42657513622150134, 1453.119160424219899, 211.0495624056229929 ) ) ;
#66755 = CARTESIAN_POINT ( 'NONE',  ( 0.2353718297500000112, 1450.904841021550055, 181.9002531089979868 ) ) ;
#66756 = CARTESIAN_POINT ( 'NONE',  ( -18.43454007138939943, 1507.986789759319890, 209.4721884240840097 ) ) ;
#66757 = CARTESIAN_POINT ( 'NONE',  ( -2.500000000000000000, 1439.450741932119854, 162.6867559029170138 ) ) ;
#66758 = ADVANCED_FACE ( 'NONE', ( #98876 ), #73321, .T. ) ;
#66759 = CARTESIAN_POINT ( 'NONE',  ( -15.81201443571409904, 1506.433683733589987, 193.8503163142329981 ) ) ;
#66760 = CARTESIAN_POINT ( 'NONE',  ( -12.31967538750000202, 1378.053937865659918, 209.2867312853659882 ) ) ;
#66761 = CARTESIAN_POINT ( 'NONE',  ( 36.37832870499009630, 1435.767865672110020, 135.0591074476149913 ) ) ;
#66762 = DIRECTION ( 'NONE',  ( 1.755985294532469921E-16, -1.000000000000000000, 1.338183447452831989E-16 ) ) ;
#66763 = CARTESIAN_POINT ( 'NONE',  ( 30.24841015875314909, 1524.082740465118832, 222.4736143106622706 ) ) ;
#66764 = ADVANCED_FACE ( 'NONE', ( #22693 ), #81288, .T. ) ;
#66765 = CARTESIAN_POINT ( 'NONE',  ( -11.69890093100000072, 1391.698097032839769, 212.7312234011589851 ) ) ;
#66766 = CARTESIAN_POINT ( 'NONE',  ( -74.96309076845238906, 1384.767266604889983, 275.4021836984660467 ) ) ;
#66767 = EDGE_LOOP ( 'NONE', ( #88761, #30474, #4911, #11920, #50835 ) ) ;
#66768 =( BOUNDED_CURVE ( )  B_SPLINE_CURVE ( 3, ( #101855, #110827, #17842, #7270 ),
 .UNSPECIFIED., .F., .T. ) 
 B_SPLINE_CURVE_WITH_KNOTS ( ( 4, 4 ),
 ( 1.007411674165658022, 2.134181044723490128 ),
 .UNSPECIFIED. ) 
 CURVE ( )  GEOMETRIC_REPRESENTATION_ITEM ( )  RATIONAL_B_SPLINE_CURVE ( ( 1.000000000000000000, 0.8969682421527426230, 0.8969682421527426230, 1.000000000000000000 ) ) 
 REPRESENTATION_ITEM ( '' )  );
#66769 = CARTESIAN_POINT ( 'NONE',  ( 2.290886266485000267, 1517.184383877180153, 201.7830921018669983 ) ) ;
#66770 = CARTESIAN_POINT ( 'NONE',  ( -5.014195139944999546, 1517.120861839400050, 207.4163795216369977 ) ) ;
#66771 = ORIENTED_EDGE ( 'NONE', *, *, #9926, .T. ) ;
#66772 = CARTESIAN_POINT ( 'NONE',  ( 11.81027685177540043, 1428.753867292769883, 148.6741505271899939 ) ) ;
#66773 = CARTESIAN_POINT ( 'NONE',  ( 19.44271374779999917, 1487.524084985929903, 228.4659268090980220 ) ) ;
#66774 = ORIENTED_EDGE ( 'NONE', *, *, #69348, .T. ) ;
#66775 = CARTESIAN_POINT ( 'NONE',  ( -14.45750869480000134, 1416.828040475729949, 221.3916373288979855 ) ) ;
#66776 = CARTESIAN_POINT ( 'NONE',  ( 6.360756793238519613, 1429.512739015589887, 216.1615566237340147 ) ) ;
#66777 = CARTESIAN_POINT ( 'NONE',  ( -18.44377863300000087, 1443.022878208090106, 205.4489113795289938 ) ) ;
#66778 = CARTESIAN_POINT ( 'NONE',  ( 9.638115859575000499, 1520.551704408390151, 214.4931927712770232 ) ) ;
#66779 = CARTESIAN_POINT ( 'NONE',  ( -12.90256217089999957, 1426.055024770130103, 222.3411140444979992 ) ) ;
#66780 = CARTESIAN_POINT ( 'NONE',  ( -10.29555775080639002, 1446.577085899077929, 153.2855484792325171 ) ) ;
#66781 = DIRECTION ( 'NONE',  ( 0.9455185755993178454, 0.000000000000000000, -0.3255681544571537578 ) ) ;
#66782 = CARTESIAN_POINT ( 'NONE',  ( 7.229059247251790943, 1441.096153942899946, 154.2643636836130270 ) ) ;
#66783 = CARTESIAN_POINT ( 'NONE',  ( -17.16792151400000321, 1507.624001480129891, 224.4229799719980178 ) ) ;
#66785 = CARTESIAN_POINT ( 'NONE',  ( -3.045280019940000305, 1464.258769156330118, 184.9382089438980188 ) ) ;
#66784 = CARTESIAN_POINT ( 'NONE',  ( 12.17526685459999847, 1461.764631763230000, 233.4497560276980153 ) ) ;
#66786 = CARTESIAN_POINT ( 'NONE',  ( 19.55988977460000200, 1474.636381753090063, 214.0184790771390055 ) ) ;
#66787 = CARTESIAN_POINT ( 'NONE',  ( 3.454748808194999743, 1516.609912606490070, 216.4448802441970088 ) ) ;
#66788 = EDGE_LOOP ( 'NONE', ( #103246, #96537, #87912, #11630 ) ) ;
#66789 = DIRECTION ( 'NONE',  ( 0.000000000000000000, 0.000000000000000000, 1.000000000000000000 ) ) ;
#66790 = CARTESIAN_POINT ( 'NONE',  ( -0.01329177500952799865, 1508.926402960789801, 179.5289494733509912 ) ) ;
#66791 = CARTESIAN_POINT ( 'NONE',  ( -22.04658049762760896, 1524.075132568162417, 233.7649773472511470 ) ) ;
#66792 = CARTESIAN_POINT ( 'NONE',  ( 0.01306000193830150063, 1516.939762005280045, 213.7404293621069939 ) ) ;
#66793 = CARTESIAN_POINT ( 'NONE',  ( 2.898099067781010341, 1515.492902831140100, 213.2585957832889960 ) ) ;
#66794 = CARTESIAN_POINT ( 'NONE',  ( -31.81407709660785699, 1501.977400791986611, 196.2902540610632229 ) ) ;
#66796 = ORIENTED_EDGE ( 'NONE', *, *, #79151, .T. ) ;
#66795 = CARTESIAN_POINT ( 'NONE',  ( -11.77310042539119905, 1501.438875975280098, 211.3558264699879885 ) ) ;
#66797 = CARTESIAN_POINT ( 'NONE',  ( -8.156761245049999332, 1384.910749514120198, 199.6468897218990151 ) ) ;
#66798 = CARTESIAN_POINT ( 'NONE',  ( -0.9646231412680019712, 1508.481254761890114, 220.5684046465989923 ) ) ;
#66799 = CARTESIAN_POINT ( 'NONE',  ( -11.76893999620000031, 1432.294269540009964, 150.8119674620979822 ) ) ;
#66800 = CARTESIAN_POINT ( 'NONE',  ( -2.916739703929999816, 1436.466740336890098, 227.4199358109989930 ) ) ;
#66801 = CARTESIAN_POINT ( 'NONE',  ( -5.823377452736959725, 1441.464471037789963, 202.2443272568390000 ) ) ;
#66802 = CARTESIAN_POINT ( 'NONE',  ( 11.81421920076309995, 1428.091863512399868, 150.2203696085690012 ) ) ;
#66803 = CARTESIAN_POINT ( 'NONE',  ( 20.93524908849999733, 1496.483007425989854, 206.0866933769390243 ) ) ;
#66804 = CARTESIAN_POINT ( 'NONE',  ( -2.446787376320000096, 1432.353341358199941, 150.2884730787980061 ) ) ;
#66806 = CARTESIAN_POINT ( 'NONE',  ( -10.25236302078530137, 1481.942182559430194, 205.9183910829460160 ) ) ;
#66805 = CARTESIAN_POINT ( 'NONE',  ( -25.53892276620000246, 1482.721804240530219, 213.6785391664080009 ) ) ;
#66807 = LINE ( 'NONE', #102561, #49652 ) ;
#66808 = ORIENTED_EDGE ( 'NONE', *, *, #17166, .F. ) ;
#66809 = CARTESIAN_POINT ( 'NONE',  ( -4.623788007495000407, 1516.947419719950176, 205.6726967363569827 ) ) ;
#66810 = CARTESIAN_POINT ( 'NONE',  ( 9.852114434889999828, 1407.017073787930030, 269.2595063332979635 ) ) ;
#66811 = CARTESIAN_POINT ( 'NONE',  ( 0.009290522623869999774, 1410.298660454629953, 185.0095042931980061 ) ) ;
#66812 = B_SPLINE_CURVE_WITH_KNOTS ( 'NONE', 3,
 ( #30793, #12335, #4510, #72277, #82852, #90138 ),
 .UNSPECIFIED., .F., .F.,
 ( 4, 2, 4 ),
 ( -1.285435071098408229E-05, 0.001079388306740762700, 0.002171630964192509169 ),
 .UNSPECIFIED. ) ;
#66813 = CARTESIAN_POINT ( 'NONE',  ( 14.45783227242900004, 1416.839692127189892, 196.8516148535319985 ) ) ;
#66814 = CARTESIAN_POINT ( 'NONE',  ( -0.2730513641314620266, 1508.977834863310136, 238.8681177356729961 ) ) ;
#66815 = CARTESIAN_POINT ( 'NONE',  ( 1.890874494093850000, 1454.654138192250002, 218.3350682022239937 ) ) ;
#66816 = CARTESIAN_POINT ( 'NONE',  ( 2.470168521978398868, 1512.187213306747481, 242.8787258963054683 ) ) ;
#66817 = CARTESIAN_POINT ( 'NONE',  ( 14.14095063499999938, 1460.769213631630237, 232.7918287509980075 ) ) ;
#66818 = CARTESIAN_POINT ( 'NONE',  ( -16.64004004550000104, 1417.307962343580130, 206.7231940078289938 ) ) ;
#66819 = CARTESIAN_POINT ( 'NONE',  ( -13.05435892270000053, 1444.863344029789914, 186.3556100537979887 ) ) ;
#66820 = CARTESIAN_POINT ( 'NONE',  ( 1.469498570049999842, 1450.684669992949921, 155.6080914330979965 ) ) ;
#66821 = DIRECTION ( 'NONE',  ( 0.9417419115949662300, -0.2378257470769920556, 0.2378257470769920556 ) ) ;
#66822 = CARTESIAN_POINT ( 'NONE',  ( 15.45910333959999861, 1409.623955960430067, 270.0849031534979758 ) ) ;
#66823 = CARTESIAN_POINT ( 'NONE',  ( 1.455936843708680151, 1499.898551737820071, 181.4280194235350052 ) ) ;
#66824 = FACE_OUTER_BOUND ( 'NONE', #91934, .T. ) ;
#66825 = CARTESIAN_POINT ( 'NONE',  ( 11.44337041098931884, 1425.811177062257002, 138.6327568690129510 ) ) ;
#66826 = CARTESIAN_POINT ( 'NONE',  ( 20.69714064973412349, 1525.848198008145346, 233.9618268462910180 ) ) ;
#66827 = CARTESIAN_POINT ( 'NONE',  ( -4.991700414389999452, 1475.854790790129982, 268.4734068006980579 ) ) ;
#66828 = DIRECTION ( 'NONE',  ( 5.204170427930416866E-14, 0.000000000000000000, 1.000000000000000000 ) ) ;
#66829 = CARTESIAN_POINT ( 'NONE',  ( -20.99782421929999643, 1509.712776153829964, 187.9222525847980023 ) ) ;
#66830 = CARTESIAN_POINT ( 'NONE',  ( 1.909775791882409202, 1526.107880201381477, 240.8769681478140399 ) ) ;
#66831 = CARTESIAN_POINT ( 'NONE',  ( -46.05768597449060309, 1384.759096880909965, 253.6622143525649733 ) ) ;
#66832 = CARTESIAN_POINT ( 'NONE',  ( -106.4480318723080075, 1391.913060387289988, 303.4929453003720141 ) ) ;
#66833 = CARTESIAN_POINT ( 'NONE',  ( 12.06130973522970073, 1415.890045859200200, 223.3762606109779938 ) ) ;
#66834 = CARTESIAN_POINT ( 'NONE',  ( -25.74355351751919940, 1470.054056054910006, 210.8602373093899871 ) ) ;
#66835 = CARTESIAN_POINT ( 'NONE',  ( 4.326992699989999913, 1515.158586642889986, 208.7649733894699864 ) ) ;
#66836 = CARTESIAN_POINT ( 'NONE',  ( -2.244413514002144616, 1507.820143033591194, 221.0491532391985743 ) ) ;
#66837 = CARTESIAN_POINT ( 'NONE',  ( -21.69939614430000319, 1409.835269271030029, 202.8599322941780088 ) ) ;
#66838 = CARTESIAN_POINT ( 'NONE',  ( -9.270207532385544624, 1381.215922526254872, 200.8810307281849532 ) ) ;
#66839 = CARTESIAN_POINT ( 'NONE',  ( -15.49863863286799948, 1421.635490484141883, 227.2930321168060175 ) ) ;
#66840 = CARTESIAN_POINT ( 'NONE',  ( -37.66082768700000116, 1421.358466341330086, 269.1862046009979395 ) ) ;
#66841 = ADVANCED_FACE ( 'NONE', ( #73708 ), #30575, .F. ) ;
#66842 = ORIENTED_EDGE ( 'NONE', *, *, #26404, .F. ) ;
#66843 = CARTESIAN_POINT ( 'NONE',  ( -3.460923246345533943, 1410.410939174867508, 232.3865415841924857 ) ) ;
#66844 = CARTESIAN_POINT ( 'NONE',  ( -19.22849213419559788, 1445.326212981899971, 199.8420603585589959 ) ) ;
#66845 = CARTESIAN_POINT ( 'NONE',  ( -7.465999380592456269, 1510.821818217233613, 215.2858853877662284 ) ) ;
#66846 = CARTESIAN_POINT ( 'NONE',  ( -8.229007828222330900, 1439.448142495530192, 228.6152152553840153 ) ) ;
#66848 = CARTESIAN_POINT ( 'NONE',  ( 13.89554995500000167, 1452.733480491630189, 223.3956528723979886 ) ) ;
#66847 = PLANE ( 'NONE',  #19243 ) ;
#66849 = CARTESIAN_POINT ( 'NONE',  ( 16.94364159994348284, 1525.231887713385731, 236.8652194622064826 ) ) ;
#66850 = CARTESIAN_POINT ( 'NONE',  ( -7.722579826676089887, 1517.051704428850144, 208.6871515679729896 ) ) ;
#66851 = CARTESIAN_POINT ( 'NONE',  ( 39.63966549301360232, 1448.134706967000056, 136.4410930580840215 ) ) ;
#66852 = AXIS2_PLACEMENT_3D ( 'NONE', #21384, #53386, #20847 ) ;
#66853 = CARTESIAN_POINT ( 'NONE',  ( -0.4331437097091430100, 1420.567764534569960, 183.4025247420120195 ) ) ;
#66854 = CARTESIAN_POINT ( 'NONE',  ( -0.7543882209519990889, 1516.727502608469877, 202.5709757879969857 ) ) ;
#66855 = DIRECTION ( 'NONE',  ( -0.7414773880254650340, -0.000000000000000000, -0.6709778558543747495 ) ) ;
#66856 = CARTESIAN_POINT ( 'NONE',  ( -13.22475641109999955, 1415.063410489829948, 220.7066272063979966 ) ) ;
#66857 = CARTESIAN_POINT ( 'NONE',  ( 15.26322408243500028, 1511.857118786289902, 196.9337341496670035 ) ) ;
#66858 = CARTESIAN_POINT ( 'NONE',  ( -20.86040077545140647, 1508.959081886482636, 190.3921826379178128 ) ) ;
#66859 = CARTESIAN_POINT ( 'NONE',  ( -3.771520285720249888, 1380.389610322579983, 209.1217750815700072 ) ) ;
#66860 = CARTESIAN_POINT ( 'NONE',  ( 20.49664126143500198, 1509.564783478530217, 230.0195525190269734 ) ) ;
#66861 = CIRCLE ( 'NONE', #59732, 2.000000000000003109 ) ;
#66863 = VERTEX_POINT ( 'NONE', #103266 ) ;
#66862 = CARTESIAN_POINT ( 'NONE',  ( -52.20072447709220143, 1379.700295299539903, 250.0227394179869691 ) ) ;
#66864 = ORIENTED_EDGE ( 'NONE', *, *, #3034, .F. ) ;
#66866 = EDGE_CURVE ( 'NONE', #89357, #10275, #88257, .T. ) ;
#66865 = CARTESIAN_POINT ( 'NONE',  ( 11.71402527498609913, 1434.165202139100074, 151.1281046944980062 ) ) ;
#66867 = CARTESIAN_POINT ( 'NONE',  ( -4.791785870520000046, 1396.080393236430155, 219.8298651381980164 ) ) ;
#66868 = ORIENTED_EDGE ( 'NONE', *, *, #805, .F. ) ;
#66869 = CARTESIAN_POINT ( 'NONE',  ( -105.2826783650000095, 1379.306804825290101, 305.8448452370589621 ) ) ;
#66870 = LINE ( 'NONE', #65208, #99347 ) ;
#66871 = DIRECTION ( 'NONE',  ( -0.8090169943749422332, 0.000000000000000000, 0.5877852522924802425 ) ) ;
#66873 = CARTESIAN_POINT ( 'NONE',  ( -14.22567049866490052, 1509.383945902550067, 183.2093469327639923 ) ) ;
#66872 = CARTESIAN_POINT ( 'NONE',  ( 0.4875494646660009646, 1444.157371980789776, 200.0448216578990071 ) ) ;
#66874 = CARTESIAN_POINT ( 'NONE',  ( 15.83539164919999997, 1468.698963289930134, 189.4138077346979969 ) ) ;
#66875 = CARTESIAN_POINT ( 'NONE',  ( -3.165749237226819890, 1462.941186258239895, 199.8678155363639917 ) ) ;
#66876 = DIRECTION ( 'NONE',  ( -0.03489949670258984948, -0.9993908270190926535, 0.000000000000000000 ) ) ;
#66877 = B_SPLINE_SURFACE_WITH_KNOTS ( 'NONE', 5, 5, ( 
 ( #86686, #9980, #44150, #78285, #79403, #85563, #8860, #20563, #54764, #72660, #28442, #81041, #4354, #90538, #105151, #55315, #55871, #97833, #30642, #73203, #96757, #20029, #39598, #106250, #64829, #79950, #47456, #39024, #63722, #62638, #54223, #80507, #88896 ),
 ( #13817, #29535, #21111, #72131, #3266, #45817, #28999, #88349, #11639, #3823, #37395, #71596, #98937, #105716, #63187, #81580, #21662, #12739, #97293, #12181, #107347, #46372, #89447, #4883, #37952, #82139, #106787, #46922, #38483, #30078, #64270, #98392, #89992 ),
 ( #22212, #56408, #13267, #48002, #5440, #67024, #14373, #49116, #40141, #84885, #92199, #65373, #7094, #100042, #23871, #31736, #101131, #41251, #8179, #50749, #74325, #33377, #93294, #92745, #109562, #91647, #49667, #99477, #48565, #6545, #40695, #24426, #82702 ),
 ( #59175, #23331, #58612, #5991, #83248, #108454, #73770, #15471, #22758, #75424, #57522, #58066, #65920, #16020, #32831, #107893, #31186, #14922, #67573, #16556, #50221, #84347, #74867, #83799, #56964, #109013, #32298, #66481, #7638, #100589, #41793, #91093, #75952 ),
 ( #110103, #101677, #24966, #27753, #70348, #35046, #110650, #69226, #42911, #43466, #34500, #33937, #1461, #35598, #68677, #103337, #93832, #10399, #9848, #18780, #60836, #61390, #95509, #78715, #78152, #86553, #19335, #77612, #102781, #96063, #42346, #9301, #52978 ),
 ( #61946, #76501, #26640, #103909, #94963, #2031, #44569, #68135, #102246, #87679, #923, #36163, #17105, #87110, #104460, #18231, #25526, #59715, #17665, #26075, #27207, #53535, #85433, #378, #51296, #52426, #69789, #8731, #77068, #60267, #94386, #51866, #44017 ),
 ( #86004, #19895, #64145, #38352, #29397, #105021, #56273, #89866, #54098, #12058, #98263, #79278, #98815, #89317, #45136, #80376, #88226, #12613, #46794, #4221, #72007, #37821, #105583, #13135, #47319, #63599, #107219, #37272, #72531, #62505, #97166, #11518, #22077 ),
 ( #29951, #63064, #96624, #45693, #106661, #2587, #10964, #70904, #81446, #30507, #46246, #28314, #21532, #79832, #64697, #4754, #3138, #71466, #28870, #38897, #36711, #20437, #3691, #54645, #73080, #88776, #106123, #20988, #55747, #97717, #55193, #80923, #47869 ),
 ( #5871, #67450, #101549, #41675, #82006, #5311, #57400, #6421, #99349, #15890, #66899, #58485, #48991, #56828, #82580, #23200, #91527, #108324, #39469, #49540, #40013, #74193, #57940, #13682, #66352, #100470, #75834, #90403, #40566, #41115, #83123, #50089, #92613 ),
 ( #73641, #74737, #90963, #31057, #23753, #92072, #15345, #24842, #101006, #84217, #14805, #7515, #107771, #109984, #108875, #32166, #83665, #65238, #22624, #14250, #48440, #31607, #65785, #99905, #6962, #33261, #75294, #109439, #32718, #24305, #77492, #42230, #104339 ),
 ( #60145, #17542, #43886, #84762, #1908, #27092, #51744, #36046, #792, #25395, #52854, #85878, #69670, #18656, #50630, #59044, #94265, #93166, #86982, #16436, #8059, #69108, #9720, #44448, #10271, #9181, #76378, #43344, #59587, #34921, #51180, #110527, #18110 ),
 ( #103209, #68005, #95392, #35477, #61276, #26515, #93703, #85310, #102650, #25950, #76939, #33811, #52306, #8605, #42780, #60713, #102116, #94834, #86430, #78592, #16981, #78030, #1338, #103792, #70233, #250, #34377, #68550, #72952, #28738, #64017, #2467, #80798 ),
 ( #4637, #4104, #106542, #62943, #29831, #19201, #47197, #97054, #20318, #105449, #36584, #79159, #62369, #53403, #87554, #3014, #45014, #70781, #21404, #61818, #104894, #38228, #55063, #46115, #10842, #27632, #98129, #28183, #54524, #72412, #95941, #38776, #106007 ),
 ( #96495, #80246, #19774, #55614, #88658, #89738, #13011, #81323, #3564, #53976, #88109, #20868, #11398, #37138, #45567, #79708, #37686, #71335, #71891, #11935, #29283, #63479, #89190, #97597, #12483, #46665, #107645, #66770, #15745, #15210, #32033, #14116, #82990 ),
 ( #73509, #39336, #83527, #75160, #65656, #30928, #99218, #39888, #74055, #48307, #21947, #66222, #22496, #56697, #74607, #30377, #6282, #40430, #92475, #107088, #57272, #57812, #99773, #32593, #109307, #98687, #56140, #41547, #108184, #100869, #81878, #49401, #40980 ),
 ( #6821, #24160, #31475, #58350, #90276, #49946, #23062, #91399, #14677, #5180, #47743, #65106, #13557, #90833, #82448, #5745, #48864, #84084, #64567, #108742, #7382, #23630, #100341, #91936, #10137, #43748, #7926, #76795, #52159, #33127, #52709, #43204, #109850 ),
 ( #17404, #42096, #69528, #68420, #86292, #77899, #1206, #94133, #61135, #101974, #68974, #16303, #51051, #76244, #86844, #51600, #67314, #9032, #25260, #25814, #33671, #103075, #77354, #75703, #101411, #110391, #35340, #95249, #94691, #656, #93573, #85733, #24703 ),
 ( #67863, #103648, #58900, #93032, #112, #50507, #26946, #84629, #59463, #34787, #26376, #18512, #16848, #102522, #85183, #60012, #8469, #34234, #42642, #60571, #17964, #9576, #36435, #106802, #95796, #13832, #62227, #70086, #4898, #70632, #104750, #13281, #78452 ),
 ( #31204, #44308, #30092, #107362, #38499, #82156, #48018, #35903, #104199, #91112, #46937, #5455, #19063, #98952, #90554, #4370, #1765, #27484, #19631, #28037, #30657, #56980, #87407, #2325, #39614, #72676, #39038, #53268, #73784, #107909, #64842, #61673, #81056 ),
 ( #10700, #44872, #22225, #73218, #64286, #79023, #96353, #65388, #53832, #98407, #56424, #87971, #22775, #47472, #12756, #21678, #55885, #81594, #99492, #90005, #75439, #41266, #109033, #84364, #93309, #91662, #109576, #76514, #65937, #6560, #58080, #84901, #8193 ),
 ( #40711, #32846, #83264, #41810, #92759, #59730, #102260, #14937, #42359, #33957, #33391, #50237, #32315, #101146, #6006, #100061, #92213, #15485, #7654, #23348, #7112, #82716, #16570, #74883, #67038, #110663, #74341, #49132, #24986, #68152, #75967, #16037, #49683 ),
 ( #25540, #14388, #40158, #108468, #83812, #24439, #57538, #50766, #101693, #48581, #58628, #66498, #100604, #110119, #67587, #23886, #59190, #31752, #69806, #103924, #79291, #93850, #44030, #44585, #86569, #19350, #61961, #85447, #8744, #28327, #94978, #53549, #68690 ),
 ( #61403, #70921, #70362, #96075, #18245, #87697, #42928, #2601, #52441, #9862, #60853, #102795, #34512, #17679, #77085, #393, #69243, #26092, #60281, #10977, #17121, #94401, #36178, #10416, #1479, #51883, #51310, #45150, #86019, #78166, #104475, #9318, #105037 ),
 ( #35610, #43483, #27222, #77626, #36726, #95525, #27769, #938, #35061, #18797, #103352, #26653, #87126, #52993, #78731, #2046, #73656, #80936, #54110, #106675, #88788, #12629, #20450, #89878, #29965, #107787, #39485, #63077, #22090, #82021, #81461, #98276, #80389 ),
 ( #54659, #28882, #105599, #56289, #88239, #62518, #63613, #96641, #90417, #19910, #11531, #72544, #13148, #47883, #13697, #55204, #45706, #89332, #97177, #97729, #12069, #79844, #21550, #55762, #46261, #46806, #3153, #30523, #64158, #38910, #4234, #4767, #73093 ),
 ( #47333, #37286, #21000, #3704, #5325, #107232, #37834, #71477, #72019, #64714, #106136, #29413, #38368, #98831, #50646, #66366, #14265, #50105, #82594, #84776, #109997, #99921, #108339, #74211, #101567, #22639, #76391, #32182, #31072, #24857, #65253, #90977, #41129 ),
 ( #41688, #93182, #92630, #109453, #100485, #57415, #8073, #42243, #16449, #56844, #99365, #108889, #57953, #40029, #67464, #7531, #33273, #23766, #31623, #23215, #74752, #92086, #49005, #48456, #101021, #91541, #14818, #32732, #5884, #6978, #75310, #65799, #83140 ),
 ( #15361, #6435, #66912, #84230, #15904, #40580, #49554, #83679, #24318, #58501, #75847, #59058, #87573, #86998, #78609, #809, #1925, #102129, #19219, #34935, #69121, #77506, #85325, #51194, #34391, #25409, #59601, #85894, #16994, #8620, #104355, #33830, #42796 ),
 ( #266, #103808, #52324, #35493, #69688, #103225, #26534, #95409, #93718, #53422, #36062, #60731, #10860, #86448, #76956, #27651, #94852, #10287, #70248, #61837, #18127, #95957, #25964, #27107, #68567, #9199, #102665, #45033, #9738, #43904, #44464, #78045, #110542 ),
 ( #1354, #61292, #18674, #68021, #60160, #94281, #17558, #51760, #52870, #43361, #53994, #21423, #13027, #37707, #36602, #104912, #54542, #105469, #64034, #90294, #11416, #37160, #47214, #71908, #38246, #19792, #81341, #38794, #98148, #2485, #3583, #88127, #80815 ),
 ( #55633, #106561, #97615, #62388, #13574, #4654, #45585, #80266, #89756, #70800, #56158, #46683, #28201, #106024, #79726, #4121, #72429, #29848, #29299, #63497, #62960, #72969, #107106, #3033, #20885, #30396, #71354, #28756, #11953, #64586, #98705, #21964, #20337 ),
 ( #79178, #96513, #97071, #88675, #46137, #55083, #89208, #12504, #66787, #99238, #67335, #15765, #5764, #14137, #90850, #7402, #39355, #93052, #48883, #47760, #41567, #81895, #107663, #57829, #109327, #33147, #75723, #40448, #5200, #74625, #48327, #83010, #39906 ),
 ( #40998, #74076, #108760, #22513, #49965, #15230, #24182, #66241, #100887, #58370, #84103, #83546, #91955, #24723, #6302, #108205, #101433, #73529, #30949, #65125, #32051, #109868, #56716, #92496, #58920, #100360, #82466, #31493, #23083, #65674, #32611, #99792, #57292 ) ),
 .UNSPECIFIED., .F., .F., .F.,
 ( 6, 3, 3, 3, 3, 3, 3, 3, 3, 3, 6 ),
 ( 6, 3, 3, 3, 3, 3, 3, 3, 3, 3, 6 ),
 ( 0.000000000000000000, 1.936717162300000128, 3.873434324599999812, 4.841792905749999321, 5.810151486899999718, 7.746868649199999624, 9.683585811500000418, 10.65194439270000082, 11.62030297379999944, 13.55702013610000023, 15.49373729840000102 ),
 ( 0.000000000000000000, 1.936717162300000128, 3.873434324599999812, 4.841792905749999321, 5.810151486899999718, 7.746868649199999624, 9.683585811500000418, 10.65194439270000082, 11.62030297379999944, 13.55702013610000023, 15.49373729840000102 ),
 .UNSPECIFIED. ) ;
#66878 = CARTESIAN_POINT ( 'NONE',  ( 2.564080272660000048, 1443.257105148589972, 214.7475389528890162 ) ) ;
#66879 = CARTESIAN_POINT ( 'NONE',  ( 1.064544241010000114, 1415.263254644529979, 191.1462797974980106 ) ) ;
#66880 = CARTESIAN_POINT ( 'NONE',  ( 10.96948772520000048, 1432.349142915770017, 151.7703043505979963 ) ) ;
#66881 = CARTESIAN_POINT ( 'NONE',  ( 5.450092238964659330, 1509.109689566522320, 180.1788934176617261 ) ) ;
#66882 = ORIENTED_EDGE ( 'NONE', *, *, #83756, .T. ) ;
#66883 = CARTESIAN_POINT ( 'NONE',  ( 13.30485551143830136, 1434.923289955479959, 149.2654130802310135 ) ) ;
#66884 = VECTOR ( 'NONE', #49798, 1000.000000000000114 ) ;
#66885 = VERTEX_POINT ( 'NONE', #84818 ) ;
#66886 = VERTEX_POINT ( 'NONE', #59653 ) ;
#66887 = CARTESIAN_POINT ( 'NONE',  ( -19.00201092185649898, 1497.942407030830054, 229.3262107436430028 ) ) ;
#66888 = CARTESIAN_POINT ( 'NONE',  ( -4.015348745509998984, 1465.563087846730014, 234.9746089298979825 ) ) ;
#66889 = CARTESIAN_POINT ( 'NONE',  ( -108.0818973204794418, 1388.984710564502166, 310.0551414095012319 ) ) ;
#66890 = CARTESIAN_POINT ( 'NONE',  ( -1.708747662384999977, 1517.213554313520035, 216.0740123525270064 ) ) ;
#66891 = CARTESIAN_POINT ( 'NONE',  ( -19.50318791720000178, 1467.690391532990134, 205.2505305201189856 ) ) ;
#66892 = ADVANCED_FACE ( 'NONE', ( #93231 ), #68610, .F. ) ;
#66893 = ORIENTED_EDGE ( 'NONE', *, *, #107778, .T. ) ;
#66894 = CARTESIAN_POINT ( 'NONE',  ( -12.57798105409999856, 1503.242005039890046, 208.6149048402859876 ) ) ;
#66895 = DIRECTION ( 'NONE',  ( 0.000000000000000000, 0.000000000000000000, -1.000000000000000000 ) ) ;
#66896 = CARTESIAN_POINT ( 'NONE',  ( -7.567621161430000853, 1375.366160259910203, 208.3364483328870165 ) ) ;
#66897 = ADVANCED_FACE ( 'NONE', ( #86488 ), #51801, .T. ) ;
#66898 = EDGE_LOOP ( 'NONE', ( #107973, #109165, #18536, #5058 ) ) ;
#66899 = CARTESIAN_POINT ( 'NONE',  ( 2.865911516645000212, 1516.906233342200039, 205.6598507734169914 ) ) ;
#66900 = VERTEX_POINT ( 'NONE', #77552 ) ;
#66901 = CARTESIAN_POINT ( 'NONE',  ( -3.455495871984999745, 1516.939877939420057, 209.1351200182310208 ) ) ;
#66902 = CARTESIAN_POINT ( 'NONE',  ( -21.01954463430000430, 1509.698214774029793, 230.2158738807979717 ) ) ;
#66903 = CARTESIAN_POINT ( 'NONE',  ( -11.54610603179999906, 1410.690116826029907, 189.0374836358980133 ) ) ;
#66904 = CARTESIAN_POINT ( 'NONE',  ( -32.37018134260392088, 1511.187213306747708, 218.0712926453366833 ) ) ;
#66906 = VERTEX_POINT ( 'NONE', #77003 ) ;
#66905 = CARTESIAN_POINT ( 'NONE',  ( -0.02268235318324710037, 1415.088136167450102, 226.1092841930270083 ) ) ;
#66907 = CARTESIAN_POINT ( 'NONE',  ( 19.90855454129999913, 1426.369513873829874, 221.4890869410980088 ) ) ;
#66908 = CARTESIAN_POINT ( 'NONE',  ( 4.363122647530000009, 1419.257904667329967, 165.6263425522979844 ) ) ;
#66909 = CARTESIAN_POINT ( 'NONE',  ( -67.18675499840000498, 1383.787653363379832, 292.0788269227589922 ) ) ;
#66910 = FACE_OUTER_BOUND ( 'NONE', #37533, .T. ) ;
#66911 = CARTESIAN_POINT ( 'NONE',  ( 5.260635151189210212, 1409.438182731229972, 270.3705377465669812 ) ) ;
#66912 = CARTESIAN_POINT ( 'NONE',  ( 6.946748518954999341, 1516.983995446890049, 214.1250666973070054 ) ) ;
#66913 = CARTESIAN_POINT ( 'NONE',  ( 24.13962150589999922, 1410.980605758129968, 209.1808452922209938 ) ) ;
#66914 = DIRECTION ( 'NONE',  ( -1.755985294532469921E-16, 1.000000000000000000, -1.338183447452831989E-16 ) ) ;
#66915 = CARTESIAN_POINT ( 'NONE',  ( 2.032300221149999864, 1441.827160225690022, 218.8459470114090379 ) ) ;
#66916 = CARTESIAN_POINT ( 'NONE',  ( 6.551871745751780551, 1508.551566289579796, 216.0836877189279903 ) ) ;
#66917 = CARTESIAN_POINT ( 'NONE',  ( -3.447128498755000159, 1516.778853242349896, 210.2570310142770040 ) ) ;
#66918 = CARTESIAN_POINT ( 'NONE',  ( 13.66603629819999810, 1410.384381565130070, 271.1218459616979999 ) ) ;
#66919 = CARTESIAN_POINT ( 'NONE',  ( 17.83486663330486621, 1523.678648413191695, 180.3677388339000061 ) ) ;
#66920 = CARTESIAN_POINT ( 'NONE',  ( 3.912681475688819521, 1422.009998005289162, 137.0999999980402038 ) ) ;
#66922 = EDGE_LOOP ( 'NONE', ( #26477, #107646, #56873, #66081 ) ) ;
#66921 = CARTESIAN_POINT ( 'NONE',  ( -55.46135264680000176, 1389.548669515830170, 241.4579668749589985 ) ) ;
#66923 = CARTESIAN_POINT ( 'NONE',  ( -49.22592528755399854, 1385.126725678709818, 260.1312381994819702 ) ) ;
#66924 = CARTESIAN_POINT ( 'NONE',  ( 43.50124903029999501, 1440.913060358479925, 263.8967010685980199 ) ) ;
#66925 = DIRECTION ( 'NONE',  ( 0.000000000000000000, 0.000000000000000000, 1.000000000000000000 ) ) ;
#66926 = CARTESIAN_POINT ( 'NONE',  ( -14.49383181622579997, 1422.099016211560183, 229.4564907068830166 ) ) ;
#66927 = CARTESIAN_POINT ( 'NONE',  ( 9.058637367069879431, 1472.814398557088680, 216.2138489941888508 ) ) ;
#66928 = CARTESIAN_POINT ( 'NONE',  ( -15.96075179420000367, 1466.903945902690111, 196.1521398069990312 ) ) ;
#66929 = CARTESIAN_POINT ( 'NONE',  ( 1.530052826864370052, 1452.704406626560058, 183.4894965714629791 ) ) ;
#66930 = AXIS2_PLACEMENT_3D ( 'NONE', #21946, #14115, #27214 ) ;
#66931 = B_SPLINE_CURVE_WITH_KNOTS ( 'NONE', 3,
 ( #18158, #102699, #25993, #103835, #87029, #10319, #78637, #1953, #51223, #103254, #36090, #27683, #102161, #25443, #59637, #85927, #42828, #60191, #94310, #15736, #91926, #6812 ),
 .UNSPECIFIED., .F., .F.,
 ( 4, 2, 1, 1, 2, 2, 2, 2, 1, 1, 2, 2, 4 ),
 ( 0.000000000000000000, 0.1250000000002231271, 0.1875000000003487211, 0.2187500000003965162, 0.2343750000004201361, 0.2500000000004437561, 0.5000000000003356204, 0.6250000000002815526, 0.6875000000002354783, 0.7187500000001927347, 0.7343750000001930678, 0.7500000000001934009, 1.000000000000000000 ),
 .UNSPECIFIED. ) ;
#66933 = CARTESIAN_POINT ( 'NONE',  ( 0.3255681544566436103, 1492.051704408390151, 210.0673645372983174 ) ) ;
#66932 = LINE ( 'NONE', #50662, #98325 ) ;
#66934 = CARTESIAN_POINT ( 'NONE',  ( -9.544534124909469952, 1448.313337447510094, 209.6434600324809878 ) ) ;
#66935 = CARTESIAN_POINT ( 'NONE',  ( 30.80549360313091967, 1524.130440953581001, 221.8448932001212484 ) ) ;
#66936 = ORIENTED_EDGE ( 'NONE', *, *, #33674, .T. ) ;
#66937 = CARTESIAN_POINT ( 'NONE',  ( -7.331183129075000693, 1516.882217593000178, 202.1801186797769674 ) ) ;
#66938 = CARTESIAN_POINT ( 'NONE',  ( 1.600048698852036821, 1402.754281879943164, 137.0999999980979851 ) ) ;
#66939 = VECTOR ( 'NONE', #95185, 1000.000000000000000 ) ;
#66940 = CARTESIAN_POINT ( 'NONE',  ( 22.10609025900000191, 1451.545546232430070, 221.1255554720980001 ) ) ;
#66941 = CARTESIAN_POINT ( 'NONE',  ( 10.95069398041579944, 1461.279514859859773, 209.5869465053850149 ) ) ;
#66942 = CARTESIAN_POINT ( 'NONE',  ( 2.372478608332516892, 1501.977400791986611, 174.8996806668726549 ) ) ;
#66943 = CARTESIAN_POINT ( 'NONE',  ( -1.003913049989999973, 1443.013031698689929, 219.0745052372589896 ) ) ;
#66944 = CARTESIAN_POINT ( 'NONE',  ( 14.56058096671784696, 1420.278162403178612, 228.1987085794017389 ) ) ;
#66945 = CARTESIAN_POINT ( 'NONE',  ( 30.84777211902780181, 1435.574755141710057, 135.1614299696309729 ) ) ;
#66946 = CARTESIAN_POINT ( 'NONE',  ( 38.06107368031250360, 1448.769205308820119, 136.3873687041340190 ) ) ;
#66947 = CARTESIAN_POINT ( 'NONE',  ( 18.97170715521336959, 1506.426094403162324, 220.2326835074680105 ) ) ;
#66948 = CARTESIAN_POINT ( 'NONE',  ( -42.03398950740197648, 1454.231940949233831, 269.0747901792028642 ) ) ;
#66949 = CARTESIAN_POINT ( 'NONE',  ( -109.9057131499999969, 1385.910548283320168, 297.0533992618589991 ) ) ;
#66950 = CARTESIAN_POINT ( 'NONE',  ( 8.365518969610000966, 1508.201463035029974, 182.8802338420979936 ) ) ;
#66951 = B_SPLINE_CURVE_WITH_KNOTS ( 'NONE', 3,
 ( #36462, #80678, #11818, #37571 ),
 .UNSPECIFIED., .F., .F.,
 ( 4, 4 ),
 ( 0.000000000000000000, 0.0002960034161021618732 ),
 .UNSPECIFIED. ) ;
#66952 = CARTESIAN_POINT ( 'NONE',  ( 19.30300490008536229, 1526.348417187218274, 185.0858834514518492 ) ) ;
#66953 = DIRECTION ( 'NONE',  ( 0.000000000000000000, 1.000000000000000000, 0.000000000000000000 ) ) ;
#66954 = ORIENTED_EDGE ( 'NONE', *, *, #44527, .F. ) ;
#66955 = CARTESIAN_POINT ( 'NONE',  ( -8.697262469415090180, 1440.006290268419889, 206.1600271334220054 ) ) ;
#66956 = CARTESIAN_POINT ( 'NONE',  ( -32.91875957721972412, 1417.237689351310792, 269.2963688217181470 ) ) ;
#66957 = DIRECTION ( 'NONE',  ( 1.755985294532469921E-16, -1.000000000000000000, 1.338183447452831989E-16 ) ) ;
#66958 = CARTESIAN_POINT ( 'NONE',  ( 14.71671434821139890, 1437.593839606849997, 190.2862900904850108 ) ) ;
#66959 = CARTESIAN_POINT ( 'NONE',  ( -0.02064597189409999797, 1416.982031923930208, 234.1905971974979934 ) ) ;
#66960 = CARTESIAN_POINT ( 'NONE',  ( -12.96700364194406063, 1444.896546755032659, 186.2391592067185115 ) ) ;
#66961 = DIRECTION ( 'NONE',  ( 0.000000000000000000, 0.000000000000000000, 1.000000000000000000 ) ) ;
#66962 = CARTESIAN_POINT ( 'NONE',  ( -3.542321145578850139, 1515.375307573260216, 213.1422533703459976 ) ) ;
#66963 = CARTESIAN_POINT ( 'NONE',  ( 5.303300839834999891, 1513.301704408390151, 219.3748942783669804 ) ) ;
#66964 = CARTESIAN_POINT ( 'NONE',  ( -25.25200574389469921, 1450.804213008409988, 137.6134964715130025 ) ) ;
#66965 = CARTESIAN_POINT ( 'NONE',  ( 24.93753932649999783, 1435.554748705289967, 136.7196437487980063 ) ) ;
#66966 = CARTESIAN_POINT ( 'NONE',  ( -12.54032227232971941, 1442.774810664047664, 169.4746785633205377 ) ) ;
#66968 = ORIENTED_EDGE ( 'NONE', *, *, #65961, .T. ) ;
#66967 = CARTESIAN_POINT ( 'NONE',  ( -13.82592499520000118, 1409.562390380129955, 226.4595049929980064 ) ) ;
#66969 = CARTESIAN_POINT ( 'NONE',  ( 0.1558546717571289986, 1414.913057860449953, 192.7215652979920151 ) ) ;
#66970 = CARTESIAN_POINT ( 'NONE',  ( -1.331498055899999811, 1408.959557324029902, 231.4960598541979948 ) ) ;
#66971 = ORIENTED_EDGE ( 'NONE', *, *, #57100, .F. ) ;
#66972 = ORIENTED_EDGE ( 'NONE', *, *, #3817, .F. ) ;
#66973 = CARTESIAN_POINT ( 'NONE',  ( -11.61029367559999947, 1501.887990983090049, 208.8313354872300067 ) ) ;
#66974 = CARTESIAN_POINT ( 'NONE',  ( 12.71038950080000163, 1507.471771860230092, 233.3404623603979928 ) ) ;
#66976 = CARTESIAN_POINT ( 'NONE',  ( -8.693754259799998607, 1462.836994988729884, 231.7886756190980009 ) ) ;
#66975 = CARTESIAN_POINT ( 'NONE',  ( -11.71230443242549057, 1428.980197708463947, 142.1750151601944196 ) ) ;
#66977 = CARTESIAN_POINT ( 'NONE',  ( -3.129785590100000015, 1444.786455221890037, 217.7016765222190031 ) ) ;
#66978 = CARTESIAN_POINT ( 'NONE',  ( -11.87682048279999947, 1433.080538608139932, 149.9786578666980006 ) ) ;
#66979 = CARTESIAN_POINT ( 'NONE',  ( -12.30864129963430109, 1378.374850116299967, 209.8264313038230000 ) ) ;
#66980 = CARTESIAN_POINT ( 'NONE',  ( 13.92686551478569967, 1517.051704405520013, 192.0624604828410043 ) ) ;
#66981 = CARTESIAN_POINT ( 'NONE',  ( 7.616741216099999434, 1423.421902274779995, 213.1545376211790028 ) ) ;
#66982 = CARTESIAN_POINT ( 'NONE',  ( -24.11734200909999970, 1437.967381767040024, 211.4545393857079887 ) ) ;
#66983 = FACE_BOUND ( 'NONE', #50349, .T. ) ;
#66984 = CARTESIAN_POINT ( 'NONE',  ( 2.208852557009999718, 1450.292621906749901, 182.8591303368980050 ) ) ;
#66985 = CARTESIAN_POINT ( 'NONE',  ( 6.892224678239999847, 1361.632554499750086, 207.6218459616989946 ) ) ;
#66986 = CARTESIAN_POINT ( 'NONE',  ( -113.3410085367727334, 1390.913060387289988, 301.7225420527170172 ) ) ;
#66988 = ORIENTED_EDGE ( 'NONE', *, *, #19245, .F. ) ;
#66987 = CARTESIAN_POINT ( 'NONE',  ( -2.613846493977370076E-09, 1415.477284282600067, 242.7389708432399971 ) ) ;
#66989 = VERTEX_POINT ( 'NONE', #310 ) ;
#66990 = EDGE_CURVE ( 'NONE', #75001, #63161, #38307, .T. ) ;
#66991 = CARTESIAN_POINT ( 'NONE',  ( -11.85313930576219832, 1431.434453636790067, 149.9099107531910136 ) ) ;
#66992 = CARTESIAN_POINT ( 'NONE',  ( 13.52266831577220074, 1497.923527929759985, 227.8730120457710200 ) ) ;
#66993 = CARTESIAN_POINT ( 'NONE',  ( -5.319674814159999876, 1473.030992683929981, 270.4258975184980613 ) ) ;
#66994 = CARTESIAN_POINT ( 'NONE',  ( 0.2136372107412991272, 1473.445861986991986, 219.3446630527206480 ) ) ;
#66995 = CARTESIAN_POINT ( 'NONE',  ( -107.0031525618482107, 1366.350733876290633, 315.0056284496591275 ) ) ;
#66996 = CARTESIAN_POINT ( 'NONE',  ( 38.60868605548520094, 1450.040723184470153, 135.2652482427139944 ) ) ;
#66997 = CARTESIAN_POINT ( 'NONE',  ( 2.131986625866193030, 1526.000688113870183, 240.6925538244833831 ) ) ;
#66998 = CARTESIAN_POINT ( 'NONE',  ( -7.260870878720000476, 1480.575647549590030, 208.3277293783959863 ) ) ;
#66999 = ADVANCED_FACE ( 'NONE', ( #50687 ), #41732, .F. ) ;
#67000 = CARTESIAN_POINT ( 'NONE',  ( 12.78743207240877844, 1416.839570626248587, 223.0777679028553280 ) ) ;
#67001 = CARTESIAN_POINT ( 'NONE',  ( -17.20730882039999798, 1475.513060387329915, 197.3895399271980011 ) ) ;
#67002 = B_SPLINE_CURVE_WITH_KNOTS ( 'NONE', 3,
 ( #80686, #4534, #31368, #48752, #66112, #3997, #82332, #65551, #31920, #14007, #89624, #100236 ),
 .UNSPECIFIED., .F., .F.,
 ( 4, 2, 2, 2, 2, 4 ),
 ( 0.000000000000000000, 0.0007194225121803780225, 0.001079133768270252669, 0.001438845024360127425, 0.002158267536539321824, 0.002877690048718516656 ),
 .UNSPECIFIED. ) ;
#67003 = CARTESIAN_POINT ( 'NONE',  ( 11.06163309507687664, 1367.380938442054003, 208.3718459617010978 ) ) ;
#67004 = CARTESIAN_POINT ( 'NONE',  ( -8.912705131193250807, 1448.592310648610010, 211.1800892463350010 ) ) ;
#67005 = CARTESIAN_POINT ( 'NONE',  ( -20.31811729283709766, 1410.278425004400106, 269.5165023367199524 ) ) ;
#67006 = CARTESIAN_POINT ( 'NONE',  ( -13.03512055435489891, 1436.019541896100236, 150.7289522397179837 ) ) ;
#67007 = EDGE_LOOP ( 'NONE', ( #85559, #7403, #15420, #17799 ) ) ;
#67008 = CARTESIAN_POINT ( 'NONE',  ( -4.329415431089000066, 1515.066066275049934, 210.8307989536980074 ) ) ;
#67009 = B_SPLINE_SURFACE_WITH_KNOTS ( 'NONE', 5, 5, ( 
 ( #43921, #10309, #97090, #61856, #88694, #78068 ),
 ( #78628, #11975, #46156, #80286, #3602, #1371 ),
 ( #79196, #52889, #37725, #44482, #71929, #69706 ),
 ( #35513, #36081, #27671, #95976, #19237, #53446 ),
 ( #10880, #45052, #70821, #2502, #104933, #28220 ),
 ( #64606, #81917, #82486, #47783, #47234, #107127 ) ),
 .UNSPECIFIED., .F., .F., .F.,
 ( 6, 6 ),
 ( 6, 6 ),
 ( 30.40177460600000003, 157.7844419379999863 ),
 ( 0.000000000000000000, 1.000000000000000000 ),
 .UNSPECIFIED. ) ;
#67010 = VECTOR ( 'NONE', #44195, 1000.000000000000000 ) ;
#67011 = ORIENTED_EDGE ( 'NONE', *, *, #49019, .T. ) ;
#67012 = ORIENTED_EDGE ( 'NONE', *, *, #70047, .T. ) ;
#67013 = CARTESIAN_POINT ( 'NONE',  ( 4.998158967913196804, 1422.670539410961510, 184.4254624145364119 ) ) ;
#67014 = CARTESIAN_POINT ( 'NONE',  ( 8.586756624946868754, 1425.130607248830074, 194.8120923273959875 ) ) ;
#67015 = VECTOR ( 'NONE', #10852, 1000.000000000000000 ) ;
#67017 = DIRECTION ( 'NONE',  ( 1.755985294532464991E-16, -1.000000000000000000, 1.338183447452830017E-16 ) ) ;
#67016 = CARTESIAN_POINT ( 'NONE',  ( -4.028307778284999863, 1516.797038924770050, 212.3881954442970255 ) ) ;
#67018 = CARTESIAN_POINT ( 'NONE',  ( -17.60022530830000065, 1470.471392115730168, 189.3785151195980063 ) ) ;
#67019 = AXIS2_PLACEMENT_3D ( 'NONE', #87478, #2394, #14040 ) ;
#67020 = CARTESIAN_POINT ( 'NONE',  ( -18.18137326301040346, 1507.608478571330124, 229.7139312028679967 ) ) ;
#67021 = B_SPLINE_SURFACE_WITH_KNOTS ( 'NONE', 5, 5, ( 
 ( #47714, #5148, #107609, #6247, #40397, #74573, #32001, #66189, #100309, #23594, #95218, #24668, #102493, #17370, #50475, #71, #109816, #9545, #25227, #33095, #103615, #26913, #94658, #85150, #101939, #61101, #8436 ),
 ( #43715, #51015, #58867, #34202, #41513, #42609, #8997, #76762, #77866, #59981, #34753, #75672, #86812, #68941, #85701, #17929, #52127, #25783, #51568, #43169, #18479, #67828, #69493, #77323, #59430, #16273, #84599 ),
 ( #16815, #52676, #94099, #622, #93542, #92997, #103042, #26339, #1176, #60536, #68386, #86255, #35306, #67284, #101376, #7890, #42061, #76212, #110357, #33634, #88476, #45391, #12299, #28564, #3387, #44277, #55433 ),
 ( #63300, #97418, #71149, #96879, #11760, #97954, #36405, #38066, #20148, #70597, #95766, #19033, #11229, #62194, #2294, #45930, #72243, #71718, #80065, #20688, #44836, #36953, #78421, #61636, #105272, #53234, #29114 ),
 ( #54885, #3938, #104713, #54345, #21224, #62762, #89010, #63843, #35871, #79530, #46491, #80624, #96321, #37515, #105836, #106370, #29657, #28006, #10104, #19598, #87376, #1732, #70055, #104166, #27452, #10670, #78991 ),
 ( #53801, #87938, #2832, #82271, #64938, #108012, #13943, #100172, #108572, #4475, #22331, #39720, #40263, #81160, #13387, #30757, #57651, #14500, #56532, #90660, #6107, #91763, #47574, #106911, #48133, #21779, #48690 ) ),
 .UNSPECIFIED., .F., .F., .F.,
 ( 6, 6 ),
 ( 6, 3, 3, 3, 3, 3, 3, 3, 6 ),
 ( 2.214628081880000376, 99.53245534100000214 ),
 ( 27.66703433360000020, 34.17017220330000526, 36.60162405750000403, 37.81734998450000518, 38.42521294809999688, 39.03307591160000101, 39.44313445199999535, 39.85319299230000212, 40.67331007300000323 ),
 .UNSPECIFIED. ) ;
#67022 = ORIENTED_EDGE ( 'NONE', *, *, #97884, .F. ) ;
#67023 = DIRECTION ( 'NONE',  ( -1.755985294532469921E-16, 1.000000000000000000, -1.338183447452831989E-16 ) ) ;
#67024 = CARTESIAN_POINT ( 'NONE',  ( 5.003220727074999985, 1516.983995446890049, 202.1750974131470286 ) ) ;
#67025 = B_SPLINE_SURFACE_WITH_KNOTS ( 'NONE', 3, 5, ( 
 ( #19924, #54123, #105612, #80950, #21565, #90989 ),
 ( #108354, #23778, #89890, #99934, #73672, #109466 ),
 ( #40594, #14277, #65269, #47347, #57428, #81475 ),
 ( #13161, #99380, #48468, #30537, #39498, #98843 ) ),
 .UNSPECIFIED., .F., .F., .F.,
 ( 4, 4 ),
 ( 6, 6 ),
 ( 5.479561967899999608, 5.505632814020000154 ),
 ( 0.000000000000000000, 1.000000000000000000 ),
 .UNSPECIFIED. ) ;
#67026 = DIRECTION ( 'NONE',  ( 2.428612866367527723E-14, 0.000000000000000000, 1.000000000000000000 ) ) ;
#67027 = CARTESIAN_POINT ( 'NONE',  ( -47.05400443392269949, 1384.607290103919922, 220.9981132380000020 ) ) ;
#67028 = CARTESIAN_POINT ( 'NONE',  ( -2.807027225260000147, 1408.949922547829829, 194.9270130112979871 ) ) ;
#67029 = CARTESIAN_POINT ( 'NONE',  ( -17.83486663330527122, 1523.678648413191695, 180.3677388339002050 ) ) ;
#67031 = EDGE_LOOP ( 'NONE', ( #54919, #8236, #30970, #6804 ) ) ;
#67030 = CARTESIAN_POINT ( 'NONE',  ( 21.44521871417756032, 1525.343710797494850, 184.8098458366069394 ) ) ;
#67032 = CARTESIAN_POINT ( 'NONE',  ( 9.651063919191019025, 1425.440657924460083, 195.4941620015079877 ) ) ;
#67033 = CARTESIAN_POINT ( 'NONE',  ( 27.78146449860000189, 1508.131230137430066, 211.9290048573379863 ) ) ;
#67034 = CARTESIAN_POINT ( 'NONE',  ( -29.86461515634909603, 1525.960063244516959, 220.9690070206026178 ) ) ;
#67035 = DIRECTION ( 'NONE',  ( -0.7071067811865474617, -5.176495448588656087E-16, 0.7071067811865474617 ) ) ;
#67036 = CARTESIAN_POINT ( 'NONE',  ( -23.93699678040000123, 1435.351892431589931, 137.2158235772980106 ) ) ;
#67037 = CARTESIAN_POINT ( 'NONE',  ( -24.39131474979999936, 1441.263362519649945, 211.3484880528980057 ) ) ;
#67038 = CARTESIAN_POINT ( 'NONE',  ( -3.445407572115000150, 1516.764084769670262, 211.4198948937369948 ) ) ;
#67039 = CARTESIAN_POINT ( 'NONE',  ( -68.78035032010001260, 1379.747955697800080, 280.2621870389589844 ) ) ;
#67040 = CARTESIAN_POINT ( 'NONE',  ( -1.858959159852470178, 1484.242442314900018, 182.8691889360869993 ) ) ;
#67041 = CARTESIAN_POINT ( 'NONE',  ( 7.097314899640720043, 1439.093628026630086, 216.1530160518380228 ) ) ;
#67042 = CARTESIAN_POINT ( 'NONE',  ( -12.98226561589999939, 1414.913060387329779, 219.9156672276980089 ) ) ;
#67043 = AXIS2_PLACEMENT_3D ( 'NONE', #61632, #16812, #60532 ) ;
#67044 = CARTESIAN_POINT ( 'NONE',  ( -1.137296688934999800, 1516.908147884120126, 207.4199954749970232 ) ) ;
#67045 = ORIENTED_EDGE ( 'NONE', *, *, #62468, .F. ) ;
#67046 = CARTESIAN_POINT ( 'NONE',  ( -2.639044490659959941, 1451.958037943090176, 184.7018172437709893 ) ) ;
#67047 = CARTESIAN_POINT ( 'NONE',  ( -8.650219412924689877, 1438.157521317829833, 208.3097233004990017 ) ) ;
#67048 = CARTESIAN_POINT ( 'NONE',  ( -19.50204366554770274, 1457.206926615194106, 226.0571257576273183 ) ) ;
#67049 = VERTEX_POINT ( 'NONE', #54036 ) ;
#67050 = CARTESIAN_POINT ( 'NONE',  ( 19.64599270300000100, 1476.662575758389949, 214.0395835971089866 ) ) ;
#67051 = FACE_OUTER_BOUND ( 'NONE', #109408, .T. ) ;
#67052 = CARTESIAN_POINT ( 'NONE',  ( -4.107056636162540464, 1441.387641401842757, 184.3702559431454233 ) ) ;
#67053 = CIRCLE ( 'NONE', #50976, 1.999999999999999556 ) ;
#67054 = CARTESIAN_POINT ( 'NONE',  ( -14.92733988109999999, 1416.530231069960109, 207.6074944693189934 ) ) ;
#67055 = CARTESIAN_POINT ( 'NONE',  ( -10.98289517778636792, 1424.968082807670953, 138.3353964325996515 ) ) ;
#67056 = CARTESIAN_POINT ( 'NONE',  ( 6.223729794970000562, 1487.458568572190188, 200.0625369783790006 ) ) ;
#67057 = DIRECTION ( 'NONE',  ( -0.000000000000000000, -1.000000000000000000, -0.000000000000000000 ) ) ;
#67058 = CARTESIAN_POINT ( 'NONE',  ( 4.224932291032190257, 1441.576670139289718, 166.5005718325089958 ) ) ;
#67060 = CARTESIAN_POINT ( 'NONE',  ( -17.97880235851549457, 1445.573137004940918, 203.2555883697691286 ) ) ;
#67059 = CARTESIAN_POINT ( 'NONE',  ( -2.867803664234999772, 1516.994127245590107, 213.7465828294170080 ) ) ;
#67061 = CARTESIAN_POINT ( 'NONE',  ( 21.02506697189999940, 1509.639958400629894, 188.3976031865980190 ) ) ;
#67062 = CARTESIAN_POINT ( 'NONE',  ( 7.331183090945000203, 1516.882217593000178, 216.0635732225570109 ) ) ;
#67063 = ORIENTED_EDGE ( 'NONE', *, *, #76848, .F. ) ;
#67064 = CARTESIAN_POINT ( 'NONE',  ( -18.53418666356940037, 1507.620785846770104, 229.7143111648900060 ) ) ;
#67065 = CARTESIAN_POINT ( 'NONE',  ( -17.06299074029999829, 1420.289561323179896, 203.8301379063090337 ) ) ;
#67066 = CARTESIAN_POINT ( 'NONE',  ( 0.1469571361719999858, 1420.465545067329913, 183.3355639602979750 ) ) ;
#67067 = EDGE_CURVE ( 'NONE', #72816, #71731, #93587, .T. ) ;
#67068 =( BOUNDED_CURVE ( )  B_SPLINE_CURVE ( 3, ( #70430, #105104, #19982, #54176 ),
 .UNSPECIFIED., .F., .F. ) 
 B_SPLINE_CURVE_WITH_KNOTS ( ( 4, 4 ),
 ( 0.000000000000000000, 0.7048113239778082129 ),
 .UNSPECIFIED. ) 
 CURVE ( )  GEOMETRIC_REPRESENTATION_ITEM ( )  RATIONAL_B_SPLINE_CURVE ( ( 1.000000000000000000, 0.9590300661663089254, 0.9590300661663089254, 1.000000000000000000 ) ) 
 REPRESENTATION_ITEM ( '' )  );
#67069 = CARTESIAN_POINT ( 'NONE',  ( -0.1492209459390009818, 1474.475942019490049, 219.5409241924989772 ) ) ;
#67070 = CARTESIAN_POINT ( 'NONE',  ( 2.865545859819519148, 1525.651285554128663, 177.1364457139975173 ) ) ;
#67071 = UNCERTAINTY_MEASURE_WITH_UNIT (LENGTH_MEASURE( 1.000000000000000082E-05 ), #33917, 'distance_accuracy_value', 'NONE');
#67072 = CARTESIAN_POINT ( 'NONE',  ( -0.08180352518808278739, 1423.482083046089883, 191.1879846049409934 ) ) ;
#67073 = CARTESIAN_POINT ( 'NONE',  ( -11.38946577428759888, 1470.924613609000062, 208.4453646624949954 ) ) ;
#67074 = CARTESIAN_POINT ( 'NONE',  ( -5.309623260221089325, 1508.254033944475623, 220.3333518336809504 ) ) ;
#67075 = CARTESIAN_POINT ( 'NONE',  ( 17.38836599616480427, 1422.723741091718466, 226.5637347084151259 ) ) ;
#67076 = ADVANCED_FACE ( 'NONE', ( #79768 ), #56346, .T. ) ;
#67077 = CARTESIAN_POINT ( 'NONE',  ( 18.80339027203730140, 1425.953307585449693, 225.0197318394450008 ) ) ;
#67078 = CARTESIAN_POINT ( 'NONE',  ( -8.661115458674929329E-07, 1407.922920414400096, 222.3762974436029936 ) ) ;
#67080 = EDGE_CURVE ( 'NONE', #85866, #109412, #70844, .T. ) ;
#67079 = CARTESIAN_POINT ( 'NONE',  ( 42.85777160514339812, 1440.913060354170057, 263.0145395452340153 ) ) ;
#67082 = CARTESIAN_POINT ( 'NONE',  ( -0.8685429202199980159, 1491.841791262990000, 188.0762365942990186 ) ) ;
#67081 = CARTESIAN_POINT ( 'NONE',  ( -15.23238439385559850, 1418.498828849909842, 202.0312086372670137 ) ) ;
#67083 = CARTESIAN_POINT ( 'NONE',  ( 12.78671360849999772, 1416.817366564930126, 222.1376795749980033 ) ) ;
#67084 = VERTEX_POINT ( 'NONE', #96559 ) ;
#67085 = VERTEX_POINT ( 'NONE', #90896 ) ;
#67086 = DIRECTION ( 'NONE',  ( 0.000000000000000000, 0.000000000000000000, 1.000000000000000000 ) ) ;
#67087 = AXIS2_PLACEMENT_3D ( 'NONE', #37536, #61126, #95239 ) ;
#67088 = CARTESIAN_POINT ( 'NONE',  ( 2.902322711624676882E-15, 1523.409940573003951, 232.8211094035767985 ) ) ;
#67089 = CARTESIAN_POINT ( 'NONE',  ( -27.87492310950000274, 1509.195406832029903, 210.7637215495180101 ) ) ;
#67090 = DIRECTION ( 'NONE',  ( -6.162707975952100561E-15, -1.000000000000000000, -1.094450614310000083E-14 ) ) ;
#67091 = CARTESIAN_POINT ( 'NONE',  ( 740.1067240283520050, 11216.44053380570222, 2045.284428720447750 ) ) ;
#67092 = CARTESIAN_POINT ( 'NONE',  ( 27.56820608061211075, 1509.987796949902304, 220.9537938550800220 ) ) ;
#67093 = CARTESIAN_POINT ( 'NONE',  ( -5.473890262062679923, 1440.659206222230068, 154.7842680559549819 ) ) ;
#67094 = CARTESIAN_POINT ( 'NONE',  ( 19.37774363895821850, 1525.878013734320120, 181.3897518523426982 ) ) ;
#67095 = CARTESIAN_POINT ( 'NONE',  ( -73.43657703184560148, 1383.782119018540016, 298.3839446379640208 ) ) ;
#67096 = CARTESIAN_POINT ( 'NONE',  ( -9.604690719327259566E-16, 1522.051704408389924, 209.1218459616989946 ) ) ;
#67097 = LINE ( 'NONE', #92270, #1737 ) ;
#67098 = CARTESIAN_POINT ( 'NONE',  ( 11.42677157140140132, 1491.914064927579830, 210.1973818834709959 ) ) ;
#67100 = VERTEX_POINT ( 'NONE', #91999 ) ;
#67099 = CARTESIAN_POINT ( 'NONE',  ( 1.660746386170000033, 1456.055583820689890, 218.8271601458489783 ) ) ;
#67101 = DIRECTION ( 'NONE',  ( -1.000000000000000000, 0.000000000000000000, 0.000000000000000000 ) ) ;
#67102 = B_SPLINE_SURFACE_WITH_KNOTS ( 'NONE', 5, 4, ( 
 ( #58420, #16373, #16919, #69045, #34857 ),
 ( #60642, #26449, #7997, #34304, #50571 ),
 ( #41049, #8544, #109379, #42162, #32656 ),
 ( #110465, #33742, #17474, #102587, #59526 ),
 ( #42718, #100941, #92546, #15814, #68486 ),
 ( #25886, #50018, #41614, #104828, #63413 ),
 ( #43821, #71266, #97528, #18587, #103720 ),
 ( #28114, #20255, #27565, #78530, #88591 ),
 ( #19710, #53913, #80179, #35415, #53342 ) ),
 .UNSPECIFIED., .F., .F., .F.,
 ( 6, 3, 6 ),
 ( 5, 5 ),
 ( -1.776356839400000001E-15, 5.782490304330000441, 11.25975508159999983 ),
 ( 25.78146411700000229, 39.23969207129999859 ),
 .UNSPECIFIED. ) ;
#67103 = CARTESIAN_POINT ( 'NONE',  ( -73.04349225800000056, 1383.258802109350199, 272.3818029833590231 ) ) ;
#67104 = CARTESIAN_POINT ( 'NONE',  ( 8.506705275679738776, 1436.886745436839874, 207.6663867986219998 ) ) ;
#67105 = VERTEX_POINT ( 'NONE', #22555 ) ;
#67106 = ORIENTED_EDGE ( 'NONE', *, *, #94509, .F. ) ;
#67107 = CARTESIAN_POINT ( 'NONE',  ( -8.605913743462409116, 1385.346776729300018, 218.6535381029370058 ) ) ;
#67108 = CARTESIAN_POINT ( 'NONE',  ( -3.644352556202699933, 1515.551704204679936, 205.8496992207700202 ) ) ;
#67110 = CARTESIAN_POINT ( 'NONE',  ( -38.60856581307790236, 1443.613625294319945, 137.1750438966080026 ) ) ;
#67109 = CARTESIAN_POINT ( 'NONE',  ( 3.330134165755000097, 1515.051704408389924, 213.4516374609670208 ) ) ;
#67111 = CARTESIAN_POINT ( 'NONE',  ( -6.040927710290000086, 1463.272537550489915, 201.2370028249389975 ) ) ;
#67112 = CARTESIAN_POINT ( 'NONE',  ( -104.6820493169999935, 1380.404521281969892, 300.7508435114589815 ) ) ;
#67113 = CARTESIAN_POINT ( 'NONE',  ( 2.236830499889160162, 1495.676457076940096, 221.2569898194790028 ) ) ;
#67114 = CARTESIAN_POINT ( 'NONE',  ( 41.66021864449999867, 1443.875655612860101, 135.6929158170979974 ) ) ;
#67115 = CARTESIAN_POINT ( 'NONE',  ( -15.49290351828469881, 1508.551704408389924, 214.3946075353640026 ) ) ;
#67116 = CARTESIAN_POINT ( 'NONE',  ( 23.84533589473599946, 1452.080362908450070, 136.9869410992479857 ) ) ;
#67117 = CARTESIAN_POINT ( 'NONE',  ( 0.9336696193000000310, 1408.945664848729848, 186.1949048084980234 ) ) ;
#67118 = CARTESIAN_POINT ( 'NONE',  ( 3.256906394843720243, 1487.066025393580048, 197.6188337626330167 ) ) ;
#67119 = CARTESIAN_POINT ( 'NONE',  ( 49.24962907673570811, 1526.382868172863937, 10.34030387146701635 ) ) ;
#67120 = CARTESIAN_POINT ( 'NONE',  ( -3.134579720209279774, 1440.880072796180002, 159.2383936985540061 ) ) ;
#67121 = DIRECTION ( 'NONE',  ( -0.7384854939282339270, -4.299149317525499380E-13, 0.6742693640212139572 ) ) ;
#67122 = VERTEX_POINT ( 'NONE', #5240 ) ;
#67123 = AXIS2_PLACEMENT_3D ( 'NONE', #59777, #61446, #26699 ) ;
#67124 = CARTESIAN_POINT ( 'NONE',  ( -0.8167354255590000278, 1432.353341358199941, 150.3995506339979897 ) ) ;
#67125 = CARTESIAN_POINT ( 'NONE',  ( -9.736852438091474937, 1428.340212313232087, 134.0999999980979567 ) ) ;
#67126 = CARTESIAN_POINT ( 'NONE',  ( 14.91777843120000036, 1430.152623513529988, 190.7961912442980008 ) ) ;
#67127 = CARTESIAN_POINT ( 'NONE',  ( -8.598089374990029619E-11, 1469.758488426850136, 253.3729536691440387 ) ) ;
#67128 = CARTESIAN_POINT ( 'NONE',  ( -13.31089767776890120, 1503.456584347970193, 208.6977459380580058 ) ) ;
#67130 = ADVANCED_FACE ( 'NONE', ( #48366 ), #22325, .T. ) ;
#67129 = CARTESIAN_POINT ( 'NONE',  ( -1.547118986179999878, 1416.568813549730066, 228.0093688194979791 ) ) ;
#67131 = CARTESIAN_POINT ( 'NONE',  ( 2.115055685359999771, 1476.785742987490039, 198.5761133807990007 ) ) ;
#67132 = CARTESIAN_POINT ( 'NONE',  ( -104.5024257390000031, 1390.098467524800071, 305.3418556385589682 ) ) ;
#67133 = AXIS2_PLACEMENT_3D ( 'NONE', #79013, #61660, #28582 ) ;
#67134 = CARTESIAN_POINT ( 'NONE',  ( -8.654780631634018562, 1511.434547101049930, 214.5059332195740183 ) ) ;
#67135 = CARTESIAN_POINT ( 'NONE',  ( -10.31239467132616561, 1362.904424737038880, 207.6218459616987673 ) ) ;
#67136 = CARTESIAN_POINT ( 'NONE',  ( -46.27883891992610188, 1440.696393458320017, 267.5894411246799791 ) ) ;
#67137 = CARTESIAN_POINT ( 'NONE',  ( 0.8644693283286819518, 1429.652419925939967, 217.3904187270329942 ) ) ;
#67138 = CARTESIAN_POINT ( 'NONE',  ( -8.477967594009999885, 1424.852341466620146, 205.3179503978689979 ) ) ;
#67139 = CARTESIAN_POINT ( 'NONE',  ( 4.618583391875000110, 1516.939762005280045, 209.1087859301640322 ) ) ;
#67140 = CARTESIAN_POINT ( 'NONE',  ( -2.478627793510000288, 1436.625092229730171, 157.6517990276980186 ) ) ;
#67141 = B_SPLINE_SURFACE_WITH_KNOTS ( 'NONE', 5, 5, ( 
 ( #61544, #53708, #44742, #78892, #2198, #2747 ),
 ( #62668, #96789, #20059, #32332, #106815, #14951 ),
 ( #83278, #13294, #6576, #108484, #64857, #97862 ),
 ( #55344, #21137, #89478, #98966, #12773, #22240 ),
 ( #49146, #22791, #81070, #91126, #40725, #90017 ),
 ( #99508, #107927, #73798, #74356, #39053, #90569 ),
 ( #31767, #6021, #82730, #39630, #65954, #31220 ),
 ( #65402, #47487, #72692, #56996, #4385, #64301 ),
 ( #14403, #74898, #48596, #13847, #48032, #100078 ) ),
 .UNSPECIFIED., .F., .F., .F.,
 ( 6, 3, 6 ),
 ( 6, 6 ),
 ( 0.7655572723400000390, 2.316155491850000026, 3.835724788489999870 ),
 ( 0.000000000000000000, 1.000000000000000000 ),
 .UNSPECIFIED. ) ;
#67142 = CARTESIAN_POINT ( 'NONE',  ( 4.329448776040000446, 1515.064792882589927, 206.7917118356089929 ) ) ;
#67143 = CARTESIAN_POINT ( 'NONE',  ( 7.405955376734920215, 1426.244457028639999, 212.5578732180090071 ) ) ;
#67144 = CARTESIAN_POINT ( 'NONE',  ( -26.62605130868620051, 1450.898279949580001, 136.4493292573559984 ) ) ;
#67145 = EDGE_LOOP ( 'NONE', ( #32572, #70074 ) ) ;
#67146 = CARTESIAN_POINT ( 'NONE',  ( -3.034064455719999779E-09, 1416.682256071730080, 238.2947578363979915 ) ) ;
#67148 = CARTESIAN_POINT ( 'NONE',  ( -14.76103606440959837, 1512.125809830880144, 221.3468319615099915 ) ) ;
#67147 = CARTESIAN_POINT ( 'NONE',  ( -11.21869170107060043, 1491.835551150570154, 206.9930840995259871 ) ) ;
#67149 = CARTESIAN_POINT ( 'NONE',  ( -1.748905610829809998, 1488.269106374019884, 219.8524659745219765 ) ) ;
#67150 = CARTESIAN_POINT ( 'NONE',  ( -8.652776130911478347, 1511.435001053830092, 214.5073691320910143 ) ) ;
#67151 = CARTESIAN_POINT ( 'NONE',  ( -1.640992637469999904, 1486.309234237589862, 220.9425018421990217 ) ) ;
#67152 = CARTESIAN_POINT ( 'NONE',  ( 0.4666204826262328464, 1415.437692837088889, 233.3904393389156269 ) ) ;
#67153 = CARTESIAN_POINT ( 'NONE',  ( 20.59684415639999955, 1507.762623716630060, 209.5602205471840023 ) ) ;
#67154 = EDGE_LOOP ( 'NONE', ( #8772, #47864, #45554, #6956 ) ) ;
#67155 = CARTESIAN_POINT ( 'NONE',  ( 14.27715652531434820, 1416.818673809773600, 196.5253453210812609 ) ) ;
#67156 = DIRECTION ( 'NONE',  ( 0.000000000000000000, 1.000000000000000000, -1.836970198721029688E-16 ) ) ;
#67157 = CARTESIAN_POINT ( 'NONE',  ( 9.728472712500000341, 1463.031710894390017, 210.0816964760090002 ) ) ;
#67158 = EDGE_LOOP ( 'NONE', ( #15743, #20586, #108010, #59723 ) ) ;
#67159 = ORIENTED_EDGE ( 'NONE', *, *, #69252, .T. ) ;
#67160 = CARTESIAN_POINT ( 'NONE',  ( -53.47364387789999540, 1384.899415174140131, 230.7470315883589933 ) ) ;
#67161 = CARTESIAN_POINT ( 'NONE',  ( -22.97501113406280382, 1409.745379998360249, 209.4185639539470003 ) ) ;
#67162 = EDGE_CURVE ( 'NONE', #62788, #66505, #15273, .T. ) ;
#67163 = VERTEX_POINT ( 'NONE', #39396 ) ;
#67164 = CARTESIAN_POINT ( 'NONE',  ( -104.0419184278400024, 1314.643966242390206, 309.3341892202889767 ) ) ;
#67165 = CARTESIAN_POINT ( 'NONE',  ( 3.160865718646527434, 1370.358796302880364, 211.5724212009420739 ) ) ;
#67166 = CARTESIAN_POINT ( 'NONE',  ( -12.32958673350000112, 1507.632494499530139, 233.3296017327979825 ) ) ;
#67167 = FACE_OUTER_BOUND ( 'NONE', #88532, .T. ) ;
#67168 = CARTESIAN_POINT ( 'NONE',  ( 46.11011654448370223, 1442.803748059199961, 268.2059351147869961 ) ) ;
#67169 = CIRCLE ( 'NONE', #18852, 1.000000000000000888 ) ;
#67170 = CARTESIAN_POINT ( 'NONE',  ( -1.462741316680280068, 1424.166085031260081, 228.3696464465570273 ) ) ;
#67171 = CARTESIAN_POINT ( 'NONE',  ( -17.05655558861789345, 1422.119710870798144, 226.7808225676212430 ) ) ;
#67172 = CARTESIAN_POINT ( 'NONE',  ( 3.448206878685000198, 1516.904492006980036, 205.0794281543969646 ) ) ;
#67173 = ORIENTED_EDGE ( 'NONE', *, *, #43218, .T. ) ;
#67174 = CARTESIAN_POINT ( 'NONE',  ( 18.36669116892507958, 1459.044192910584343, 227.7581707921801524 ) ) ;
#67175 = CARTESIAN_POINT ( 'NONE',  ( 14.90569722004390130, 1513.941944658620059, 194.3080451509249826 ) ) ;
#67176 = DIRECTION ( 'NONE',  ( -0.000000000000000000, -1.000000000000000000, -0.000000000000000000 ) ) ;
#67177 = ORIENTED_EDGE ( 'NONE', *, *, #37186, .T. ) ;
#67178 = CARTESIAN_POINT ( 'NONE',  ( 2.994866067409999832, 1448.618510723430063, 183.8359025843979850 ) ) ;
#67179 = CARTESIAN_POINT ( 'NONE',  ( 26.71026096653610082, 1451.513660524960187, 136.0795779202579752 ) ) ;
#67180 = CARTESIAN_POINT ( 'NONE',  ( -4.984765438550020633, 1508.551704408389924, 211.7339477409330186 ) ) ;
#67181 = CARTESIAN_POINT ( 'NONE',  ( 0.8647627281377370245, 1452.882862207440212, 152.5191013288349779 ) ) ;
#67182 = CARTESIAN_POINT ( 'NONE',  ( 7.477592609290000247, 1422.768710552009907, 195.6698503542990011 ) ) ;
#67183 = CARTESIAN_POINT ( 'NONE',  ( -1.447235060822049890, 1432.423094547480105, 218.5251106399929881 ) ) ;
#67184 = CARTESIAN_POINT ( 'NONE',  ( 10.70780782887229954, 1479.022113073340051, 205.9701340518660118 ) ) ;
#67185 = CARTESIAN_POINT ( 'NONE',  ( 2.038497153056070044, 1408.984246276509793, 186.9383856488950073 ) ) ;
#67187 = PLANE ( 'NONE',  #45802 ) ;
#67186 = CARTESIAN_POINT ( 'NONE',  ( 1.324323477659999915, 1416.409446159829940, 233.0341864379980166 ) ) ;
#67188 = CARTESIAN_POINT ( 'NONE',  ( 11.50132634430500111, 1426.392275987999938, 206.5139615940070144 ) ) ;
#67189 = CARTESIAN_POINT ( 'NONE',  ( -11.99239960049999887, 1380.797795605900092, 215.7904316102089979 ) ) ;
#67190 = ADVANCED_FACE ( 'NONE', ( #98745 ), #9100, .F. ) ;
#67191 = DIRECTION ( 'NONE',  ( 0.3282391760791589785, -0.000000000000000000, 0.9445946449598763284 ) ) ;
#67192 = ORIENTED_EDGE ( 'NONE', *, *, #33566, .T. ) ;
#67193 = CARTESIAN_POINT ( 'NONE',  ( 12.78353013627689982, 1416.221314539589912, 221.8283297262470057 ) ) ;
#67194 = CARTESIAN_POINT ( 'NONE',  ( -4.500000000000000000, 1411.429641636930000, 127.2892455880980123 ) ) ;
#67195 = CARTESIAN_POINT ( 'NONE',  ( 31.10384971727509651, 1525.795403621570813, 201.8948720197292630 ) ) ;
#67197 = EDGE_CURVE ( 'NONE', #95247, #10483, #31562, .T. ) ;
#67196 = VECTOR ( 'NONE', #11881, 1000.000000000000000 ) ;
#67198 = CARTESIAN_POINT ( 'NONE',  ( -10.84052017329999806, 1388.346876310129801, 201.9571177318990181 ) ) ;
#67199 = CARTESIAN_POINT ( 'NONE',  ( 11.19200130296239948, 1422.145316461549783, 210.4507779064919930 ) ) ;
#67200 = CARTESIAN_POINT ( 'NONE',  ( 10.96812435474240033, 1424.188686434009924, 203.1558521378470061 ) ) ;
#67201 = EDGE_CURVE ( 'NONE', #101260, #97990, #79830, .T. ) ;
#67202 = CARTESIAN_POINT ( 'NONE',  ( 0.7162966257659990621, 1429.709262178790141, 217.4063658874189855 ) ) ;
#67203 = CARTESIAN_POINT ( 'NONE',  ( 6.661338147749999709E-15, 1470.874276671130019, 268.3665355202980436 ) ) ;
#67204 = CARTESIAN_POINT ( 'NONE',  ( -21.46027262497062793, 1509.101876609105830, 191.8002388787112693 ) ) ;
#67205 = EDGE_CURVE ( 'NONE', #81708, #26498, #30163, .T. ) ;
#67206 = CARTESIAN_POINT ( 'NONE',  ( 11.16482994470000101, 1433.388395248510051, 151.6286288133979951 ) ) ;
#67207 = CARTESIAN_POINT ( 'NONE',  ( 6.092217245739999676, 1469.463552837929910, 265.6112250856980381 ) ) ;
#67209 = EDGE_CURVE ( 'NONE', #34958, #108026, #109908, .T. ) ;
#67208 = CARTESIAN_POINT ( 'NONE',  ( 11.70695556603179988, 1414.913057860449953, 197.6353021862890103 ) ) ;
#67210 = TOROIDAL_SURFACE ( 'NONE', #11725, 2.000000000000000000, 1.000000000000000000 ) ;
#67211 =( BOUNDED_SURFACE ( )  B_SPLINE_SURFACE ( 3, 2, ( 
 ( #75430, #22763, #92204 ),
 ( #14378, #81584, #82706 ),
 ( #107898, #13821, #82145 ),
 ( #108458, #5444, #67029 ) ),
 .UNSPECIFIED., .F., .F., .F. ) 
 B_SPLINE_SURFACE_WITH_KNOTS ( ( 4, 4 ),
 ( 3, 3 ),
 ( 0.000000000000000000, 0.0002960034161023850021 ),
 ( 0.000000000000000000, 1.000000000000000000 ),
 .UNSPECIFIED. ) 
 GEOMETRIC_REPRESENTATION_ITEM ( )  RATIONAL_B_SPLINE_SURFACE ( (
 ( 1.000000000000000000, 0.8072480644198086752, 1.000000000000000000),
 ( 1.000000000000000000, 0.8072480346917640937, 1.000000000000000000),
 ( 1.000000000000000000, 0.8071723757218238759, 1.000000000000000000),
 ( 1.000000000000000000, 0.8070209408750101954, 1.000000000000000000) ) ) 
 REPRESENTATION_ITEM ( '' )  SURFACE ( )  );
#67212 = CARTESIAN_POINT ( 'NONE',  ( -22.86388141640000171, 1443.913060387330006, 134.0999999980979851 ) ) ;
#67213 = CARTESIAN_POINT ( 'NONE',  ( 10.13868529792319961, 1424.969151293629920, 198.0587525885179900 ) ) ;
#67214 = CARTESIAN_POINT ( 'NONE',  ( 9.280010414808909758, 1463.749110535250111, 212.8038994763399785 ) ) ;
#67215 = EDGE_CURVE ( 'NONE', #69697, #61631, #18034, .T. ) ;
#67216 = LINE ( 'NONE', #31929, #81747 ) ;
#67217 = CARTESIAN_POINT ( 'NONE',  ( 32.85805783624308418, 1523.678648413191695, 217.1983043299902931 ) ) ;
#67218 = CARTESIAN_POINT ( 'NONE',  ( -17.02454731339999938, 1409.507570680530080, 224.4911189336980044 ) ) ;
#67219 = CARTESIAN_POINT ( 'NONE',  ( 23.88743783590000191, 1410.917949436429808, 210.4190463509079905 ) ) ;
#67220 = DIRECTION ( 'NONE',  ( 0.000000000000000000, 0.000000000000000000, 1.000000000000000000 ) ) ;
#67221 = DIRECTION ( 'NONE',  ( -0.4090087482554316534, 0.000000000000000000, -0.9125304618753967700 ) ) ;
#67222 = CARTESIAN_POINT ( 'NONE',  ( -11.20885044277319942, 1383.862009336539813, 218.6925135829310136 ) ) ;
#67223 = CARTESIAN_POINT ( 'NONE',  ( -0.7800921441517267851, 1526.382868172863937, 176.7869413415625388 ) ) ;
#67224 = CARTESIAN_POINT ( 'NONE',  ( 2.104155298439795985, 1498.155611471770271, 198.0147149805754623 ) ) ;
#67226 = ADVANCED_FACE ( 'NONE', ( #42155 ), #68479, .T. ) ;
#67225 = CARTESIAN_POINT ( 'NONE',  ( -12.45618503170000047, 1416.218047894730262, 222.0802477567980304 ) ) ;
#67227 = CARTESIAN_POINT ( 'NONE',  ( -17.44763429059999993, 1419.603095734770022, 210.4313944482690033 ) ) ;
#67228 = CARTESIAN_POINT ( 'NONE',  ( 0.1994830306498499850, 1463.291321531269887, 182.8118295327159899 ) ) ;
#67230 = ORIENTED_EDGE ( 'NONE', *, *, #49168, .T. ) ;
#67229 = CARTESIAN_POINT ( 'NONE',  ( 0.03232803809133739242, 1407.837594165099972, 222.3069522204950204 ) ) ;
#67231 = CARTESIAN_POINT ( 'NONE',  ( -13.76936860679999874, 1444.324653571829003, 176.3340081878980641 ) ) ;
#67232 = CARTESIAN_POINT ( 'NONE',  ( -17.25884833950082609, 1444.159326553692381, 200.5184012139974357 ) ) ;
#67233 = DIRECTION ( 'NONE',  ( -0.6736849260863839728, 0.000000000000000000, 0.7390186874254150995 ) ) ;
#67234 = CARTESIAN_POINT ( 'NONE',  ( -40.80783872826999925, 1447.308166564250087, 134.0999999984899773 ) ) ;
#67235 = CARTESIAN_POINT ( 'NONE',  ( -109.1652045310000005, 1384.878244280709850, 297.1328263764589792 ) ) ;
#67236 = ORIENTED_EDGE ( 'NONE', *, *, #75435, .F. ) ;
#67238 = EDGE_CURVE ( 'NONE', #9574, #44418, #73950, .T. ) ;
#67237 = CARTESIAN_POINT ( 'NONE',  ( -0.7967004023129989898, 1485.728201538589929, 197.6341324597989910 ) ) ;
#67239 = DIRECTION ( 'NONE',  ( -0.7067700363769178207, -0.03085824620771834489, -0.7067700363772886352 ) ) ;
#67240 = CARTESIAN_POINT ( 'NONE',  ( -104.0864640810399635, 1380.258016915853659, 306.7182003634226817 ) ) ;
#67241 = DIRECTION ( 'NONE',  ( 0.2054769195713296304, 0.000000000000000000, -0.9786619618251631847 ) ) ;
#67242 = EDGE_CURVE ( 'NONE', #50666, #38471, #718, .T. ) ;
#67243 = CARTESIAN_POINT ( 'NONE',  ( -4.027171621128789347, 1433.589808380620070, 217.4404546235140003 ) ) ;
#67244 = CARTESIAN_POINT ( 'NONE',  ( 0.4578175030638683696, 1418.682250877671322, 184.7073717525739482 ) ) ;
#67245 = CARTESIAN_POINT ( 'NONE',  ( 15.90990255763500016, 1516.551704408390151, 198.1616908427670296 ) ) ;
#67246 = LINE ( 'NONE', #43134, #46804 ) ;
#67247 = CARTESIAN_POINT ( 'NONE',  ( -0.1681676274470000065, 1420.473121337229941, 182.7663689088979879 ) ) ;
#67248 = CARTESIAN_POINT ( 'NONE',  ( -70.69551388654410573, 1385.115795056309935, 267.3360060303040200 ) ) ;
#67249 = CARTESIAN_POINT ( 'NONE',  ( -19.39983987834741797, 1522.861859112240154, 239.2921289694189682 ) ) ;
#67250 = CARTESIAN_POINT ( 'NONE',  ( 11.75990446747050022, 1426.852756732119815, 206.8413600417420071 ) ) ;
#67251 = VERTEX_POINT ( 'NONE', #67379 ) ;
#67252 = EDGE_CURVE ( 'NONE', #108761, #36610, #16861, .T. ) ;
#67253 = CARTESIAN_POINT ( 'NONE',  ( -33.29550038720000060, 1451.750386302530160, 134.7337860542980081 ) ) ;
#67254 = CARTESIAN_POINT ( 'NONE',  ( -15.81239927484159935, 1409.848076597319960, 226.2976557237249722 ) ) ;
#67255 = VECTOR ( 'NONE', #103067, 1000.000000000000000 ) ;
#67257 = ORIENTED_EDGE ( 'NONE', *, *, #35093, .F. ) ;
#67256 = DIRECTION ( 'NONE',  ( 5.980589973904019347E-17, -1.000000000000000000, 1.736889445713099699E-16 ) ) ;
#67258 = CARTESIAN_POINT ( 'NONE',  ( 4.808466515050000112, 1473.073685605089850, 218.2848264561289966 ) ) ;
#67259 = VECTOR ( 'NONE', #105553, 1000.000000000000000 ) ;
#67260 = B_SPLINE_CURVE_WITH_KNOTS ( 'NONE', 5,
 ( #92260, #41317, #75488, #32893, #37331, #95574, #88832, #2647, #18844 ),
 .UNSPECIFIED., .F., .F.,
 ( 6, 3, 6 ),
 ( 0.000000000000000000, 0.3683424536080230349, 1.000000000000000000 ),
 .UNSPECIFIED. ) ;
#67261 = CARTESIAN_POINT ( 'NONE',  ( -20.72940845510794361, 1410.996615820652323, 219.0750059994481092 ) ) ;
#67262 = CARTESIAN_POINT ( 'NONE',  ( -109.1169852539999994, 1384.611753107699997, 311.2523998022589922 ) ) ;
#67263 = CARTESIAN_POINT ( 'NONE',  ( -11.24222043440000007, 1491.652723429889875, 206.9322345682190303 ) ) ;
#67264 = DIRECTION ( 'NONE',  ( 0.02616798426500960631, -0.9993150019883682011, -0.02616798426500960631 ) ) ;
#67265 = CARTESIAN_POINT ( 'NONE',  ( 15.78436436265907794, 1512.151624459632103, 197.9925267198427150 ) ) ;
#67266 = CARTESIAN_POINT ( 'NONE',  ( 17.06090267708677644, 1433.319433169794138, 217.0403965233522854 ) ) ;
#67267 = CARTESIAN_POINT ( 'NONE',  ( 2.879377773099999871, 1417.724437854929874, 234.4927649805979968 ) ) ;
#67268 = CARTESIAN_POINT ( 'NONE',  ( -13.73095700724906543, 1379.766849082292993, 213.0184867138244442 ) ) ;
#67269 = CARTESIAN_POINT ( 'NONE',  ( -101.7585531838400357, 1320.102705746892298, 310.5815974945691096 ) ) ;
#67270 = CARTESIAN_POINT ( 'NONE',  ( 3.820241900599999510E-10, 1475.513060387329915, 229.7676991014980104 ) ) ;
#67271 = CARTESIAN_POINT ( 'NONE',  ( -2.255841543630000334, 1456.176501937790135, 199.9086794445890121 ) ) ;
#67272 = CARTESIAN_POINT ( 'NONE',  ( 3.446942071715000111, 1516.842852731759876, 205.8545543269370057 ) ) ;
#67273 = CARTESIAN_POINT ( 'NONE',  ( 3.138402309729999562, 1447.047508311479987, 157.7990817848980214 ) ) ;
#67274 = ORIENTED_EDGE ( 'NONE', *, *, #48895, .T. ) ;
#67275 = CARTESIAN_POINT ( 'NONE',  ( 0.000000000000000000, 1523.051704408389696, 209.1218459616979999 ) ) ;
#67276 = CARTESIAN_POINT ( 'NONE',  ( 13.79590917850000054, 1416.844618635429924, 196.3342909300980068 ) ) ;
#67278 = VERTEX_POINT ( 'NONE', #85802 ) ;
#67277 = CARTESIAN_POINT ( 'NONE',  ( -68.46644754685360112, 1379.747474136280061, 280.0435952495369634 ) ) ;
#67279 = EDGE_CURVE ( 'NONE', #46630, #38078, #34848, .T. ) ;
#67280 = CIRCLE ( 'NONE', #104829, 1.999999999999998668 ) ;
#67281 = CARTESIAN_POINT ( 'NONE',  ( -10.29823179855451265, 1379.271150225059955, 215.9527657008635231 ) ) ;
#67282 = ORIENTED_EDGE ( 'NONE', *, *, #18644, .F. ) ;
#67283 = CYLINDRICAL_SURFACE ( 'NONE', #77827, 0.4999999999999909517 ) ;
#67284 = CARTESIAN_POINT ( 'NONE',  ( -25.18172488869999981, 1449.799985351279929, 206.2325939675880022 ) ) ;
#67286 = CARTESIAN_POINT ( 'NONE',  ( 15.84346258294009857, 1409.719321388350181, 192.1077202728040163 ) ) ;
#67285 = CARTESIAN_POINT ( 'NONE',  ( -11.74236480618606926, 1426.276761585844952, 144.5884759014079464 ) ) ;
#67287 = CARTESIAN_POINT ( 'NONE',  ( -7.321169269124999879, 1516.531533746980131, 210.8305669548069829 ) ) ;
#67288 = EDGE_CURVE ( 'NONE', #20620, #74525, #28104, .T. ) ;
#67289 = CARTESIAN_POINT ( 'NONE',  ( 39.77278037070129812, 1440.034032915139960, 136.7118410945930123 ) ) ;
#67290 = CARTESIAN_POINT ( 'NONE',  ( 5.408518632609999834E-10, 1408.296887868130170, 262.4989398460980397 ) ) ;
#67291 = DIRECTION ( 'NONE',  ( 1.000000000000000000, 0.000000000000000000, 0.000000000000000000 ) ) ;
#67292 = CARTESIAN_POINT ( 'NONE',  ( 12.66352736667499990, 1500.820466445309876, 210.2033082695159862 ) ) ;
#67293 = ITEM_DEFINED_TRANSFORMATION ( 'NONE', 'NONE', #73635,  #21632 ) ;
#67294 = CARTESIAN_POINT ( 'NONE',  ( 36.72650137404210113, 1451.114006374460132, 134.0999999987039644 ) ) ;
#67295 = CARTESIAN_POINT ( 'NONE',  ( -35.70801268710279430, 1437.331117183020069, 136.5359098274630014 ) ) ;
#67296 = EDGE_LOOP ( 'NONE', ( #108681, #108837 ) ) ;
#67297 = CARTESIAN_POINT ( 'NONE',  ( -9.609622886946858955, 1464.248407205509920, 228.1966016402350022 ) ) ;
#67298 = DIRECTION ( 'NONE',  ( 0.000000000000000000, -0.7071067811865475727, -0.7071067811865475727 ) ) ;
#67299 = VERTEX_POINT ( 'NONE', #61200 ) ;
#67300 = VERTEX_POINT ( 'NONE', #105936 ) ;
#67301 = CARTESIAN_POINT ( 'NONE',  ( 10.24817655218739887, 1453.388637960930055, 211.8760523666580298 ) ) ;
#67302 = ADVANCED_FACE ( 'NONE', ( #2939 ), #83391, .T. ) ;
#67303 = CARTESIAN_POINT ( 'NONE',  ( -14.28952585159370159, 1380.314717283680011, 210.1167927017139903 ) ) ;
#67304 = CARTESIAN_POINT ( 'NONE',  ( -13.59236344883730041, 1508.248948055430219, 209.5387630291689902 ) ) ;
#67305 = CARTESIAN_POINT ( 'NONE',  ( 4.325231581420000637, 1515.225841049890050, 210.2096722485289888 ) ) ;
#67306 = CARTESIAN_POINT ( 'NONE',  ( -4.659350606432629327, 1455.294773417379929, 200.9200808099520259 ) ) ;
#67307 = CARTESIAN_POINT ( 'NONE',  ( 36.37832872589339672, 1435.767865734180077, 134.7402661757760143 ) ) ;
#67308 = CARTESIAN_POINT ( 'NONE',  ( 4.752602785698186949, 1516.784510156639953, 214.9408003802788301 ) ) ;
#67309 = CARTESIAN_POINT ( 'NONE',  ( 27.30844321330000213, 1439.416619586579827, 137.0772895148980126 ) ) ;
#67310 = CARTESIAN_POINT ( 'NONE',  ( -11.83879355810000078, 1391.851285459460087, 211.5674355249090013 ) ) ;
#67311 = CARTESIAN_POINT ( 'NONE',  ( -85.93326510183719336, 1384.821889067519805, 289.5792165609069571 ) ) ;
#67312 = ORIENTED_EDGE ( 'NONE', *, *, #90442, .F. ) ;
#67313 = CARTESIAN_POINT ( 'NONE',  ( -6.942973667334999988, 1516.833844030519913, 201.7931697622170191 ) ) ;
#67314 = CARTESIAN_POINT ( 'NONE',  ( -1.906501101195560124E-08, 1517.020990152690047, 209.1218459511669892 ) ) ;
#67315 = ORIENTED_EDGE ( 'NONE', *, *, #74694, .F. ) ;
#67316 = CARTESIAN_POINT ( 'NONE',  ( 10.79382126600000014, 1414.913060387329779, 222.1041115775979904 ) ) ;
#67317 = ADVANCED_FACE ( 'NONE', ( #36511 ), #68859, .T. ) ;
#67318 = CARTESIAN_POINT ( 'NONE',  ( 4.963882991561403557, 1511.398734635483606, 217.6327391777064122 ) ) ;
#67319 = ORIENTED_EDGE ( 'NONE', *, *, #5484, .F. ) ;
#67320 = CARTESIAN_POINT ( 'NONE',  ( -13.91566348329999947, 1415.553739809529816, 221.3028765811980065 ) ) ;
#67321 = CARTESIAN_POINT ( 'NONE',  ( -12.53380499169999851, 1442.773887286369927, 169.4755105685979970 ) ) ;
#67322 = CARTESIAN_POINT ( 'NONE',  ( -18.60427693160000118, 1442.816495467589903, 206.3589439838089845 ) ) ;
#67323 = CARTESIAN_POINT ( 'NONE',  ( -4.138380534042295444, 1488.912756140813372, 219.2090725797449409 ) ) ;
#67324 = CARTESIAN_POINT ( 'NONE',  ( -12.74111566449999877, 1416.823634022930037, 221.9826245047979967 ) ) ;
#67325 = EDGE_CURVE ( 'NONE', #80757, #57302, #103776, .T. ) ;
#67326 = CARTESIAN_POINT ( 'NONE',  ( 10.16156728606890169, 1469.494191575119885, 207.3232880352639711 ) ) ;
#67327 = LINE ( 'NONE', #91949, #10181 ) ;
#67328 = CARTESIAN_POINT ( 'NONE',  ( -16.82650407848411334, 1517.015068014068447, 194.8356516383118731 ) ) ;
#67329 = CARTESIAN_POINT ( 'NONE',  ( -62.16362557989999971, 1379.729112816429961, 266.3118224345589624 ) ) ;
#67330 = CARTESIAN_POINT ( 'NONE',  ( -16.47067245780000277, 1485.103171130329883, 223.7192837535979777 ) ) ;
#67332 = CARTESIAN_POINT ( 'NONE',  ( 6.046917389341460058, 1467.277928683999789, 199.7767350800179997 ) ) ;
#67331 = CARTESIAN_POINT ( 'NONE',  ( 17.94899309970000090, 1459.572665234330088, 228.0797701638979902 ) ) ;
#67333 = CARTESIAN_POINT ( 'NONE',  ( 6.454036364709999418, 1470.375359969389820, 211.5526526928690032 ) ) ;
#67334 = B_SPLINE_CURVE_WITH_KNOTS ( 'NONE', 5,
 ( #44630, #80973, #10456, #79882, #71518, #36215 ),
 .UNSPECIFIED., .F., .F.,
 ( 6, 6 ),
 ( -92.88478189117469697, -23.15748665169219578 ),
 .UNSPECIFIED. ) ;
#67335 = CARTESIAN_POINT ( 'NONE',  ( 2.873329360754999673, 1516.572193931679976, 216.4439510378570048 ) ) ;
#67336 = ORIENTED_EDGE ( 'NONE', *, *, #81902, .F. ) ;
#67337 = CARTESIAN_POINT ( 'NONE',  ( -1.924560002181862739, 1486.146552202361818, 181.8515281887476362 ) ) ;
#67338 = CARTESIAN_POINT ( 'NONE',  ( 0.8595391288403605445, 1516.693423516305984, 216.8350443691653879 ) ) ;
#67339 = CARTESIAN_POINT ( 'NONE',  ( -2.286446363765000100, 1517.042661899400173, 213.7475398352470108 ) ) ;
#67340 = EDGE_CURVE ( 'NONE', #15596, #22899, #54310, .T. ) ;
#67341 = CARTESIAN_POINT ( 'NONE',  ( 17.69507376876702764, 1521.951704408389787, 202.0148427140983358 ) ) ;
#67342 = CARTESIAN_POINT ( 'NONE',  ( -11.60004869885204037, 1426.058235232188963, 138.8694919005308179 ) ) ;
#67344 = VERTEX_POINT ( 'NONE', #9637 ) ;
#67343 = CARTESIAN_POINT ( 'NONE',  ( -12.22599082290759931, 1501.771664294480161, 211.5404786625699955 ) ) ;
#67345 = CARTESIAN_POINT ( 'NONE',  ( -8.156587055619999305, 1384.920249147410232, 199.6468410606589998 ) ) ;
#67346 = CARTESIAN_POINT ( 'NONE',  ( 17.71193101246160140, 1521.951704408389787, 196.6727161460330251 ) ) ;
#67347 = EDGE_CURVE ( 'NONE', #71735, #67105, #78507, .T. ) ;
#67348 = CARTESIAN_POINT ( 'NONE',  ( -11.75953795439999894, 1426.408695322430049, 145.8957383316979985 ) ) ;
#67349 = DIRECTION ( 'NONE',  ( 0.9455185755993178454, 0.000000000000000000, -0.3255681544571539243 ) ) ;
#67350 = CARTESIAN_POINT ( 'NONE',  ( 2.532296112024570167, 1445.968147867059997, 199.3366315615400026 ) ) ;
#67351 = CARTESIAN_POINT ( 'NONE',  ( -1.010302820291719810E-14, 1421.486528639720063, 147.6331986621470094 ) ) ;
#67352 = CARTESIAN_POINT ( 'NONE',  ( -6.871201816620469138, 1426.439416242710195, 202.8156393802020148 ) ) ;
#67353 = CARTESIAN_POINT ( 'NONE',  ( 7.105427357599999217E-15, 1432.413060387330006, 146.1721969590979882 ) ) ;
#67354 = EDGE_CURVE ( 'NONE', #30026, #89438, #54973, .T. ) ;
#67356 = CARTESIAN_POINT ( 'NONE',  ( -3.515242004654977492, 1419.856981650250191, 137.0999999980978430 ) ) ;
#67355 = CARTESIAN_POINT ( 'NONE',  ( -19.02532173170000007, 1470.092591092030034, 227.7517131706979967 ) ) ;
#67357 = DIRECTION ( 'NONE',  ( 0.1261098496724238627, 0.9885420249951558658, -0.08295161622340639640 ) ) ;
#67358 = VERTEX_POINT ( 'NONE', #18577 ) ;
#67359 = CARTESIAN_POINT ( 'NONE',  ( -7.724423432224999608, 1517.122088787240045, 205.6676733166769964 ) ) ;
#67360 = CARTESIAN_POINT ( 'NONE',  ( 3.756404312819999980, 1406.179919416030089, 269.0400515133979980 ) ) ;
#67361 = CARTESIAN_POINT ( 'NONE',  ( -32.23107245337067184, 1523.542365884047285, 216.8383915158452453 ) ) ;
#67362 = CARTESIAN_POINT ( 'NONE',  ( 19.84704116899999704, 1449.730418169799805, 193.3609370523980147 ) ) ;
#67363 = EDGE_CURVE ( 'NONE', #49086, #90041, #2456, .T. ) ;
#67364 = AXIS2_PLACEMENT_3D ( 'NONE', #50137, #5168, #66211 ) ;
#67365 = CARTESIAN_POINT ( 'NONE',  ( -0.1579380382326590060, 1508.143587606610026, 237.5556629045009913 ) ) ;
#67366 = CARTESIAN_POINT ( 'NONE',  ( -9.640608181049721281, 1389.788252704991919, 216.8809208289262358 ) ) ;
#67367 = CARTESIAN_POINT ( 'NONE',  ( -1.757532404670000048, 1451.933574905729756, 184.1885909310980196 ) ) ;
#67368 = CARTESIAN_POINT ( 'NONE',  ( 16.63395377013535636, 1459.015803111507921, 231.1847133987910468 ) ) ;
#67369 = CARTESIAN_POINT ( 'NONE',  ( -15.81441164190000315, 1416.657489259210024, 207.5143518867189982 ) ) ;
#67370 = CARTESIAN_POINT ( 'NONE',  ( -13.02484207390000037, 1445.915793797939841, 187.8647291817979976 ) ) ;
#67371 = CARTESIAN_POINT ( 'NONE',  ( -15.98141629860000101, 1475.513060387329915, 223.7206687197979988 ) ) ;
#67372 = CARTESIAN_POINT ( 'NONE',  ( -17.64146421497870065, 1419.304501645640130, 207.1873797621490212 ) ) ;
#67373 = CARTESIAN_POINT ( 'NONE',  ( -4.885870092120000230, 1496.077246227390106, 219.2393726144989898 ) ) ;
#67374 = B_SPLINE_CURVE_WITH_KNOTS ( 'NONE', 5,
 ( #3096, #106617, #54601, #96581, #12017, #20945 ),
 .UNSPECIFIED., .F., .F.,
 ( 6, 6 ),
 ( -2.000000000000000000, 0.000000000000000000 ),
 .UNSPECIFIED. ) ;
#67375 = CARTESIAN_POINT ( 'NONE',  ( -2.151012986799999638, 1477.102208436890123, 201.8328325564689862 ) ) ;
#67376 = CARTESIAN_POINT ( 'NONE',  ( -18.57221558799999883, 1434.150321635919909, 219.6133835466979747 ) ) ;
#67377 = ADVANCED_FACE ( 'NONE', ( #44377 ), #27556, .T. ) ;
#67378 = CARTESIAN_POINT ( 'NONE',  ( -10.68670300233429948, 1508.551704408280102, 208.2058367971190194 ) ) ;
#67379 = CARTESIAN_POINT ( 'NONE',  ( -14.49383181622579997, 1422.099016211560183, 229.4564907068830166 ) ) ;
#67380 = CARTESIAN_POINT ( 'NONE',  ( -9.911219186020000294, 1475.204444335230164, 267.1956757164980445 ) ) ;
#67381 = CARTESIAN_POINT ( 'NONE',  ( 1.361307284737899970, 1413.955589619809871, 232.7931714649010075 ) ) ;
#67382 = CARTESIAN_POINT ( 'NONE',  ( -12.41968314313910682, 1391.384630218451093, 211.0556431160394197 ) ) ;
#67383 = ADVANCED_FACE ( 'NONE', ( #21872 ), #89658, .F. ) ;
#67384 = LINE ( 'NONE', #43272, #11055 ) ;
#67385 = CARTESIAN_POINT ( 'NONE',  ( -46.40682475798950435, 1384.757411015490106, 254.3673974098619794 ) ) ;
#67386 = CARTESIAN_POINT ( 'NONE',  ( -106.6958069642329860, 1391.913060387289988, 302.4589463478089897 ) ) ;
#67387 = CARTESIAN_POINT ( 'NONE',  ( 11.53151684852190151, 1415.184612916159949, 222.8541440776940021 ) ) ;
#67388 = CARTESIAN_POINT ( 'NONE',  ( -107.6455384790000096, 1378.913060387289988, 299.9332720164590000 ) ) ;
#67389 = CARTESIAN_POINT ( 'NONE',  ( 2.500000000000000000, 1440.913060387330006, 137.0999999980979851 ) ) ;
#67390 = CARTESIAN_POINT ( 'NONE',  ( -45.88374309256568750, 1440.913026864722724, 266.4124039852627561 ) ) ;
#67391 =( BOUNDED_SURFACE ( )  B_SPLINE_SURFACE ( 4, 2, ( 
 ( #43121, #33584, #25734 ),
 ( #77280, #34703, #51515 ),
 ( #93496, #15665, #85648 ),
 ( #577, #68895, #50970 ),
 ( #9503, #102997, #7303 ) ),
 .UNSPECIFIED., .F., .F., .F. ) 
 B_SPLINE_SURFACE_WITH_KNOTS ( ( 5, 5 ),
 ( 3, 3 ),
 ( 3.613988937040000238, 5.260361675040000407 ),
 ( 5.300753508049940166, 6.150222949633159963 ),
 .UNSPECIFIED. ) 
 GEOMETRIC_REPRESENTATION_ITEM ( )  RATIONAL_B_SPLINE_SURFACE ( (
 ( 0.8627701935039370218, 0.8230338693346749279, 0.9546124223293859234),
 ( 0.8627701935039370218, 0.8230338693346749279, 0.9546124223293859234),
 ( 0.8627701935039370218, 0.8230338693346749279, 0.9546124223293859234),
 ( 0.8627701935039370218, 0.8230338693346749279, 0.9546124223293859234),
 ( 0.8627701935039370218, 0.8230338693346749279, 0.9546124223293859234) ) ) 
 REPRESENTATION_ITEM ( '' )  SURFACE ( )  );
#67392 = CARTESIAN_POINT ( 'NONE',  ( -22.19955145049999956, 1411.048519434129958, 202.6338174844580067 ) ) ;
#67393 = CARTESIAN_POINT ( 'NONE',  ( -9.033771706128597145, 1381.576731241501420, 200.6091943981350312 ) ) ;
#67394 = CARTESIAN_POINT ( 'NONE',  ( 12.49224530861089910, 1421.594377902519909, 207.3542241632320042 ) ) ;
#67395 = CARTESIAN_POINT ( 'NONE',  ( 11.05809750370510081, 1479.027348187909865, 206.7510526044619894 ) ) ;
#67396 = CARTESIAN_POINT ( 'NONE',  ( 2.500000000000000000, 1443.913060387330006, 150.6726614421979775 ) ) ;
#67397 = CARTESIAN_POINT ( 'NONE',  ( 5.278853968920000028, 1437.432420937689812, 228.7383191228989858 ) ) ;
#67398 = CARTESIAN_POINT ( 'NONE',  ( 17.19757137884747777, 1524.059547553518996, 180.8698536207154461 ) ) ;
#67399 = CARTESIAN_POINT ( 'NONE',  ( -17.11734381175650199, 1420.830841924690048, 201.6585952501770009 ) ) ;
#67401 = CARTESIAN_POINT ( 'NONE',  ( -13.41525439013790155, 1379.584674364849889, 211.7907235378989981 ) ) ;
#67400 = CARTESIAN_POINT ( 'NONE',  ( -16.88664006666689943, 1417.438760776740082, 207.9215829781489902 ) ) ;
#67402 = CARTESIAN_POINT ( 'NONE',  ( 11.73199753003260071, 1426.699139563339941, 143.8094287576769830 ) ) ;
#67403 = CARTESIAN_POINT ( 'NONE',  ( 17.29393938232482952, 1523.621879633028811, 237.3864571009499969 ) ) ;
#67404 = CARTESIAN_POINT ( 'NONE',  ( -123.7789942036000070, 1376.302340817389904, 298.5517755817790544 ) ) ;
#67405 = CARTESIAN_POINT ( 'NONE',  ( 6.788622268498730072, 1448.339992550449779, 201.4086086841240331 ) ) ;
#67406 = CARTESIAN_POINT ( 'NONE',  ( -0.06052882951021919949, 1420.434688371959965, 183.3377468054080168 ) ) ;
#67407 = CARTESIAN_POINT ( 'NONE',  ( -7.333070173014999860, 1516.955859323880077, 203.3428461583270064 ) ) ;
#67408 = DIRECTION ( 'NONE',  ( -0.08330058268155800250, -0.04363816682463637214, -0.9955685427538869536 ) ) ;
#67409 = FACE_OUTER_BOUND ( 'NONE', #108550, .T. ) ;
#67410 = CARTESIAN_POINT ( 'NONE',  ( 16.76527320893499962, 1513.875858217490077, 195.2591379279669752 ) ) ;
#67411 = CARTESIAN_POINT ( 'NONE',  ( 7.878537825433329367, 1517.051704408389924, 200.0586249522280013 ) ) ;
#67412 = CARTESIAN_POINT ( 'NONE',  ( -35.15050912068899436, 1380.172863641740150, 221.1654657214490101 ) ) ;
#67413 = CARTESIAN_POINT ( 'NONE',  ( 19.99715769724119951, 1508.853444755030068, 229.3809204472839838 ) ) ;
#67416 = ORIENTED_EDGE ( 'NONE', *, *, #78822, .T. ) ;
#67415 = CARTESIAN_POINT ( 'NONE',  ( -36.52309517079940093, 1379.688050188520037, 223.7231089615120254 ) ) ;
#67414 = AXIS2_PLACEMENT_3D ( 'NONE', #66152, #31960, #34167 ) ;
#67417 = ORIENTED_EDGE ( 'NONE', *, *, #16854, .T. ) ;
#67418 = CARTESIAN_POINT ( 'NONE',  ( 11.98355472118069898, 1433.631889606809864, 149.9631560847739706 ) ) ;
#67419 = CARTESIAN_POINT ( 'NONE',  ( -11.29356329139999993, 1396.307440307529987, 211.1970805475479835 ) ) ;
#67420 = ORIENTED_EDGE ( 'NONE', *, *, #66055, .T. ) ;
#67421 = CARTESIAN_POINT ( 'NONE',  ( -105.8600500019999942, 1378.913059667080006, 305.6175922275590437 ) ) ;
#67422 = DIRECTION ( 'NONE',  ( -1.755985294532469921E-16, 1.000000000000000000, -1.338183447452830017E-16 ) ) ;
#67423 = CARTESIAN_POINT ( 'NONE',  ( 2.849562163010020299, 1515.551843419029865, 205.1388868824799943 ) ) ;
#67425 = DIRECTION ( 'NONE',  ( -4.648609652910299899E-17, -1.000000000000000000, 2.252106476759999926E-16 ) ) ;
#67424 = CARTESIAN_POINT ( 'NONE',  ( -16.73628186595804479, 1526.382868172863937, 234.1845039693045862 ) ) ;
#67426 = CARTESIAN_POINT ( 'NONE',  ( 18.73044736589999815, 1507.815472637730181, 230.0234365859979846 ) ) ;
#67427 =( BOUNDED_CURVE ( )  B_SPLINE_CURVE ( 3, ( #91090, #42345, #60265, #9299 ),
 .UNSPECIFIED., .F., .T. ) 
 B_SPLINE_CURVE_WITH_KNOTS ( ( 4, 4 ),
 ( 1.268017761107936181, 1.928411118409885106 ),
 .UNSPECIFIED. ) 
 CURVE ( )  GEOMETRIC_REPRESENTATION_ITEM ( )  RATIONAL_B_SPLINE_CURVE ( ( 1.000000000000000000, 0.9639857285903185025, 0.9639857285903185025, 1.000000000000000000 ) ) 
 REPRESENTATION_ITEM ( '' )  );
#67428 = CARTESIAN_POINT ( 'NONE',  ( 0.6876992757690000291, 1429.776213807130034, 184.2878479203979794 ) ) ;
#67429 = CARTESIAN_POINT ( 'NONE',  ( 2.800557851600000259, 1466.634424046189906, 219.8247096032989987 ) ) ;
#67430 = CARTESIAN_POINT ( 'NONE',  ( 42.06232107069909887, 1440.913053860320133, 269.6487541118979721 ) ) ;
#67431 =( NAMED_UNIT ( * ) PLANE_ANGLE_UNIT ( ) SI_UNIT ( $, .RADIAN. ) );
#67432 = CARTESIAN_POINT ( 'NONE',  ( 11.31770122492290120, 1479.526177409110232, 208.6192917484059990 ) ) ;
#67433 = CARTESIAN_POINT ( 'NONE',  ( -1.547462741870939906, 1414.913060391199906, 225.9340804956229931 ) ) ;
#67434 = CARTESIAN_POINT ( 'NONE',  ( 11.76160536819999969, 1431.728708710070123, 150.7840645346979898 ) ) ;
#67435 = CARTESIAN_POINT ( 'NONE',  ( 6.059489635994999013, 1514.830240247470101, 201.1594993559769762 ) ) ;
#67436 = ORIENTED_EDGE ( 'NONE', *, *, #43456, .T. ) ;
#67437 = CARTESIAN_POINT ( 'NONE',  ( 13.06529732548069944, 1434.818778377569970, 149.3188580375970105 ) ) ;
#67438 = EDGE_LOOP ( 'NONE', ( #107843, #50618, #12814, #1549 ) ) ;
#67439 = ORIENTED_EDGE ( 'NONE', *, *, #94615, .T. ) ;
#67440 = CARTESIAN_POINT ( 'NONE',  ( 13.44971459290628601, 1444.299826105456532, 169.3629876352260055 ) ) ;
#67441 = CARTESIAN_POINT ( 'NONE',  ( -4.894696787210000011, 1465.369418360130112, 234.6993435765979825 ) ) ;
#67442 = CARTESIAN_POINT ( 'NONE',  ( -8.866214871307620982, 1407.269089423789865, 199.4203128504979929 ) ) ;
#67443 = AXIS2_PLACEMENT_3D ( 'NONE', #92622, #7526, #41684 ) ;
#67444 = CARTESIAN_POINT ( 'NONE',  ( 1.128757561074999805, 1516.608208975040043, 216.8328129478670121 ) ) ;
#67445 = CARTESIAN_POINT ( 'NONE',  ( -8.652776130911478347, 1511.435001053830092, 214.5073691320910143 ) ) ;
#67446 = CARTESIAN_POINT ( 'NONE',  ( -11.33291981729999875, 1502.012779296890130, 207.3104068824690103 ) ) ;
#67447 = CARTESIAN_POINT ( 'NONE',  ( 0.000000000000000000, 1526.382868172863937, 209.1218459616979999 ) ) ;
#67448 = CARTESIAN_POINT ( 'NONE',  ( -26.37171023119999802, 1379.942807944750029, 211.7994354412990106 ) ) ;
#67449 = VERTEX_POINT ( 'NONE', #39256 ) ;
#67450 = CARTESIAN_POINT ( 'NONE',  ( 7.323034273964999841, 1516.609912606490070, 205.6670971239069843 ) ) ;
#67451 = ORIENTED_EDGE ( 'NONE', *, *, #16679, .F. ) ;
#67452 = CARTESIAN_POINT ( 'NONE',  ( 20.33301140202129886, 1440.913060387330006, 218.5204036554350182 ) ) ;
#67453 = CYLINDRICAL_SURFACE ( 'NONE', #107030, 0.9999999999999888978 ) ;
#67454 = CARTESIAN_POINT ( 'NONE',  ( -11.89919548239999969, 1409.328589449730089, 190.2794074207979804 ) ) ;
#67455 = CARTESIAN_POINT ( 'NONE',  ( 7.587489894784999578, 1513.914017980350081, 215.5240844366570059 ) ) ;
#67457 = VERTEX_POINT ( 'NONE', #12944 ) ;
#67456 = CARTESIAN_POINT ( 'NONE',  ( -0.7266101759396799142, 1414.971717244350202, 226.0555041422940121 ) ) ;
#67458 = CARTESIAN_POINT ( 'NONE',  ( 22.72408229139999847, 1432.100443994239868, 218.1715127473280234 ) ) ;
#67459 = CARTESIAN_POINT ( 'NONE',  ( 3.346707516019999940, 1443.005054410889898, 217.3642451189890323 ) ) ;
#67460 = DIRECTION ( 'NONE',  ( -1.755985294532469921E-16, 1.000000000000000000, -1.338183447452831989E-16 ) ) ;
#67461 = FACE_OUTER_BOUND ( 'NONE', #97558, .T. ) ;
#67462 = B_SPLINE_CURVE_WITH_KNOTS ( 'NONE', 5,
 ( #82664, #39557, #56367, #40653, #66436, #14885 ),
 .UNSPECIFIED., .F., .F.,
 ( 6, 6 ),
 ( 0.000000000000000000, 1.000000000000000000 ),
 .UNSPECIFIED. ) ;
#67463 = CIRCLE ( 'NONE', #85324, 1.638701816490922836 ) ;
#67464 = CARTESIAN_POINT ( 'NONE',  ( 1.133516965105000107, 1516.713079096360161, 213.7319258036569920 ) ) ;
#67465 = CARTESIAN_POINT ( 'NONE',  ( -3.775538771436770080, 1428.481285291019958, 200.5571954888419839 ) ) ;
#67466 = FACE_OUTER_BOUND ( 'NONE', #5684, .T. ) ;
#67467 = CARTESIAN_POINT ( 'NONE',  ( 7.443079126130860423, 1508.729257035799947, 215.2419638459840030 ) ) ;
#67468 = CARTESIAN_POINT ( 'NONE',  ( 5.012938863775000087, 1517.051603658920158, 211.6026598552170128 ) ) ;
#67469 = CARTESIAN_POINT ( 'NONE',  ( 9.738091431092259498, 1435.054350372520048, 207.9788105490890189 ) ) ;
#67470 = CARTESIAN_POINT ( 'NONE',  ( 14.29520360740000129, 1410.788278508630128, 191.3967167922980082 ) ) ;
#67471 = DIRECTION ( 'NONE',  ( 0.7067699325522937004, 0.03085807370314938569, -0.7067701477335875948 ) ) ;
#67473 = ORIENTED_EDGE ( 'NONE', *, *, #57841, .F. ) ;
#67472 = CARTESIAN_POINT ( 'NONE',  ( -49.69844455709999664, 1386.731746342069755, 260.8593201508589914 ) ) ;
#67474 = CARTESIAN_POINT ( 'NONE',  ( -52.69031413145209797, 1385.105943313089938, 267.2253354263970095 ) ) ;
#67475 = EDGE_CURVE ( 'NONE', #85422, #65987, #93044, .T. ) ;
#67476 = CARTESIAN_POINT ( 'NONE',  ( 34.48978216820000142, 1440.913060384829805, 250.0021841762979875 ) ) ;
#67477 = EDGE_CURVE ( 'NONE', #70504, #52452, #105661, .T. ) ;
#67478 = CARTESIAN_POINT ( 'NONE',  ( -115.0779893851147193, 1305.733110638860126, 307.2933849238752373 ) ) ;
#67479 = CARTESIAN_POINT ( 'NONE',  ( -3.454294121580000265, 1417.605600631229890, 235.1430308038980002 ) ) ;
#67480 = B_SPLINE_CURVE_WITH_KNOTS ( 'NONE', 5,
 ( #4188, #53086, #103450, #94499, #27869, #81411 ),
 .UNSPECIFIED., .F., .F.,
 ( 6, 6 ),
 ( 0.000000000000000000, 1.000000000000000000 ),
 .UNSPECIFIED. ) ;
#67481 = CARTESIAN_POINT ( 'NONE',  ( -24.02240277289999781, 1444.576888666170134, 212.2493134410879918 ) ) ;
#67482 = CARTESIAN_POINT ( 'NONE',  ( 11.02428137103500028, 1512.359593911809952, 224.9978793913670074 ) ) ;
#67483 = AXIS2_PLACEMENT_3D ( 'NONE', #33713, #16346, #41020 ) ;
#67485 = CARTESIAN_POINT ( 'NONE',  ( -8.297681820259999341, 1384.894008818040220, 218.7035870978390051 ) ) ;
#67484 = CARTESIAN_POINT ( 'NONE',  ( -4.616899872884999922, 1517.050041317280147, 216.8443827349270236 ) ) ;
#67486 = CARTESIAN_POINT ( 'NONE',  ( -9.310808169944788659, 1449.136903302260180, 208.8655000368800074 ) ) ;
#67487 = CARTESIAN_POINT ( 'NONE',  ( -109.6092339890690113, 1383.179580026969916, 311.2151190870969799 ) ) ;
#67488 = ORIENTED_EDGE ( 'NONE', *, *, #26320, .T. ) ;
#67489 = CARTESIAN_POINT ( 'NONE',  ( -1.709358701255000001, 1516.542957540330008, 202.1882582765869927 ) ) ;
#67490 = CARTESIAN_POINT ( 'NONE',  ( 0.2341451561260000092, 1497.013800431029949, 230.6965820202980240 ) ) ;
#67491 = VECTOR ( 'NONE', #10497, 1000.000000000000114 ) ;
#67492 = ADVANCED_FACE ( 'NONE', ( #41880 ), #30852, .T. ) ;
#67493 = CYLINDRICAL_SURFACE ( 'NONE', #73358, 0.4999999999999449329 ) ;
#67494 = DIRECTION ( 'NONE',  ( -5.980589973904019347E-17, 1.000000000000000000, -1.736889445713099699E-16 ) ) ;
#67495 = CARTESIAN_POINT ( 'NONE',  ( -7.992444398102118264, 1461.756363228467990, 203.5959791406405088 ) ) ;
#67496 = CARTESIAN_POINT ( 'NONE',  ( 4.789673499540000101, 1465.867933640490037, 219.0700355186390027 ) ) ;
#67497 = CARTESIAN_POINT ( 'NONE',  ( 14.94073065363653008, 1420.536355086338062, 228.0011852406256025 ) ) ;
#67498 = CARTESIAN_POINT ( 'NONE',  ( 32.00873930189860062, 1435.615230547090050, 135.1257559928430112 ) ) ;
#67499 = CARTESIAN_POINT ( 'NONE',  ( 38.29258608828820343, 1448.551925925989963, 136.4167175071939937 ) ) ;
#67500 = FACE_OUTER_BOUND ( 'NONE', #89937, .T. ) ;
#67501 = CARTESIAN_POINT ( 'NONE',  ( -109.4241442180000092, 1385.278508194390042, 297.1426266650590264 ) ) ;
#67502 = CARTESIAN_POINT ( 'NONE',  ( 10.23468988059999951, 1508.269291830929888, 183.6304174551979997 ) ) ;
#67503 = CARTESIAN_POINT ( 'NONE',  ( -21.11881948555236121, 1525.651286436460396, 184.9294397280434623 ) ) ;
#67504 = CARTESIAN_POINT ( 'NONE',  ( -27.06221056512304912, 1464.234489086119765, 269.4420994688821338 ) ) ;
#67505 = VERTEX_POINT ( 'NONE', #91318 ) ;
#67506 = CARTESIAN_POINT ( 'NONE',  ( 9.793647689141911528, 1463.364106758136359, 209.6829145745567757 ) ) ;
#67507 = CARTESIAN_POINT ( 'NONE',  ( -11.29656894142413037, 1407.765265707235130, 269.6109022948709253 ) ) ;
#67508 = CARTESIAN_POINT ( 'NONE',  ( 5.172586535390000684, 1492.767659076290101, 188.8148697515989909 ) ) ;
#67509 = CARTESIAN_POINT ( 'NONE',  ( 16.12453495796710001, 1481.913039286089997, 188.8995036690789959 ) ) ;
#67510 = CARTESIAN_POINT ( 'NONE',  ( 10.91296393538931220, 1424.870198133627355, 138.2545201306494960 ) ) ;
#67512 = VECTOR ( 'NONE', #428, 1000.000000000000000 ) ;
#67511 = CARTESIAN_POINT ( 'NONE',  ( 12.68801076269999939, 1500.413651118889902, 208.6561541774999853 ) ) ;
#67513 = CARTESIAN_POINT ( 'NONE',  ( -28.25086640909999858, 1508.135711191930113, 208.8579954691720104 ) ) ;
#67514 = EDGE_CURVE ( 'NONE', #10483, #69831, #102776, .T. ) ;
#67515 = CARTESIAN_POINT ( 'NONE',  ( -9.361409357458470026, 1438.259538539160076, 210.6630235057149889 ) ) ;
#67516 = CARTESIAN_POINT ( 'NONE',  ( 2.020654978418439995, 1495.217425279760164, 220.5028404108620066 ) ) ;
#67517 = DIRECTION ( 'NONE',  ( 0.000000000000000000, 0.000000000000000000, 1.000000000000000000 ) ) ;
#67518 = CARTESIAN_POINT ( 'NONE',  ( -14.65103220135884499, 1451.163773513072101, 149.9447318886720382 ) ) ;
#67519 = CARTESIAN_POINT ( 'NONE',  ( -5.552491127060000586, 1484.291244666589819, 199.5131677064289875 ) ) ;
#67520 = CARTESIAN_POINT ( 'NONE',  ( 24.74089786250000245, 1435.642227076270046, 137.1785840707979958 ) ) ;
#67522 = ADVANCED_FACE ( 'NONE', ( #98609 ), #26012, .F. ) ;
#67521 = CARTESIAN_POINT ( 'NONE',  ( -12.95651626014300639, 1442.923275661127491, 169.4280452214743775 ) ) ;
#67523 = ORIENTED_EDGE ( 'NONE', *, *, #98663, .F. ) ;
#67524 = DIRECTION ( 'NONE',  ( 0.000000000000000000, 0.000000000000000000, 1.000000000000000000 ) ) ;
#67525 = CARTESIAN_POINT ( 'NONE',  ( -12.04245058442665695, 1377.963961494413525, 211.7131635820066435 ) ) ;
#67526 = ORIENTED_EDGE ( 'NONE', *, *, #73287, .T. ) ;
#67527 = VERTEX_POINT ( 'NONE', #2117 ) ;
#67528 = CARTESIAN_POINT ( 'NONE',  ( 1.477486856589759867, 1435.528368648049991, 227.5227238277980177 ) ) ;
#67529 = CARTESIAN_POINT ( 'NONE',  ( -15.30308233943090102, 1416.035155480296453, 206.6202068181550828 ) ) ;
#67531 = CARTESIAN_POINT ( 'NONE',  ( -16.00255113769999937, 1456.293564252130182, 216.3706747924380238 ) ) ;
#67530 = CARTESIAN_POINT ( 'NONE',  ( 1.758536932969999800, 1455.155312436190115, 218.3895007395989865 ) ) ;
#67532 = CARTESIAN_POINT ( 'NONE',  ( -8.272393485109997613, 1447.204352650790042, 213.4245211968789988 ) ) ;
#67533 = CARTESIAN_POINT ( 'NONE',  ( 4.292760611305180163, 1425.438012504090239, 185.4035972331899984 ) ) ;
#67534 = CARTESIAN_POINT ( 'NONE',  ( -12.31039754504540085, 1378.376187213689946, 209.7956876274450053 ) ) ;
#67535 = CIRCLE ( 'NONE', #74729, 11.34254167809999991 ) ;
#67536 = CARTESIAN_POINT ( 'NONE',  ( -2.656119403435029280, 1420.364487350997479, 185.9144866987654154 ) ) ;
#67537 = CARTESIAN_POINT ( 'NONE',  ( 7.377911345740000293, 1424.802628287519838, 212.4706883527589696 ) ) ;
#67538 = CARTESIAN_POINT ( 'NONE',  ( -24.23237730770000198, 1438.888001088869942, 211.7327264377979645 ) ) ;
#67539 = FACE_BOUND ( 'NONE', #70471, .T. ) ;
#67540 = CARTESIAN_POINT ( 'NONE',  ( 0.003568499702431209702, 1467.142144108200000, 235.6416276161930057 ) ) ;
#67541 = CARTESIAN_POINT ( 'NONE',  ( 8.379275254603339107, 1362.454991452494141, 210.6218459616987957 ) ) ;
#67542 = CARTESIAN_POINT ( 'NONE',  ( -18.89431622735909855, 1483.154720315450049, 218.3089724768730093 ) ) ;
#67544 = ORIENTED_EDGE ( 'NONE', *, *, #78365, .F. ) ;
#67543 = CARTESIAN_POINT ( 'NONE',  ( -6.317740384107130598E-10, 1416.973155798829794, 237.0820494564949854 ) ) ;
#67545 = ORIENTED_EDGE ( 'NONE', *, *, #27065, .T. ) ;
#67546 = CARTESIAN_POINT ( 'NONE',  ( -32.38114538885259464, 1523.604703353109699, 202.1233279672532888 ) ) ;
#67547 = CARTESIAN_POINT ( 'NONE',  ( 7.509820308583667448, 1510.675349056233244, 203.1409315813798173 ) ) ;
#67548 = CARTESIAN_POINT ( 'NONE',  ( -4.101685208650000192, 1471.292125227329961, 269.3367844517979961 ) ) ;
#67549 = CARTESIAN_POINT ( 'NONE',  ( 11.87563351815570023, 1433.006677199550040, 147.6591432317509884 ) ) ;
#67550 = CARTESIAN_POINT ( 'NONE',  ( -130.6584559203110416, 1340.114449826970940, 321.4803018775702412 ) ) ;
#67551 = CARTESIAN_POINT ( 'NONE',  ( 19.67658020740000069, 1453.313060387329870, 209.1218459613160121 ) ) ;
#67552 = CARTESIAN_POINT ( 'NONE',  ( -7.963748113860001254, 1384.780449526809889, 199.4915856325789889 ) ) ;
#67553 =( NAMED_UNIT ( * ) PLANE_ANGLE_UNIT ( ) SI_UNIT ( $, .RADIAN. ) );
#67554 = CARTESIAN_POINT ( 'NONE',  ( -21.62349440730000083, 1475.513060387329915, 208.1442046935659960 ) ) ;
#67555 = CARTESIAN_POINT ( 'NONE',  ( 5.215187551879999717, 1368.779556716650177, 207.6218459616989946 ) ) ;
#67556 = CARTESIAN_POINT ( 'NONE',  ( -8.992323206176040529, 1449.218714500919987, 210.9227175850809886 ) ) ;
#67557 = CARTESIAN_POINT ( 'NONE',  ( -15.46812277936250091, 1408.003561489749927, 268.9519026408210038 ) ) ;
#67558 = CARTESIAN_POINT ( 'NONE',  ( -13.51745720335679835, 1434.977168586970038, 149.1397909361569987 ) ) ;
#67559 = ORIENTED_EDGE ( 'NONE', *, *, #103432, .T. ) ;
#67560 = CARTESIAN_POINT ( 'NONE',  ( -4.327051608332210364, 1515.156337024050117, 209.3139746709489941 ) ) ;
#67561 = ORIENTED_EDGE ( 'NONE', *, *, #65318, .T. ) ;
#67562 = TOROIDAL_SURFACE ( 'NONE', #60443, 1.000000000000000000, 1.000000000000000000 ) ;
#67563 = ORIENTED_EDGE ( 'NONE', *, *, #74939, .T. ) ;
#67564 = CARTESIAN_POINT ( 'NONE',  ( -21.99231067425982999, 1506.446781340468078, 209.3764100870739355 ) ) ;
#67565 = CARTESIAN_POINT ( 'NONE',  ( -5.551188713984379852, 1510.480349263560129, 201.5713426139130320 ) ) ;
#67566 = CARTESIAN_POINT ( 'NONE',  ( 3.460101851884999746, 1516.812923327049930, 213.1504765548870068 ) ) ;
#67567 = CARTESIAN_POINT ( 'NONE',  ( -19.10795447410000136, 1485.490635589229896, 189.6432606092980109 ) ) ;
#67568 = AXIS2_PLACEMENT_3D ( 'NONE', #79770, #55129, #36105 ) ;
#67569 = CARTESIAN_POINT ( 'NONE',  ( -16.98603930835629683, 1470.451025123820045, 228.5667710449559991 ) ) ;
#67570 = VERTEX_POINT ( 'NONE', #36242 ) ;
#67571 = CYLINDRICAL_SURFACE ( 'NONE', #70761, 1.999999999999996225 ) ;
#67572 = VECTOR ( 'NONE', #69769, 1000.000000000000000 ) ;
#67573 = CARTESIAN_POINT ( 'NONE',  ( -1.130607502004999931, 1516.632821972880038, 202.5736453444569918 ) ) ;
#67574 = CARTESIAN_POINT ( 'NONE',  ( -28.75306173559999579, 1509.589359939629958, 208.3584206130200016 ) ) ;
#67575 = CARTESIAN_POINT ( 'NONE',  ( 11.60004869885204570, 1426.273943615695998, 138.2686089212693332 ) ) ;
#67576 = CARTESIAN_POINT ( 'NONE',  ( -45.63678974650149911, 1384.601836401760011, 219.1382722429960097 ) ) ;
#67577 = CARTESIAN_POINT ( 'NONE',  ( -14.51138743262410102, 1379.682357218360039, 208.2400043102109919 ) ) ;
#67578 = CARTESIAN_POINT ( 'NONE',  ( -108.6463189709999995, 1386.108622646309868, 311.0727272582590217 ) ) ;
#67580 = ORIENTED_EDGE ( 'NONE', *, *, #101696, .T. ) ;
#67579 = CARTESIAN_POINT ( 'NONE',  ( 22.08327125186925954, 1523.604703353109699, 184.4267662568470598 ) ) ;
#67581 = CARTESIAN_POINT ( 'NONE',  ( -26.85728217208029989, 1488.762426835850192, 210.5633333958139701 ) ) ;
#67582 = CARTESIAN_POINT ( 'NONE',  ( 26.47779523700000226, 1469.247571737029830, 210.0128041243490031 ) ) ;
#67583 = CARTESIAN_POINT ( 'NONE',  ( -55.83192871552868297, 1379.712800777655048, 257.4612982601994986 ) ) ;
#67584 = CARTESIAN_POINT ( 'NONE',  ( 10.74646275119079952, 1460.429788200699704, 207.1630952569950068 ) ) ;
#67585 = CARTESIAN_POINT ( 'NONE',  ( -13.24677860586930045, 1436.091658137889908, 150.6304371349799851 ) ) ;
#67586 = CARTESIAN_POINT ( 'NONE',  ( -24.47138174589999693, 1442.190446117989950, 211.0555081549980230 ) ) ;
#67587 = CARTESIAN_POINT ( 'NONE',  ( 1.136547584984999970, 1516.839862955080207, 211.5998212856970042 ) ) ;
#67588 = CARTESIAN_POINT ( 'NONE',  ( -68.71298160489999418, 1379.747970726529957, 280.0474361183589735 ) ) ;
#67589 = CARTESIAN_POINT ( 'NONE',  ( -4.869818399669999742, 1491.215867106689984, 188.8099941780989752 ) ) ;
#67590 = CARTESIAN_POINT ( 'NONE',  ( -18.31482527320000031, 1445.278739201789904, 204.5307550449689984 ) ) ;
#67591 = CARTESIAN_POINT ( 'NONE',  ( -12.98226561589999939, 1414.913060387329779, 219.9156672276980089 ) ) ;
#67592 = CARTESIAN_POINT ( 'NONE',  ( -4.625790014595000166, 1517.104192383289956, 208.0004623403669939 ) ) ;
#67593 = ORIENTED_EDGE ( 'NONE', *, *, #52472, .T. ) ;
#67594 = DIRECTION ( 'NONE',  ( 6.546194519182246997E-06, 0.000000000000000000, 0.9999999999785736948 ) ) ;
#67595 = CARTESIAN_POINT ( 'NONE',  ( -10.30262272859999939, 1471.797637931690133, 208.8808052225769814 ) ) ;
#67596 = DIRECTION ( 'NONE',  ( -3.334807482003173289E-08, 5.770116306383727380E-11, -0.9999999999999995559 ) ) ;
#67597 = EDGE_LOOP ( 'NONE', ( #39640, #67974, #22588, #82759, #88451, #72120 ) ) ;
#67598 = CARTESIAN_POINT ( 'NONE',  ( -3.258294392304168507, 1524.756004293092474, 241.7666560717732978 ) ) ;
#67599 = CARTESIAN_POINT ( 'NONE',  ( 12.74071504291650037, 1434.633262964860023, 149.4353413572609952 ) ) ;
#67600 = CARTESIAN_POINT ( 'NONE',  ( 17.21575504016569980, 1459.307510025329975, 228.5504449505849891 ) ) ;
#67601 = CARTESIAN_POINT ( 'NONE',  ( -12.14128143079999944, 1416.006154796849842, 206.7539641484389961 ) ) ;
#67602 = CARTESIAN_POINT ( 'NONE',  ( 26.07120187149999779, 1452.002625937929906, 135.0137028555979839 ) ) ;
#67603 = CARTESIAN_POINT ( 'NONE',  ( 5.653236855950000361, 1487.809232560990040, 198.9822455535989718 ) ) ;
#67604 = DIRECTION ( 'NONE',  ( -0.000000000000000000, -1.000000000000000000, -0.000000000000000000 ) ) ;
#67605 = CARTESIAN_POINT ( 'NONE',  ( -11.60674135321730027, 1507.508082919659955, 207.5537295141489835 ) ) ;
#67606 = CIRCLE ( 'NONE', #53309, 29.83173541461230727 ) ;
#67608 = FACE_OUTER_BOUND ( 'NONE', #43731, .T. ) ;
#67607 = CARTESIAN_POINT ( 'NONE',  ( -7.324914956285000223, 1516.685667699390024, 213.7393364370070117 ) ) ;
#67609 = CARTESIAN_POINT ( 'NONE',  ( -8.878224064888490474, 1385.253402910369914, 218.6672395676210101 ) ) ;
#67610 = CARTESIAN_POINT ( 'NONE',  ( -4.033653302454999867, 1517.028034847769959, 215.6825881955670070 ) ) ;
#67611 = EDGE_LOOP ( 'NONE', ( #9543, #27353, #6216, #72255, #19484 ) ) ;
#67612 = CARTESIAN_POINT ( 'NONE',  ( 1.582067810090000045E-15, 1508.551704408389924, 209.1218459616989946 ) ) ;
#67613 = CARTESIAN_POINT ( 'NONE',  ( -17.02334047809999973, 1420.318775465339968, 203.7071964112190017 ) ) ;
#67614 = ORIENTED_EDGE ( 'NONE', *, *, #100669, .F. ) ;
#67615 = CARTESIAN_POINT ( 'NONE',  ( -18.17086109458769982, 1508.551704408389924, 210.8151139196999679 ) ) ;
#67616 = ADVANCED_FACE ( 'NONE', ( #1551 ), #95594, .F. ) ;
#67617 = DIRECTION ( 'NONE',  ( 0.000000000000000000, 0.000000000000000000, 1.000000000000000000 ) ) ;
#67618 = CARTESIAN_POINT ( 'NONE',  ( -29.40443212115401650, 1511.187213306747708, 196.1539082851718661 ) ) ;
#67619 = CARTESIAN_POINT ( 'NONE',  ( -0.4696341913122200062, 1423.394439732270030, 191.2019798439270062 ) ) ;
#67620 = CARTESIAN_POINT ( 'NONE',  ( -7.756928808066270165, 1508.430203411700177, 219.4938965895260026 ) ) ;
#67621 = CARTESIAN_POINT ( 'NONE',  ( 17.41395121031547788, 1422.770471704767260, 226.5406294010037413 ) ) ;
#67622 = DIRECTION ( 'NONE',  ( 0.000000000000000000, -1.000000000000000000, 0.000000000000000000 ) ) ;
#67623 = DIRECTION ( 'NONE',  ( 1.000000000000000000, 0.000000000000000000, 0.000000000000000000 ) ) ;
#67624 = EDGE_CURVE ( 'NONE', #17762, #11785, #457, .T. ) ;
#67625 = CARTESIAN_POINT ( 'NONE',  ( -2.461716435160000049, 1435.943783413959864, 150.4083956814980070 ) ) ;
#67626 = CARTESIAN_POINT ( 'NONE',  ( 44.10764275524749678, 1440.913060362949864, 264.4775968722539687 ) ) ;
#67628 = DIRECTION ( 'NONE',  ( 1.000000000000000000, 0.000000000000000000, 0.000000000000000000 ) ) ;
#67627 = CARTESIAN_POINT ( 'NONE',  ( -12.16253720638220059, 1419.838831633310065, 197.2883658129150035 ) ) ;
#67629 = DIRECTION ( 'NONE',  ( -0.7074300732371815448, 0.02470400256250997878, 0.7063514732320074208 ) ) ;
#67630 = ORIENTED_EDGE ( 'NONE', *, *, #49168, .F. ) ;
#67632 = ORIENTED_EDGE ( 'NONE', *, *, #9021, .T. ) ;
#67631 = B_SPLINE_CURVE_WITH_KNOTS ( 'NONE', 3,
 ( #109143, #39154, #49787, #13388, #81700, #30758, #64939, #99053, #22332, #56533, #34625, #92869, #58732, #25655, #32958, #59305, #67147, #85561, #67699, #102372, #101808, #84476, #16686, #60964, #93970, #110224, #51431, #1052, #76628, #18356, #41382, #50883, #76086, #93419 ),
 .UNSPECIFIED., .F., .F.,
 ( 4, 3, 3, 3, 3, 3, 3, 3, 3, 3, 3, 4 ),
 ( -2.000000000000000000, -1.872087319251769966, -1.687892984705650079, -1.501460662300799997, -1.313840537329579838, -1.124757636572869979, -0.9352500492189879111, -0.7457836696873179072, -0.5568196230199600194, -0.3695388451267069829, -0.1838439808487151161, 0.000000000000000000 ),
 .UNSPECIFIED. ) ;
#67633 = CARTESIAN_POINT ( 'NONE',  ( -4.318206861440000210, 1497.528676090189947, 220.7835062296990145 ) ) ;
#67634 = AXIS2_PLACEMENT_3D ( 'NONE', #57026, #61716, #95838 ) ;
#67635 = CARTESIAN_POINT ( 'NONE',  ( -18.22821675530000007, 1443.229620277490085, 204.5519556382290034 ) ) ;
#67636 = CARTESIAN_POINT ( 'NONE',  ( -29.15071157469999719, 1509.931025666729965, 211.8621304569779795 ) ) ;
#67637 = CARTESIAN_POINT ( 'NONE',  ( 2.352760052573430016, 1410.373437767319956, 185.5341168253151523 ) ) ;
#67638 = VECTOR ( 'NONE', #86924, 1000.000000000000000 ) ;
#67639 = CARTESIAN_POINT ( 'NONE',  ( 11.78238356083980065, 1440.882651838439870, 188.1224447589279976 ) ) ;
#67640 = CARTESIAN_POINT ( 'NONE',  ( 10.08036567563580199, 1422.462408472209972, 212.0547761052640112 ) ) ;
#67641 = CIRCLE ( 'NONE', #92631, 1.999999999999999556 ) ;
#67642 = B_SPLINE_CURVE_WITH_KNOTS ( 'NONE', 3,
 ( #67077, #93892, #101181, #41848, #83849, #41305, #75478, #109611, #24476, #16072, #58664, #50274, #84404, #76003, #33426, #25025, #59227 ),
 .UNSPECIFIED., .F., .F.,
 ( 4, 2, 2, 1, 1, 1, 2, 2, 2, 4 ),
 ( 0.000000000000000000, 0.2499999999972815079, 0.3749999999959241492, 0.4374999999953910201, 0.4687499999951194596, 0.4843749999949900076, 0.4921874999949239493, 0.4999999999948580021, 0.7499999999974289455, 1.000000000000000000 ),
 .UNSPECIFIED. ) ;
#67643 = DIRECTION ( 'NONE',  ( 0.6709778558543728622, 0.000000000000000000, 0.7414773880254666993 ) ) ;
#67644 = CARTESIAN_POINT ( 'NONE',  ( 18.94656048379999902, 1455.761273475090093, 200.3458234316790083 ) ) ;
#67645 = CARTESIAN_POINT ( 'NONE',  ( -56.77970903073529740, 1383.801243860249997, 274.8410118865560321 ) ) ;
#67646 = CIRCLE ( 'NONE', #92715, 3.000000000000002665 ) ;
#67647 = CARTESIAN_POINT ( 'NONE',  ( 24.18195368869999839, 1450.840504138970118, 140.0925686386979976 ) ) ;
#67648 = CARTESIAN_POINT ( 'NONE',  ( -27.12970500513406336, 1508.933968740432874, 212.0467364469421909 ) ) ;
#67649 = CARTESIAN_POINT ( 'NONE',  ( 10.54079341922740021, 1491.061758365090100, 212.2573636860299757 ) ) ;
#67651 = ORIENTED_EDGE ( 'NONE', *, *, #80204, .T. ) ;
#67650 = FACE_OUTER_BOUND ( 'NONE', #81033, .T. ) ;
#67652 = CARTESIAN_POINT ( 'NONE',  ( 32.92528853941223588, 1523.611961620354123, 217.2368972417801558 ) ) ;
#67653 = CARTESIAN_POINT ( 'NONE',  ( -61.45879576459999782, 1381.674944668329999, 249.7621233603589985 ) ) ;
#67654 = CARTESIAN_POINT ( 'NONE',  ( -16.38529656942809964, 1409.485247551910106, 224.6959546567310042 ) ) ;
#67655 = VERTEX_POINT ( 'NONE', #69874 ) ;
#67656 = VERTEX_POINT ( 'NONE', #86090 ) ;
#67657 = CARTESIAN_POINT ( 'NONE',  ( -4.993214567250789493, 1391.653935164599716, 214.7089805434449943 ) ) ;
#67658 = CARTESIAN_POINT ( 'NONE',  ( -8.170894480889998590, 1500.638869073389969, 209.8833235920569962 ) ) ;
#67659 = CARTESIAN_POINT ( 'NONE',  ( 40.09667693707910274, 1442.092650259239917, 136.9432980588629789 ) ) ;
#67661 = CARTESIAN_POINT ( 'NONE',  ( 1.682318894840000079, 1409.475163267829885, 232.0401757884979759 ) ) ;
#67660 = LINE ( 'NONE', #100672, #17396 ) ;
#67662 = CARTESIAN_POINT ( 'NONE',  ( -10.28857233090000101, 1463.185141274090256, 204.9217573806190273 ) ) ;
#67663 = CARTESIAN_POINT ( 'NONE',  ( -108.8778232199999962, 1382.941140509790102, 297.5244794079590065 ) ) ;
#67664 = FACE_OUTER_BOUND ( 'NONE', #82301, .T. ) ;
#67665 = DIRECTION ( 'NONE',  ( -1.305148739725796033E-31, 1.000000000000000000, -1.836970198721029688E-16 ) ) ;
#67666 = CARTESIAN_POINT ( 'NONE',  ( -11.35885305070239859, 1508.551704408389924, 217.6084463250130057 ) ) ;
#67667 = VECTOR ( 'NONE', #490, 1000.000000000000000 ) ;
#67668 = CARTESIAN_POINT ( 'NONE',  ( 3.642177762369999794, 1409.207669089330011, 186.4969686919980063 ) ) ;
#67669 = CARTESIAN_POINT ( 'NONE',  ( -1.553759244419499863, 1485.745504604600001, 197.3241831226270051 ) ) ;
#67670 = CARTESIAN_POINT ( 'NONE',  ( -2.130922739038390024, 1467.954349360780043, 220.0452206896550251 ) ) ;
#67671 = CARTESIAN_POINT ( 'NONE',  ( 11.86614525289999911, 1432.349253981680022, 150.3971727848980038 ) ) ;
#67672 = CARTESIAN_POINT ( 'NONE',  ( -22.65242742670000098, 1452.122020190730154, 139.7531684575980080 ) ) ;
#67673 = CARTESIAN_POINT ( 'NONE',  ( 0.2762028305379999882, 1466.385324525529995, 235.6853349533979838 ) ) ;
#67674 = ORIENTED_EDGE ( 'NONE', *, *, #50282, .T. ) ;
#67676 = CARTESIAN_POINT ( 'NONE',  ( 20.53971479803719902, 1476.913985495619954, 217.7491938173760104 ) ) ;
#67675 = B_SPLINE_CURVE_WITH_KNOTS ( 'NONE', 5,
 ( #39391, #30984, #31534, #97648, #73006, #55668 ),
 .UNSPECIFIED., .F., .F.,
 ( 6, 6 ),
 ( 0.000000000000000000, 1.000000000000000000 ),
 .UNSPECIFIED. ) ;
#67677 = CARTESIAN_POINT ( 'NONE',  ( -2.409586283469999923, 1426.663880916129983, 144.1938086916980239 ) ) ;
#67678 = CARTESIAN_POINT ( 'NONE',  ( -27.74152896854549866, 1446.393007474169963, 137.1637341980870133 ) ) ;
#67679 = DIRECTION ( 'NONE',  ( 0.000000000000000000, 0.000000000000000000, 1.000000000000000000 ) ) ;
#67680 = CARTESIAN_POINT ( 'NONE',  ( 17.14891132210000180, 1507.633349707429943, 188.2623345620979762 ) ) ;
#67681 = CARTESIAN_POINT ( 'NONE',  ( -7.045284513412829670E-09, 1472.436258976460067, 259.9932842362949827 ) ) ;
#67682 = CARTESIAN_POINT ( 'NONE',  ( -20.00399723164029808, 1488.559828140339960, 190.9486810803579999 ) ) ;
#67683 = CARTESIAN_POINT ( 'NONE',  ( -11.96878399062378939, 1507.593741241288626, 208.5523078659349494 ) ) ;
#67684 = CARTESIAN_POINT ( 'NONE',  ( -0.4967073768120000010, 1415.438070335630073, 233.3911243366979988 ) ) ;
#67685 = CARTESIAN_POINT ( 'NONE',  ( 0.2414385729460010177, 1476.817046155289972, 198.6010158731990032 ) ) ;
#67686 = CARTESIAN_POINT ( 'NONE',  ( -108.0873157920000125, 1388.188583901430093, 310.1965002822589668 ) ) ;
#67687 = CARTESIAN_POINT ( 'NONE',  ( -8.490445737682099647, 1511.451733153379791, 214.5038762997880042 ) ) ;
#67688 = CARTESIAN_POINT ( 'NONE',  ( -5.986709854327127545, 1361.264879806976069, 210.6218459616991936 ) ) ;
#67689 = CARTESIAN_POINT ( 'NONE',  ( -45.97429859279590403, 1438.843789423260205, 266.6795026073090185 ) ) ;
#67690 = CARTESIAN_POINT ( 'NONE',  ( 3.260623164134589747, 1428.697964756740021, 216.7257091047359836 ) ) ;
#67691 = CARTESIAN_POINT ( 'NONE',  ( -7.885009387709999373, 1425.368775642419905, 206.6265662114490169 ) ) ;
#67692 = CARTESIAN_POINT ( 'NONE',  ( 5.006259848694999626, 1516.939723362869927, 209.1089481433290018 ) ) ;
#67693 = FACE_OUTER_BOUND ( 'NONE', #5998, .T. ) ;
#67694 = DIRECTION ( 'NONE',  ( 0.000000000000000000, 1.000000000000000000, 0.000000000000000000 ) ) ;
#67695 = CARTESIAN_POINT ( 'NONE',  ( 7.446545243910679623, 1426.150453638759927, 212.4588778087180003 ) ) ;
#67696 = CARTESIAN_POINT ( 'NONE',  ( -26.72416512552139878, 1451.509345559029953, 136.0758556284789904 ) ) ;
#67697 = ORIENTED_EDGE ( 'NONE', *, *, #11192, .F. ) ;
#67698 = CARTESIAN_POINT ( 'NONE',  ( 24.66839858290000009, 1432.416040610029995, 225.6916884349980137 ) ) ;
#67700 = CARTESIAN_POINT ( 'NONE',  ( 15.39496762990000001, 1488.801231227030030, 194.1127781847980032 ) ) ;
#67699 = CARTESIAN_POINT ( 'NONE',  ( -11.14769255285479943, 1491.958836887719826, 207.0420635619269945 ) ) ;
#67701 = CARTESIAN_POINT ( 'NONE',  ( 12.67629937430701936, 1426.478869958664063, 202.7079000866955028 ) ) ;
#67702 = CARTESIAN_POINT ( 'NONE',  ( -19.16951723229999871, 1456.627470220629903, 228.8719212425980061 ) ) ;
#67703 = CARTESIAN_POINT ( 'NONE',  ( 8.935942533379998665, 1425.567594377970181, 193.3040559142989991 ) ) ;
#67704 = CARTESIAN_POINT ( 'NONE',  ( -23.84533141485470153, 1452.080363065020038, 136.9869391916130041 ) ) ;
#67705 = CARTESIAN_POINT ( 'NONE',  ( -9794.298952052929963, 2837.541834147239570, -1088.485032349865833 ) ) ;
#67706 = ORIENTED_EDGE ( 'NONE', *, *, #6266, .T. ) ;
#67707 = CARTESIAN_POINT ( 'NONE',  ( -0.6132286398022869234, 1408.236656115740061, 270.3925693042170337 ) ) ;
#67708 = CARTESIAN_POINT ( 'NONE',  ( 10.54373566122539962, 1419.511555201090005, 230.6885890306220119 ) ) ;
#67709 = CARTESIAN_POINT ( 'NONE',  ( 8.909790489964100502, 1434.607596429470050, 206.3238506486309802 ) ) ;
#67710 = ORIENTED_EDGE ( 'NONE', *, *, #66055, .F. ) ;
#67711 = ORIENTED_EDGE ( 'NONE', *, *, #97988, .T. ) ;
#67712 = CARTESIAN_POINT ( 'NONE',  ( -22.73045215911909978, 1409.706683828489986, 209.4201699003199906 ) ) ;
#67713 = ORIENTED_EDGE ( 'NONE', *, *, #11712, .F. ) ;
#67714 = DIRECTION ( 'NONE',  ( -2.513978196838388281E-18, -0.7071067811865475727, -0.7071067811865475727 ) ) ;
#67715 = CARTESIAN_POINT ( 'NONE',  ( -6.742596065479999901, 1428.329919402730184, 101.8807690336980016 ) ) ;
#67716 = AXIS2_PLACEMENT_3D ( 'NONE', #48409, #6932, #23727 ) ;
#67717 = TOROIDAL_SURFACE ( 'NONE', #30121, 32.13701971169416538, 1.000000000000000000 ) ;
#67718 = CARTESIAN_POINT ( 'NONE',  ( -18.78618306029910201, 1416.259629939410161, 207.5733126889130062 ) ) ;
#67719 = CARTESIAN_POINT ( 'NONE',  ( 4.303242241110600830, 1508.728291974460035, 212.9101315294259678 ) ) ;
#67720 = CIRCLE ( 'NONE', #40924, 0.5866484772300107897 ) ;
#67721 = CARTESIAN_POINT ( 'NONE',  ( 22.61737647487870007, 1471.968567494569925, 267.6424710453320017 ) ) ;
#67722 = CARTESIAN_POINT ( 'NONE',  ( -10.68745674553450087, 1391.913060387239966, 205.2244091230350023 ) ) ;
#67723 = CARTESIAN_POINT ( 'NONE',  ( -17.15598988914259238, 1422.277001189961311, 226.7238155055327411 ) ) ;
#67724 =( BOUNDED_SURFACE ( )  B_SPLINE_SURFACE ( 3, 2, ( 
 ( #62774, #96889, #20159 ),
 ( #13954, #107472, #15593 ),
 ( #64949, #91230, #15051 ),
 ( #22895, #14510, #16156 ) ),
 .UNSPECIFIED., .F., .F., .F. ) 
 B_SPLINE_SURFACE_WITH_KNOTS ( ( 4, 4 ),
 ( 3, 3 ),
 ( 0.000000000000000000, 0.0002960034161023842431 ),
 ( 0.000000000000000000, 1.000000000000000000 ),
 .UNSPECIFIED. ) 
 GEOMETRIC_REPRESENTATION_ITEM ( )  RATIONAL_B_SPLINE_SURFACE ( (
 ( 1.000000000000000000, 0.8072480644198088973, 1.000000000000000000),
 ( 1.000000000000000000, 0.8072480346917659810, 1.000000000000000000),
 ( 1.000000000000000000, 0.8071723757218326467, 1.000000000000000000),
 ( 1.000000000000000000, 0.8070209408750008695, 1.000000000000000000) ) ) 
 REPRESENTATION_ITEM ( '' )  SURFACE ( )  );
#67725 = CARTESIAN_POINT ( 'NONE',  ( -5.009478105444999940, 1516.886345593249871, 204.5093386581970094 ) ) ;
#67726 = ORIENTED_EDGE ( 'NONE', *, *, #100830, .F. ) ;
#67727 = CARTESIAN_POINT ( 'NONE',  ( 18.34455336298703543, 1459.088291602529353, 227.7786510797382959 ) ) ;
#67728 = CARTESIAN_POINT ( 'NONE',  ( 15.06905040192160072, 1513.645442088320124, 194.5599833342589875 ) ) ;
#67729 = CARTESIAN_POINT ( 'NONE',  ( 31.23437356469446868, 1512.187213306747481, 222.8968241038843701 ) ) ;
#67730 = ORIENTED_EDGE ( 'NONE', *, *, #70167, .T. ) ;
#67731 = CARTESIAN_POINT ( 'NONE',  ( -10.44591860737159905, 1479.590090999679887, 210.1597183799869697 ) ) ;
#67732 = CARTESIAN_POINT ( 'NONE',  ( 26.92792935968680013, 1450.870610057039812, 136.4174504459710136 ) ) ;
#67733 = CARTESIAN_POINT ( 'NONE',  ( -14.86941682237170070, 1514.013728164699842, 194.2615873074070123 ) ) ;
#67734 = CARTESIAN_POINT ( 'NONE',  ( -1.546867746862319981, 1416.839692133689823, 228.0214409764060122 ) ) ;
#67735 = CARTESIAN_POINT ( 'NONE',  ( 7.573774609450000028, 1421.897575251010039, 195.7040863559990100 ) ) ;
#67736 = CARTESIAN_POINT ( 'NONE',  ( -2.557552783909830207, 1432.931063180149977, 218.3108672520129971 ) ) ;
#67737 = CARTESIAN_POINT ( 'NONE',  ( -4.311223378659999383, 1495.728807022490173, 198.3651121709989980 ) ) ;
#67738 = CARTESIAN_POINT ( 'NONE',  ( 1.185993768368289958, 1408.954476202319938, 186.7131526092149727 ) ) ;
#67740 = DIRECTION ( 'NONE',  ( -0.000000000000000000, -1.000000000000000000, -0.000000000000000000 ) ) ;
#67739 = CARTESIAN_POINT ( 'NONE',  ( 2.004290588779999993, 1417.602443405030044, 234.4383503574979954 ) ) ;
#67741 = CIRCLE ( 'NONE', #23022, 1.999999999999998668 ) ;
#67742 = CARTESIAN_POINT ( 'NONE',  ( -11.23128131019999998, 1378.642388353129945, 214.2935887347389894 ) ) ;
#67743 = CARTESIAN_POINT ( 'NONE',  ( 3.143095077906818524, 1525.137881624898682, 241.5427404054744329 ) ) ;
#67744 = ORIENTED_EDGE ( 'NONE', *, *, #15362, .T. ) ;
#67745 = CARTESIAN_POINT ( 'NONE',  ( 12.74994028582560013, 1415.933499560010205, 221.6250176366550022 ) ) ;
#67746 = FACE_OUTER_BOUND ( 'NONE', #39856, .T. ) ;
#67747 = CARTESIAN_POINT ( 'NONE',  ( -11.05503427808429961, 1483.026236761159907, 204.6865788484709867 ) ) ;
#67748 = CARTESIAN_POINT ( 'NONE',  ( -14.02793429120000113, 1390.368118300530114, 208.3706668749019855 ) ) ;
#67749 = CARTESIAN_POINT ( 'NONE',  ( 9.104124838956808574, 1427.252791609349742, 211.0639582536120145 ) ) ;
#67750 = CARTESIAN_POINT ( 'NONE',  ( 12.18334191729579885, 1421.374448972539994, 203.4336414120620020 ) ) ;
#67751 = CARTESIAN_POINT ( 'NONE',  ( 13.08154635940000077, 1418.696939362130024, 221.6904558216980092 ) ) ;
#67752 = CARTESIAN_POINT ( 'NONE',  ( -6.438546668579999910, 1470.874276671330108, 268.3665355204980187 ) ) ;
#67753 = CARTESIAN_POINT ( 'NONE',  ( -8.860697296614830520, 1384.856270409599801, 218.6846939278150046 ) ) ;
#67754 = CARTESIAN_POINT ( 'NONE',  ( 11.47665303230000156, 1433.538822946230084, 151.3125183399980074 ) ) ;
#67755 = CARTESIAN_POINT ( 'NONE',  ( 3.444929440920000197, 1456.909266848530024, 224.8635561966979708 ) ) ;
#67756 = CARTESIAN_POINT ( 'NONE',  ( 12.45618235599049939, 1416.218047878440075, 196.1634418539379965 ) ) ;
#67757 = CARTESIAN_POINT ( 'NONE',  ( -29.71163624023799343, 1526.333389947990554, 201.1407003069400048 ) ) ;
#67758 = CARTESIAN_POINT ( 'NONE',  ( -7.769784805680000517, 1383.283764732429972, 218.8591787099389876 ) ) ;
#67759 = CARTESIAN_POINT ( 'NONE',  ( 4.653685083909150144, 1466.070315411240017, 218.6935422048629789 ) ) ;
#67760 = CARTESIAN_POINT ( 'NONE',  ( 14.44303130513500122, 1516.995662938509895, 192.4521789031669812 ) ) ;
#67761 = FACE_OUTER_BOUND ( 'NONE', #101979, .T. ) ;
#67762 = CARTESIAN_POINT ( 'NONE',  ( -28.08216322107800167, 1509.932735855700003, 222.4427074788879963 ) ) ;
#67763 = AXIS2_PLACEMENT_3D ( 'NONE', #11529, #63075, #2043 ) ;
#67764 = CARTESIAN_POINT ( 'NONE',  ( 24.22746707339999972, 1430.355866414130105, 212.3409394264880063 ) ) ;
#67765 = CARTESIAN_POINT ( 'NONE',  ( 0.3646030894699989755, 1473.314417745290257, 216.5794721063890051 ) ) ;
#67766 = CARTESIAN_POINT ( 'NONE',  ( 26.79413740735880367, 1436.761939593030093, 136.7822073642480234 ) ) ;
#67767 = CARTESIAN_POINT ( 'NONE',  ( -17.22212745223800212, 1383.856419954710191, 219.8022064494420249 ) ) ;
#67768 = CARTESIAN_POINT ( 'NONE',  ( 12.70693932329499809, 1426.829486560239957, 205.0434112651460055 ) ) ;
#67769 = CARTESIAN_POINT ( 'NONE',  ( -9.838224544249689174, 1462.268909281400056, 227.9668214889109947 ) ) ;
#67770 = CARTESIAN_POINT ( 'NONE',  ( 2.298048923505000118, 1516.764084769670262, 212.5672535042169784 ) ) ;
#67771 = CARTESIAN_POINT ( 'NONE',  ( -18.45566820803939834, 1419.316056982640021, 207.4717884025210139 ) ) ;
#67772 = CARTESIAN_POINT ( 'NONE',  ( 0.2069650299334150068, 1459.057086511930038, 182.9935364721550002 ) ) ;
#67774 = ORIENTED_EDGE ( 'NONE', *, *, #61954, .T. ) ;
#67773 = CARTESIAN_POINT ( 'NONE',  ( -31.81407709660760830, 1522.382868172863937, 221.9534378623334590 ) ) ;
#67775 = CARTESIAN_POINT ( 'NONE',  ( 1.800936940629440430, 1526.306647125542668, 178.3505287518698026 ) ) ;
#67776 = AXIS2_PLACEMENT_3D ( 'NONE', #43021, #49770, #34052 ) ;
#67777 = CARTESIAN_POINT ( 'NONE',  ( 10.10004869885203682, 0.000000000000000000, 135.5999999980979851 ) ) ;
#67778 = CARTESIAN_POINT ( 'NONE',  ( 12.91282902989999926, 1434.774388673019985, 149.7891053277979836 ) ) ;
#67779 = CARTESIAN_POINT ( 'NONE',  ( -41.28347186119889756, 1446.141341654479902, 134.0999999985599800 ) ) ;
#67780 = CARTESIAN_POINT ( 'NONE',  ( -109.8954864790000130, 1384.895399018540047, 297.0284339997589882 ) ) ;
#67781 = ORIENTED_EDGE ( 'NONE', *, *, #95252, .T. ) ;
#67782 = B_SPLINE_SURFACE_WITH_KNOTS ( 'NONE', 5, 5, ( 
 ( #49214, #22304, #22861, #4449, #6638, #40793, #6087, #97930, #90635 ),
 ( #65470, #74970, #40238, #73302, #90078, #91194, #39694, #99578, #14474 ),
 ( #48102, #38576, #82242, #21198, #13360, #89539, #81133, #81672, #39122 ),
 ( #107436, #73861, #107989, #31285, #102341, #83894, #34596, #102881, #51400 ),
 ( #7199, #26179, #66580, #41355, #85532, #59818, #50854, #15563, #77713 ),
 ( #75523, #33472, #8827, #100684, #9399, #110752, #23968, #101779, #109656 ) ),
 .UNSPECIFIED., .F., .F., .F.,
 ( 6, 6 ),
 ( 6, 3, 6 ),
 ( 7.509787108449399895, 11.13865211956250079 ),
 ( -3.527284231174740019E-05, 1.000000000000000000, 2.000000000000000000 ),
 .UNSPECIFIED. ) ;
#67783 = CARTESIAN_POINT ( 'NONE',  ( -11.39446584399999907, 1470.674086033289996, 209.5209555135179755 ) ) ;
#67784 = CARTESIAN_POINT ( 'NONE',  ( 2.621078202466677443, 1523.542365884047285, 176.0837307636417393 ) ) ;
#67785 = CARTESIAN_POINT ( 'NONE',  ( 9.146237114798470458, 1449.998848199699978, 208.1168068718100130 ) ) ;
#67786 = CARTESIAN_POINT ( 'NONE',  ( -17.71193100849139768, 1519.551704408389924, 221.5709757781449980 ) ) ;
#67787 = EDGE_CURVE ( 'NONE', #31041, #43965, #12918, .T. ) ;
#67788 = CARTESIAN_POINT ( 'NONE',  ( -6.865221456288480795, 1434.987526699120053, 214.6275269604420259 ) ) ;
#67789 = CARTESIAN_POINT ( 'NONE',  ( -2.021663551027474082, 1408.983658434181052, 187.9413203637166987 ) ) ;
#67790 = AXIS2_PLACEMENT_3D ( 'NONE', #4809, #80979, #98320 ) ;
#67791 = CARTESIAN_POINT ( 'NONE',  ( -15.68237649659999811, 1416.893877491339936, 210.3432287165989862 ) ) ;
#67792 = CARTESIAN_POINT ( 'NONE',  ( -5.367207161296789764, 1422.334098476926783, 140.1444612193151897 ) ) ;
#67793 = CARTESIAN_POINT ( 'NONE',  ( -12.23230767969999810, 1391.519584735709941, 206.9802348098490086 ) ) ;
#67794 = CARTESIAN_POINT ( 'NONE',  ( -81.94711355757770832, 1385.165090159550118, 285.5376096483210517 ) ) ;
#67795 = CARTESIAN_POINT ( 'NONE',  ( -10.38284638997270015, 1391.913060387289988, 213.8006219875449858 ) ) ;
#67796 = CARTESIAN_POINT ( 'NONE',  ( 12.45038714344340036, 1421.619513592610019, 207.5027818182680051 ) ) ;
#67797 = ORIENTED_EDGE ( 'NONE', *, *, #92401, .F. ) ;
#67798 = AXIS2_PLACEMENT_3D ( 'NONE', #103526, #44198, #28490 ) ;
#67799 = CARTESIAN_POINT ( 'NONE',  ( -33.92643244749999809, 1451.728353150429939, 135.1493689542980121 ) ) ;
#67800 = CARTESIAN_POINT ( 'NONE',  ( 13.51610093809999924, 1443.501467202829872, 169.3501091259980171 ) ) ;
#67802 = VERTEX_POINT ( 'NONE', #21067 ) ;
#67801 = CARTESIAN_POINT ( 'NONE',  ( -1.191524307911315583, 1526.382868172863937, 239.2353018730792087 ) ) ;
#67803 = CARTESIAN_POINT ( 'NONE',  ( 3.028998513489999933, 1474.332429607289896, 219.7118052044990009 ) ) ;
#67804 = CIRCLE ( 'NONE', #19493, 15.41143114519999990 ) ;
#67805 = DIRECTION ( 'NONE',  ( -0.7071068048275286344, 1.153083735983437180E-10, -0.7071067575455656229 ) ) ;
#67806 = CARTESIAN_POINT ( 'NONE',  ( -7.940496932319466517, 1364.770096069278225, 209.6218459617148824 ) ) ;
#67807 = CARTESIAN_POINT ( 'NONE',  ( -11.38768754900000069, 1491.978877293390042, 204.2815689120989759 ) ) ;
#67808 = CARTESIAN_POINT ( 'NONE',  ( -111.7097258769571368, 1305.913060387289988, 299.1967830284323782 ) ) ;
#67809 = CARTESIAN_POINT ( 'NONE',  ( 1.569161254424999985, 1517.051704408389924, 201.3992656178269840 ) ) ;
#67810 = CARTESIAN_POINT ( 'NONE',  ( 16.64291266002331326, 1432.692105207829854, 217.7214433012767358 ) ) ;
#67811 = CARTESIAN_POINT ( 'NONE',  ( 1.707043585809999930, 1416.544879546130005, 232.5604860032980241 ) ) ;
#67812 = CARTESIAN_POINT ( 'NONE',  ( 2.500000000000000000, 1431.405490181040022, 183.1416673786320075 ) ) ;
#67813 = DIRECTION ( 'NONE',  ( -0.4874171250595387694, 0.8731692540388111823, 0.000000000000000000 ) ) ;
#67814 = CARTESIAN_POINT ( 'NONE',  ( 22.17671526344968314, 1509.715724164745325, 189.3973745417270038 ) ) ;
#67815 = CARTESIAN_POINT ( 'NONE',  ( -3.271538066909999820, 1454.292002242289982, 199.1638777246189989 ) ) ;
#67816 = CARTESIAN_POINT ( 'NONE',  ( 4.027697225915000345, 1516.766397346390022, 206.2431526829570032 ) ) ;
#67817 = VECTOR ( 'NONE', #95135, 1000.000000000000227 ) ;
#67818 = DIRECTION ( 'NONE',  ( 0.5877852522924673639, 0.000000000000000000, -0.8090169943749514481 ) ) ;
#67819 = B_SPLINE_SURFACE_WITH_KNOTS ( 'NONE', 5, 1, ( 
 ( #24817, #82560 ),
 ( #14785, #48416 ),
 ( #75811, #5852 ),
 ( #14228, #15324 ),
 ( #32696, #65763 ),
 ( #108300, #50609 ),
 ( #7493, #48970 ),
 ( #84741, #23178 ),
 ( #41655, #109962 ) ),
 .UNSPECIFIED., .F., .F., .F.,
 ( 6, 3, 6 ),
 ( 2, 2 ),
 ( 0.000000000000000000, 3.215063553959999876, 6.404940046369999251 ),
 ( 0.000000000000000000, 14.00000000000000000 ),
 .UNSPECIFIED. ) ;
#67820 = CARTESIAN_POINT ( 'NONE',  ( -32.15938645527118922, 1524.538768545234007, 216.1010655287031739 ) ) ;
#67821 = CARTESIAN_POINT ( 'NONE',  ( -2.699177585649999767, 1497.662919768989923, 198.1511405123989960 ) ) ;
#67823 = ORIENTED_EDGE ( 'NONE', *, *, #21553, .F. ) ;
#67822 = CARTESIAN_POINT ( 'NONE',  ( -68.61467808968738780, 1379.747555724440190, 280.2219422655999779 ) ) ;
#67824 = CARTESIAN_POINT ( 'NONE',  ( 40.65896460247470401, 1444.188686613040090, 137.0313705377079998 ) ) ;
#67825 = ORIENTED_EDGE ( 'NONE', *, *, #105132, .T. ) ;
#67826 = DIRECTION ( 'NONE',  ( -1.000000000000000000, 0.000000000000000000, 0.000000000000000000 ) ) ;
#67827 = EDGE_CURVE ( 'NONE', #60554, #47910, #79910, .T. ) ;
#67828 = CARTESIAN_POINT ( 'NONE',  ( -24.69009492209999834, 1430.360063187129981, 207.6875836211879971 ) ) ;
#67830 = CARTESIAN_POINT ( 'NONE',  ( 16.50452789831379974, 1410.127611398650060, 191.9106860492449869 ) ) ;
#67829 = CARTESIAN_POINT ( 'NONE',  ( -11.67474245070000016, 1426.737381196229762, 139.7158479479979860 ) ) ;
#67831 = ADVANCED_FACE ( 'NONE', ( #89943 ), #77009, .T. ) ;
#67832 = CARTESIAN_POINT ( 'NONE',  ( -6.933616859135000254, 1516.548716157039962, 211.4141532006069895 ) ) ;
#67833 = CARTESIAN_POINT ( 'NONE',  ( 16.28988456800818341, 1509.602866217699102, 183.9209087581965321 ) ) ;
#67834 = EDGE_CURVE ( 'NONE', #99393, #80584, #71684, .T. ) ;
#67835 = CARTESIAN_POINT ( 'NONE',  ( 21.48648064083751663, 1524.477587234266366, 234.0869179060386216 ) ) ;
#67836 = CARTESIAN_POINT ( 'NONE',  ( -37.00344541100000129, 1420.039541595830087, 266.5575487690979912 ) ) ;
#67837 = CARTESIAN_POINT ( 'NONE',  ( -12.47841591940709982, 1378.791065535750022, 209.0505839962389985 ) ) ;
#67838 = EDGE_CURVE ( 'NONE', #32890, #58486, #67068, .T. ) ;
#67839 = CARTESIAN_POINT ( 'NONE',  ( 11.36622730368661038, 1464.114352876782277, 231.8218590705467932 ) ) ;
#67840 = CARTESIAN_POINT ( 'NONE',  ( 4.714200449835320050, 1508.551704408389924, 212.7479841881830112 ) ) ;
#67841 = CARTESIAN_POINT ( 'NONE',  ( -39.32574430968750079, 1440.209197080029980, 136.7482234617440042 ) ) ;
#67842 = ORIENTED_EDGE ( 'NONE', *, *, #1598, .F. ) ;
#67843 = CARTESIAN_POINT ( 'NONE',  ( 12.14532673125249929, 1396.857034010459984, 213.7755067647490250 ) ) ;
#67844 = CARTESIAN_POINT ( 'NONE',  ( 9.831033741157400030, 1461.797019875059959, 208.3422837267889918 ) ) ;
#67845 = DIRECTION ( 'NONE',  ( 0.02091224828123190022, 0.9990482215818557998, 0.03827961371219716635 ) ) ;
#67846 = ORIENTED_EDGE ( 'NONE', *, *, #74162, .F. ) ;
#67847 = ORIENTED_EDGE ( 'NONE', *, *, #6332, .T. ) ;
#67848 = CARTESIAN_POINT ( 'NONE',  ( -29.60477471821983642, 1509.968944135829588, 210.6717049192871514 ) ) ;
#67849 = CARTESIAN_POINT ( 'NONE',  ( 10.47141298996499970, 1453.021995586940193, 210.7640114736790053 ) ) ;
#67850 = CARTESIAN_POINT ( 'NONE',  ( -14.31906343784990021, 1380.323795378649947, 209.9058136714729983 ) ) ;
#67851 = CARTESIAN_POINT ( 'NONE',  ( -13.58463681145030044, 1508.551704409039985, 210.0579325790299947 ) ) ;
#67852 = CARTESIAN_POINT ( 'NONE',  ( 4.038581993089999322, 1515.598601291389969, 209.4983956875140052 ) ) ;
#67853 = VECTOR ( 'NONE', #61004, 1000.000000000000114 ) ;
#67854 = CARTESIAN_POINT ( 'NONE',  ( 15.13342375178309851, 1507.606285622089899, 226.3974328904010065 ) ) ;
#67855 = CARTESIAN_POINT ( 'NONE',  ( 33.91369104887559871, 1435.681798505150027, 135.6938344556039908 ) ) ;
#67856 = CARTESIAN_POINT ( 'NONE',  ( -31.12456774391181469, 1525.960063244516959, 201.1524202391567258 ) ) ;
#67857 = CARTESIAN_POINT ( 'NONE',  ( 27.26752121369999671, 1441.515264365290022, 137.3262971963980021 ) ) ;
#67858 = FACE_OUTER_BOUND ( 'NONE', #81207, .T. ) ;
#67859 = ADVANCED_FACE ( 'NONE', ( #98345 ), #72610, .T. ) ;
#67860 = CARTESIAN_POINT ( 'NONE',  ( -94.44617500847539304, 1384.855411388800121, 294.7348737027389802 ) ) ;
#67861 = ORIENTED_EDGE ( 'NONE', *, *, #97083, .F. ) ;
#67862 = CARTESIAN_POINT ( 'NONE',  ( -3.454748846324999789, 1516.609912606490070, 201.7988116581369979 ) ) ;
#67863 = CARTESIAN_POINT ( 'NONE',  ( 7.724874613184999461, 1517.139320148880188, 209.8621665372610039 ) ) ;
#67864 = EDGE_LOOP ( 'NONE', ( #16475, #60962, #51402, #68667 ) ) ;
#67865 = CARTESIAN_POINT ( 'NONE',  ( 11.75520567813219941, 1426.817959112909875, 145.4357449278519994 ) ) ;
#67866 = AXIS2_PLACEMENT_3D ( 'NONE', #3905, #38569, #106874 ) ;
#67867 = CARTESIAN_POINT ( 'NONE',  ( 2.942029629868560203, 1512.314860014990018, 217.0136234555809835 ) ) ;
#67868 = ORIENTED_EDGE ( 'NONE', *, *, #20166, .F. ) ;
#67869 = CARTESIAN_POINT ( 'NONE',  ( 17.66551557756463353, 1521.951704408389787, 217.9010776241849214 ) ) ;
#67870 = CARTESIAN_POINT ( 'NONE',  ( -12.93929867839810122, 1442.831169986189252, 169.4513495753611210 ) ) ;
#67871 = CARTESIAN_POINT ( 'NONE',  ( -8.589426147275000645, 1436.798469860880004, 209.9038450004319998 ) ) ;
#67872 = ADVANCED_FACE ( 'NONE', ( #11048 ), #60033, .F. ) ;
#67873 =( BOUNDED_CURVE ( )  B_SPLINE_CURVE ( 3, ( #68182, #103381, #424, #42957 ),
 .UNSPECIFIED., .F., .F. ) 
 B_SPLINE_CURVE_WITH_KNOTS ( ( 4, 4 ),
 ( 1.529854054923474926, 1.666126868289663721 ),
 .UNSPECIFIED. ) 
 CURVE ( )  GEOMETRIC_REPRESENTATION_ITEM ( )  RATIONAL_B_SPLINE_CURVE ( ( 1.000000000000000000, 0.9984530753092233368, 0.9984530753092233368, 1.000000000000000000 ) ) 
 REPRESENTATION_ITEM ( '' )  );
#67874 = CARTESIAN_POINT ( 'NONE',  ( -7.145047903430882030, 1489.825692955459090, 217.4065108216325370 ) ) ;
#67875 = CARTESIAN_POINT ( 'NONE',  ( -13.34764978429999971, 1422.966168412730212, 222.0983912147980277 ) ) ;
#67876 = CARTESIAN_POINT ( 'NONE',  ( 10.37416452553040003, 1469.777074456880200, 207.1978045308729861 ) ) ;
#67877 = CARTESIAN_POINT ( 'NONE',  ( -9.404697644369997889, 1472.841355724789992, 204.0220805676790121 ) ) ;
#67878 = EDGE_CURVE ( 'NONE', #91956, #73515, #98946, .T. ) ;
#67879 = CARTESIAN_POINT ( 'NONE',  ( 7.701966595568799256, 1441.125018358639863, 154.1230950460079896 ) ) ;
#67880 = CARTESIAN_POINT ( 'NONE',  ( -56.77117924490000433, 1379.710828546099947, 254.2839483103589941 ) ) ;
#67881 = CARTESIAN_POINT ( 'NONE',  ( -16.13533334829999788, 1485.106086671430148, 223.9657626398980028 ) ) ;
#67883 = CARTESIAN_POINT ( 'NONE',  ( 4.849004271086250206, 1466.839050287979944, 199.1402214942249884 ) ) ;
#67882 = CARTESIAN_POINT ( 'NONE',  ( 17.60092044200000316, 1458.856313947630042, 228.4764048559979983 ) ) ;
#67884 = CARTESIAN_POINT ( 'NONE',  ( -5.012111505640171494, 1423.085453659650284, 184.7955982197375420 ) ) ;
#67885 = CARTESIAN_POINT ( 'NONE',  ( -2.499957339885570118, 1419.383124631570126, 144.0983870681699841 ) ) ;
#67886 = EDGE_LOOP ( 'NONE', ( #105993, #34339, #70986, #109290, #24911 ) ) ;
#67887 = VECTOR ( 'NONE', #65583, 1000.000000000000000 ) ;
#67888 = ADVANCED_FACE ( 'NONE', ( #32789 ), #9054, .T. ) ;
#67889 = CARTESIAN_POINT ( 'NONE',  ( 16.66966702893499885, 1516.995662938509895, 223.5648772753669959 ) ) ;
#67890 = CARTESIAN_POINT ( 'NONE',  ( -21.39303731107321127, 1524.776010967693082, 233.9875059046097192 ) ) ;
#67891 = CARTESIAN_POINT ( 'NONE',  ( 2.490245914424999985, 1516.691389976299888, 213.7302634767470124 ) ) ;
#67892 = CARTESIAN_POINT ( 'NONE',  ( 5.476230074880000132, 1506.245546354389944, 219.4133339360989794 ) ) ;
#67893 = CARTESIAN_POINT ( 'NONE',  ( -14.86110812849999974, 1416.023439710309958, 213.2201437424990047 ) ) ;
#67895 = VERTEX_POINT ( 'NONE', #42864 ) ;
#67894 = CARTESIAN_POINT ( 'NONE',  ( -11.31981798910900139, 1500.653229225639961, 211.0236618496560084 ) ) ;
#67896 = CARTESIAN_POINT ( 'NONE',  ( -8.371593325730000146, 1384.916486876450108, 199.7749919984989901 ) ) ;
#67897 = CARTESIAN_POINT ( 'NONE',  ( -2.174382577350000290, 1508.375792276090124, 220.6907864031990130 ) ) ;
#67898 = CARTESIAN_POINT ( 'NONE',  ( -11.81835065930000006, 1428.979157509329980, 149.3874597924980208 ) ) ;
#67899 = PLANE ( 'NONE',  #75502 ) ;
#67900 = CARTESIAN_POINT ( 'NONE',  ( 31.61373788305444421, 1450.520975417251975, 136.3130673618244941 ) ) ;
#67901 = CARTESIAN_POINT ( 'NONE',  ( 0.000000000000000000, 1523.382868172864164, 209.1218459616979999 ) ) ;
#67902 = B_SPLINE_CURVE_WITH_KNOTS ( 'NONE', 5,
 ( #58864, #91898, #101373, #40947, #90800, #75124, #57232, #16270, #109272 ),
 .UNSPECIFIED., .F., .F.,
 ( 6, 3, 6 ),
 ( 0.000000000000000000, 0.7318475515115363539, 1.000000000000000000 ),
 .UNSPECIFIED. ) ;
#67903 = DIRECTION ( 'NONE',  ( 1.000000000000000000, 0.000000000000000000, 0.000000000000000000 ) ) ;
#67905 = CARTESIAN_POINT ( 'NONE',  ( -10.17045319919999891, 1479.387637944790185, 211.9243876371689908 ) ) ;
#67904 = CARTESIAN_POINT ( 'NONE',  ( -20.65050755260000059, 1470.086394453330058, 225.2399685796980293 ) ) ;
#67906 = CARTESIAN_POINT ( 'NONE',  ( -16.32520297863799996, 1459.451184924540030, 228.9510746369849983 ) ) ;
#67907 = AXIS2_PLACEMENT_3D ( 'NONE', #44811, #89412, #43144 ) ;
#67908 = ORIENTED_EDGE ( 'NONE', *, *, #106963, .T. ) ;
#67909 = CARTESIAN_POINT ( 'NONE',  ( -3.461360131404999763, 1516.874084700499907, 205.8683838714370040 ) ) ;
#67910 = CARTESIAN_POINT ( 'NONE',  ( 26.80873977519999940, 1412.873887987429953, 269.2446989046979979 ) ) ;
#67911 = CARTESIAN_POINT ( 'NONE',  ( 1.326713953160000070, 1454.806608698389937, 218.4390644836289823 ) ) ;
#67912 = B_SPLINE_SURFACE_WITH_KNOTS ( 'NONE', 5, 5, ( 
 ( #94417, #36744, #43499, #34528, #53569, #17694 ),
 ( #94997, #2064, #78186, #78748, #2618, #85463 ),
 ( #36195, #27788, #35080, #53010, #35630, #27239 ),
 ( #51898, #87146, #9337, #77643, #86588, #104496 ),
 ( #93871, #69261, #103368, #9879, #87715, #69823 ),
 ( #10995, #102815, #68711, #26671, #79307, #60870 ) ),
 .UNSPECIFIED., .F., .F., .F.,
 ( 6, 6 ),
 ( 6, 6 ),
 ( 8.883702454569998963, 11.85812885390000027 ),
 ( 0.000000000000000000, 1.447371157720000134 ),
 .UNSPECIFIED. ) ;
#67913 = CARTESIAN_POINT ( 'NONE',  ( 19.11094363509999994, 1430.303984236330052, 193.7458470186979866 ) ) ;
#67914 = CARTESIAN_POINT ( 'NONE',  ( -0.03650439547260889844, 1507.115325378910029, 237.3518449088199986 ) ) ;
#67915 = CARTESIAN_POINT ( 'NONE',  ( 1.326713953160000070, 1454.806608698389937, 218.4390644836289823 ) ) ;
#67916 = CARTESIAN_POINT ( 'NONE',  ( 7.012921545624998920, 1508.551704408389924, 214.6352815241970120 ) ) ;
#67917 = CARTESIAN_POINT ( 'NONE',  ( -13.77266209894789917, 1517.051704408389924, 217.0393652727940150 ) ) ;
#67918 = CARTESIAN_POINT ( 'NONE',  ( -10.48877660729999839, 1461.381695361490074, 212.5316338973990185 ) ) ;
#67919 = AXIS2_PLACEMENT_3D ( 'NONE', #82210, #81108, #6614 ) ;
#67920 = CARTESIAN_POINT ( 'NONE',  ( -12.69395104490000037, 1446.088563078959851, 187.6870124384980159 ) ) ;
#67921 = CARTESIAN_POINT ( 'NONE',  ( -16.64332109206937815, 1419.610251472236087, 209.0439647319126948 ) ) ;
#67922 = CARTESIAN_POINT ( 'NONE',  ( -5.269464883259999510, 1497.518825018089956, 219.5548267382990275 ) ) ;
#67923 = ORIENTED_EDGE ( 'NONE', *, *, #89991, .T. ) ;
#67924 = CARTESIAN_POINT ( 'NONE',  ( 1.462963723040370034, 1493.088310213640170, 181.7250244461219779 ) ) ;
#67925 = LINE ( 'NONE', #22553, #5026 ) ;
#67926 = B_SPLINE_SURFACE_WITH_KNOTS ( 'NONE', 5, 5, ( 
 ( #47600, #12880, #47059, #30226, #81726, #30783 ),
 ( #56557, #6687, #109706, #74472, #16707, #50909 ),
 ( #57120, #68286, #49263, #85040, #108600, #34094 ),
 ( #40288, #110247, #76652, #76107, #57675, #40844 ),
 ( #31888, #8330, #23483, #91790, #75017, #109167 ),
 ( #15066, #22912, #83389, #66074, #110802, #100199 ) ),
 .UNSPECIFIED., .F., .F., .F.,
 ( 6, 6 ),
 ( 6, 6 ),
 ( 4.250940516431640503, 7.082035122218359291 ),
 ( -9.670478362889549828E-06, 0.5000000000000000000 ),
 .UNSPECIFIED. ) ;
#67927 = ADVANCED_FACE ( 'NONE', ( #52928 ), #26026, .T. ) ;
#67928 = CARTESIAN_POINT ( 'NONE',  ( 10.54494294924669973, 1481.809169021529897, 210.1168006503139907 ) ) ;
#67929 = DIRECTION ( 'NONE',  ( 0.000000000000000000, 1.000000000000000000, 0.000000000000000000 ) ) ;
#67930 = CARTESIAN_POINT ( 'NONE',  ( -9.885589491230001968, 1475.057254907329934, 266.9235355597979833 ) ) ;
#67931 = CARTESIAN_POINT ( 'NONE',  ( -30.51921334599336788, 1524.059663615499858, 196.3739632444808763 ) ) ;
#67932 = CARTESIAN_POINT ( 'NONE',  ( -21.68903860500000036, 1509.722673403329964, 188.7015949552979919 ) ) ;
#67933 = ADVANCED_FACE ( 'NONE', ( #43966 ), #105338, .T. ) ;
#67934 = CARTESIAN_POINT ( 'NONE',  ( 17.92070293022930016, 1421.080221703320149, 224.5097658201460149 ) ) ;
#67935 = CARTESIAN_POINT ( 'NONE',  ( -42.89705200377979821, 1384.774197275369943, 247.4398508610279919 ) ) ;
#67936 = CARTESIAN_POINT ( 'NONE',  ( -13.67545600135260031, 1384.939478993019975, 200.4147283641960087 ) ) ;
#67937 = CARTESIAN_POINT ( 'NONE',  ( 11.90198537394640077, 1415.595619977620117, 223.2201660334189910 ) ) ;
#67938 = B_SPLINE_SURFACE_WITH_KNOTS ( 'NONE', 5, 5, ( 
 ( #27787, #78747, #53568, #17693, #87714, #61975 ),
 ( #62536, #955, #77102, #10994, #45165, #9336 ),
 ( #17136, #1497, #36194, #70936, #42943, #18263 ),
 ( #19365, #103367, #44605, #35629, #87144, #69822 ),
 ( #2063, #35079, #26108, #9878, #85461, #79306 ),
 ( #8762, #2617, #36743, #70378, #60869, #26670 ),
 ( #52457, #44046, #104495, #51326, #410, #34527 ),
 ( #68709, #102814, #78185, #60298, #27238, #94415 ),
 ( #61419, #51897, #86038, #12643, #21015, #46821 ),
 ( #72036, #13163, #80951, #5342, #106152, #21568 ),
 ( #39501, #47901, #12084, #29431, #13715, #38385 ),
 ( #64172, #107247, #20464, #4251, #19928, #37301 ) ),
 .UNSPECIFIED., .F., .F., .F.,
 ( 6, 3, 3, 6 ),
 ( 6, 6 ),
 ( 52.42854093907030233, 57.31387688920000301, 62.19918898450000455, 65.17288249872970596 ),
 ( 0.000000000000000000, 2.000023854729739980 ),
 .UNSPECIFIED. ) ;
#67939 = CARTESIAN_POINT ( 'NONE',  ( -25.20740283234720280, 1470.078870519829934, 211.7617687522999859 ) ) ;
#67940 = CARTESIAN_POINT ( 'NONE',  ( -19.00259723423208769, 1526.382868173645647, 185.3307583834140928 ) ) ;
#67941 = CARTESIAN_POINT ( 'NONE',  ( 12.26364123839999820, 1375.886883438980021, 209.1218459572589836 ) ) ;
#67942 = CARTESIAN_POINT ( 'NONE',  ( -23.69114534980000286, 1411.100850862329935, 207.0316896202280361 ) ) ;
#67943 = DIRECTION ( 'NONE',  ( 0.000000000000000000, 0.000000000000000000, -1.000000000000000000 ) ) ;
#67944 = CARTESIAN_POINT ( 'NONE',  ( 4.474738246519999407, 1484.773668731990028, 219.2871524305990079 ) ) ;
#67945 = CIRCLE ( 'NONE', #57241, 3.250000000000000000 ) ;
#67946 = ADVANCED_FACE ( 'NONE', ( #50704 ), #43035, .T. ) ;
#67947 = CARTESIAN_POINT ( 'NONE',  ( -16.35645674180000242, 1409.677081954430150, 270.0833092963979993 ) ) ;
#67948 = B_SPLINE_SURFACE_WITH_KNOTS ( 'NONE', 5, 5, ( 
 ( #83318, #15538, #6613, #40766, #100657, #109630 ),
 ( #55932, #90051, #92818, #93910, #86078, #67647 ),
 ( #1540, #85505, #94460, #93364, #51370, #41868 ),
 ( #69303, #78228, #101755, #9374, #43537, #26716 ),
 ( #26152, #101199, #102312, #76573, #103411, #35674 ),
 ( #8250, #60908, #76024, #16629, #24495, #16089 ),
 ( #110725, #34014, #58685, #110174, #42416, #34568 ),
 ( #95035, #60340, #18303, #68209, #25599, #50296 ),
 ( #84424, #68753, #7709, #25043, #59245, #77682 ) ),
 .UNSPECIFIED., .F., .F., .F.,
 ( 6, 3, 6 ),
 ( 6, 6 ),
 ( 17.98526101469999716, 36.72584873329999766, 62.49779112240000245 ),
 ( 0.000000000000000000, 1.596925542399999953 ),
 .UNSPECIFIED. ) ;
#67949 = DIRECTION ( 'NONE',  ( -0.7067700363771035610, 0.03085824620770448445, 0.7067700363771036720 ) ) ;
#67950 = CARTESIAN_POINT ( 'NONE',  ( -19.47049107349999630, 1446.886758059190015, 200.1674925962190059 ) ) ;
#67951 = CARTESIAN_POINT ( 'NONE',  ( -5.513240571345160213, 1508.551563895499839, 216.2888651835419864 ) ) ;
#67952 = CARTESIAN_POINT ( 'NONE',  ( -36.00227781734899679, 1442.549544043670039, 137.1411661128690014 ) ) ;
#67954 = CARTESIAN_POINT ( 'NONE',  ( -9.226044223009999712, 1381.782332506340026, 200.7881398668789927 ) ) ;
#67953 = CARTESIAN_POINT ( 'NONE',  ( -22.60520452300000116, 1410.200391382629959, 211.1984955222980034 ) ) ;
#67955 = CARTESIAN_POINT ( 'NONE',  ( 11.72881690059139892, 1426.701155718149948, 143.5815159837019905 ) ) ;
#67956 = DIRECTION ( 'NONE',  ( -1.000000000000000000, 0.000000000000000000, 0.000000000000000000 ) ) ;
#67957 = CIRCLE ( 'NONE', #3547, 1.000000000000000888 ) ;
#67958 = DIRECTION ( 'NONE',  ( 0.000000000000000000, -1.000000000000000000, 0.000000000000000000 ) ) ;
#67959 = DIRECTION ( 'NONE',  ( 1.643460219210440075E-32, 1.000000000000000000, -6.123233995736769734E-17 ) ) ;
#67960 = CARTESIAN_POINT ( 'NONE',  ( 11.60004869885203149, 1428.971947790928198, 136.1000015555673315 ) ) ;
#67961 = CARTESIAN_POINT ( 'NONE',  ( 1.123101578415000024, 1517.157901477309906, 203.3331546065870157 ) ) ;
#67962 = CARTESIAN_POINT ( 'NONE',  ( 22.59589169820000265, 1507.700907224229923, 227.3081670307980175 ) ) ;
#67963 = CARTESIAN_POINT ( 'NONE',  ( -30.45769963431186866, 1526.208281990536761, 201.0929247824073229 ) ) ;
#67964 = CARTESIAN_POINT ( 'NONE',  ( 5.662343758720000508, 1504.894618425089902, 220.5557215505990314 ) ) ;
#67965 = CARTESIAN_POINT ( 'NONE',  ( -8.881784197001250351E-16, 1522.051704408389924, 209.1218459616989946 ) ) ;
#67966 = CARTESIAN_POINT ( 'NONE',  ( 1.607042714549999918, 1508.277410111030122, 236.9905385516979948 ) ) ;
#67967 = CIRCLE ( 'NONE', #39327, 1.000000000000000888 ) ;
#67968 = CARTESIAN_POINT ( 'NONE',  ( 20.31245813560099833, 1507.850129543419825, 228.7302837791660295 ) ) ;
#67970 = ORIENTED_EDGE ( 'NONE', *, *, #38482, .F. ) ;
#67969 = CARTESIAN_POINT ( 'NONE',  ( -31.47360974209560069, 1379.679433932790062, 219.1936121500959871 ) ) ;
#67971 = ORIENTED_EDGE ( 'NONE', *, *, #26512, .T. ) ;
#67972 = CARTESIAN_POINT ( 'NONE',  ( 11.64843754084820127, 1434.007725651600140, 151.1673272559080203 ) ) ;
#67973 = CARTESIAN_POINT ( 'NONE',  ( -5.436310085770000633, 1397.763550466030210, 221.4241563309980165 ) ) ;
#67974 = ORIENTED_EDGE ( 'NONE', *, *, #46601, .T. ) ;
#67975 = CARTESIAN_POINT ( 'NONE',  ( -106.7853852970000048, 1379.183277988550117, 308.1922113726590169 ) ) ;
#67976 = EDGE_CURVE ( 'NONE', #80118, #90450, #2005, .T. ) ;
#67977 = CARTESIAN_POINT ( 'NONE',  ( -22.52609275360000041, 1509.699688879929909, 190.9355249643979846 ) ) ;
#67978 = CARTESIAN_POINT ( 'NONE',  ( 4.329415281104790125, 1515.068899390480283, 206.1637483033499905 ) ) ;
#67980 = DIRECTION ( 'NONE',  ( -1.000000000000000000, 0.000000000000000000, 0.000000000000000000 ) ) ;
#67979 = CARTESIAN_POINT ( 'NONE',  ( -2.500000000000529798, 1448.894380907979894, 155.6080925131469996 ) ) ;
#67981 = CARTESIAN_POINT ( 'NONE',  ( 18.41333652109999974, 1507.814877555129897, 230.2405691312980025 ) ) ;
#67982 = CARTESIAN_POINT ( 'NONE',  ( 12.99461696440000047, 1468.696672636130188, 187.3355539092980280 ) ) ;
#67983 = CARTESIAN_POINT ( 'NONE',  ( 6.632916768162448129, 1509.144686944858449, 237.5225686160735847 ) ) ;
#67984 = CARTESIAN_POINT ( 'NONE',  ( -4.500000000000000000, 1439.615672362369878, 128.3512065685980019 ) ) ;
#67985 = CARTESIAN_POINT ( 'NONE',  ( 2.468689065161279839, 1395.999268909109787, 198.3831816525220120 ) ) ;
#67986 = CARTESIAN_POINT ( 'NONE',  ( 14.40791762927999997, 1416.384967875050052, 196.9030818062619801 ) ) ;
#67987 = CARTESIAN_POINT ( 'NONE',  ( 11.29023540169999862, 1431.477258515079939, 151.4697263553979951 ) ) ;
#67988 = CARTESIAN_POINT ( 'NONE',  ( 5.706397847405000334, 1514.325389163589989, 201.4706566950069941 ) ) ;
#67989 = ORIENTED_EDGE ( 'NONE', *, *, #70801, .T. ) ;
#67990 = CARTESIAN_POINT ( 'NONE',  ( 13.42353523596650078, 1434.939809150270094, 149.0761011451980096 ) ) ;
#67991 = ORIENTED_EDGE ( 'NONE', *, *, #81643, .F. ) ;
#67992 = ORIENTED_EDGE ( 'NONE', *, *, #50445, .F. ) ;
#67993 = EDGE_CURVE ( 'NONE', #110792, #94174, #43420, .T. ) ;
#67994 = CARTESIAN_POINT ( 'NONE',  ( 13.32446307317308154, 1444.551246767114890, 169.3762330793057913 ) ) ;
#67995 = CARTESIAN_POINT ( 'NONE',  ( -6.651410363940000181, 1465.239839440230071, 233.9266418807979733 ) ) ;
#67996 = CARTESIAN_POINT ( 'NONE',  ( -7.852484159231844174, 1474.938952242313007, 202.4682600550963514 ) ) ;
#67997 = CARTESIAN_POINT ( 'NONE',  ( 2.873329360754999673, 1516.572193931679976, 216.4439510378570048 ) ) ;
#67998 = CARTESIAN_POINT ( 'NONE',  ( -7.887508661103116658, 1512.146863357109623, 212.0793319856411756 ) ) ;
#67999 = ADVANCED_BREP_SHAPE_REPRESENTATION ( '', ( #46097, #21632 ), #71657 ) ;
#68000 = EDGE_CURVE ( 'NONE', #42483, #75452, #98401, .T. ) ;
#68001 = CARTESIAN_POINT ( 'NONE',  ( 11.35450994474380160, 1422.091444931230171, 210.1627864600919793 ) ) ;
#68002 = CARTESIAN_POINT ( 'NONE',  ( 2.500000000000000000, 1448.204674875420096, 169.9458606413469965 ) ) ;
#68003 = CARTESIAN_POINT ( 'NONE',  ( 7.203018087042108522E-14, 1375.720597897399784, 207.5503168488490076 ) ) ;
#68004 = ORIENTED_EDGE ( 'NONE', *, *, #53740, .T. ) ;
#68005 = CARTESIAN_POINT ( 'NONE',  ( 7.321455873725000174, 1516.545806094630279, 206.6359999332069890 ) ) ;
#68006 = ORIENTED_EDGE ( 'NONE', *, *, #104717, .T. ) ;
#68007 = CARTESIAN_POINT ( 'NONE',  ( 21.96624934842110122, 1440.913060387330006, 227.2068459464609873 ) ) ;
#68008 = CONICAL_SURFACE ( 'NONE', #17910, 8.000000000000003553, 0.02617993877989872875 ) ;
#68009 = CARTESIAN_POINT ( 'NONE',  ( -19.75308352559999747, 1509.626197081729970, 231.2246848602980265 ) ) ;
#68010 = CARTESIAN_POINT ( 'NONE',  ( -8.912128646530000253, 1409.224278777129939, 189.0536454187979984 ) ) ;
#68011 = CARTESIAN_POINT ( 'NONE',  ( 7.569982661595000550, 1513.743447518359972, 215.3638997164470084 ) ) ;
#68013 = VERTEX_POINT ( 'NONE', #28819 ) ;
#68012 = CARTESIAN_POINT ( 'NONE',  ( -0.08631495460232219141, 1416.225364278609959, 227.2130314078410152 ) ) ;
#68014 = CARTESIAN_POINT ( 'NONE',  ( 20.41137819500000106, 1427.953452258230072, 221.0141490875980139 ) ) ;
#68015 = DIRECTION ( 'NONE',  ( 0.000000000000000000, -1.000000000000000000, 0.000000000000000000 ) ) ;
#68016 = EDGE_CURVE ( 'NONE', #54755, #96843, #51613, .T. ) ;
#68017 = CARTESIAN_POINT ( 'NONE',  ( 1.598076626895770458, 1456.722266292764971, 199.3428600893386715 ) ) ;
#68018 = LINE ( 'NONE', #18124, #14106 ) ;
#68019 = CARTESIAN_POINT ( 'NONE',  ( 20.60985939166121739, 1525.581535527369397, 181.7364793965037677 ) ) ;
#68020 = EDGE_CURVE ( 'NONE', #51946, #40367, #97040, .T. ) ;
#68021 = CARTESIAN_POINT ( 'NONE',  ( 6.556651371285000529, 1516.858146885269889, 215.6747433371770057 ) ) ;
#68022 = CARTESIAN_POINT ( 'NONE',  ( 23.89892804850000019, 1410.398181719029935, 209.5833347769950024 ) ) ;
#68023 = CARTESIAN_POINT ( 'NONE',  ( 23.69134403178578907, 1410.129789052333081, 209.5325411534778084 ) ) ;
#68024 = CARTESIAN_POINT ( 'NONE',  ( -7.720322753056100495, 1516.965532036659852, 209.0131533299550028 ) ) ;
#68025 = CARTESIAN_POINT ( 'NONE',  ( -4.608146819384999482, 1516.677239312369920, 211.4179708211670174 ) ) ;
#68026 = CARTESIAN_POINT ( 'NONE',  ( -21.59395510246054073, 1525.159177407155539, 233.4989687676688845 ) ) ;
#68027 = CARTESIAN_POINT ( 'NONE',  ( -11.85515813369189964, 1482.126388357829910, 208.2119403444889940 ) ) ;
#68028 = CARTESIAN_POINT ( 'NONE',  ( -4.982512062026007271, 1485.996114690913828, 182.4005058417187968 ) ) ;
#68030 = ORIENTED_EDGE ( 'NONE', *, *, #52876, .F. ) ;
#68029 = CARTESIAN_POINT ( 'NONE',  ( -75.49308973149999247, 1385.139059930169878, 276.6890413075590232 ) ) ;
#68031 = CARTESIAN_POINT ( 'NONE',  ( -65.68353430217270272, 1385.040512093280086, 289.6969188980430090 ) ) ;
#68032 = AXIS2_PLACEMENT_3D ( 'NONE', #11200, #69463, #45364 ) ;
#68033 = CARTESIAN_POINT ( 'NONE',  ( 6.526381463449999920, 1473.529262900630101, 262.4990045935979879 ) ) ;
#68034 = CARTESIAN_POINT ( 'NONE',  ( -27.16116926167260104, 1509.861549318230118, 220.2428113040780318 ) ) ;
#68035 = CARTESIAN_POINT ( 'NONE',  ( -8.664662764387241367, 1509.043723808620143, 236.1803171092909963 ) ) ;
#68036 = AXIS2_PLACEMENT_3D ( 'NONE', #11074, #19449, #80483 ) ;
#68037 = CARTESIAN_POINT ( 'NONE',  ( 11.82041243239999950, 1421.864495970979760, 207.3036273995689669 ) ) ;
#68038 = CARTESIAN_POINT ( 'NONE',  ( 0.7059648962766970071, 1452.945346370949892, 183.3242576825529966 ) ) ;
#68040 = CARTESIAN_POINT ( 'NONE',  ( 17.40660825725099770, 1409.684622116380069, 222.5152860288629881 ) ) ;
#68039 = CARTESIAN_POINT ( 'NONE',  ( 23.59335433453006559, 1521.951704408389787, 208.3625261891680793 ) ) ;
#68041 = CARTESIAN_POINT ( 'NONE',  ( -9.183331090101370719, 1449.795978047580093, 208.6042095093999933 ) ) ;
#68042 = CARTESIAN_POINT ( 'NONE',  ( -107.6966557359999968, 1380.358943897680092, 309.6768259782589894 ) ) ;
#68043 = ORIENTED_EDGE ( 'NONE', *, *, #91812, .F. ) ;
#68044 = CARTESIAN_POINT ( 'NONE',  ( -6.556651409415000131, 1516.858146885269889, 202.5689485651570010 ) ) ;
#68045 = CARTESIAN_POINT ( 'NONE',  ( -10.38930660322390054, 1508.437704431200018, 218.6021076291179952 ) ) ;
#68046 = AXIS2_PLACEMENT_3D ( 'NONE', #84470, #9421, #43584 ) ;
#68047 = CARTESIAN_POINT ( 'NONE',  ( 8.013264357029996177, 1374.913060387290216, 209.1218459572589836 ) ) ;
#68048 = CARTESIAN_POINT ( 'NONE',  ( 12.61640438689999932, 1416.837080256829950, 223.3238927095979989 ) ) ;
#68049 = CARTESIAN_POINT ( 'NONE',  ( 10.94755632455209948, 1461.011583818969939, 208.8505059419150029 ) ) ;
#68050 = CARTESIAN_POINT ( 'NONE',  ( -6.451353027019999686, 1421.812455514629846, 186.8014209383979960 ) ) ;
#68051 = CARTESIAN_POINT ( 'NONE',  ( -1.073543300500000131, 1444.993504060389796, 218.0402178135990141 ) ) ;
#68052 = CARTESIAN_POINT ( 'NONE',  ( 0.3919100467378520136, 1450.899374586919976, 181.2708617675390030 ) ) ;
#68053 = CARTESIAN_POINT ( 'NONE',  ( 27.05706720676449706, 1435.442239277179851, 135.2793738133329953 ) ) ;
#68054 = CARTESIAN_POINT ( 'NONE',  ( 9.862951377358559313, 1517.151704408390060, 189.8497022443989977 ) ) ;
#68055 = FACE_OUTER_BOUND ( 'NONE', #76366, .T. ) ;
#68056 = CARTESIAN_POINT ( 'NONE',  ( -109.3769603020000005, 1386.852787485200224, 297.3396656358589780 ) ) ;
#68057 = CARTESIAN_POINT ( 'NONE',  ( 10.58064693039999860, 1509.111078008130107, 182.8327862588980111 ) ) ;
#68058 = CARTESIAN_POINT ( 'NONE',  ( -21.46350454714179534, 1524.972383263452912, 183.7395372259029784 ) ) ;
#68059 = CARTESIAN_POINT ( 'NONE',  ( -2.699757113132419839, 1445.584394931136330, 217.7557302367460750 ) ) ;
#68060 = ORIENTED_EDGE ( 'NONE', *, *, #7663, .T. ) ;
#68061 = CARTESIAN_POINT ( 'NONE',  ( -9.359063114774409442, 1440.623793696270013, 205.4860248794589950 ) ) ;
#68062 = CARTESIAN_POINT ( 'NONE',  ( -34.06505905677735768, 1418.159631727885198, 269.2714297548777154 ) ) ;
#68063 = EDGE_CURVE ( 'NONE', #28836, #94675, #59219, .T. ) ;
#68064 = CARTESIAN_POINT ( 'NONE',  ( -4.115882557953129961, 1509.032029208890208, 213.4860371167349911 ) ) ;
#68065 = CARTESIAN_POINT ( 'NONE',  ( 14.00412664368519877, 1415.247667709120151, 190.9862133854840351 ) ) ;
#68066 = AXIS2_PLACEMENT_3D ( 'NONE', #53478, #10908, #63544 ) ;
#68067 = CARTESIAN_POINT ( 'NONE',  ( 10.85845406881951192, 1424.793774302243946, 138.1921923613813590 ) ) ;
#68069 = CARTESIAN_POINT ( 'NONE',  ( 33.34040796508542570, 1523.342713519623203, 196.1259889609349329 ) ) ;
#68068 = CARTESIAN_POINT ( 'NONE',  ( 11.40247488079999982, 1503.020469010889883, 210.7587791148490055 ) ) ;
#68070 = CARTESIAN_POINT ( 'NONE',  ( -13.09898176730286146, 1444.802254457625395, 186.4275170488816684 ) ) ;
#68071 = B_SPLINE_SURFACE_WITH_KNOTS ( 'NONE', 5, 1, ( 
 ( #68536, #51165 ),
 ( #85293, #89717 ),
 ( #4085, #46645 ),
 ( #55043, #89170 ),
 ( #72393, #62352 ),
 ( #27614, #37668 ) ),
 .UNSPECIFIED., .F., .F., .F.,
 ( 6, 6 ),
 ( 2, 2 ),
 ( 0.000000000000000000, 14.54369801220000014 ),
 ( 0.000000000000000000, 14.00000000000000000 ),
 .UNSPECIFIED. ) ;
#68072 = DIRECTION ( 'NONE',  ( -0.6736849260863837507, 0.000000000000000000, 0.7390186874254154326 ) ) ;
#68073 = CARTESIAN_POINT ( 'NONE',  ( -2.329957323386520063, 1515.551704201149960, 212.9510108339450198 ) ) ;
#68074 = DIRECTION ( 'NONE',  ( -0.1294182776648229727, -0.05003219150570591828, -0.9903270617424362321 ) ) ;
#68075 = CARTESIAN_POINT ( 'NONE',  ( -38.41729418502210081, 1444.641748168739923, 137.0880170107530205 ) ) ;
#68076 = CARTESIAN_POINT ( 'NONE',  ( -21.25708629881845368, 1435.239819464369702, 139.1347687532081636 ) ) ;
#68077 = CARTESIAN_POINT ( 'NONE',  ( 25.70089172607919892, 1435.395012783340235, 135.4164353173910058 ) ) ;
#68078 = CARTESIAN_POINT ( 'NONE',  ( -13.38944205750223126, 1443.385879950765684, 169.3692234598943287 ) ) ;
#68079 = VERTEX_POINT ( 'NONE', #27708 ) ;
#68080 = TOROIDAL_SURFACE ( 'NONE', #94911, 1.000000000000000000, 1.000000000000000000 ) ;
#68081 = ADVANCED_FACE ( 'NONE', ( #46741 ), #17044, .T. ) ;
#68082 = CARTESIAN_POINT ( 'NONE',  ( 0.1222452018807889951, 1415.427621830080170, 191.5619203254349827 ) ) ;
#68083 = CARTESIAN_POINT ( 'NONE',  ( 21.72816364826307378, 1509.385241731590213, 226.6647666414965840 ) ) ;
#68084 = ORIENTED_EDGE ( 'NONE', *, *, #62431, .T. ) ;
#68085 = VERTEX_POINT ( 'NONE', #107165 ) ;
#68086 = CARTESIAN_POINT ( 'NONE',  ( -2.275164556450000042, 1500.397458187289885, 230.3260808154989832 ) ) ;
#68087 = DIRECTION ( 'NONE',  ( 0.000000000000000000, 1.000000000000000000, 0.000000000000000000 ) ) ;
#68089 = CARTESIAN_POINT ( 'NONE',  ( -18.28461450430000212, 1458.543868107529988, 231.7753221004980162 ) ) ;
#68088 = CARTESIAN_POINT ( 'NONE',  ( 9.983193396660000829, 1425.227045000729959, 93.46322213869791540 ) ) ;
#68090 = CARTESIAN_POINT ( 'NONE',  ( -6.864156050670000120, 1445.800717418090017, 215.8105125318990076 ) ) ;
#68091 = CARTESIAN_POINT ( 'NONE',  ( 4.372068842044389392, 1425.711177915499775, 185.4562312974719873 ) ) ;
#68092 = CARTESIAN_POINT ( 'NONE',  ( -12.31029123717709872, 1378.376174907870109, 209.7976204910740137 ) ) ;
#68093 = CARTESIAN_POINT ( 'NONE',  ( -2.706452301512094039, 1420.190219406222923, 186.0099876176680027 ) ) ;
#68094 = CARTESIAN_POINT ( 'NONE',  ( -0.4992773797353681764, 1524.841055067849766, 244.1317247718872920 ) ) ;
#68095 = CARTESIAN_POINT ( 'NONE',  ( -24.77772770919999701, 1438.702763892639950, 210.4551298550980221 ) ) ;
#68096 = FACE_BOUND ( 'NONE', #30651, .T. ) ;
#68097 = CARTESIAN_POINT ( 'NONE',  ( 2.706438817270000019, 1450.839219090760025, 183.6941181407979968 ) ) ;
#68098 = CARTESIAN_POINT ( 'NONE',  ( 7.811382534051993787, 1363.278400952723359, 207.6218459616988241 ) ) ;
#68099 = CARTESIAN_POINT ( 'NONE',  ( -28.93059565662124299, 1510.034316939833616, 201.1399980697655963 ) ) ;
#68101 = ORIENTED_EDGE ( 'NONE', *, *, #75722, .F. ) ;
#68100 = CARTESIAN_POINT ( 'NONE',  ( -1.079296730995619915E-09, 1416.674463692480231, 238.2624803028730014 ) ) ;
#68102 = ORIENTED_EDGE ( 'NONE', *, *, #104342, .T. ) ;
#68103 = CARTESIAN_POINT ( 'NONE',  ( -11.75870877344729948, 1426.873346726019918, 145.6745198646130177 ) ) ;
#68104 = CARTESIAN_POINT ( 'NONE',  ( -2.500000000000000000, 1448.210448412289907, 176.8331131016979896 ) ) ;
#68105 = CARTESIAN_POINT ( 'NONE',  ( -5.551115123129999164E-16, 1408.913060387329779, 226.8598803041980148 ) ) ;
#68106 = DIRECTION ( 'NONE',  ( 0.9774101051267699569, 0.000000000000000000, -0.2113515706023416929 ) ) ;
#68107 = CARTESIAN_POINT ( 'NONE',  ( -113.4000000000000057, 1311.832804576489934, 313.5405874544189828 ) ) ;
#68108 = AXIS2_PLACEMENT_3D ( 'NONE', #2704, #78272, #18899 ) ;
#68109 = CYLINDRICAL_SURFACE ( 'NONE', #105518, 13.00000000000000355 ) ;
#68110 = EDGE_CURVE ( 'NONE', #46740, #100339, #51717, .T. ) ;
#68111 = CARTESIAN_POINT ( 'NONE',  ( -0.8344454606485569581, 1475.590793790669977, 197.7023485705600194 ) ) ;
#68112 =( NAMED_UNIT ( * ) SI_UNIT ( $, .STERADIAN. ) SOLID_ANGLE_UNIT ( ) );
#68113 = CARTESIAN_POINT ( 'NONE',  ( -21.20437582439999957, 1519.913060387329779, 199.9189094530979958 ) ) ;
#68114 = CARTESIAN_POINT ( 'NONE',  ( 4.763849656990267079, 1370.128942875427583, 210.6218459617030021 ) ) ;
#68115 = CARTESIAN_POINT ( 'NONE',  ( -9.521762932734290530, 1448.211015946100133, 209.8758324204249845 ) ) ;
#68116 = CARTESIAN_POINT ( 'NONE',  ( -6.122247995272200427, 1406.053493193089935, 267.5211899804779705 ) ) ;
#68117 = EDGE_CURVE ( 'NONE', #45131, #59426, #32116, .T. ) ;
#68118 = CARTESIAN_POINT ( 'NONE',  ( -14.30322175442669952, 1435.879355932359886, 149.9105199582620287 ) ) ;
#68119 = EDGE_LOOP ( 'NONE', ( #47950, #18898, #83113, #74422, #68697, #100994, #55922, #60344, #108474, #35091, #52192, #34454 ) ) ;
#68120 = CARTESIAN_POINT ( 'NONE',  ( -4.327012684985790614, 1515.157823446690145, 209.2498876927999731 ) ) ;
#68121 = CARTESIAN_POINT ( 'NONE',  ( 13.86472875750000000, 1443.323743473050172, 189.2628177551980286 ) ) ;
#68123 = ORIENTED_EDGE ( 'NONE', *, *, #11208, .T. ) ;
#68122 = B_SPLINE_CURVE_WITH_KNOTS ( 'NONE', 3,
 ( #29076, #63260, #87894, #44230 ),
 .UNSPECIFIED., .F., .F.,
 ( 4, 4 ),
 ( 0.000000000000000000, 1.000000000000000000 ),
 .UNSPECIFIED. ) ;
#68124 = ORIENTED_EDGE ( 'NONE', *, *, #95913, .F. ) ;
#68125 = EDGE_CURVE ( 'NONE', #38761, #21803, #83071, .T. ) ;
#68126 = CARTESIAN_POINT ( 'NONE',  ( 4.680157983689395174, 1422.155807250380803, 184.1346165008071694 ) ) ;
#68127 = CARTESIAN_POINT ( 'NONE',  ( 8.149545062026291475, 1425.007426972460053, 194.5668190883189936 ) ) ;
#68128 = CARTESIAN_POINT ( 'NONE',  ( -1.704794841465000044, 1517.096587378560116, 213.7484378375869767 ) ) ;
#68129 = CARTESIAN_POINT ( 'NONE',  ( -10.61951293090000092, 1485.478317074230063, 185.0532574409980100 ) ) ;
#68130 = VECTOR ( 'NONE', #55471, 1000.000000000000000 ) ;
#68131 = EDGE_CURVE ( 'NONE', #45774, #64698, #66301, .T. ) ;
#68132 = CARTESIAN_POINT ( 'NONE',  ( 7.121584085660000341, 1409.161751583630121, 222.2855843900980233 ) ) ;
#68133 = ORIENTED_EDGE ( 'NONE', *, *, #5003, .F. ) ;
#68134 = LINE ( 'NONE', #103333, #92202 ) ;
#68135 = CARTESIAN_POINT ( 'NONE',  ( 4.031142351675000235, 1516.929569650079884, 204.1114229688670036 ) ) ;
#68136 = CARTESIAN_POINT ( 'NONE',  ( -28.12061240270000084, 1509.153472191830133, 206.7763965112779943 ) ) ;
#68137 = CARTESIAN_POINT ( 'NONE',  ( 11.60004869885203682, 1428.983126981193436, 134.0999999980966777 ) ) ;
#68138 = B_SPLINE_CURVE_WITH_KNOTS ( 'NONE', 3,
 ( #53579, #35639, #2073, #70947, #61986, #37311 ),
 .UNSPECIFIED., .F., .F.,
 ( 4, 2, 4 ),
 ( 1.040834085586084103E-17, 0.001087661325621710768, 0.002175322651243411128 ),
 .UNSPECIFIED. ) ;
#68139 = CARTESIAN_POINT ( 'NONE',  ( -39.93074616002299848, 1384.582610175510126, 212.8423831063259968 ) ) ;
#68140 = DIRECTION ( 'NONE',  ( -0.3363363879354877017, -0.9417419148315043786, -3.002409420756286433E-08 ) ) ;
#68141 = AXIS2_PLACEMENT_3D ( 'NONE', #13754, #54711, #79341 ) ;
#68142 = CARTESIAN_POINT ( 'NONE',  ( -11.39446592756109844, 1470.674086296440009, 209.5209556861319982 ) ) ;
#68144 = VERTEX_POINT ( 'NONE', #13630 ) ;
#68143 = CARTESIAN_POINT ( 'NONE',  ( -11.12931925038936498, 1512.151624459630966, 193.3374815694428435 ) ) ;
#68145 = CARTESIAN_POINT ( 'NONE',  ( -24.17543378828390033, 1411.086233064730095, 209.0052275329530005 ) ) ;
#68146 = CARTESIAN_POINT ( 'NONE',  ( 27.09023322280000201, 1488.688618553730066, 211.1670471512279903 ) ) ;
#68147 = CARTESIAN_POINT ( 'NONE',  ( -47.49308081550576333, 1379.683368846476242, 241.0371517381914543 ) ) ;
#68148 = DIRECTION ( 'NONE',  ( 0.2054769195713296304, -0.000000000000000000, 0.9786619618251631847 ) ) ;
#68149 = CARTESIAN_POINT ( 'NONE',  ( 14.12038737319999804, 1509.406339941330089, 234.8413163218980060 ) ) ;
#68150 = CIRCLE ( 'NONE', #94897, 2.000000000000003553 ) ;
#68151 = EDGE_CURVE ( 'NONE', #58486, #108102, #20851, .T. ) ;
#68152 = CARTESIAN_POINT ( 'NONE',  ( -6.546039433425000276, 1516.565291103010168, 211.4147861392469849 ) ) ;
#68153 = CARTESIAN_POINT ( 'NONE',  ( -68.64714017240000032, 1379.747635037359942, 279.8389543138589488 ) ) ;
#68154 = CARTESIAN_POINT ( 'NONE',  ( 9.163876979147371316, 1436.806046061350116, 211.4130592609789971 ) ) ;
#68155 = CARTESIAN_POINT ( 'NONE',  ( 4.709428332219590452, 1480.407433587830155, 228.9870284858090201 ) ) ;
#68156 = CARTESIAN_POINT ( 'NONE',  ( 7.326072144144999854, 1516.714320817460020, 208.3685457967989976 ) ) ;
#68157 = EDGE_CURVE ( 'NONE', #30294, #49664, #38848, .T. ) ;
#68158 = VERTEX_POINT ( 'NONE', #109388 ) ;
#68159 = CARTESIAN_POINT ( 'NONE',  ( -2.798509278424440083, 1451.959363124020001, 184.7388509875849820 ) ) ;
#68160 = CARTESIAN_POINT ( 'NONE',  ( -10.16202339710000047, 1410.292653515729853, 229.5428569793980103 ) ) ;
#68161 = CARTESIAN_POINT ( 'NONE',  ( -5.959427381639999410, 1385.323914143830052, 218.4985401614089824 ) ) ;
#68162 = ORIENTED_EDGE ( 'NONE', *, *, #52443, .T. ) ;
#68164 = AXIS2_PLACEMENT_3D ( 'NONE', #56059, #47660, #81787 ) ;
#68163 = DIRECTION ( 'NONE',  ( -1.836970198721029688E-16, -1.000000000000000000, 0.000000000000000000 ) ) ;
#68165 = CARTESIAN_POINT ( 'NONE',  ( -3.707800477540000195, 1428.659817276889953, 200.9450977677189769 ) ) ;
#68166 = CARTESIAN_POINT ( 'NONE',  ( -23.88501998544221294, 1509.754567424550487, 226.4501273782086059 ) ) ;
#68167 = CARTESIAN_POINT ( 'NONE',  ( -4.069498839565195425, 1440.810691400258065, 185.0753115836025984 ) ) ;
#68168 = CARTESIAN_POINT ( 'NONE',  ( -17.71996445940000342, 1417.056829823310181, 208.8389207556330120 ) ) ;
#68169 = CARTESIAN_POINT ( 'NONE',  ( -18.46438761643240056, 1509.557851011080174, 231.7133587057680018 ) ) ;
#68170 = CARTESIAN_POINT ( 'NONE',  ( 3.971087474159999520, 1486.546787240489948, 198.9371065660989757 ) ) ;
#68171 = DIRECTION ( 'NONE',  ( -0.7074300732391541890, 0.02470400240461650618, 0.7063514732355541392 ) ) ;
#68172 = DIRECTION ( 'NONE',  ( -0.000000000000000000, 0.02617694830742909803, 0.9996573249755689172 ) ) ;
#68174 = CARTESIAN_POINT ( 'NONE',  ( -4.500000000000000000, 1508.551704408389924, 209.1218459616989946 ) ) ;
#68173 = CARTESIAN_POINT ( 'NONE',  ( -0.7365612166329978949, 1517.066898074209803, 213.7457380308570123 ) ) ;
#68175 = CARTESIAN_POINT ( 'NONE',  ( 20.84357890140000080, 1509.537325846329850, 188.5527488798980187 ) ) ;
#68176 = CARTESIAN_POINT ( 'NONE',  ( 3.260378255074999565, 1516.582197289609894, 216.8321318079170226 ) ) ;
#68177 = ORIENTED_EDGE ( 'NONE', *, *, #32170, .T. ) ;
#68178 = CARTESIAN_POINT ( 'NONE',  ( -10.78869837093980166, 1414.913060387399810, 195.9645814724970023 ) ) ;
#68179 = CARTESIAN_POINT ( 'NONE',  ( -17.35289783740000047, 1420.153549694379990, 203.7868233213689848 ) ) ;
#68180 = ORIENTED_EDGE ( 'NONE', *, *, #91161, .F. ) ;
#68181 = CARTESIAN_POINT ( 'NONE',  ( -17.18717870511359891, 1508.551704408389924, 212.3238880613659774 ) ) ;
#68182 = CARTESIAN_POINT ( 'NONE',  ( -109.1321487942470014, 1384.869787291219836, 311.2644937792119322 ) ) ;
#68183 = DIRECTION ( 'NONE',  ( 0.000000000000000000, -1.836970198721029688E-16, -1.000000000000000000 ) ) ;
#68184 = UNCERTAINTY_MEASURE_WITH_UNIT (LENGTH_MEASURE( 1.000000000000000082E-05 ), #2320, 'distance_accuracy_value', 'NONE');
#68185 = CARTESIAN_POINT ( 'NONE',  ( -7.545069326662110498, 1384.921616245829910, 219.0875787902100171 ) ) ;
#68186 = CARTESIAN_POINT ( 'NONE',  ( -11.27898552558059997, 1471.200097733860275, 207.3676664588759877 ) ) ;
#68187 = CARTESIAN_POINT ( 'NONE',  ( -7.088902828084099994, 1508.383691274782677, 219.7372291895070759 ) ) ;
#68188 = CARTESIAN_POINT ( 'NONE',  ( 17.61970473800957038, 1423.169058096252002, 226.3196634091193289 ) ) ;
#68189 = FACE_OUTER_BOUND ( 'NONE', #66266, .T. ) ;
#68190 = CARTESIAN_POINT ( 'NONE',  ( 9.326415766526549689, 1460.944052182000178, 206.0389247924669860 ) ) ;
#68191 = CARTESIAN_POINT ( 'NONE',  ( -9.740283752330000766, 1438.194204504490017, 148.7998369308980102 ) ) ;
#68192 = CARTESIAN_POINT ( 'NONE',  ( 40.87114964212709367, 1440.913060358009943, 260.4862142944329548 ) ) ;
#68194 = PLANE ( 'NONE',  #62293 ) ;
#68193 = CARTESIAN_POINT ( 'NONE',  ( -4.255262048852619827, 1420.457194194370004, 194.1488550391260048 ) ) ;
#68195 = CARTESIAN_POINT ( 'NONE',  ( 11.94272607768921368, 1433.497737235805744, 149.9957492810318627 ) ) ;
#68196 = ORIENTED_EDGE ( 'NONE', *, *, #5143, .T. ) ;
#68197 = ORIENTED_EDGE ( 'NONE', *, *, #24762, .T. ) ;
#68198 = B_SPLINE_CURVE_WITH_KNOTS ( 'NONE', 5,
 ( #80262, #3578, #55079, #12499, #61289, #95405 ),
 .UNSPECIFIED., .F., .F.,
 ( 6, 6 ),
 ( -157.9969979290000026, -29.50720980489998624 ),
 .UNSPECIFIED. ) ;
#68199 = DIRECTION ( 'NONE',  ( -5.980589973904019347E-17, 1.000000000000000000, -1.736889445713099699E-16 ) ) ;
#68200 = CARTESIAN_POINT ( 'NONE',  ( -4.226426730299999157, 1515.477082009390188, 209.1218459616989946 ) ) ;
#68201 = CARTESIAN_POINT ( 'NONE',  ( -27.74968902340000199, 1508.601238165030054, 210.5367534243380021 ) ) ;
#68202 = CARTESIAN_POINT ( 'NONE',  ( 4.040293861182902013, 1410.430566701483258, 186.0441672988231971 ) ) ;
#68203 = CARTESIAN_POINT ( 'NONE',  ( -3.083506393234342724, 1425.993302487229357, 185.5564644828080532 ) ) ;
#68204 = STYLED_ITEM ( 'NONE', ( #10944 ), #100095 ) ;
#68205 = CARTESIAN_POINT ( 'NONE',  ( 28.27139721233034919, 1526.382868172864164, 219.5606225550385204 ) ) ;
#68206 = LINE ( 'NONE', #41865, #25420 ) ;
#68207 = CARTESIAN_POINT ( 'NONE',  ( -17.65532971150000208, 1419.497219977419945, 207.2321558962389929 ) ) ;
#68208 = CARTESIAN_POINT ( 'NONE',  ( -58.43686276432150351, 1383.798853279400191, 277.8809885620339628 ) ) ;
#68209 = CARTESIAN_POINT ( 'NONE',  ( 3.623662524359999804, 1452.348591074630122, 153.7833281135980030 ) ) ;
#68210 = FACE_OUTER_BOUND ( 'NONE', #75392, .T. ) ;
#68212 = ORIENTED_EDGE ( 'NONE', *, *, #28233, .F. ) ;
#68211 = FACE_OUTER_BOUND ( 'NONE', #84111, .T. ) ;
#68213 = CARTESIAN_POINT ( 'NONE',  ( 30.99338347248546555, 1526.382868172863937, 218.3719692838077719 ) ) ;
#68214 = CARTESIAN_POINT ( 'NONE',  ( -43.23635582379999676, 1383.823167092340100, 247.4293989253590098 ) ) ;
#68215 = CARTESIAN_POINT ( 'NONE',  ( 19.77866157937050318, 1507.866340390989990, 229.2788407071620043 ) ) ;
#68216 = ORIENTED_EDGE ( 'NONE', *, *, #82837, .F. ) ;
#68217 = EDGE_LOOP ( 'NONE', ( #13035, #89402, #40473, #8738 ) ) ;
#68218 = CARTESIAN_POINT ( 'NONE',  ( 19.72812719659350122, 1509.538929610160039, 230.6333991359829838 ) ) ;
#68219 = CARTESIAN_POINT ( 'NONE',  ( 1.467768375174040179E-06, 1443.913060387330006, 126.8032257208279958 ) ) ;
#68220 = CARTESIAN_POINT ( 'NONE',  ( 37.86301218237910149, 1438.513682760549955, 136.5996409465739987 ) ) ;
#68222 = DIRECTION ( 'NONE',  ( 0.000000000000000000, 0.000000000000000000, -1.000000000000000000 ) ) ;
#68221 = CARTESIAN_POINT ( 'NONE',  ( 18.24515611230000189, 1416.817366564930126, 209.2838582706760064 ) ) ;
#68223 = CARTESIAN_POINT ( 'NONE',  ( 11.66681882931680114, 1479.992204709489897, 210.8129482343040024 ) ) ;
#68224 = CARTESIAN_POINT ( 'NONE',  ( -109.0547027409999998, 1384.148091023459756, 297.1846209902590203 ) ) ;
#68225 = CARTESIAN_POINT ( 'NONE',  ( -32.38845791999490586, 1523.382868172864164, 216.1254071228449902 ) ) ;
#68226 = AXIS2_PLACEMENT_3D ( 'NONE', #73137, #73707, #64764 ) ;
#68227 = CARTESIAN_POINT ( 'NONE',  ( -12.83843010853493283, 1435.934049928529475, 150.8131814970956270 ) ) ;
#68228 = CARTESIAN_POINT ( 'NONE',  ( -18.96814374670399772, 1466.784892475500101, 227.5901968024730024 ) ) ;
#68229 = CARTESIAN_POINT ( 'NONE',  ( 3.236814144259999804, 1409.530546742930028, 186.0023276647980026 ) ) ;
#68230 = CARTESIAN_POINT ( 'NONE',  ( 4.661455296369999779, 1424.482000793030011, 185.3998824713980014 ) ) ;
#68231 = CARTESIAN_POINT ( 'NONE',  ( 6.648508775361010592, 1432.796636464459880, 201.9740405741240181 ) ) ;
#68232 = CARTESIAN_POINT ( 'NONE',  ( -3.671612586564420244, 1441.354008908910146, 162.1785783326109822 ) ) ;
#68233 = CARTESIAN_POINT ( 'NONE',  ( 11.81421903917279970, 1428.091851616979966, 150.2203617970459959 ) ) ;
#68234 = CARTESIAN_POINT ( 'NONE',  ( 0.2305905531100000128, 1465.018788707330032, 237.3910730024980182 ) ) ;
#68235 = EDGE_LOOP ( 'NONE', ( #16402, #20240, #88493, #93882 ) ) ;
#68236 = CARTESIAN_POINT ( 'NONE',  ( -4.635574868235029733, 1480.378675748950172, 230.9803143308730000 ) ) ;
#68237 = CARTESIAN_POINT ( 'NONE',  ( 17.06401309437801217, 1526.329757971584513, 237.1783921619710895 ) ) ;
#68238 = CARTESIAN_POINT ( 'NONE',  ( -12.26996133465255845, 1416.831922878780688, 194.6642422945479325 ) ) ;
#68239 = CARTESIAN_POINT ( 'NONE',  ( -113.4000000000000057, 1305.913060387289988, 304.2218459572590064 ) ) ;
#68240 = CARTESIAN_POINT ( 'NONE',  ( 15.30440149880000078, 1449.517001060780103, 190.0710924244979765 ) ) ;
#68241 = AXIS2_PLACEMENT_3D ( 'NONE', #16321, #76814, #52726 ) ;
#68242 = CARTESIAN_POINT ( 'NONE',  ( -9.057141760850039745E-09, 1474.953449740560018, 265.2715189222170125 ) ) ;
#68243 = EDGE_CURVE ( 'NONE', #102730, #52385, #56973, .T. ) ;
#68244 = CARTESIAN_POINT ( 'NONE',  ( -19.98564276653569749, 1487.965312040789968, 190.9658536150159875 ) ) ;
#68245 = CARTESIAN_POINT ( 'NONE',  ( -1.952774559090199924, 1420.709932442649915, 193.8387323542239926 ) ) ;
#68246 = CARTESIAN_POINT ( 'NONE',  ( -4.398754361689999115, 1417.887151154330013, 234.1121797774980280 ) ) ;
#68247 = CARTESIAN_POINT ( 'NONE',  ( 1.251899778580000122, 1477.970563818089886, 198.7571063212990055 ) ) ;
#68248 = CARTESIAN_POINT ( 'NONE',  ( -106.1218566759999931, 1390.573852006310062, 307.5911815855589566 ) ) ;
#68249 = CIRCLE ( 'NONE', #70010, 2.000000000000001776 ) ;
#68250 = CARTESIAN_POINT ( 'NONE',  ( -8.160415419918159330, 1511.384673127000042, 214.5167964041220046 ) ) ;
#68251 = CARTESIAN_POINT ( 'NONE',  ( 5.887860814122072739, 1360.176812065337344, 207.6218459616987673 ) ) ;
#68252 = CARTESIAN_POINT ( 'NONE',  ( -45.84352532457269547, 1439.431483318510118, 266.4135387465440203 ) ) ;
#68253 = LINE ( 'NONE', #77187, #67667 ) ;
#68254 = CARTESIAN_POINT ( 'NONE',  ( -7.788352316159999233, 1425.537561632160077, 206.3143906032090058 ) ) ;
#68255 = EDGE_LOOP ( 'NONE', ( #37400, #6420, #3771, #94376, #14475 ) ) ;
#68256 = CARTESIAN_POINT ( 'NONE',  ( -1.715109485185000171, 1516.963431999339946, 208.3866188148990091 ) ) ;
#68257 = CARTESIAN_POINT ( 'NONE',  ( -10.17260142399999978, 1386.954104889990049, 200.6847011332289981 ) ) ;
#68258 = CARTESIAN_POINT ( 'NONE',  ( -5.886614042649569001, 1470.748248646887305, 217.3971333049484258 ) ) ;
#68259 = CARTESIAN_POINT ( 'NONE',  ( 7.418470818223539709, 1426.217778447260116, 212.5279654691829876 ) ) ;
#68260 = CIRCLE ( 'NONE', #89639, 2.000000000000001776 ) ;
#68261 = CARTESIAN_POINT ( 'NONE',  ( -26.44085854399180135, 1451.923913589589802, 135.4526211769480142 ) ) ;
#68262 = ORIENTED_EDGE ( 'NONE', *, *, #75677, .F. ) ;
#68263 = EDGE_CURVE ( 'NONE', #50393, #26041, #96388, .T. ) ;
#68264 = CARTESIAN_POINT ( 'NONE',  ( 12.80168991080000040, 1420.300675106630024, 231.9932541996980149 ) ) ;
#68266 = CARTESIAN_POINT ( 'NONE',  ( -15.27803607861480018, 1512.526687531790003, 222.3611531480509882 ) ) ;
#68265 = CARTESIAN_POINT ( 'NONE',  ( -2.664543536381771549, 1524.964158026965606, 176.5360755200448182 ) ) ;
#68267 = CARTESIAN_POINT ( 'NONE',  ( -2.919621720534709919, 1419.522956690290130, 186.2043860719099939 ) ) ;
#68268 = CARTESIAN_POINT ( 'NONE',  ( -3.152270375085599596, 1474.954422185709745, 198.1306180807430053 ) ) ;
#68269 = CARTESIAN_POINT ( 'NONE',  ( 8.045781271640001009, 1426.290936267859934, 211.5934327219790134 ) ) ;
#68270 = ADVANCED_FACE ( 'NONE', ( #15826 ), #133, .F. ) ;
#68271 = CARTESIAN_POINT ( 'NONE',  ( -23.64739862777970103, 1452.087275030800129, 137.4458378415889968 ) ) ;
#68272 = DIRECTION ( 'NONE',  ( 0.2054769195713296581, 0.000000000000000000, -0.9786619618251632957 ) ) ;
#68273 = ORIENTED_EDGE ( 'NONE', *, *, #42536, .T. ) ;
#68274 = CARTESIAN_POINT ( 'NONE',  ( -1.789119454972039946, 1410.413094933679986, 269.3349920968730089 ) ) ;
#68275 = CARTESIAN_POINT ( 'NONE',  ( 4.752796431384060938, 1418.054332079780124, 232.9684996267220072 ) ) ;
#68276 = CARTESIAN_POINT ( 'NONE',  ( 8.665450313672950600, 1435.069259100369891, 206.7692196636689914 ) ) ;
#68277 = VERTEX_POINT ( 'NONE', #92557 ) ;
#68278 = ORIENTED_EDGE ( 'NONE', *, *, #30146, .T. ) ;
#68279 = CARTESIAN_POINT ( 'NONE',  ( -23.53967062633439866, 1410.852811126989991, 210.4592016816770013 ) ) ;
#68280 = CARTESIAN_POINT ( 'NONE',  ( -0.4537698790271669780, 1408.928907069390107, 186.1253897045490078 ) ) ;
#68281 = DIRECTION ( 'NONE',  ( -0.6456859403403140130, -3.014380202827815434E-11, 0.7636030817426319173 ) ) ;
#68282 = CARTESIAN_POINT ( 'NONE',  ( -44.72199813584910544, 1433.780093884953658, 266.2156661089638874 ) ) ;
#68283 = CARTESIAN_POINT ( 'NONE',  ( -20.93296107774385462, 1436.459762213529984, 144.3971198658650792 ) ) ;
#68284 = CARTESIAN_POINT ( 'NONE',  ( 4.487249027372319787, 1509.038643251730036, 211.6097700576100067 ) ) ;
#68285 = CARTESIAN_POINT ( 'NONE',  ( 35.63549790119169813, 1463.085316031469802, 266.7196555065800112 ) ) ;
#68286 = CARTESIAN_POINT ( 'NONE',  ( -4.119379060793310288, 1508.879004046169939, 204.7521175727229945 ) ) ;
#68287 = CARTESIAN_POINT ( 'NONE',  ( -5.667996024009999800, 1427.963166378290225, 202.8006845438689822 ) ) ;
#68288 = CARTESIAN_POINT ( 'NONE',  ( -0.01328397755539850039, 1516.939580991450157, 205.8601936452070049 ) ) ;
#68289 = ADVANCED_FACE ( 'NONE', ( #110474 ), #33752, .F. ) ;
#68290 = VERTEX_POINT ( 'NONE', #7460 ) ;
#68291 = CARTESIAN_POINT ( 'NONE',  ( 18.75812740016049318, 1458.154557397180952, 227.2553891438375331 ) ) ;
#68292 = CARTESIAN_POINT ( 'NONE',  ( 1.932637921108910195, 1445.685508784159993, 199.2156413524129732 ) ) ;
#68293 = FACE_OUTER_BOUND ( 'NONE', #96845, .T. ) ;
#68294 = VERTEX_POINT ( 'NONE', #75776 ) ;
#68295 = CARTESIAN_POINT ( 'NONE',  ( 2.664554167959999997, 1448.256636474130119, 183.4094032644979677 ) ) ;
#68296 = CARTESIAN_POINT ( 'NONE',  ( 27.01619435114130141, 1451.969645972749959, 135.0017328818020133 ) ) ;
#68297 = CARTESIAN_POINT ( 'NONE',  ( -4.333038850355530158, 1508.551704408389924, 213.2968085732719885 ) ) ;
#68298 = CARTESIAN_POINT ( 'NONE',  ( -17.91820893009999693, 1388.567218049629901, 218.5290927580890070 ) ) ;
#68299 = CARTESIAN_POINT ( 'NONE',  ( 7.405238242969999440, 1422.788992526760012, 195.6018663419989991 ) ) ;
#68300 = CARTESIAN_POINT ( 'NONE',  ( -0.8336025234663499983, 1432.165250642160117, 218.5883475804189686 ) ) ;
#68301 = CARTESIAN_POINT ( 'NONE',  ( 3.780176498421650155, 1409.045067059440044, 187.4689532811570132 ) ) ;
#68303 = CARTESIAN_POINT ( 'NONE',  ( -17.93227703497376524, 1423.574558478578865, 225.8942140318575582 ) ) ;
#68302 = CARTESIAN_POINT ( 'NONE',  ( 1.116230662139999996, 1415.987376048129818, 233.0984228107980130 ) ) ;
#68304 = CARTESIAN_POINT ( 'NONE',  ( 1.420887417485810156, 1452.418213911920247, 183.4780521848920216 ) ) ;
#68305 = VECTOR ( 'NONE', #35970, 1000.000000000000000 ) ;
#68306 = CARTESIAN_POINT ( 'NONE',  ( -12.87022724600000068, 1379.571428314189916, 212.7941117598390122 ) ) ;
#68307 = CARTESIAN_POINT ( 'NONE',  ( 2.385609657812846951, 1525.697946996627479, 241.0978147455549845 ) ) ;
#68308 = ORIENTED_EDGE ( 'NONE', *, *, #58015, .T. ) ;
#68309 = CARTESIAN_POINT ( 'NONE',  ( 11.74757148146339958, 1414.971390223319986, 220.9933141604269906 ) ) ;
#68310 = CARTESIAN_POINT ( 'NONE',  ( -9.828026979480000591, 1446.801135606790012, 212.2328361272089978 ) ) ;
#68311 = CARTESIAN_POINT ( 'NONE',  ( 19.02704169900689735, 1456.915441405320053, 225.6706379604710264 ) ) ;
#68312 = CARTESIAN_POINT ( 'NONE',  ( -11.34705161930000017, 1388.497955604420213, 202.3274404867889871 ) ) ;
#68313 = CARTESIAN_POINT ( 'NONE',  ( 8.490723549529160863, 1425.167024220250141, 210.6110084034939973 ) ) ;
#68314 = CARTESIAN_POINT ( 'NONE',  ( -35.24640315935789658, 1450.253616403709884, 136.2305448810739961 ) ) ;
#68315 = DIRECTION ( 'NONE',  ( 0.000000000000000000, 0.000000000000000000, -1.000000000000000000 ) ) ;
#68316 = AXIS2_PLACEMENT_3D ( 'NONE', #66673, #24610, #15119 ) ;
#68317 = CARTESIAN_POINT ( 'NONE',  ( -36.06124927489999976, 1440.913060387330006, 262.6648722463980334 ) ) ;
#68318 = CARTESIAN_POINT ( 'NONE',  ( -21.46972948204773601, 1509.114287412469821, 191.7923745190988711 ) ) ;
#68319 = CARTESIAN_POINT ( 'NONE',  ( 11.91481860790000091, 1433.381974997530051, 150.0448548111979790 ) ) ;
#68320 = CARTESIAN_POINT ( 'NONE',  ( 6.509745749769999534, 1455.357238104129920, 219.6133833021979740 ) ) ;
#68321 = CARTESIAN_POINT ( 'NONE',  ( 12.74111629471100038, 1416.830086716310007, 196.2606222955850228 ) ) ;
#68322 = CARTESIAN_POINT ( 'NONE',  ( 14.07282483770000070, 1429.542793039189974, 194.9276198725990241 ) ) ;
#68323 = CARTESIAN_POINT ( 'NONE',  ( 9.931914985161359510, 1420.236473162700122, 196.5017368352029905 ) ) ;
#68324 = CARTESIAN_POINT ( 'NONE',  ( 9.726491193908251375E-12, 1408.913060387299993, 194.1220083575990145 ) ) ;
#68325 = CARTESIAN_POINT ( 'NONE',  ( -19.58697162420000382, 1486.201721251429944, 189.8983747997980061 ) ) ;
#68326 = CARTESIAN_POINT ( 'NONE',  ( 12.60638609191129156, 1398.286777232254053, 205.9470198407383066 ) ) ;
#68327 = CARTESIAN_POINT ( 'NONE',  ( -28.21231394539000092, 1509.976025385810090, 222.5052518413109794 ) ) ;
#68328 = AXIS2_PLACEMENT_3D ( 'NONE', #89784, #73561, #38822 ) ;
#68329 = CARTESIAN_POINT ( 'NONE',  ( 20.32611051209999786, 1410.902622695729860, 219.5117589930979989 ) ) ;
#68330 = DIRECTION ( 'NONE',  ( -1.987897879952545076E-13, 0.000000000000000000, 1.000000000000000000 ) ) ;
#68331 = FACE_OUTER_BOUND ( 'NONE', #81050, .T. ) ;
#68332 = CARTESIAN_POINT ( 'NONE',  ( -1.094850995740000110, 1515.349842019790003, 204.8390133007890199 ) ) ;
#68333 = CARTESIAN_POINT ( 'NONE',  ( 5.047151244050088970, 1472.875750233941744, 217.9874323986091440 ) ) ;
#68334 = CARTESIAN_POINT ( 'NONE',  ( 10.37959263469830162, 1453.090484190960069, 190.0119661209870117 ) ) ;
#68335 = CARTESIAN_POINT ( 'NONE',  ( -5.772727946874999461, 1516.691414181030041, 212.5791125756269935 ) ) ;
#68337 = VECTOR ( 'NONE', #53509, 1000.000000000000000 ) ;
#68336 = CARTESIAN_POINT ( 'NONE',  ( -11.87156193126500092, 1422.672759239169864, 205.5660461887279951 ) ) ;
#68338 = CARTESIAN_POINT ( 'NONE',  ( 0.1964394189208260033, 1465.025380390069813, 182.7374004966019925 ) ) ;
#68340 = VERTEX_POINT ( 'NONE', #102057 ) ;
#68339 = CARTESIAN_POINT ( 'NONE',  ( 4.821407917150390210E-08, 1406.911841293459929, 222.1218459631980124 ) ) ;
#68341 = CARTESIAN_POINT ( 'NONE',  ( 31.92108011125350231, 1512.187213306747481, 220.9591791661896139 ) ) ;
#68342 = CARTESIAN_POINT ( 'NONE',  ( -8.366082161509995174, 1446.966775783084813, 191.6214408458980074 ) ) ;
#68343 = CARTESIAN_POINT ( 'NONE',  ( 11.87509769129999881, 1433.007199317849881, 149.6991846015980059 ) ) ;
#68344 = CARTESIAN_POINT ( 'NONE',  ( -39.19204896935080029, 1449.501219045460175, 134.0999999980739688 ) ) ;
#68345 = CARTESIAN_POINT ( 'NONE',  ( -37.66849514949689848, 1445.052233488579986, 137.0436250779820000 ) ) ;
#68346 = ORIENTED_EDGE ( 'NONE', *, *, #38464, .T. ) ;
#68347 = CARTESIAN_POINT ( 'NONE',  ( -10.96172188900000144, 1470.923991379590007, 209.2568965565250210 ) ) ;
#68348 = CARTESIAN_POINT ( 'NONE',  ( -12.10381429186880098, 1391.176685838770027, 212.4734229069189837 ) ) ;
#68349 = CARTESIAN_POINT ( 'NONE',  ( -16.17135632760000163, 1414.913060387329779, 211.6988393313379788 ) ) ;
#68350 = FACE_OUTER_BOUND ( 'NONE', #31366, .T. ) ;
#68351 = CARTESIAN_POINT ( 'NONE',  ( -8.812222042580639680, 1437.453945644680061, 211.4808504019430018 ) ) ;
#68352 = CARTESIAN_POINT ( 'NONE',  ( -15.05526703829680102, 1490.297662996039890, 193.6804093798809845 ) ) ;
#68353 = CARTESIAN_POINT ( 'NONE',  ( 21.35837619879999849, 1471.309462468929951, 210.2388403116680138 ) ) ;
#68354 = CARTESIAN_POINT ( 'NONE',  ( 8.735814283539220071, 1409.218121743860138, 221.2697303220529932 ) ) ;
#68355 = CARTESIAN_POINT ( 'NONE',  ( -12.28448051250000006, 1391.742831658529894, 209.7423389907770002 ) ) ;
#68356 = CARTESIAN_POINT ( 'NONE',  ( -82.21241141603550773, 1385.166088929280022, 285.8448996073630042 ) ) ;
#68357 = CARTESIAN_POINT ( 'NONE',  ( 12.61823209568870041, 1416.826860677879949, 196.1892328963569980 ) ) ;
#68358 = CARTESIAN_POINT ( 'NONE',  ( 9.729357915104159815, 1424.710738619140102, 208.6220594428340007 ) ) ;
#68359 = EDGE_LOOP ( 'NONE', ( #8945, #63209 ) ) ;
#68360 = CARTESIAN_POINT ( 'NONE',  ( -32.69005633750000328, 1450.911397438570020, 136.2076752502979673 ) ) ;
#68361 = CARTESIAN_POINT ( 'NONE',  ( 16.68533971102617741, 1442.773887286371291, 162.0931267225411148 ) ) ;
#68363 = EDGE_LOOP ( 'NONE', ( #54380, #88947, #56659, #10079 ) ) ;
#68362 = CARTESIAN_POINT ( 'NONE',  ( -2.596261494520238688, 1525.907212628473644, 240.7735774411713123 ) ) ;
#68364 = CARTESIAN_POINT ( 'NONE',  ( 4.672259132070000653, 1473.556464307690248, 218.6750198893490165 ) ) ;
#68365 = CARTESIAN_POINT ( 'NONE',  ( 25.31820978150000201, 1509.573487416829948, 221.0603481741979692 ) ) ;
#68366 = CARTESIAN_POINT ( 'NONE',  ( -9.328535443860001664, 1363.278783432130012, 207.6218459616989946 ) ) ;
#68367 = CARTESIAN_POINT ( 'NONE',  ( -10.42285073610000090, 1493.346802325689850, 205.0798751281189993 ) ) ;
#68368 = CARTESIAN_POINT ( 'NONE',  ( -4.652381700140650445, 1440.963318135419968, 155.5568945814929975 ) ) ;
#68369 = DIRECTION ( 'NONE',  ( -5.980589973904019347E-17, 1.000000000000000000, -1.736889445713099699E-16 ) ) ;
#68370 = FACE_OUTER_BOUND ( 'NONE', #87594, .T. ) ;
#68371 = FACE_OUTER_BOUND ( 'NONE', #80226, .T. ) ;
#68372 = CARTESIAN_POINT ( 'NONE',  ( 12.44780699480000052, 1501.268281545989794, 211.7240718090590121 ) ) ;
#68373 = CARTESIAN_POINT ( 'NONE',  ( 15.09047375999177021, 1517.151704408390060, 215.6125241866901661 ) ) ;
#68374 = CARTESIAN_POINT ( 'NONE',  ( -10.30220861077111216, 1368.409031475352094, 209.6218459617033432 ) ) ;
#68375 = CARTESIAN_POINT ( 'NONE',  ( -2.868493496300000167, 1454.499781787289976, 199.0262477489989976 ) ) ;
#68376 = CARTESIAN_POINT ( 'NONE',  ( 7.709032137684999952, 1516.534320418310244, 206.6366287381669906 ) ) ;
#68377 = CARTESIAN_POINT ( 'NONE',  ( 2.500000000000000000, 1448.346004463229974, 162.8188077318980334 ) ) ;
#68378 = CARTESIAN_POINT ( 'NONE',  ( -32.05392771830335619, 1524.756004293092701, 216.1108249500459237 ) ) ;
#68379 = CARTESIAN_POINT ( 'NONE',  ( 45.63713230869999649, 1440.913060384009896, 268.9747493906979798 ) ) ;
#68381 = ORIENTED_EDGE ( 'NONE', *, *, #32172, .F. ) ;
#68380 = CARTESIAN_POINT ( 'NONE',  ( 1.554813298490000051, 1495.819410965689940, 221.3803746977989988 ) ) ;
#68382 = CARTESIAN_POINT ( 'NONE',  ( -2.038847259689231084, 1501.977400791986611, 244.9330574173806951 ) ) ;
#68383 = ORIENTED_EDGE ( 'NONE', *, *, #72916, .T. ) ;
#68384 = EDGE_CURVE ( 'NONE', #85993, #38713, #62447, .T. ) ;
#68385 = CARTESIAN_POINT ( 'NONE',  ( 0.000000000000000000, 1414.421228241719973, 209.1218459616989946 ) ) ;
#68386 = CARTESIAN_POINT ( 'NONE',  ( -24.93139309809999915, 1449.798359909379997, 205.3225103653480232 ) ) ;
#68388 = CARTESIAN_POINT ( 'NONE',  ( 16.11681422559630050, 1409.475865535250250, 193.1327842899079883 ) ) ;
#68387 = CARTESIAN_POINT ( 'NONE',  ( -11.37160906494359836, 1425.522438667359893, 139.7055457720969969 ) ) ;
#68389 = CARTESIAN_POINT ( 'NONE',  ( -6.546039433425000276, 1516.565291103010168, 211.4147861392469849 ) ) ;
#68390 =( BOUNDED_CURVE ( )  B_SPLINE_CURVE ( 3, ( #74935, #83859, #23934, #22828 ),
 .UNSPECIFIED., .F., .F. ) 
 B_SPLINE_CURVE_WITH_KNOTS ( ( 4, 4 ),
 ( 1.036132084875134307, 2.105460515756535145 ),
 .UNSPECIFIED. ) 
 CURVE ( )  GEOMETRIC_REPRESENTATION_ITEM ( )  RATIONAL_B_SPLINE_CURVE ( ( 1.000000000000000000, 0.9069598516813908162, 0.9069598516813908162, 1.000000000000000000 ) ) 
 REPRESENTATION_ITEM ( '' )  );
#68391 = CARTESIAN_POINT ( 'NONE',  ( 27.67506469288673898, 1509.991447327714695, 220.7024101144958763 ) ) ;
#68392 = CARTESIAN_POINT ( 'NONE',  ( 1.546867617820790075, 1416.839692126689897, 190.2222510973109877 ) ) ;
#68393 = CARTESIAN_POINT ( 'NONE',  ( 2.299422874330000137E-10, 1405.830933579830116, 267.2558761554980151 ) ) ;
#68394 = CARTESIAN_POINT ( 'NONE',  ( -13.12590621660049983, 1379.413787799840065, 208.5216990791799958 ) ) ;
#68395 = CARTESIAN_POINT ( 'NONE',  ( 28.29378357456099735, 1508.482245359879926, 209.4043078930619970 ) ) ;
#68396 = ADVANCED_FACE ( 'NONE', ( #33206 ), #93964, .T. ) ;
#68397 = CARTESIAN_POINT ( 'NONE',  ( 3.507271589441150361, 1508.551704408389924, 213.8929761831950032 ) ) ;
#68398 = B_SPLINE_CURVE_WITH_KNOTS ( 'NONE', 5,
 ( #87120, #105594, #104470, #62513, #52988, #28877 ),
 .UNSPECIFIED., .F., .F.,
 ( 6, 6 ),
 ( 0.000000000000000000, 1.000000000000000000 ),
 .UNSPECIFIED. ) ;
#68399 = CARTESIAN_POINT ( 'NONE',  ( -38.43658860624190510, 1439.043532485229889, 136.6419780607560028 ) ) ;
#68400 = ORIENTED_EDGE ( 'NONE', *, *, #92675, .T. ) ;
#68401 = CARTESIAN_POINT ( 'NONE',  ( 12.64817333528600152, 1398.288027439289863, 213.9887766886679970 ) ) ;
#68402 = DIRECTION ( 'NONE',  ( -1.755985294532469921E-16, 1.000000000000000000, -1.338183447452831989E-16 ) ) ;
#68403 = CARTESIAN_POINT ( 'NONE',  ( -18.34469986919999940, 1457.405375599930039, 229.1958636041979958 ) ) ;
#68404 = ORIENTED_EDGE ( 'NONE', *, *, #92115, .T. ) ;
#68405 = ORIENTED_EDGE ( 'NONE', *, *, #82518, .T. ) ;
#68406 = CARTESIAN_POINT ( 'NONE',  ( 11.60004869885204570, 1426.273943615695998, 138.2686089212693332 ) ) ;
#68407 = CARTESIAN_POINT ( 'NONE',  ( 8.376099081319999584, 1424.325079649750023, 195.9777991686989935 ) ) ;
#68408 = CARTESIAN_POINT ( 'NONE',  ( -0.5000000000000000000, 1448.894380913990062, 169.5117309619979835 ) ) ;
#68409 = CARTESIAN_POINT ( 'NONE',  ( -12.18109756395920051, 1417.441079092732707, 199.6933909727965215 ) ) ;
#68410 = CARTESIAN_POINT ( 'NONE',  ( 4.226426710960000221, 1515.477082012290111, 209.4928269685999851 ) ) ;
#68411 = B_SPLINE_CURVE_WITH_KNOTS ( 'NONE', 5,
 ( #57389, #56261, #14795, #5862, #40003, #30496 ),
 .UNSPECIFIED., .F., .F.,
 ( 6, 6 ),
 ( 0.000000000000000000, 1.000000000000000000 ),
 .UNSPECIFIED. ) ;
#68412 = CARTESIAN_POINT ( 'NONE',  ( -4.523944140811339665, 1455.378620635879997, 200.8408219016489795 ) ) ;
#68413 = CARTESIAN_POINT ( 'NONE',  ( -4.338666831039999394, 1461.192105632430184, 234.4075396365979884 ) ) ;
#68414 = CARTESIAN_POINT ( 'NONE',  ( 4.181771622075575401, 1516.718258641771627, 215.3525544691363507 ) ) ;
#68415 = CARTESIAN_POINT ( 'NONE',  ( 9.718886300337560513, 1452.141959363349997, 209.5745625312270022 ) ) ;
#68416 = CARTESIAN_POINT ( 'NONE',  ( -11.04795325579999954, 1391.825117937869891, 213.7027257443090207 ) ) ;
#68417 = CARTESIAN_POINT ( 'NONE',  ( -88.24446303712089446, 1384.831625806059947, 291.4064741984150260 ) ) ;
#68418 = EDGE_LOOP ( 'NONE', ( #58017, #76520, #15241, #79748, #21478 ) ) ;
#68419 = CARTESIAN_POINT ( 'NONE',  ( 4.615017327834999961, 1516.987478262539980, 202.5620478758069964 ) ) ;
#68420 = CARTESIAN_POINT ( 'NONE',  ( 6.556850996575000146, 1516.939568781210028, 209.1101343261499892 ) ) ;
#68421 = ORIENTED_EDGE ( 'NONE', *, *, #39908, .F. ) ;
#68422 = CARTESIAN_POINT ( 'NONE',  ( 11.77484973565070092, 1427.254610112360069, 146.7344958145999954 ) ) ;
#68423 = CARTESIAN_POINT ( 'NONE',  ( 20.60026074440000343, 1507.873289787829890, 228.0392264067980364 ) ) ;
#68424 = VERTEX_POINT ( 'NONE', #96443 ) ;
#68425 = CARTESIAN_POINT ( 'NONE',  ( -13.22475641109999955, 1415.063410489829948, 220.7066272063979966 ) ) ;
#68426 = CARTESIAN_POINT ( 'NONE',  ( -11.77504666877200101, 1432.336839525429923, 150.6178357199280242 ) ) ;
#68427 = CARTESIAN_POINT ( 'NONE',  ( -8.508749110203201127, 1436.403459463997706, 210.5997781497169399 ) ) ;
#68428 = CARTESIAN_POINT ( 'NONE',  ( -9.670072478253100456, 1461.149693659710238, 208.5233768627159918 ) ) ;
#68429 = CARTESIAN_POINT ( 'NONE',  ( -4.556667256680000833, 1420.452533403130019, 186.4400355392980089 ) ) ;
#68430 = CARTESIAN_POINT ( 'NONE',  ( 9.967393941860828832, 1469.042125965680043, 207.5003470271620074 ) ) ;
#68431 = CARTESIAN_POINT ( 'NONE',  ( -10.56464281290000073, 1472.012291739390093, 204.5722061169090011 ) ) ;
#68432 = CARTESIAN_POINT ( 'NONE',  ( 6.508711678220000074, 1494.153788970689902, 218.6819253028189962 ) ) ;
#68433 = CARTESIAN_POINT ( 'NONE',  ( -14.13710051290000003, 1379.612303426159997, 208.0723505047189974 ) ) ;
#68434 = CARTESIAN_POINT ( 'NONE',  ( -14.87670423429999822, 1451.329521634429966, 222.9740515411980084 ) ) ;
#68436 = CARTESIAN_POINT ( 'NONE',  ( 3.281831459213320201, 1466.303209658950209, 198.5678429405679992 ) ) ;
#68435 = CARTESIAN_POINT ( 'NONE',  ( 18.22804834760000148, 1459.311383086529759, 227.8763781793979888 ) ) ;
#68437 = CARTESIAN_POINT ( 'NONE',  ( -4.881429273560958570, 1423.432558903203699, 184.6511038030233465 ) ) ;
#68438 = CARTESIAN_POINT ( 'NONE',  ( -2.499957339842320270, 1419.383212207730139, 144.0944162744979735 ) ) ;
#68439 = VERTEX_POINT ( 'NONE', #3508 ) ;
#68440 = CARTESIAN_POINT ( 'NONE',  ( 18.02920443208860135, 1424.486262421390165, 224.5040309780439998 ) ) ;
#68441 = CARTESIAN_POINT ( 'NONE',  ( 0.9174002424232758912, 1516.679308524277985, 216.8346747550911573 ) ) ;
#68442 = CARTESIAN_POINT ( 'NONE',  ( -2.899297689372634323, 1484.395568125579302, 183.3060837819314202 ) ) ;
#68443 = CARTESIAN_POINT ( 'NONE',  ( -14.87918228200000037, 1415.865102022439942, 212.9009079454490063 ) ) ;
#68445 = VERTEX_POINT ( 'NONE', #12423 ) ;
#68444 = CARTESIAN_POINT ( 'NONE',  ( 1.475794680595370112, 1515.075282686660103, 204.7926718715959851 ) ) ;
#68446 = CARTESIAN_POINT ( 'NONE',  ( 1.115901143310000121, 1489.466917449630046, 186.9663283330980050 ) ) ;
#68447 = CARTESIAN_POINT ( 'NONE',  ( -12.26979726809049964, 1416.828039266780024, 194.6643405733680083 ) ) ;
#68448 = CARTESIAN_POINT ( 'NONE',  ( -10.82836173039999927, 1424.910041191229993, 145.2218151137980158 ) ) ;
#68449 = CARTESIAN_POINT ( 'NONE',  ( -10.86693375039079079, 1425.933726053461669, 148.0815712597264735 ) ) ;
#68450 = CARTESIAN_POINT ( 'NONE',  ( -10.99821780924659897, 1462.161413399840058, 209.8874997588229974 ) ) ;
#68451 = DIRECTION ( 'NONE',  ( 1.225338022780404242E-19, -0.5877852522921362954, 0.8090169943751921444 ) ) ;
#68452 = CARTESIAN_POINT ( 'NONE',  ( -6.374652409100740158, 1426.817684424950130, 202.3048622467989901 ) ) ;
#68453 = CARTESIAN_POINT ( 'NONE',  ( -16.57141203446500199, 1514.216506490359961, 223.4987549717669992 ) ) ;
#68454 = CARTESIAN_POINT ( 'NONE',  ( 11.61695163049999913, 1410.397346041930177, 229.1624418486979948 ) ) ;
#68456 = CARTESIAN_POINT ( 'NONE',  ( -10.54015973009999918, 1480.209825774290039, 212.3170011562690149 ) ) ;
#68455 = CARTESIAN_POINT ( 'NONE',  ( -19.72763672960000036, 1470.089429620230021, 226.7169729388979817 ) ) ;
#68457 = CARTESIAN_POINT ( 'NONE',  ( -2.813822098188480059, 1367.641464703512383, 209.1220808600859300 ) ) ;
#68458 = VERTEX_POINT ( 'NONE', #88058 ) ;
#68459 = CARTESIAN_POINT ( 'NONE',  ( 4.027051405805000428, 1516.733363207009916, 206.6306575737070261 ) ) ;
#68460 = CARTESIAN_POINT ( 'NONE',  ( 23.72341811100000086, 1410.667716130429881, 268.2433620527979770 ) ) ;
#68461 = CARTESIAN_POINT ( 'NONE',  ( 7.509380762641779228, 1508.909942010254326, 214.6352815282469351 ) ) ;
#68462 = CARTESIAN_POINT ( 'NONE',  ( 17.38485634039999894, 1410.884445771429910, 192.4603913046979926 ) ) ;
#68463 = CARTESIAN_POINT ( 'NONE',  ( 2.161903390967117922, 1506.361658163160655, 231.0098389382108337 ) ) ;
#68464 = EDGE_CURVE ( 'NONE', #81952, #109869, #7365, .T. ) ;
#68465 = CARTESIAN_POINT ( 'NONE',  ( 1.777651795228360143, 1454.685074748580064, 218.3589571427669966 ) ) ;
#68466 = DIRECTION ( 'NONE',  ( 0.000000000000000000, 1.000000000000000000, 0.000000000000000000 ) ) ;
#68467 = DIRECTION ( 'NONE',  ( -0.000000000000000000, -1.000000000000000000, -0.000000000000000000 ) ) ;
#68468 = CARTESIAN_POINT ( 'NONE',  ( -16.25046204339999889, 1416.958518179149905, 207.5324767410789946 ) ) ;
#68469 = CARTESIAN_POINT ( 'NONE',  ( -13.84069052210000095, 1443.989035751789970, 188.2135015426979976 ) ) ;
#68470 = EDGE_CURVE ( 'NONE', #39930, #54321, #78566, .T. ) ;
#68471 = CARTESIAN_POINT ( 'NONE',  ( -2.345429900402050016, 1485.575015422800107, 197.4542373693989816 ) ) ;
#68472 = EDGE_CURVE ( 'NONE', #75409, #48999, #94219, .T. ) ;
#68473 = DIRECTION ( 'NONE',  ( -0.7414773880254664773, -0.000000000000000000, 0.6709778558543730842 ) ) ;
#68474 = CARTESIAN_POINT ( 'NONE',  ( 41.65085711740252350, 1427.189773105231097, 269.7492452597979877 ) ) ;
#68475 = ORIENTED_EDGE ( 'NONE', *, *, #85308, .F. ) ;
#68476 = CARTESIAN_POINT ( 'NONE',  ( 1.457290784524640115, 1498.568683518979924, 181.4860206734340125 ) ) ;
#68477 = CARTESIAN_POINT ( 'NONE',  ( -14.62787175408529983, 1409.423876925000059, 206.1255987914319974 ) ) ;
#68478 = CARTESIAN_POINT ( 'NONE',  ( -10.86685207181099955, 1508.551704408280102, 208.7084760166389970 ) ) ;
#68479 = CYLINDRICAL_SURFACE ( 'NONE', #20534, 0.5000000000000026645 ) ;
#68480 = CARTESIAN_POINT ( 'NONE',  ( -12.70598598470000162, 1474.665014927529910, 267.1690917002979972 ) ) ;
#68481 = DIRECTION ( 'NONE',  ( 0.09872124640252573358, 0.9946467452574913048, -0.03052814533198805816 ) ) ;
#68482 = CARTESIAN_POINT ( 'NONE',  ( -13.06907221071063319, 1513.473942842487531, 192.3324832216730442 ) ) ;
#68483 = CARTESIAN_POINT ( 'NONE',  ( -24.07284968513953061, 1444.387198279564927, 212.0163994439685951 ) ) ;
#68484 = CARTESIAN_POINT ( 'NONE',  ( -63.63973605229279684, 1384.682326359059971, 286.7712759306380121 ) ) ;
#68485 = CARTESIAN_POINT ( 'NONE',  ( 13.58245575526007443, 1416.835806643160140, 196.3346083899895120 ) ) ;
#68486 = CARTESIAN_POINT ( 'NONE',  ( -1.887379141860000372E-15, 1438.194204504490017, 155.6035180864980134 ) ) ;
#68487 = CARTESIAN_POINT ( 'NONE',  ( -24.08134052106170131, 1444.794274679859882, 211.7743307240010040 ) ) ;
#68488 = CARTESIAN_POINT ( 'NONE',  ( 4.326992699989999913, 1515.158586642889986, 209.1218459616989946 ) ) ;
#68489 = CARTESIAN_POINT ( 'NONE',  ( -2.188078410709979771, 1508.020976590390092, 220.9453026643990086 ) ) ;
#68490 = CARTESIAN_POINT ( 'NONE',  ( -22.32273759649999789, 1409.692587561330129, 207.4115339668879869 ) ) ;
#68491 = EDGE_CURVE ( 'NONE', #108306, #80118, #44599, .T. ) ;
#68492 = CARTESIAN_POINT ( 'NONE',  ( 17.36177572460000107, 1416.518532928429977, 203.7896239905979883 ) ) ;
#68493 = B_SPLINE_CURVE_WITH_KNOTS ( 'NONE', 3,
 ( #22401, #47648, #81777, #73955 ),
 .UNSPECIFIED., .F., .F.,
 ( 4, 4 ),
 ( 0.000000000000000000, 1.000000000000000000 ),
 .UNSPECIFIED. ) ;
#68494 = DIRECTION ( 'NONE',  ( -0.8090169943749385695, 0.000000000000000000, 0.5877852522924854606 ) ) ;
#68495 = CARTESIAN_POINT ( 'NONE',  ( 10.51780859130439971, 1480.734537470010082, 208.3820307640789906 ) ) ;
#68496 = DIRECTION ( 'NONE',  ( 0.04361938736533144123, 0.9990482215818579093, 0.000000000000000000 ) ) ;
#68497 = CARTESIAN_POINT ( 'NONE',  ( -19.50074017869999921, 1447.081821278189864, 200.2081706008290212 ) ) ;
#68499 = EDGE_CURVE ( 'NONE', #8871, #26117, #87506, .T. ) ;
#68498 = CARTESIAN_POINT ( 'NONE',  ( 16.92737646175363508, 1525.317359687841190, 181.4495904955261665 ) ) ;
#68500 = DIRECTION ( 'NONE',  ( -0.9525506456058961957, 0.2950089284981370352, 0.07494664543641200993 ) ) ;
#68502 = CARTESIAN_POINT ( 'NONE',  ( -12.91320920036129927, 1379.508606576809825, 211.2369201494429944 ) ) ;
#68501 = CARTESIAN_POINT ( 'NONE',  ( -21.56891622590000068, 1409.666263542329943, 211.8934861044880051 ) ) ;
#68503 = CARTESIAN_POINT ( 'NONE',  ( 11.72712749186690040, 1426.702236078659780, 143.4605025666630240 ) ) ;
#68504 = DIRECTION ( 'NONE',  ( -9.153092986051941045E-47, 1.000000000000000000, -1.836970198721029688E-16 ) ) ;
#68505 = CARTESIAN_POINT ( 'NONE',  ( -15.16604635449859906, 1420.474734527899955, 211.5444020733049797 ) ) ;
#68506 = DIRECTION ( 'NONE',  ( -0.7071067811865493491, 0.000000000000000000, -0.7071067811865457964 ) ) ;
#68507 = CARTESIAN_POINT ( 'NONE',  ( -16.42420382550000113, 1507.212883782629888, 224.6993357452979865 ) ) ;
#68508 = CARTESIAN_POINT ( 'NONE',  ( -0.01244697378919850002, 1516.939646076049939, 203.3402601539570185 ) ) ;
#68509 = B_SPLINE_CURVE_WITH_KNOTS ( 'NONE', 5,
 ( #83279, #6577, #100617, #40726, #74899, #109049 ),
 .UNSPECIFIED., .F., .F.,
 ( 6, 6 ),
 ( -168.5477119569999900, -31.28316115780000928 ),
 .UNSPECIFIED. ) ;
#68510 = CARTESIAN_POINT ( 'NONE',  ( -4.536954624239665890, 1398.048335974680867, 221.3051406648845045 ) ) ;
#68511 = CARTESIAN_POINT ( 'NONE',  ( -3.607350949321984412, 1440.817088961761328, 156.6135841830677293 ) ) ;
#68512 = CARTESIAN_POINT ( 'NONE',  ( 8.568313680894998896, 1512.631076693560090, 221.2256935570670180 ) ) ;
#68513 = CARTESIAN_POINT ( 'NONE',  ( -18.60709431639999778, 1430.292579561230013, 194.6369243821980035 ) ) ;
#68514 = DIRECTION ( 'NONE',  ( -1.000000000000000000, 0.000000000000000000, 0.000000000000000000 ) ) ;
#68516 = ORIENTED_EDGE ( 'NONE', *, *, #104508, .T. ) ;
#68515 = CARTESIAN_POINT ( 'NONE',  ( -60.23506803088569939, 1379.735844319070111, 265.9408027383549893 ) ) ;
#68517 = ORIENTED_EDGE ( 'NONE', *, *, #71381, .F. ) ;
#68518 = CARTESIAN_POINT ( 'NONE',  ( 11.86099846289999959, 1433.814634837920039, 150.7353243123980064 ) ) ;
#68519 = CARTESIAN_POINT ( 'NONE',  ( 21.26059330700248040, 1525.055427061254932, 184.3612831740845479 ) ) ;
#68520 = EDGE_LOOP ( 'NONE', ( #76098, #57112, #26637, #77900, #77459, #93318 ) ) ;
#68521 = CARTESIAN_POINT ( 'NONE',  ( -0.0002529968379770906732, 1396.150242178169037, 221.0765849288899574 ) ) ;
#68522 = CARTESIAN_POINT ( 'NONE',  ( -21.04382066049999978, 1508.388118462830107, 192.1514652868980022 ) ) ;
#68523 = CARTESIAN_POINT ( 'NONE',  ( 3.542321145568990026, 1515.375307573260216, 205.1014385530530149 ) ) ;
#68525 = CARTESIAN_POINT ( 'NONE',  ( 0.5620975284970839425, 1416.851343896850040, 190.4751211475700075 ) ) ;
#68524 = CARTESIAN_POINT ( 'NONE',  ( 17.36735080831220301, 1468.293338259049960, 189.7435350345869836 ) ) ;
#68526 = CARTESIAN_POINT ( 'NONE',  ( 16.39757969585189912, 1498.110351991700099, 231.0166114906680264 ) ) ;
#68527 = CARTESIAN_POINT ( 'NONE',  ( 0.02470720775370000011, 1488.177913144229933, 181.6829962196979977 ) ) ;
#68528 = CARTESIAN_POINT ( 'NONE',  ( -5.335636987560000044, 1416.823418193329871, 191.7467471926979954 ) ) ;
#68529 = CARTESIAN_POINT ( 'NONE',  ( -24.24870063226580186, 1444.787720494630094, 211.3850291965160011 ) ) ;
#68530 = EDGE_CURVE ( 'NONE', #52143, #56179, #15940, .T. ) ;
#68531 = SURFACE_SIDE_STYLE ('',( #51722 ) ) ;
#68532 = CARTESIAN_POINT ( 'NONE',  ( -2.283570671295000132, 1516.909589401870107, 212.0033943946770023 ) ) ;
#68533 = CARTESIAN_POINT ( 'NONE',  ( 17.78284146230000218, 1432.724246433989947, 213.5810953123289835 ) ) ;
#68534 = CARTESIAN_POINT ( 'NONE',  ( 14.31665923840910004, 1416.051481378869994, 196.9967738469869971 ) ) ;
#68535 = CARTESIAN_POINT ( 'NONE',  ( 11.85510997289999935, 1431.526737989079948, 150.3422258050980247 ) ) ;
#68536 = CARTESIAN_POINT ( 'NONE',  ( 0.4279777834130009673, 1433.008008542290099, 203.3794753978790197 ) ) ;
#68537 = EDGE_LOOP ( 'NONE', ( #108725, #95194, #24012, #76860 ) ) ;
#68538 = CARTESIAN_POINT ( 'NONE',  ( 13.90979721639719990, 1435.199138253310139, 149.4519102904939984 ) ) ;
#68539 = ORIENTED_EDGE ( 'NONE', *, *, #96912, .T. ) ;
#68540 = ORIENTED_EDGE ( 'NONE', *, *, #68491, .F. ) ;
#68541 = CARTESIAN_POINT ( 'NONE',  ( 13.43766692883458269, 1444.332322004376692, 169.3644260008774438 ) ) ;
#68542 = CARTESIAN_POINT ( 'NONE',  ( -4.363122647530000009, 1417.926080483629903, 166.9581667359979917 ) ) ;
#68543 = CARTESIAN_POINT ( 'NONE',  ( -2.814434489400770012, 1407.025243844600027, 222.1218459754350363 ) ) ;
#68544 = CARTESIAN_POINT ( 'NONE',  ( 2.485845998894999909, 1516.545806094630279, 216.4433018439569878 ) ) ;
#68545 = CARTESIAN_POINT ( 'NONE',  ( -7.895935239610811784, 1512.041030487407625, 212.1227011107451688 ) ) ;
#68546 = CARTESIAN_POINT ( 'NONE',  ( 11.19147978021466550, 1422.145535819584893, 210.4506286102420916 ) ) ;
#68547 = CARTESIAN_POINT ( 'NONE',  ( -34.38452233966944505, 1379.638702217783703, 217.4075408561711527 ) ) ;
#68548 = CARTESIAN_POINT ( 'NONE',  ( -19.47048158160000142, 1377.796266888499986, 207.6494986257190192 ) ) ;
#68549 = ORIENTED_EDGE ( 'NONE', *, *, #104242, .F. ) ;
#68550 = CARTESIAN_POINT ( 'NONE',  ( -5.012938901904998801, 1517.051603658920158, 206.6410320471169939 ) ) ;
#68551 = ORIENTED_EDGE ( 'NONE', *, *, #100705, .T. ) ;
#68552 = CARTESIAN_POINT ( 'NONE',  ( 20.08821595115609782, 1440.913060387330006, 216.9936666811269959 ) ) ;
#68553 = DIRECTION ( 'NONE',  ( 0.000000000000000000, 1.000000000000000000, 0.000000000000000000 ) ) ;
#68554 = EDGE_LOOP ( 'NONE', ( #83506, #27340, #3620, #80024 ) ) ;
#68555 = CARTESIAN_POINT ( 'NONE',  ( -4.323257523719999718, 1409.231785804929814, 187.3862315473980118 ) ) ;
#68556 = B_SPLINE_CURVE_WITH_KNOTS ( 'NONE', 3,
 ( #29805, #70210, #104315, #46088, #63451, #62346, #63993, #98104, #27608, #61793, #95915, #53381, #10817, #44987, #79135, #2443, #104868, #96471, #19750, #57242, #14090, #30350, #49372, #23038, #82423, #40955, #5719, #47172, #66740, #74579, #100843, #39863, #75134, #91371, #99748, #48279, #74027, #108160, #56117, #40402, #81300, #73481, #23600, #100314, #30899, #90251, #21922, #14651, #38749, #48838, #57788, #108715 ),
 .UNSPECIFIED., .F., .F.,
 ( 4, 3, 3, 3, 3, 3, 3, 3, 3, 3, 3, 3, 3, 3, 3, 3, 3, 4 ),
 ( -12.17647483446349987, -11.45127338244570048, -10.72607193042779983, -9.975235041999999552, -9.382994760010351598, -8.586766221277258637, -7.762798876129999748, -7.064923798146399925, -6.276317141653310117, -5.531936552890000414, -4.937941270824259377, -4.105330589925559437, -3.273015945220000944, -3.105111820674819612, -2.294061070765691213, -1.507377760193390870, -0.7388578846428242031, -2.629008122312370688E-13 ),
 .UNSPECIFIED. ) ;
#68557 = CARTESIAN_POINT ( 'NONE',  ( 7.573276829334999682, 1513.355826799109764, 216.9658125846070220 ) ) ;
#68559 = ORIENTED_EDGE ( 'NONE', *, *, #10326, .F. ) ;
#68558 = CARTESIAN_POINT ( 'NONE',  ( -3.220674668504990290, 1433.265634988960073, 218.1214075394389909 ) ) ;
#68560 = CARTESIAN_POINT ( 'NONE',  ( 21.56408335959999789, 1429.453335383130025, 218.9472881200579764 ) ) ;
#68561 = CARTESIAN_POINT ( 'NONE',  ( -13.58041510073769942, 1508.551704408389924, 210.3416170870220014 ) ) ;
#68562 = DIRECTION ( 'NONE',  ( 0.6831251091958939758, -0.2299220283779639940, -0.6931637224008919684 ) ) ;
#68564 = EDGE_CURVE ( 'NONE', #41801, #32360, #48810, .T. ) ;
#68563 = CARTESIAN_POINT ( 'NONE',  ( 0.003579571106766400116, 1467.142144048650152, 235.6416276143629887 ) ) ;
#68565 = CARTESIAN_POINT ( 'NONE',  ( 21.19880661588985404, 1526.382868172863937, 184.6948938244646854 ) ) ;
#68566 = EDGE_CURVE ( 'NONE', #44537, #80100, #49949, .T. ) ;
#68567 = CARTESIAN_POINT ( 'NONE',  ( -3.451033427095000050, 1517.025653221279981, 214.9083735325669977 ) ) ;
#68568 = CARTESIAN_POINT ( 'NONE',  ( 2.601664184880000175, 1468.435072065989971, 215.8528537042190010 ) ) ;
#68569 = CARTESIAN_POINT ( 'NONE',  ( -20.58126087740000187, 1507.779106712530165, 190.0921675882979969 ) ) ;
#68570 = CARTESIAN_POINT ( 'NONE',  ( 6.081400497050199583, 1508.610505975320166, 216.4418972163030048 ) ) ;
#68571 = CARTESIAN_POINT ( 'NONE',  ( -6.933879441005000643, 1516.560253536979872, 211.6083207129769903 ) ) ;
#68572 = CARTESIAN_POINT ( 'NONE',  ( 14.24543712669999884, 1409.914297001830164, 191.5991055419980000 ) ) ;
#68574 = EDGE_LOOP ( 'NONE', ( #93155, #16890, #74312 ) ) ;
#68573 = CARTESIAN_POINT ( 'NONE',  ( -53.42810237920000560, 1386.663619491189820, 230.7733755451590127 ) ) ;
#68575 = CARTESIAN_POINT ( 'NONE',  ( -74.53493904026449002, 1385.009369445449920, 299.6431026865259923 ) ) ;
#68576 = CARTESIAN_POINT ( 'NONE',  ( 39.40334551520000161, 1445.870380880999846, 259.1105671997980266 ) ) ;
#68577 = CARTESIAN_POINT ( 'NONE',  ( 2.611439748538543437, 1452.027163526197228, 183.7718830791166340 ) ) ;
#68578 = CARTESIAN_POINT ( 'NONE',  ( -7.572192888655000509, 1511.308638870219966, 211.6864797536570109 ) ) ;
#68579 = CARTESIAN_POINT ( 'NONE',  ( -1.673272949882680161, 1509.003834942280037, 238.7500911974470057 ) ) ;
#68580 = CARTESIAN_POINT ( 'NONE',  ( -24.09814616339999915, 1444.255785636859855, 212.5772553282479862 ) ) ;
#68582 = CARTESIAN_POINT ( 'NONE',  ( 17.00957473938450093, 1409.517103885259985, 222.2161159761519968 ) ) ;
#68581 = LINE ( 'NONE', #68039, #75089 ) ;
#68583 = CARTESIAN_POINT ( 'NONE',  ( -9.270159725700629849, 1448.714146504459904, 209.7629294459360096 ) ) ;
#68584 = CARTESIAN_POINT ( 'NONE',  ( -108.7614019690100093, 1383.708971085589837, 311.0587876456319805 ) ) ;
#68585 = EDGE_LOOP ( 'NONE', ( #32516, #98096 ) ) ;
#68586 = CARTESIAN_POINT ( 'NONE',  ( 1.706797785944999868, 1517.164987839469859, 203.3324512698969784 ) ) ;
#68587 = EDGE_CURVE ( 'NONE', #19422, #89981, #52018, .T. ) ;
#68588 = CARTESIAN_POINT ( 'NONE',  ( 0.2151019729850000006, 1406.066550330029941, 269.0456880831980016 ) ) ;
#68589 = CARTESIAN_POINT ( 'NONE',  ( 28.20849540440000069, 1509.668627050129771, 207.1396464727879732 ) ) ;
#68590 = ADVANCED_FACE ( 'NONE', ( #38721 ), #72358, .F. ) ;
#68591 = CARTESIAN_POINT ( 'NONE',  ( 24.65284882109999742, 1440.998884811290054, 212.5088486048679783 ) ) ;
#68592 = CARTESIAN_POINT ( 'NONE',  ( -7.506265444784725460, 1461.911152747223696, 202.9443364886544998 ) ) ;
#68593 = CARTESIAN_POINT ( 'NONE',  ( 3.604343046649999938, 1467.193817153390000, 218.5376378362390142 ) ) ;
#68594 = DIRECTION ( 'NONE',  ( -1.407418274235009893E-17, -1.000000000000000000, 2.576261870300909820E-17 ) ) ;
#68595 = EDGE_CURVE ( 'NONE', #78107, #27485, #66029, .T. ) ;
#68596 = CARTESIAN_POINT ( 'NONE',  ( 33.27875429775290428, 1435.659579155510073, 135.0862773368370142 ) ) ;
#68597 = CARTESIAN_POINT ( 'NONE',  ( -113.4000000000000057, 1304.231242809270043, 304.2218459572590064 ) ) ;
#68598 = CARTESIAN_POINT ( 'NONE',  ( -12.78743204916831822, 1416.839570625586930, 195.1659244036679866 ) ) ;
#68599 = CARTESIAN_POINT ( 'NONE',  ( -1.879007491539999908, 1430.448079191990018, 200.8521231223890027 ) ) ;
#68600 = CARTESIAN_POINT ( 'NONE',  ( 10.16713191040000019, 1507.687633808930059, 183.8172474484979944 ) ) ;
#68601 = CARTESIAN_POINT ( 'NONE',  ( 10.47063686347510014, 1481.493996793529959, 210.6398709714650010 ) ) ;
#68602 = CARTESIAN_POINT ( 'NONE',  ( -21.60845823726274872, 1524.659148609483054, 183.5973147963038059 ) ) ;
#68603 = CARTESIAN_POINT ( 'NONE',  ( -7.848979634317430509, 1522.051704408389924, 202.2988320601959913 ) ) ;
#68604 = EDGE_LOOP ( 'NONE', ( #56555, #107627, #83220, #29832 ) ) ;
#68605 = CARTESIAN_POINT ( 'NONE',  ( 1.613214857710000061, 1426.534415841129885, 146.0564723340980038 ) ) ;
#68606 = CARTESIAN_POINT ( 'NONE',  ( -33.91369269983620427, 1450.440666099120108, 136.2454419983430114 ) ) ;
#68607 = AXIS2_PLACEMENT_3D ( 'NONE', #32011, #108721, #5724 ) ;
#68608 = ADVANCED_FACE ( 'NONE', ( #72896 ), #110720, .T. ) ;
#68609 = CARTESIAN_POINT ( 'NONE',  ( -4.987081080971620395, 1508.551704408389924, 213.0804751642000099 ) ) ;
#68610 = SPHERICAL_SURFACE ( 'NONE', #41979, 2.000000000000000000 ) ;
#68611 = CARTESIAN_POINT ( 'NONE',  ( -0.7176848839889999887, 1417.283279384530033, 235.8571367780980097 ) ) ;
#68613 = CARTESIAN_POINT ( 'NONE',  ( 32.99911596133222247, 1524.244163922423922, 196.1627191131775874 ) ) ;
#68612 = CARTESIAN_POINT ( 'NONE',  ( 12.70238417940000097, 1500.652076303089871, 209.5864169051759802 ) ) ;
#68614 = CARTESIAN_POINT ( 'NONE',  ( 25.25200551730000242, 1450.804230319249882, 137.6134878989979882 ) ) ;
#68615 = FACE_OUTER_BOUND ( 'NONE', #101759, .T. ) ;
#68616 = CARTESIAN_POINT ( 'NONE',  ( -16.78480385485708481, 1526.748660780343471, 181.5273693450638746 ) ) ;
#68617 = EDGE_CURVE ( 'NONE', #4488, #39734, #73999, .T. ) ;
#68618 = B_SPLINE_CURVE_WITH_KNOTS ( 'NONE', 3,
 ( #57057, #88976, #6077, #21745, #13350, #64355, #97921, #12820, #47000, #80589 ),
 .UNSPECIFIED., .F., .F.,
 ( 4, 2, 2, 2, 4 ),
 ( 0.000000000000000000, 0.2499999999999998335, 0.4999999999999998890, 0.7499999999999998890, 1.000000000000000000 ),
 .UNSPECIFIED. ) ;
#68619 = CARTESIAN_POINT ( 'NONE',  ( 42.54897258395909176, 1440.913021756910211, 270.0691962208189807 ) ) ;
#68620 = CARTESIAN_POINT ( 'NONE',  ( -14.87261298220626848, 1451.156254727674877, 149.8042946858963944 ) ) ;
#68621 = CARTESIAN_POINT ( 'NONE',  ( -6.191729861150000680, 1483.183474162390212, 200.3799189381190047 ) ) ;
#68622 = CARTESIAN_POINT ( 'NONE',  ( 25.82385068980000042, 1436.204139849239937, 136.8568693873980067 ) ) ;
#68623 = CARTESIAN_POINT ( 'NONE',  ( -10.96840289711549943, 1396.296085456599940, 207.6085868023199907 ) ) ;
#68624 = EDGE_LOOP ( 'NONE', ( #16264, #57927, #62068, #55459, #34232 ) ) ;
#68625 = ADVANCED_FACE ( 'NONE', ( #108130 ), #65606, .T. ) ;
#68626 = CARTESIAN_POINT ( 'NONE',  ( -16.99375006173600156, 1409.880053590220086, 225.6062263545040025 ) ) ;
#68627 = CARTESIAN_POINT ( 'NONE',  ( -9.399544156962228669, 1482.890756672869884, 227.8968317774389902 ) ) ;
#68628 = ORIENTED_EDGE ( 'NONE', *, *, #16453, .T. ) ;
#68629 = ORIENTED_EDGE ( 'NONE', *, *, #50135, .T. ) ;
#68630 = CARTESIAN_POINT ( 'NONE',  ( 9.921670129709269759, 1445.422324508452675, 184.5085384531410568 ) ) ;
#68632 = EDGE_CURVE ( 'NONE', #61609, #100009, #29775, .T. ) ;
#68631 = CARTESIAN_POINT ( 'NONE',  ( -15.20276107160831103, 1416.056970463632979, 206.2047736444255293 ) ) ;
#68634 = CARTESIAN_POINT ( 'NONE',  ( -2.543319604096950126, 1457.772035387090000, 219.4813672542439917 ) ) ;
#68633 = CARTESIAN_POINT ( 'NONE',  ( 10.68580243010000075, 1425.706269979529907, 93.45797665869790194 ) ) ;
#68635 = CARTESIAN_POINT ( 'NONE',  ( 23.82311388440000144, 1410.240487848430121, 209.8684836133409704 ) ) ;
#68636 = EDGE_CURVE ( 'NONE', #32529, #67505, #100214, .T. ) ;
#68637 = CARTESIAN_POINT ( 'NONE',  ( 4.181971434956770040, 1424.905875537870088, 185.1749942703449960 ) ) ;
#68638 = CARTESIAN_POINT ( 'NONE',  ( -2.500591765228052044, 1421.109708633257696, 185.0623077226939017 ) ) ;
#68639 = CARTESIAN_POINT ( 'NONE',  ( -2.534335827540430852, 1523.982201850120191, 242.5731047040207784 ) ) ;
#68640 = CARTESIAN_POINT ( 'NONE',  ( 10.37959279779999910, 1453.090483345690018, 190.0119662633989890 ) ) ;
#68641 = CARTESIAN_POINT ( 'NONE',  ( 8.365522723199999788, 1508.201466091430120, 182.8802321776979909 ) ) ;
#68642 = CARTESIAN_POINT ( 'NONE',  ( 3.920714864009999356, 1449.393300602180261, 184.2471769888979907 ) ) ;
#68643 = EDGE_CURVE ( 'NONE', #59669, #29227, #68875, .T. ) ;
#68644 = CARTESIAN_POINT ( 'NONE',  ( 8.991947938729746070, 1365.087450627709131, 207.6218459616988241 ) ) ;
#68646 = VERTEX_POINT ( 'NONE', #52108 ) ;
#68645 = CARTESIAN_POINT ( 'NONE',  ( -14.00462132320000030, 1415.677402202029953, 214.2425697179989754 ) ) ;
#68647 = EDGE_LOOP ( 'NONE', ( #34977, #84279, #38153, #79247 ) ) ;
#68648 = CARTESIAN_POINT ( 'NONE',  ( -10.18103031238528899, 1521.804095990992209, 184.9292055843479829 ) ) ;
#68649 = CARTESIAN_POINT ( 'NONE',  ( -4.576312612474013441, 1522.051704408389924, 222.3843417993991807 ) ) ;
#68650 = CARTESIAN_POINT ( 'NONE',  ( -0.9453320770299999953, 1471.431441225329991, 269.3347421566979847 ) ) ;
#68651 = CARTESIAN_POINT ( 'NONE',  ( 13.68849417913788535, 1434.975516646386268, 146.5173254893715011 ) ) ;
#68652 = CARTESIAN_POINT ( 'NONE',  ( -120.4392612185250044, 1309.112692017090694, 300.3762800269186641 ) ) ;
#68653 = CARTESIAN_POINT ( 'NONE',  ( 15.98141629860000101, 1475.513060387329915, 194.5230232035980293 ) ) ;
#68654 = CARTESIAN_POINT ( 'NONE',  ( -8.868478827680000620, 1384.515996041270000, 199.9512279144889817 ) ) ;
#68655 = CARTESIAN_POINT ( 'NONE',  ( 16.66936639845652834, 1523.382868172864164, 237.7608804993219280 ) ) ;
#68656 = DIRECTION ( 'NONE',  ( -1.000000000000000000, 0.000000000000000000, 0.000000000000000000 ) ) ;
#68657 = CARTESIAN_POINT ( 'NONE',  ( -19.81155763900000011, 1453.313060387329870, 204.5601901296680012 ) ) ;
#68658 = CARTESIAN_POINT ( 'NONE',  ( 9.901269661657691401, 1368.573894001910048, 208.3718459617010978 ) ) ;
#68659 = CARTESIAN_POINT ( 'NONE',  ( -0.05087731996257439937, 1408.368774903450003, 195.5796676407180144 ) ) ;
#68660 = CARTESIAN_POINT ( 'NONE',  ( -24.08411849022170159, 1411.068933507980091, 268.8151254836839712 ) ) ;
#68661 = CARTESIAN_POINT ( 'NONE',  ( -14.24203721301430114, 1435.591090021740001, 149.7553460124620131 ) ) ;
#68662 = VERTEX_POINT ( 'NONE', #109257 ) ;
#68663 = DIRECTION ( 'NONE',  ( -0.6736849260863841948, 0.000000000000000000, 0.7390186874254148774 ) ) ;
#68664 = CARTESIAN_POINT ( 'NONE',  ( 14.09542765070000137, 1445.387346742360023, 189.3996806953979899 ) ) ;
#68665 = B_SPLINE_CURVE_WITH_KNOTS ( 'NONE', 3,
 ( #588, #92403, #93506, #51527, #77831, #9512, #92963, #43680, #77290, #33595, #66694, #59947, #24091, #103007, #110321, #50982, #59395, #94616, #1140, #101899, #34715, #26304, #60496, #42571, #58279, #25745, #68906, #43132 ),
 .UNSPECIFIED., .F., .F.,
 ( 4, 2, 1, 2, 2, 2, 1, 1, 2, 2, 2, 1, 1, 1, 2, 2, 4 ),
 ( 0.000000000000000000, 0.1249999999999616696, 0.1874999999999424904, 0.2187499999998885059, 0.2499999999998345213, 0.3749999999995644595, 0.4374999999994318434, 0.4687499999993567923, 0.4843749999993692823, 0.4999999999993818278, 0.6249999999998263611, 0.6875000000000558442, 0.7187500000001132427, 0.7343750000001351141, 0.7421875000000797140, 0.7500000000000243139, 1.000000000000000000 ),
 .UNSPECIFIED. ) ;
#68666 = EDGE_LOOP ( 'NONE', ( #77755, #19360, #86393, #7680 ) ) ;
#68667 = ORIENTED_EDGE ( 'NONE', *, *, #49464, .F. ) ;
#68668 = CARTESIAN_POINT ( 'NONE',  ( -21.38516915557943321, 1512.187213306747481, 237.8497028174240313 ) ) ;
#68669 = CARTESIAN_POINT ( 'NONE',  ( 6.812867228078430593, 1424.640977396479911, 193.9125305968219948 ) ) ;
#68670 = CARTESIAN_POINT ( 'NONE',  ( -7.324914956285000223, 1516.685667699390024, 213.7393364370070117 ) ) ;
#68671 = CARTESIAN_POINT ( 'NONE',  ( -17.32570511339999797, 1470.470731013029990, 189.1993959853980130 ) ) ;
#68672 = EDGE_CURVE ( 'NONE', #103394, #66505, #69642, .T. ) ;
#68673 = VERTEX_POINT ( 'NONE', #59965 ) ;
#68674 = FACE_OUTER_BOUND ( 'NONE', #20869, .T. ) ;
#68675 = EDGE_CURVE ( 'NONE', #58764, #42643, #23421, .T. ) ;
#68676 = CARTESIAN_POINT ( 'NONE',  ( -5.359822931069220253, 1422.298725726440125, 145.8185784961330000 ) ) ;
#68677 = CARTESIAN_POINT ( 'NONE',  ( 1.123101578415000024, 1517.157901477309906, 203.3331546065870157 ) ) ;
#68678 = CARTESIAN_POINT ( 'NONE',  ( -29.68011195740000119, 1509.981398976430228, 207.8176008383179862 ) ) ;
#68679 = CARTESIAN_POINT ( 'NONE',  ( -34.04223167274130191, 1384.566179893659864, 208.0543316770909996 ) ) ;
#68680 = CARTESIAN_POINT ( 'NONE',  ( -7.478246699966769384, 1428.083861423860071, 222.0822691923259811 ) ) ;
#68681 = CARTESIAN_POINT ( 'NONE',  ( -103.9064370230000094, 1389.684541055990167, 306.7300248541590122 ) ) ;
#68683 = EDGE_LOOP ( 'NONE', ( #22136, #3526, #97432, #19501 ) ) ;
#68682 = CARTESIAN_POINT ( 'NONE',  ( -10.44739388110000000, 1446.724320542959958, 186.7828859559980117 ) ) ;
#68684 = CARTESIAN_POINT ( 'NONE',  ( -24.91361132602320083, 1430.502641201929919, 208.6735168275199612 ) ) ;
#68685 = CARTESIAN_POINT ( 'NONE',  ( 27.16947874219999903, 1488.689296588730031, 210.7748653152779923 ) ) ;
#68686 = CIRCLE ( 'NONE', #61501, 26.50000000000001421 ) ;
#68687 = CARTESIAN_POINT ( 'NONE',  ( 19.34098968424050113, 1467.084471247349938, 225.9997439510970025 ) ) ;
#68688 = EDGE_CURVE ( 'NONE', #96843, #101763, #66422, .T. ) ;
#68689 = CARTESIAN_POINT ( 'NONE',  ( -24.25710768520000116, 1435.418799296620136, 137.1797428065980000 ) ) ;
#68690 = CARTESIAN_POINT ( 'NONE',  ( -7.709032175815000443, 1516.534320418310244, 211.6070631641669877 ) ) ;
#68691 = CARTESIAN_POINT ( 'NONE',  ( -68.69754074780000508, 1379.747811941090276, 279.9522140925590179 ) ) ;
#68692 = CIRCLE ( 'NONE', #43657, 1.000000000000000888 ) ;
#68693 = CARTESIAN_POINT ( 'NONE',  ( -14.87415096680000026, 1413.165999674329896, 226.7982133869979862 ) ) ;
#68694 = CARTESIAN_POINT ( 'NONE',  ( -30.15498091547243575, 1525.730671948510917, 221.2486426791599001 ) ) ;
#68695 =( BOUNDED_CURVE ( )  B_SPLINE_CURVE ( 3, ( #34991, #22845, #68076, #59116 ),
 .UNSPECIFIED., .F., .F. ) 
 B_SPLINE_CURVE_WITH_KNOTS ( ( 4, 4 ),
 ( 2.183705749549460062, 2.832670179246489894 ),
 .UNSPECIFIED. ) 
 CURVE ( )  GEOMETRIC_REPRESENTATION_ITEM ( )  RATIONAL_B_SPLINE_CURVE ( ( 1.000000000000000000, 0.9652106218148086558, 0.9652106218148086558, 1.000000000000000000 ) ) 
 REPRESENTATION_ITEM ( '' )  );
#68696 = CARTESIAN_POINT ( 'NONE',  ( -0.01012492377659850000, 1516.989863902050047, 207.9939175986969815 ) ) ;
#68697 = ORIENTED_EDGE ( 'NONE', *, *, #18138, .F. ) ;
#68698 = CARTESIAN_POINT ( 'NONE',  ( -1.948088825686169923, 1451.942038968990119, 184.3567259028899912 ) ) ;
#68699 = CARTESIAN_POINT ( 'NONE',  ( -0.8591407147159999536, 1410.309640657729915, 233.0900045620979881 ) ) ;
#68700 = CARTESIAN_POINT ( 'NONE',  ( -25.93597669760000102, 1384.979378440369828, 224.2477222537590364 ) ) ;
#68701 = VERTEX_POINT ( 'NONE', #75110 ) ;
#68703 = CARTESIAN_POINT ( 'NONE',  ( -10.67935949065659962, 1385.309203628900150, 218.7885473373299874 ) ) ;
#68702 = B_SPLINE_CURVE_WITH_KNOTS ( 'NONE', 5,
 ( #29576, #98434, #63232, #14417, #48047, #12225 ),
 .UNSPECIFIED., .F., .F.,
 ( 6, 6 ),
 ( 0.000000000000000000, 1.000000000000000000 ),
 .UNSPECIFIED. ) ;
#68704 = ADVANCED_FACE ( 'NONE', ( #92981 ), #51953, .F. ) ;
#68705 = CARTESIAN_POINT ( 'NONE',  ( -3.611921233329999925, 1429.380855016690020, 201.5074060074890099 ) ) ;
#68706 = CARTESIAN_POINT ( 'NONE',  ( 12.22857413548589989, 1435.233796397459855, 150.9813450485239912 ) ) ;
#68707 = B_SPLINE_SURFACE_WITH_KNOTS ( 'NONE', 5, 4, ( 
 ( #15630, #73379, #56578, #108061, #58234 ),
 ( #83413, #5620, #107517, #99100, #91813 ),
 ( #75597, #47624, #100751, #7266, #14551 ),
 ( #6708, #64984, #98560, #92358, #90711 ),
 ( #13997, #48182, #82321, #39771, #48739 ),
 ( #73931, #82864, #6156, #66099, #49284 ) ),
 .UNSPECIFIED., .F., .F., .F.,
 ( 6, 6 ),
 ( 5, 5 ),
 ( 0.000000000000000000, 11.48858425020000062 ),
 ( 40.20365518519999881, 50.26548245740000453 ),
 .UNSPECIFIED. ) ;
#68708 = CARTESIAN_POINT ( 'NONE',  ( -4.071675667009562183, 1441.007006124126065, 184.9002666288488683 ) ) ;
#68709 = CARTESIAN_POINT ( 'NONE',  ( -22.71192893796499845, 1509.726026642720171, 228.1488050769010272 ) ) ;
#68710 = ADVANCED_FACE ( 'NONE', ( #84034 ), #42756, .T. ) ;
#68711 = CARTESIAN_POINT ( 'NONE',  ( -1.443308691599999971, 1409.130619234930009, 186.4549414153979683 ) ) ;
#68712 = CARTESIAN_POINT ( 'NONE',  ( 0.4403324358131759930, 1517.051704035390003, 201.6347831756999938 ) ) ;
#68713 = CARTESIAN_POINT ( 'NONE',  ( 4.238435005652729792, 1441.459264359959889, 163.1404339353370005 ) ) ;
#68715 = CARTESIAN_POINT ( 'NONE',  ( -2.473077522879999712, 1421.063464807129776, 185.4030335298980106 ) ) ;
#68714 = CARTESIAN_POINT ( 'NONE',  ( 2.490245914424999985, 1516.691389976299888, 213.7302634767470124 ) ) ;
#68716 = CARTESIAN_POINT ( 'NONE',  ( 19.94169889329999990, 1509.369061810729818, 188.0276712769979781 ) ) ;
#68717 = CARTESIAN_POINT ( 'NONE',  ( 3.454119916704999849, 1516.594591938570147, 216.8324563732270178 ) ) ;
#68718 = ORIENTED_EDGE ( 'NONE', *, *, #399, .T. ) ;
#68719 = CARTESIAN_POINT ( 'NONE',  ( -12.26996141999999956, 1416.831925117829996, 194.6642422325980135 ) ) ;
#68720 = B_SPLINE_SURFACE_WITH_KNOTS ( 'NONE', 5, 5, ( 
 ( #89111, #110591, #13480, #73975, #12942, #91861 ),
 ( #4028, #14597, #65582, #107010, #56069, #47123 ),
 ( #55530, #72875, #30298, #99694, #14038, #57191 ),
 ( #29750, #81250, #72336, #22420, #38699, #63938 ),
 ( #31402, #22986, #82369, #47670, #108106, #4565 ),
 ( #91315, #38156, #48787, #82911, #64491, #90196 ),
 ( #89656, #98606, #21870, #81798, #6202, #48229 ),
 ( #40354, #98051, #5100, #106466, #56623, #39253 ),
 ( #30849, #23550, #73428, #100271, #90758, #107563 ) ),
 .UNSPECIFIED., .F., .F., .F.,
 ( 6, 3, 6 ),
 ( 6, 6 ),
 ( 3.226035699099999654, 5.548136904300000616, 7.870238109499999801 ),
 ( 0.000000000000000000, 2.000000000000000000 ),
 .UNSPECIFIED. ) ;
#68721 = AXIS2_PLACEMENT_3D ( 'NONE', #92739, #61261, #53961 ) ;
#68722 = CARTESIAN_POINT ( 'NONE',  ( -17.24072850490000164, 1420.216406558149856, 203.6744263160889830 ) ) ;
#68723 = VERTEX_POINT ( 'NONE', #41496 ) ;
#68724 = CARTESIAN_POINT ( 'NONE',  ( 4.209031986870000352, 1421.916286088630159, 184.3722574647979968 ) ) ;
#68725 = FACE_OUTER_BOUND ( 'NONE', #6286, .T. ) ;
#68726 = CARTESIAN_POINT ( 'NONE',  ( 2.700443415718799312, 1524.678872986499300, 176.3824881451254782 ) ) ;
#68727 = CARTESIAN_POINT ( 'NONE',  ( 3.028279354519999966, 1442.219580477389854, 217.5826834191090029 ) ) ;
#68728 = DIRECTION ( 'NONE',  ( 1.755985294532464991E-16, -1.000000000000000000, 1.338183447452830017E-16 ) ) ;
#68729 = CARTESIAN_POINT ( 'NONE',  ( -21.76694865736933693, 1524.152444737676660, 234.8391306143355166 ) ) ;
#68730 = CARTESIAN_POINT ( 'NONE',  ( 17.36591816528652643, 1422.683100631737943, 226.5834436581721434 ) ) ;
#68732 = ADVANCED_FACE ( 'NONE', ( #24647 ), #109796, .T. ) ;
#68731 = DIRECTION ( 'NONE',  ( 0.000000000000000000, 1.000000000000000000, 0.000000000000000000 ) ) ;
#68733 = CARTESIAN_POINT ( 'NONE',  ( -7.372143812753932046, 1458.228344989418474, 215.2092666101164582 ) ) ;
#68734 = CARTESIAN_POINT ( 'NONE',  ( 7.105427357599999217E-15, 1410.913060387329779, 137.0999999980979851 ) ) ;
#68735 = CARTESIAN_POINT ( 'NONE',  ( 43.69322311477699827, 1440.913060359309839, 264.0012025825540150 ) ) ;
#68737 = CARTESIAN_POINT ( 'NONE',  ( -5.292247061280000331, 1391.913060387289988, 203.8075142969990168 ) ) ;
#68736 = CARTESIAN_POINT ( 'NONE',  ( -13.93291478854189869, 1418.292988176089921, 201.4314801882400161 ) ) ;
#68738 = CARTESIAN_POINT ( 'NONE',  ( 11.39042046171206835, 1433.915048304869288, 151.4356557148368552 ) ) ;
#68739 = ORIENTED_EDGE ( 'NONE', *, *, #10303, .F. ) ;
#68740 = CARTESIAN_POINT ( 'NONE',  ( 1.553898488376879827, 1415.492117401580117, 190.8404010663989823 ) ) ;
#68741 = CARTESIAN_POINT ( 'NONE',  ( 22.53878404599999641, 1411.058442739730026, 206.1986151668880041 ) ) ;
#68742 = EDGE_CURVE ( 'NONE', #52693, #67085, #44172, .T. ) ;
#68743 = B_SPLINE_CURVE_WITH_KNOTS ( 'NONE', 3,
 ( #65839, #84270, #32219, #14850, #24353, #51225, #40617, #93750, #41720, #32763, #59639, #110578, #74788, #99957, #108930, #74246, #8107, #50675, #75880, #23798, #110028, #6467, #42274, #33304, #57989, #93219, #101055, #24888, #31659, #23251, #84808, #15399, #49041, #83177, #67499, #7015, #41172, #66946, #101603, #92665, #59095, #36637, #102701, #1383, #52902, #52358, #88155, #104388, #54027, #9233, #19252, #10891, #844, #43390, #70833, #27137, #297, #78640, #2513, #94312, #10321, #42830, #17591, #44495, #18161, #34969, #76991, #34424, #53458, #69151, #86475, #36093, #27685, #70279, #61323, #1955 ),
 .UNSPECIFIED., .F., .F.,
 ( 4, 3, 3, 3, 3, 3, 3, 3, 3, 3, 3, 3, 3, 3, 3, 3, 3, 3, 3, 3, 3, 3, 3, 3, 3, 4 ),
 ( -32.41280709890000367, -32.04800627787870582, -31.23028833932220039, -30.40294656779999727, -29.97571463615929943, -29.17405848693029924, -28.39797230597359956, -27.64057875201519821, -26.91504384857509891, -26.20815561766710289, -25.51808413167499978, -24.82024664080000065, -24.40663526596280164, -23.87734799550889875, -23.33898530432950125, -22.80091041601890112, -22.27434435385609746, -21.75967651710000084, -21.56181898327110247, -21.07938793902939878, -20.58798065129229826, -20.09329540484139898, -19.59996587401529666, -19.11219011100000031, -18.70494888627219865, -18.22829625880000037 ),
 .UNSPECIFIED. ) ;
#68744 = CARTESIAN_POINT ( 'NONE',  ( -27.74496046000000149, 1507.996570526829828, 210.5130752751180125 ) ) ;
#68745 = CARTESIAN_POINT ( 'NONE',  ( 2.640159921366920681, 1410.383150405935567, 185.6143680615537335 ) ) ;
#68746 = CARTESIAN_POINT ( 'NONE',  ( -10.37617513879240150, 1479.403831811299824, 210.6295454707710064 ) ) ;
#68747 = B_SPLINE_SURFACE_WITH_KNOTS ( 'NONE', 5, 5, ( 
 ( #85680, #603, #58845, #67263, #35287, #86236 ),
 ( #16252, #33610, #24645, #43148, #94635, #92979 ),
 ( #33072, #68367, #26319, #34732, #84580, #67807 ),
 ( #69472, #59963, #60511, #50456, #59411, #42039 ),
 ( #76191, #110338, #101918, #8415, #42587, #103592 ),
 ( #50997, #43695, #93524, #26892, #61082, #16793 ),
 ( #76740, #51, #77848, #95197, #102474, #25764 ),
 ( #68923, #18457, #17347, #52655, #17909, #103023 ),
 ( #75654, #86792, #41494, #109793, #104695, #55412 ) ),
 .UNSPECIFIED., .F., .F., .F.,
 ( 6, 3, 6 ),
 ( 6, 6 ),
 ( 9.378668589109999232, 19.09106091769999836, 27.09462474520000086 ),
 ( 0.000000000000000000, 2.000000000000000000 ),
 .UNSPECIFIED. ) ;
#68748 = CARTESIAN_POINT ( 'NONE',  ( 6.232532001850000114, 1407.162969929529936, 220.5304192662980256 ) ) ;
#68749 = ADVANCED_FACE ( 'NONE', ( #25209 ), #68925, .T. ) ;
#68750 = CARTESIAN_POINT ( 'NONE',  ( -1.952265610894980075, 1487.388746950699897, 219.9076763016360019 ) ) ;
#68751 = CARTESIAN_POINT ( 'NONE',  ( -19.86622903030000131, 1443.388330262490172, 213.1207022696590059 ) ) ;
#68752 = CARTESIAN_POINT ( 'NONE',  ( -57.10737429603420168, 1383.800764999470175, 275.4500855170770137 ) ) ;
#68753 = CARTESIAN_POINT ( 'NONE',  ( -0.004285587994040000043, 1452.913210043629988, 152.9532950659979917 ) ) ;
#68754 = CARTESIAN_POINT ( 'NONE',  ( -28.77730029287999969, 1509.917985857419808, 212.2396942430650029 ) ) ;
#68755 = DIRECTION ( 'NONE',  ( 5.980589973904019347E-17, -1.000000000000000000, 1.736889445713099699E-16 ) ) ;
#68757 = ORIENTED_EDGE ( 'NONE', *, *, #73521, .T. ) ;
#68756 = CARTESIAN_POINT ( 'NONE',  ( 10.57208727109580160, 1452.520229422010061, 209.3749135230609966 ) ) ;
#68758 = CARTESIAN_POINT ( 'NONE',  ( -18.41476513140925064, 1458.949142990964219, 227.7116331479677740 ) ) ;
#68759 = CARTESIAN_POINT ( 'NONE',  ( -63.55875838910000653, 1381.694990308149954, 254.4830528533589700 ) ) ;
#68760 = CARTESIAN_POINT ( 'NONE',  ( -16.81208394469999945, 1409.500151295429987, 223.9875056278980026 ) ) ;
#68761 = ORIENTED_EDGE ( 'NONE', *, *, #25557, .T. ) ;
#68762 = ORIENTED_EDGE ( 'NONE', *, *, #108978, .T. ) ;
#68763 = CARTESIAN_POINT ( 'NONE',  ( 19.26614117215169841, 1508.824729876830133, 229.9165145868500133 ) ) ;
#68764 = B_SPLINE_CURVE_WITH_KNOTS ( 'NONE', 3,
 ( #110336, #24103, #49896, #84578, #25205, #90775, #39831, #100287, #108124, #31418, #65600, #99713, #83470 ),
 .UNSPECIFIED., .F., .F.,
 ( 4, 3, 3, 3, 4 ),
 ( -1.703847294900000087, -0.8071511513289990614, 0.08392122703059357036, 0.9654601872785679717, 1.703847294900000087 ),
 .UNSPECIFIED. ) ;
#68765 = CARTESIAN_POINT ( 'NONE',  ( -31.64580750758060645, 1523.313115944345327, 196.3083633854965626 ) ) ;
#68766 = CARTESIAN_POINT ( 'NONE',  ( 39.65501738910209895, 1440.824868566870009, 136.8092738732900102 ) ) ;
#68768 = CARTESIAN_POINT ( 'NONE',  ( -43.15848718719999511, 1446.267105529279888, 263.9122466480980620 ) ) ;
#68767 = DIRECTION ( 'NONE',  ( 0.7454942576402815435, 0.000000000000000000, 0.6665120492724536660 ) ) ;
#68769 = EDGE_CURVE ( 'NONE', #61609, #30006, #6219, .T. ) ;
#68770 = AXIS2_PLACEMENT_3D ( 'NONE', #94968, #18237, #50224 ) ;
#68771 = CARTESIAN_POINT ( 'NONE',  ( 9.025697246586840805, 1436.232127817869923, 209.4982936030500014 ) ) ;
#68772 = CARTESIAN_POINT ( 'NONE',  ( -108.2161777049999927, 1381.376084645610035, 298.2029669646590264 ) ) ;
#68773 = CARTESIAN_POINT ( 'NONE',  ( -12.71745976146490342, 1435.880823605873275, 150.8653729509765355 ) ) ;
#68774 = CARTESIAN_POINT ( 'NONE',  ( -20.93293658309999827, 1485.999516591429938, 191.6309104264979908 ) ) ;
#68775 = CARTESIAN_POINT ( 'NONE',  ( 1.629670625839999998, 1408.969969738429882, 186.3700264965980011 ) ) ;
#68776 = CARTESIAN_POINT ( 'NONE',  ( 16.78480385485652704, 1526.748660780343471, 181.5273693450637040 ) ) ;
#68778 = EDGE_CURVE ( 'NONE', #1325, #12333, #24840, .T. ) ;
#68777 = CARTESIAN_POINT ( 'NONE',  ( -8.002862407569999448, 1439.449515582499998, 153.7646872161979843 ) ) ;
#68779 = CARTESIAN_POINT ( 'NONE',  ( 12.84239758539999876, 1435.935717715699866, 150.8114787689980005 ) ) ;
#68780 = CARTESIAN_POINT ( 'NONE',  ( -16.26820474405350225, 1420.723844530150018, 203.3064050127150040 ) ) ;
#68781 = CIRCLE ( 'NONE', #59817, 4.000000000000003553 ) ;
#68782 = FACE_OUTER_BOUND ( 'NONE', #58512, .T. ) ;
#68783 = CARTESIAN_POINT ( 'NONE',  ( 2.004165785690000146, 1464.806852714229990, 237.1135893016980276 ) ) ;
#68784 = ORIENTED_EDGE ( 'NONE', *, *, #107689, .T. ) ;
#68785 = CARTESIAN_POINT ( 'NONE',  ( 18.28526225389999738, 1474.357479485790009, 194.7997304761989881 ) ) ;
#68786 = CARTESIAN_POINT ( 'NONE',  ( -37.16667942899999844, 1455.848356743629893, 269.8045258284980150 ) ) ;
#68787 = CARTESIAN_POINT ( 'NONE',  ( -26.92291386341319992, 1446.493256825939852, 137.3410762857710097 ) ) ;
#68788 = CARTESIAN_POINT ( 'NONE',  ( 3.687149994097108433E-15, 1522.051704408389924, 239.2297105040643714 ) ) ;
#68789 = CARTESIAN_POINT ( 'NONE',  ( -6.677286941980000279, 1473.976478301389989, 206.5095183912090135 ) ) ;
#68790 = CARTESIAN_POINT ( 'NONE',  ( -7.626016305360259571E-09, 1472.553150102269910, 260.2551601210919898 ) ) ;
#68791 = CARTESIAN_POINT ( 'NONE',  ( -12.78943302956389871, 1502.708798875820094, 209.0180534851929792 ) ) ;
#68792 = CARTESIAN_POINT ( 'NONE',  ( -0.9088213736110000163, 1416.535385209229844, 228.0150015372980192 ) ) ;
#68793 = CARTESIAN_POINT ( 'NONE',  ( -9.980081002260000389, 1419.601693820030050, 231.3438068025980101 ) ) ;
#68794 = CARTESIAN_POINT ( 'NONE',  ( -3.152270393760000289, 1474.954422226189990, 198.1306180379989996 ) ) ;
#68795 = CARTESIAN_POINT ( 'NONE',  ( -104.7362624609999955, 1389.320518635239978, 307.7539050006589605 ) ) ;
#68796 = CARTESIAN_POINT ( 'NONE',  ( -0.2368219676957374342, 1485.961491073400111, 181.8351824008125561 ) ) ;
#68797 = CARTESIAN_POINT ( 'NONE',  ( 4.507237278552312709, 1359.634735991508478, 210.6218459617030021 ) ) ;
#68798 = CARTESIAN_POINT ( 'NONE',  ( -46.11102460466209862, 1439.417470722359894, 268.2058513100960226 ) ) ;
#68799 = CARTESIAN_POINT ( 'NONE',  ( -3.600923890900000313, 1431.488321968289938, 185.7685271587979798 ) ) ;
#68800 = CARTESIAN_POINT ( 'NONE',  ( -7.713704896070000316, 1426.546663328330169, 206.3890337723190100 ) ) ;
#68801 = ORIENTED_EDGE ( 'NONE', *, *, #6539, .T. ) ;
#68802 = CARTESIAN_POINT ( 'NONE',  ( 4.042388501175000037, 1517.045004075700035, 209.8579434088520088 ) ) ;
#68803 = CARTESIAN_POINT ( 'NONE',  ( -14.14948096550000045, 1390.186770710789915, 206.8378643784789972 ) ) ;
#68804 = CARTESIAN_POINT ( 'NONE',  ( -26.07583950859109834, 1441.264734016169996, 138.1452376982360022 ) ) ;
#68805 = CARTESIAN_POINT ( 'NONE',  ( 7.528229201135600235, 1425.827014894030071, 212.2334219967879960 ) ) ;
#68806 = CARTESIAN_POINT ( 'NONE',  ( -26.81127850451720107, 1451.960562951069960, 135.1661831948950123 ) ) ;
#68807 = VERTEX_POINT ( 'NONE', #101922 ) ;
#68808 = CARTESIAN_POINT ( 'NONE',  ( -15.59201085679999998, 1506.806593688130079, 193.4620896933980134 ) ) ;
#68810 = CARTESIAN_POINT ( 'NONE',  ( 15.65975626840000068, 1506.806593688130079, 193.5298351049979999 ) ) ;
#68809 = CARTESIAN_POINT ( 'NONE',  ( -2.385609657825171315, 1525.697946996622932, 177.1458771778526398 ) ) ;
#68811 = AXIS2_PLACEMENT_3D ( 'NONE', #28054, #44327, #37006 ) ;
#68812 = CARTESIAN_POINT ( 'NONE',  ( 3.191256178858096426, 1486.666090685424251, 219.4504335181268289 ) ) ;
#68813 = CARTESIAN_POINT ( 'NONE',  ( -23.83765245656579879, 1446.530553801166661, 215.3656821588423611 ) ) ;
#68814 = CARTESIAN_POINT ( 'NONE',  ( 7.898683012529999381, 1423.849047743189885, 212.3277966039590012 ) ) ;
#68815 = CARTESIAN_POINT ( 'NONE',  ( -2.173216434189999990, 1456.191253960590075, 215.4656985532890019 ) ) ;
#68816 = LINE ( 'NONE', #59854, #90068 ) ;
#68817 = ORIENTED_EDGE ( 'NONE', *, *, #41315, .T. ) ;
#68818 = CARTESIAN_POINT ( 'NONE',  ( -1.210091630371270099, 1409.788755468769750, 270.0714238039610109 ) ) ;
#68819 = CARTESIAN_POINT ( 'NONE',  ( -1.715109485185000171, 1516.963431999339946, 208.3866188148990091 ) ) ;
#68820 = CARTESIAN_POINT ( 'NONE',  ( 13.36103377078690002, 1421.223394105900070, 230.7424813387619906 ) ) ;
#68821 = CARTESIAN_POINT ( 'NONE',  ( 8.062481262145620775, 1436.236301647820028, 206.1279573699050047 ) ) ;
#68823 = ORIENTED_EDGE ( 'NONE', *, *, #5131, .T. ) ;
#68822 = CARTESIAN_POINT ( 'NONE',  ( -3.549497098556182006, 1367.915870260280144, 210.6218459617142003 ) ) ;
#68824 = ORIENTED_EDGE ( 'NONE', *, *, #20739, .T. ) ;
#68825 = CARTESIAN_POINT ( 'NONE',  ( -23.64789126648100037, 1411.111376611279866, 210.3824361856959797 ) ) ;
#68826 = CARTESIAN_POINT ( 'NONE',  ( -3.985554679939999900, 1423.989648005430126, 184.8079733748980118 ) ) ;
#68827 = CARTESIAN_POINT ( 'NONE',  ( -109.9849338725829995, 1384.911448804600013, 311.4561116875739799 ) ) ;
#68828 = CARTESIAN_POINT ( 'NONE',  ( -11.01124415049999961, 1428.984115384829920, 91.31218443469779800 ) ) ;
#68829 = CARTESIAN_POINT ( 'NONE',  ( -18.21027245059960009, 1417.630028607339909, 195.0416608005989758 ) ) ;
#68830 = CARTESIAN_POINT ( 'NONE',  ( -17.60168979070000006, 1415.862843299730002, 225.8220616334979809 ) ) ;
#68831 = CARTESIAN_POINT ( 'NONE',  ( 35.28102380709319874, 1462.674111978580186, 269.2449631940870063 ) ) ;
#68832 = CARTESIAN_POINT ( 'NONE',  ( -2.627082428580422846, 1466.871129784743061, 235.1219302449402448 ) ) ;
#68833 = CARTESIAN_POINT ( 'NONE',  ( -16.37191349014004516, 1421.177096782927265, 227.0079739609353737 ) ) ;
#68834 = CARTESIAN_POINT ( 'NONE',  ( 4.028307740155000261, 1516.797038924770050, 205.8554964580370097 ) ) ;
#68835 = VERTEX_POINT ( 'NONE', #29099 ) ;
#68836 = CARTESIAN_POINT ( 'NONE',  ( 18.75318093336727898, 1458.167641362951599, 227.2642414340100743 ) ) ;
#68837 = CARTESIAN_POINT ( 'NONE',  ( 2.252366801017199993, 1445.834810329979973, 199.2768572914679908 ) ) ;
#68838 = CARTESIAN_POINT ( 'NONE',  ( 0.000000000000000000, 1395.913060387330006, 215.6218459616979999 ) ) ;
#68839 = VERTEX_POINT ( 'NONE', #9529 ) ;
#68840 = CARTESIAN_POINT ( 'NONE',  ( 4.492641941105749659, 1508.880976867409800, 206.0044425539609847 ) ) ;
#68841 = CARTESIAN_POINT ( 'NONE',  ( 26.44176926394449723, 1451.249329871009877, 136.3297133206949923 ) ) ;
#68842 = CARTESIAN_POINT ( 'NONE',  ( -4.141018396419839931, 1508.551704408389924, 213.4853617037059905 ) ) ;
#68843 = CARTESIAN_POINT ( 'NONE',  ( -5.991971352970000275, 1388.626171318960132, 216.9651239126190205 ) ) ;
#68844 = CARTESIAN_POINT ( 'NONE',  ( -9.071295794445763505, 1385.910742335272971, 218.5589077471069857 ) ) ;
#68846 = B_SPLINE_SURFACE_WITH_KNOTS ( 'NONE', 5, 5, ( 
 ( #70131, #84668, #110433, #7967, #61178, #16888 ),
 ( #42134, #67905, #34275, #68456, #104243, #94732 ),
 ( #85778, #26417, #102014, #10177, #44351, #9078 ),
 ( #59498, #60610, #51093, #52204, #9617, #43786 ),
 ( #69569, #35380, #103688, #26989, #95295, #88555 ),
 ( #91152, #62268, #96398, #45468, #2914, #44917 ),
 ( #105348, #65428, #97494, #105908, #20762, #40199 ),
 ( #37031, #19105, #74382, #80696, #63378, #36484 ),
 ( #46561, #79610, #28081, #80139, #99535, #54961 ) ),
 .UNSPECIFIED., .F., .F., .F.,
 ( 6, 3, 6 ),
 ( 6, 6 ),
 ( 14.15949905700000144, 24.81975873950000278, 34.67967148589999482 ),
 ( 0.000000000000000000, 2.000000000000000000 ),
 .UNSPECIFIED. ) ;
#68845 = CARTESIAN_POINT ( 'NONE',  ( 17.95574905190000337, 1409.540088961029824, 195.3910318465979969 ) ) ;
#68847 = CARTESIAN_POINT ( 'NONE',  ( 20.75326766870000128, 1443.913060387330006, 176.0807405191980024 ) ) ;
#68848 = VECTOR ( 'NONE', #31629, 1000.000000000000000 ) ;
#68849 = CARTESIAN_POINT ( 'NONE',  ( 3.854469939346678142, 1439.700967340914303, 184.6638362761631527 ) ) ;
#68851 = CARTESIAN_POINT ( 'NONE',  ( -22.48437655502024057, 1431.424403463011231, 216.6260149409388305 ) ) ;
#68850 = CARTESIAN_POINT ( 'NONE',  ( 1.157712740350000047, 1416.622647982630042, 233.3632169813980113 ) ) ;
#68852 = CARTESIAN_POINT ( 'NONE',  ( 0.9798719467442907893, 1451.400798846600082, 182.8910064217580214 ) ) ;
#68853 = CARTESIAN_POINT ( 'NONE',  ( -0.02546055715129019736, 1508.875231489110092, 179.6647779767779980 ) ) ;
#68854 = LINE ( 'NONE', #102958, #28298 ) ;
#68855 = CIRCLE ( 'NONE', #36628, 26.00000000000000711 ) ;
#68856 = CARTESIAN_POINT ( 'NONE',  ( 17.04824238339829634, 1423.676546790900147, 228.9394188427949928 ) ) ;
#68857 = VERTEX_POINT ( 'NONE', #53786 ) ;
#68858 = CARTESIAN_POINT ( 'NONE',  ( 12.86122366611430046, 1416.830086716310007, 221.8629622564060071 ) ) ;
#68859 = TOROIDAL_SURFACE ( 'NONE', #102536, 32.13701971169416538, 1.000000000000000000 ) ;
#68860 = DIRECTION ( 'NONE',  ( -0.6736849260863840838, 0.000000000000000000, 0.7390186874254150995 ) ) ;
#68861 = CARTESIAN_POINT ( 'NONE',  ( -0.5142297307823490149, 1410.274753841589927, 233.1699704715869927 ) ) ;
#68862 = CARTESIAN_POINT ( 'NONE',  ( -10.22261203090000059, 1388.971412213310032, 201.9214163269789992 ) ) ;
#68863 = CARTESIAN_POINT ( 'NONE',  ( 8.389454068704580436, 1423.883216928779802, 211.4473611657970196 ) ) ;
#68864 = CARTESIAN_POINT ( 'NONE',  ( -0.6927649375505723350, 1420.881850026484017, 193.7326374981037702 ) ) ;
#68865 = CARTESIAN_POINT ( 'NONE',  ( -4.327986479516029661, 1515.120635733899917, 208.2727843191470072 ) ) ;
#68866 = EDGE_CURVE ( 'NONE', #100464, #44452, #82126, .T. ) ;
#68867 = CARTESIAN_POINT ( 'NONE',  ( -39.47393889809999479, 1455.502555575530096, 271.1218459616979999 ) ) ;
#68868 = CARTESIAN_POINT ( 'NONE',  ( -9.005778233164750901, 1384.117648528409973, 218.5947890724640104 ) ) ;
#68870 = ADVANCED_FACE ( 'NONE', ( #80049 ), #10085, .F. ) ;
#68869 = CARTESIAN_POINT ( 'NONE',  ( 11.05013786159999967, 1433.657746916940141, 151.7238025743979790 ) ) ;
#68871 = CARTESIAN_POINT ( 'NONE',  ( 22.74199303559999663, 1446.314437877210139, 234.3916895436979928 ) ) ;
#68872 = B_SPLINE_SURFACE_WITH_KNOTS ( 'NONE', 5, 5, ( 
 ( #88008, #45998, #28070, #2358, #2903, #29178 ),
 ( #87440, #44908, #54411, #63369, #43778, #104232 ),
 ( #36473, #62259, #20752, #79599, #9607, #96387 ),
 ( #97484, #86875, #1235, #11290, #86323, #19664 ),
 ( #10169, #53869, #45457, #71215, #105337, #28628 ),
 ( #96946, #20212, #18547, #11828, #44342, #80129 ) ),
 .UNSPECIFIED., .F., .F., .F.,
 ( 6, 6 ),
 ( 6, 6 ),
 ( 118.7831216769999969, 123.7287573859999981 ),
 ( 0.000000000000000000, 2.000000000000000000 ),
 .UNSPECIFIED. ) ;
#68873 = CARTESIAN_POINT ( 'NONE',  ( 12.85343379848070100, 1416.225364278609959, 196.3904799426800025 ) ) ;
#68874 = CARTESIAN_POINT ( 'NONE',  ( -14.22051243745750071, 1421.364670842500118, 196.1737613524439894 ) ) ;
#68875 = B_SPLINE_CURVE_WITH_KNOTS ( 'NONE', 3,
 ( #85682, #24107, #34184, #26322, #33074, #17350, #102477 ),
 .UNSPECIFIED., .F., .F.,
 ( 4, 3, 4 ),
 ( 0.000000000000000000, 0.0008424868321600594316, 0.002213898725977839644 ),
 .UNSPECIFIED. ) ;
#68876 = CARTESIAN_POINT ( 'NONE',  ( 10.03630746922679862, 1421.534750384480049, 198.5668548094549806 ) ) ;
#68877 = CARTESIAN_POINT ( 'NONE',  ( -15.06279246576909259, 1422.388300736680321, 229.4662110716209327 ) ) ;
#68878 = CARTESIAN_POINT ( 'NONE',  ( -3.511104830509999886, 1486.134592826630069, 181.9823189358980073 ) ) ;
#68879 = CARTESIAN_POINT ( 'NONE',  ( 12.73679432148881574, 1398.290618096285471, 206.5085731043449755 ) ) ;
#68880 = CARTESIAN_POINT ( 'NONE',  ( 0.05322450152090000414, 1509.045416624730024, 239.1217102979979643 ) ) ;
#68881 = CARTESIAN_POINT ( 'NONE',  ( -8.118430090829926726, 1425.413100047793023, 208.7305073936668691 ) ) ;
#68882 = ADVANCED_FACE ( 'NONE', ( #71703 ), #20668, .F. ) ;
#68883 = CARTESIAN_POINT ( 'NONE',  ( 3.503070653725943284, 1446.464826921931717, 170.5350607410328507 ) ) ;
#68884 = CARTESIAN_POINT ( 'NONE',  ( 26.72339292633054342, 1436.753392519305862, 136.7836805358251411 ) ) ;
#68885 = CARTESIAN_POINT ( 'NONE',  ( -1.114108910779999961, 1515.531799303389789, 205.0293305988190014 ) ) ;
#68886 = FACE_OUTER_BOUND ( 'NONE', #254, .T. ) ;
#68887 = AXIS2_PLACEMENT_3D ( 'NONE', #24435, #31746, #58623 ) ;
#68888 = CARTESIAN_POINT ( 'NONE',  ( 22.14279729195780178, 1473.984189419150198, 210.1089391048309949 ) ) ;
#68889 = CARTESIAN_POINT ( 'NONE',  ( 2.878693249144999466, 1516.766397346390022, 213.1495431961470217 ) ) ;
#68890 = CARTESIAN_POINT ( 'NONE',  ( -15.99159030839580176, 1420.231971570089854, 209.2067213653590159 ) ) ;
#68891 = CARTESIAN_POINT ( 'NONE',  ( 0.1631646649216179912, 1484.369741073460091, 181.9066623653069996 ) ) ;
#68893 = ORIENTED_EDGE ( 'NONE', *, *, #107785, .F. ) ;
#68892 = DIRECTION ( 'NONE',  ( 0.6212649842969746317, 0.04409479819909335047, -0.7823589125575685088 ) ) ;
#68894 = CARTESIAN_POINT ( 'NONE',  ( 11.21032122953132948, 1517.151704408390060, 188.3716648695481695 ) ) ;
#68895 = CARTESIAN_POINT ( 'NONE',  ( -33.46247258405923475, 1444.994950788469168, 154.5793418554282539 ) ) ;
#68896 = CARTESIAN_POINT ( 'NONE',  ( -9.258583944369999847E-15, 1443.913060387330006, 150.8032249175980155 ) ) ;
#68897 = CARTESIAN_POINT ( 'NONE',  ( -32.05679137160737469, 1524.478200376968744, 216.6895106740730625 ) ) ;
#68898 = CARTESIAN_POINT ( 'NONE',  ( -109.5349683309999875, 1384.900884850210105, 297.1231244331590347 ) ) ;
#68899 = ORIENTED_EDGE ( 'NONE', *, *, #96519, .F. ) ;
#68900 = CARTESIAN_POINT ( 'NONE',  ( -11.41020920480000100, 1470.800728306390056, 208.9610728516699965 ) ) ;
#68901 = AXIS2_PLACEMENT_3D ( 'NONE', #103469, #95638, #19470 ) ;
#68902 = CARTESIAN_POINT ( 'NONE',  ( -12.18719547259109959, 1391.620637730509998, 211.5989438970109973 ) ) ;
#68903 = CARTESIAN_POINT ( 'NONE',  ( -12.97490759070000088, 1414.913060387329779, 220.5751958562979951 ) ) ;
#68904 = CARTESIAN_POINT ( 'NONE',  ( -21.96543842109140954, 1523.313115944345100, 235.2592135320311399 ) ) ;
#68905 = CARTESIAN_POINT ( 'NONE',  ( -4.072722851587129433, 1432.588601696869773, 216.5672232244940005 ) ) ;
#68906 = CARTESIAN_POINT ( 'NONE',  ( -109.4677423672981575, 1382.863364883987970, 311.1289870959311656 ) ) ;
#68907 = CARTESIAN_POINT ( 'NONE',  ( 1.842963219480119985, 1515.064792700640055, 213.4512947425059792 ) ) ;
#68908 = DIRECTION ( 'NONE',  ( 0.9361323810649732069, 0.3043587179164370382, 0.1761304515121860370 ) ) ;
#68909 = CARTESIAN_POINT ( 'NONE',  ( -12.45388125799999912, 1391.576963816120042, 208.7046256454329978 ) ) ;
#68910 = CARTESIAN_POINT ( 'NONE',  ( -83.03005440452790253, 1385.169125049510058, 286.7572543505270346 ) ) ;
#68911 = EDGE_CURVE ( 'NONE', #80799, #4488, #105589, .T. ) ;
#68912 = CARTESIAN_POINT ( 'NONE',  ( -17.60565864420000182, 1410.875688248029974, 193.0296143146979944 ) ) ;
#68913 = CYLINDRICAL_SURFACE ( 'NONE', #68032, 1.000000000000000888 ) ;
#68914 = ORIENTED_EDGE ( 'NONE', *, *, #63819, .T. ) ;
#68915 = CARTESIAN_POINT ( 'NONE',  ( 17.22592482065197927, 1443.501467202829190, 162.9227486220069920 ) ) ;
#68917 = ORIENTED_EDGE ( 'NONE', *, *, #2209, .T. ) ;
#68916 = CARTESIAN_POINT ( 'NONE',  ( -2.370970874524634286, 1427.002265528474027, 137.0999999980979567 ) ) ;
#68918 = CARTESIAN_POINT ( 'NONE',  ( -11.41961239078290191, 1507.432264719158638, 233.9077293063710385 ) ) ;
#68919 = ORIENTED_EDGE ( 'NONE', *, *, #48439, .F. ) ;
#68920 = ADVANCED_FACE ( 'NONE', ( #43697 ), #32060, .T. ) ;
#68921 = CARTESIAN_POINT ( 'NONE',  ( -18.56563103275550120, 1441.651807245909822, 211.5798049646579955 ) ) ;
#68922 = CARTESIAN_POINT ( 'NONE',  ( -8.047699957360343603, 1364.705686786927117, 208.3718459617061285 ) ) ;
#68923 = CARTESIAN_POINT ( 'NONE',  ( -6.192225852249999996, 1496.322100554489907, 199.7152199997689763 ) ) ;
#68924 = DIRECTION ( 'NONE',  ( -0.000000000000000000, -1.000000000000000000, -0.000000000000000000 ) ) ;
#68925 = CYLINDRICAL_SURFACE ( 'NONE', #9012, 0.9999999999999880096 ) ;
#68926 = CARTESIAN_POINT ( 'NONE',  ( 5.776215007970000315, 1396.296062261630141, 219.5799249200979943 ) ) ;
#68927 = CARTESIAN_POINT ( 'NONE',  ( 2.797255426280000012, 1417.697071498429978, 234.5789349732979758 ) ) ;
#68928 = DIRECTION ( 'NONE',  ( 0.000000000000000000, 1.000000000000000000, 0.000000000000000000 ) ) ;
#68929 = CARTESIAN_POINT ( 'NONE',  ( -106.6287828259400072, 1306.483669372790246, 297.4506287831988516 ) ) ;
#68930 = CARTESIAN_POINT ( 'NONE',  ( -4.928286345013006553, 1370.785306328871684, 208.3718459617010978 ) ) ;
#68931 = CARTESIAN_POINT ( 'NONE',  ( -2.409586283469999923, 1426.663880916129983, 144.1938086916980239 ) ) ;
#68932 = CARTESIAN_POINT ( 'NONE',  ( 3.252530615595000452, 1516.827328999679821, 206.2418890071470230 ) ) ;
#68933 = DIRECTION ( 'NONE',  ( -1.755985294532469921E-16, 1.000000000000000000, -1.338183447452831989E-16 ) ) ;
#68934 = CARTESIAN_POINT ( 'NONE',  ( -2.500000000000000000, 1438.970653384089928, 157.7201897330980103 ) ) ;
#68935 = CARTESIAN_POINT ( 'NONE',  ( 43.39686093150000090, 1451.895030900229813, 269.7191771298979575 ) ) ;
#68937 = ORIENTED_EDGE ( 'NONE', *, *, #109189, .F. ) ;
#68936 = CARTESIAN_POINT ( 'NONE',  ( -1.337955765360000049, 1494.783074254390158, 220.2332542844989973 ) ) ;
#68938 = CARTESIAN_POINT ( 'NONE',  ( 10.79382269979189957, 1414.913060387349788, 222.1041130917409987 ) ) ;
#68939 = VERTEX_POINT ( 'NONE', #31845 ) ;
#68940 = CARTESIAN_POINT ( 'NONE',  ( -16.38124167859501412, 1514.407859703122313, 223.7133277291391664 ) ) ;
#68941 = CARTESIAN_POINT ( 'NONE',  ( -24.30946323690000099, 1430.356462489929982, 206.1914330134380009 ) ) ;
#68944 = CARTESIAN_POINT ( 'NONE',  ( 17.25149442856769610, 1410.459880232700243, 192.3767002299429976 ) ) ;
#68943 = AXIS2_PLACEMENT_3D ( 'NONE', #37219, #88729, #71416 ) ;
#68942 = CARTESIAN_POINT ( 'NONE',  ( -11.30626018579999936, 1426.878239686230017, 113.0072544287980065 ) ) ;
#68945 = CARTESIAN_POINT ( 'NONE',  ( 0.01319650876840149957, 1516.941178807709775, 211.4140629809269853 ) ) ;
#68946 = CARTESIAN_POINT ( 'NONE',  ( 29.87053939714199657, 1510.066426918421257, 204.8311492353107894 ) ) ;
#68947 = CARTESIAN_POINT ( 'NONE',  ( -21.19319384159999942, 1471.316885392730001, 208.3912962420869803 ) ) ;
#68948 = CARTESIAN_POINT ( 'NONE',  ( -14.25478412350000212, 1406.894180200230267, 267.1909259577980151 ) ) ;
#68949 = CARTESIAN_POINT ( 'NONE',  ( 19.39560819206040065, 1509.616854481060045, 231.5472923800719798 ) ) ;
#68950 = CARTESIAN_POINT ( 'NONE',  ( 28.43277596785110006, 1508.901247230659919, 209.4404433710649869 ) ) ;
#68951 = CARTESIAN_POINT ( 'NONE',  ( -5.236048985779999221, 1391.923671604790115, 214.6057402034190034 ) ) ;
#68952 = CARTESIAN_POINT ( 'NONE',  ( -39.00494972961689655, 1439.722668488820091, 136.7021091258499723 ) ) ;
#68953 = ORIENTED_EDGE ( 'NONE', *, *, #80990, .T. ) ;
#68954 = FACE_OUTER_BOUND ( 'NONE', #92695, .T. ) ;
#68955 = CARTESIAN_POINT ( 'NONE',  ( 9.505847783012139729, 1461.812439321519832, 207.0696516400899725 ) ) ;
#68956 = CARTESIAN_POINT ( 'NONE',  ( -17.39471470580000201, 1458.587118211430152, 228.8964261825979918 ) ) ;
#68957 = EDGE_LOOP ( 'NONE', ( #1983, #52448, #63071, #62018, #31194 ) ) ;
#68958 = VERTEX_POINT ( 'NONE', #108555 ) ;
#68959 = CARTESIAN_POINT ( 'NONE',  ( -29.36423093692776121, 1509.941268890160018, 211.4558441758299523 ) ) ;
#68960 = CARTESIAN_POINT ( 'NONE',  ( -6.305024129259999555, 1422.156209412130011, 144.1468801376980196 ) ) ;
#68961 = B_SPLINE_CURVE_WITH_KNOTS ( 'NONE', 5,
 ( #23273, #84295, #24374, #110052, #48511, #50167, #15418, #49609, #84828, #57470, #22703, #33326 ),
 .UNSPECIFIED., .F., .F.,
 ( 6, 3, 3, 6 ),
 ( -8.912489289840001661, -7.801458206499999548, -6.062162762929999893, -3.672001930560000460 ),
 .UNSPECIFIED. ) ;
#68962 = VERTEX_POINT ( 'NONE', #38585 ) ;
#68963 = DIRECTION ( 'NONE',  ( 0.000000000000000000, -0.8724564897876813108, -0.4886917979947663637 ) ) ;
#68964 = CARTESIAN_POINT ( 'NONE',  ( -10.34027448514628489, 1418.149532852553193, 197.7030072931336235 ) ) ;
#68965 = CARTESIAN_POINT ( 'NONE',  ( -0.7790226144181949808, 1442.687261678630193, 200.2740145696140246 ) ) ;
#68966 = CARTESIAN_POINT ( 'NONE',  ( 26.87217692225963361, 1508.240760517084027, 206.2294961738559778 ) ) ;
#68967 = CARTESIAN_POINT ( 'NONE',  ( 1.435143914157240186, 1420.925611785209867, 183.0242435332739888 ) ) ;
#68968 = VECTOR ( 'NONE', #67629, 1000.000000000000114 ) ;
#68969 = CARTESIAN_POINT ( 'NONE',  ( 9.628418581815711974, 1451.441045534420027, 207.9857633263249852 ) ) ;
#68970 = CARTESIAN_POINT ( 'NONE',  ( -11.55222382600000053, 1391.913060387289988, 210.8753015047989834 ) ) ;
#68971 = CARTESIAN_POINT ( 'NONE',  ( -87.47508722668870007, 1384.828440509849770, 290.8377656053449982 ) ) ;
#68972 = EDGE_LOOP ( 'NONE', ( #103895, #45943, #44194, #101001 ) ) ;
#68973 = CARTESIAN_POINT ( 'NONE',  ( 1.123101578415000024, 1517.157901477309906, 203.3331546065870157 ) ) ;
#68974 = CARTESIAN_POINT ( 'NONE',  ( 2.873919002525000099, 1516.940252185109784, 209.1085733957019954 ) ) ;
#68975 = ORIENTED_EDGE ( 'NONE', *, *, #65076, .F. ) ;
#68976 = CARTESIAN_POINT ( 'NONE',  ( 11.81097173189579941, 1428.791000847919804, 148.7051997554240188 ) ) ;
#68977 = CARTESIAN_POINT ( 'NONE',  ( 3.215708743572380790, 1511.798530722473515, 217.0753755202089508 ) ) ;
#68978 = ORIENTED_EDGE ( 'NONE', *, *, #105169, .T. ) ;
#68979 = CARTESIAN_POINT ( 'NONE',  ( 11.83466398051542612, 1517.051704408389924, 190.1848878783540897 ) ) ;
#68980 = CARTESIAN_POINT ( 'NONE',  ( -7.087060292473280398, 1508.534494050320063, 219.4009365383440127 ) ) ;
#68981 = CARTESIAN_POINT ( 'NONE',  ( 11.45019036429999915, 1509.312909845629974, 236.0262225088980017 ) ) ;
#68982 = CIRCLE ( 'NONE', #60021, 2.000000000000003109 ) ;
#68983 = CARTESIAN_POINT ( 'NONE',  ( -3.125914921230999788, 1369.842518795720025, 211.2713650144889925 ) ) ;
#68984 = CARTESIAN_POINT ( 'NONE',  ( -5.528991355650000550, 1423.112510947830060, 186.1101815182979919 ) ) ;
#68985 = CARTESIAN_POINT ( 'NONE',  ( 10.57863187995810073, 1410.707288523929947, 270.0764058261560194 ) ) ;
#68986 = CARTESIAN_POINT ( 'NONE',  ( -8.991629940588330427, 1509.227055023859975, 237.0095830223739881 ) ) ;
#68987 = CARTESIAN_POINT ( 'NONE',  ( -5.898813458170000246, 1474.065724237490031, 199.2881457417290108 ) ) ;
#68988 = CARTESIAN_POINT ( 'NONE',  ( -14.46866624055838990, 1410.791144959253643, 190.4540876299275283 ) ) ;
#68989 = CARTESIAN_POINT ( 'NONE',  ( -44.33415861099999944, 1379.660740675520174, 229.4371355697589649 ) ) ;
#68990 = CARTESIAN_POINT ( 'NONE',  ( -16.57804597599999852, 1485.105086709729903, 223.5480764049980280 ) ) ;
#68992 = CARTESIAN_POINT ( 'NONE',  ( 6.726720322338469948, 1467.543326730849913, 200.2279294393160001 ) ) ;
#68991 = CARTESIAN_POINT ( 'NONE',  ( 17.68181829800000315, 1459.090084424630277, 228.3014959847979810 ) ) ;
#68993 = CARTESIAN_POINT ( 'NONE',  ( -4.871044490860866105, 1423.449036601908119, 184.6413674952053441 ) ) ;
#68994 = DIRECTION ( 'NONE',  ( -0.1455443991891719746, -0.4512270418750849443, -0.8804606660977668531 ) ) ;
#68995 = CARTESIAN_POINT ( 'NONE',  ( -9.789280099085180709, 1501.631186488149979, 228.6396568906859841 ) ) ;
#68996 = ORIENTED_EDGE ( 'NONE', *, *, #58439, .F. ) ;
#68997 = CARTESIAN_POINT ( 'NONE',  ( -4.487249792034999629, 1509.038615934169911, 205.6342535031670025 ) ) ;
#68998 = DIRECTION ( 'NONE',  ( -9.341989762165448955E-47, 1.000000000000000000, -1.836970198721029688E-16 ) ) ;
#68999 = CARTESIAN_POINT ( 'NONE',  ( -2.986641160691798191, 1485.642120341665077, 182.6840798815813685 ) ) ;
#69000 = FACE_OUTER_BOUND ( 'NONE', #1685, .T. ) ;
#69002 = VERTEX_POINT ( 'NONE', #55963 ) ;
#69001 = CARTESIAN_POINT ( 'NONE',  ( 1.273031542862190113, 1515.087982642930001, 204.7930044310420215 ) ) ;
#69003 = CARTESIAN_POINT ( 'NONE',  ( 1.327504031670000195, 1471.309244717329875, 187.7603546987980110 ) ) ;
#69004 = CARTESIAN_POINT ( 'NONE',  ( -15.21149315567410021, 1507.619498552399818, 191.9000986313440364 ) ) ;
#69005 = CARTESIAN_POINT ( 'NONE',  ( -11.23092292039999940, 1427.419555970229794, 149.5756494223980155 ) ) ;
#69006 = CARTESIAN_POINT ( 'NONE',  ( -12.53380580351000084, 1442.773887400870080, 185.9733686700720057 ) ) ;
#69007 = CARTESIAN_POINT ( 'NONE',  ( -10.96786518298100077, 1462.082438629349781, 210.1872772324369976 ) ) ;
#69008 = CARTESIAN_POINT ( 'NONE',  ( -1.191524307911315583, 1526.382868172863937, 239.2353018730792087 ) ) ;
#69009 = CARTESIAN_POINT ( 'NONE',  ( -15.09629036526500023, 1514.287526756679881, 224.4071695879669903 ) ) ;
#69010 = FACE_OUTER_BOUND ( 'NONE', #48159, .T. ) ;
#69012 = CARTESIAN_POINT ( 'NONE',  ( -11.00420836870640073, 1481.586346291950122, 208.5478340898509657 ) ) ;
#69011 = CARTESIAN_POINT ( 'NONE',  ( -22.49156919629999862, 1508.010176357929822, 225.3481774520980139 ) ) ;
#69013 = CARTESIAN_POINT ( 'NONE',  ( -16.78409198796899915, 1460.264608996595825, 228.3353229335820060 ) ) ;
#69014 = CARTESIAN_POINT ( 'NONE',  ( -1.136547623115000016, 1516.839862955080207, 206.6438706166370025 ) ) ;
#69015 = CARTESIAN_POINT ( 'NONE',  ( 18.18323680749999838, 1409.226845187329900, 269.3834355279979604 ) ) ;
#69016 = CARTESIAN_POINT ( 'NONE',  ( 23.93773119740000155, 1435.477561280669761, 138.6590435606979952 ) ) ;
#69017 = CARTESIAN_POINT ( 'NONE',  ( 18.31698807710000310, 1430.307821480030043, 192.4318916728979900 ) ) ;
#69018 = CARTESIAN_POINT ( 'NONE',  ( 21.41666166824317585, 1506.776553316454283, 215.7211524448117359 ) ) ;
#69019 = CIRCLE ( 'NONE', #83292, 2.000000000000003553 ) ;
#69020 = EDGE_CURVE ( 'NONE', #110792, #49383, #11352, .T. ) ;
#69021 = CARTESIAN_POINT ( 'NONE',  ( -0.08826310995340809484, 1508.140386909309882, 237.5604311155479706 ) ) ;
#69022 = CIRCLE ( 'NONE', #20690, 2.000000000000003553 ) ;
#69023 = CARTESIAN_POINT ( 'NONE',  ( -15.15027404274539968, 1418.004900903659973, 203.1594184435460022 ) ) ;
#69024 = CARTESIAN_POINT ( 'NONE',  ( -41.66768437117050183, 1443.241400757599877, 135.6286676937990023 ) ) ;
#69025 = CARTESIAN_POINT ( 'NONE',  ( -18.61615538203637854, 1506.404057884007671, 197.4600136827062613 ) ) ;
#69026 = CARTESIAN_POINT ( 'NONE',  ( 3.024787391539412425E-15, 1523.051704408389696, 184.4225825198192013 ) ) ;
#69027 = CARTESIAN_POINT ( 'NONE',  ( -13.39006534200000154, 1443.300441888700107, 187.2669796394979755 ) ) ;
#69028 = EDGE_CURVE ( 'NONE', #7609, #53641, #12364, .T. ) ;
#69029 = CARTESIAN_POINT ( 'NONE',  ( -14.60782360329999996, 1431.113060387329824, 222.3499097932980249 ) ) ;
#69030 = B_SPLINE_SURFACE_WITH_KNOTS ( 'NONE', 5, 5, ( 
 ( #24241, #50023, #39409, #15819, #65727, #24776 ),
 ( #101490, #90909, #5819, #92014, #48379, #13626 ),
 ( #6357, #48936, #58424, #41618, #107716, #99847 ),
 ( #39958, #23140, #73585, #57344, #23696, #90346 ),
 ( #91468, #75772, #66296, #83600, #83066, #84155 ),
 ( #109922, #65179, #66837, #100412, #6898, #67392 ),
 ( #31000, #33202, #14192, #41054, #40505, #47814 ),
 ( #109383, #81949, #5253, #75233, #99291, #22566 ),
 ( #56771, #93642, #8002, #25334, #50575, #730 ),
 ( #42167, #76320, #94205, #188, #86369, #8550 ),
 ( #43280, #77973, #1845, #84701, #60090, #35420 ),
 ( #58974, #76877, #16377, #42722, #110470, #85816 ),
 ( #60646, #26453, #94770, #17479, #9652, #69050 ),
 ( #93106, #34309, #59530, #77427, #16924, #51126 ),
 ( #103725, #69607, #18591, #52787, #33747, #51679 ),
 ( #68490, #104282, #43826, #70171, #9114, #67942 ),
 ( #102050, #27027, #95330, #34862, #102591, #25891 ),
 ( #103151, #85250, #18047, #52241, #1279, #61215 ),
 ( #86923, #10214, #44392, #78534, #35980, #88052 ),
 ( #27570, #36525, #97534, #53917, #47140, #62885 ),
 ( #55549, #89673, #80736, #71272, #11337, #28119 ) ),
 .UNSPECIFIED., .F., .F., .F.,
 ( 6, 3, 3, 3, 3, 3, 6 ),
 ( 6, 6 ),
 ( 39.80009957240000062, 49.32247488090000331, 52.79489999459999439, 54.53111255139999969, 56.26732510819999789, 56.97897492249999374, 58.84485018950000068 ),
 ( 0.000000000000000000, 1.469182821640000025 ),
 .UNSPECIFIED. ) ;
#69031 = CARTESIAN_POINT ( 'NONE',  ( -30.80659297389999907, 1435.733914001370067, 136.0405333270979895 ) ) ;
#69032 = CARTESIAN_POINT ( 'NONE',  ( -7.898270967410000232, 1498.870872765589866, 219.0971900149289979 ) ) ;
#69033 = VERTEX_POINT ( 'NONE', #76064 ) ;
#69034 = CARTESIAN_POINT ( 'NONE',  ( 5.726916880756410144, 1510.539524128566654, 216.6663165935511017 ) ) ;
#69035 = CARTESIAN_POINT ( 'NONE',  ( -12.85845572773480150, 1409.362087555840162, 216.7356519297030104 ) ) ;
#69036 = CARTESIAN_POINT ( 'NONE',  ( -12.91325991995259947, 1507.673968524629800, 209.2392918421849970 ) ) ;
#69037 = CARTESIAN_POINT ( 'NONE',  ( 17.71193101246160140, 1517.051704408389924, 196.6727161460330251 ) ) ;
#69038 = CARTESIAN_POINT ( 'NONE',  ( -12.72837614330000022, 1474.761265398429941, 267.4694132100979687 ) ) ;
#69039 = CARTESIAN_POINT ( 'NONE',  ( -30.24977872777067844, 1524.075132568165145, 195.7694483101574008 ) ) ;
#69040 = CARTESIAN_POINT ( 'NONE',  ( 32.86470158750937998, 1523.580203803270933, 201.0415738342970542 ) ) ;
#69041 = CARTESIAN_POINT ( 'NONE',  ( -24.27333433320000111, 1509.087578212329845, 222.4402611466979920 ) ) ;
#69042 = CARTESIAN_POINT ( 'NONE',  ( -82.20641648805589341, 1384.634060515750207, 305.2179643079160201 ) ) ;
#69043 = CARTESIAN_POINT ( 'NONE',  ( -11.60963209123129936, 1384.935719060559904, 200.1630794765560211 ) ) ;
#69044 = CARTESIAN_POINT ( 'NONE',  ( 18.80671126632940116, 1425.657109644339926, 226.1563198364650020 ) ) ;
#69045 = CARTESIAN_POINT ( 'NONE',  ( -3.364556988579999963, 1443.913060387330006, 155.8032249175980155 ) ) ;
#69046 = DIRECTION ( 'NONE',  ( 0.9455185755993178454, 0.000000000000000000, -0.3255681544571537578 ) ) ;
#69047 = CARTESIAN_POINT ( 'NONE',  ( 4.324092179320000007, 1515.269353058490196, 209.1218459616989946 ) ) ;
#69048 = CARTESIAN_POINT ( 'NONE',  ( -46.02998242119897299, 1440.913029505377381, 268.4959138949732278 ) ) ;
#69049 = VECTOR ( 'NONE', #37073, 1000.000000000000000 ) ;
#69050 = CARTESIAN_POINT ( 'NONE',  ( -23.46122789450000212, 1411.092679750530124, 206.2085811050380073 ) ) ;
#69051 =( BOUNDED_CURVE ( )  B_SPLINE_CURVE ( 3, ( #46441, #20102, #20634, #54294 ),
 .UNSPECIFIED., .F., .F. ) 
 B_SPLINE_CURVE_WITH_KNOTS ( ( 4, 4 ),
 ( 5.498078028609830525, 7.068189169012200068 ),
 .UNSPECIFIED. ) 
 CURVE ( )  GEOMETRIC_REPRESENTATION_ITEM ( )  RATIONAL_B_SPLINE_CURVE ( ( 1.000000000000000000, 0.8048993264383194068, 0.8048993264383194068, 1.000000000000000000 ) ) 
 REPRESENTATION_ITEM ( '' )  );
#69052 = CARTESIAN_POINT ( 'NONE',  ( 14.74831652169999963, 1414.913060387329779, 202.0310540578979897 ) ) ;
#69053 = CARTESIAN_POINT ( 'NONE',  ( 4.998913908720000521, 1484.124591968289906, 219.8555354240990027 ) ) ;
#69054 = DIRECTION ( 'NONE',  ( -5.980589973904019347E-17, 1.000000000000000000, -1.736889445713099699E-16 ) ) ;
#69055 = CARTESIAN_POINT ( 'NONE',  ( 2.493947715939999643, 1442.756953654919926, 150.6345094620980092 ) ) ;
#69056 = CARTESIAN_POINT ( 'NONE',  ( 5.371360332529999226, 1437.823705336689954, 228.7343661627989775 ) ) ;
#69057 = CARTESIAN_POINT ( 'NONE',  ( 16.66231036550701461, 1523.604703353109926, 180.4882076302513099 ) ) ;
#69058 = CARTESIAN_POINT ( 'NONE',  ( -0.3862240865043620186, 1500.063269132039977, 233.1571802061429821 ) ) ;
#69060 = CARTESIAN_POINT ( 'NONE',  ( -14.08836401118779946, 1379.655773939669871, 211.5932977078229840 ) ) ;
#69059 = CARTESIAN_POINT ( 'NONE',  ( -21.74753855979999884, 1409.672501167229939, 211.1389744297880213 ) ) ;
#69061 = CARTESIAN_POINT ( 'NONE',  ( 8.481739720359620094, 1422.818663224589727, 213.7027558147750028 ) ) ;
#69062 = CARTESIAN_POINT ( 'NONE',  ( 9.820661198562449457, 1435.530196802239971, 209.1647375191699894 ) ) ;
#69063 = CARTESIAN_POINT ( 'NONE',  ( -11.28649141220000018, 1489.673453124989919, 212.4368142099590102 ) ) ;
#69064 = CARTESIAN_POINT ( 'NONE',  ( -18.26675480510339966, 1424.840341062940070, 227.6848255537819909 ) ) ;
#69065 = CARTESIAN_POINT ( 'NONE',  ( -19.27355791249999939, 1467.813399981289876, 204.3088842694490097 ) ) ;
#69066 = B_SPLINE_CURVE_WITH_KNOTS ( 'NONE', 5,
 ( #53303, #104237, #11294, #45462, #63908, #29182, #37026, #62263, #54955 ),
 .UNSPECIFIED., .F., .F.,
 ( 6, 3, 6 ),
 ( 0.9063219059076105255, 0.9212159755548054996, 1.000000000000000000 ),
 .UNSPECIFIED. ) ;
#69067 = CARTESIAN_POINT ( 'NONE',  ( -4.618749106614999711, 1516.729202374750002, 202.5720834851169911 ) ) ;
#69068 = CARTESIAN_POINT ( 'NONE',  ( -1.783433545534589104, 1397.966851194222954, 222.0187806250839060 ) ) ;
#69069 = DIRECTION ( 'NONE',  ( -1.836970198721029688E-16, -1.000000000000000000, 0.000000000000000000 ) ) ;
#69070 = CARTESIAN_POINT ( 'NONE',  ( 4.500000000000000000, 1432.413060387330006, 146.1721969590979882 ) ) ;
#69071 = DIRECTION ( 'NONE',  ( -0.8090169943749422332, -0.000000000000000000, 0.5877852522924802425 ) ) ;
#69072 = CARTESIAN_POINT ( 'NONE',  ( 37.61621548944700066, 1449.688575227499996, 136.2442305511190170 ) ) ;
#69074 = EDGE_LOOP ( 'NONE', ( #72702, #74586, #12816, #68628 ) ) ;
#69073 = CARTESIAN_POINT ( 'NONE',  ( -65.37646396962441031, 1379.739460607499950, 275.4797537947760020 ) ) ;
#69075 = EDGE_LOOP ( 'NONE', ( #4962, #25698 ) ) ;
#69076 = CARTESIAN_POINT ( 'NONE',  ( 0.2751658889820000065, 1506.798305107329952, 186.8348836488979998 ) ) ;
#69077 = CARTESIAN_POINT ( 'NONE',  ( 0.08248983565340001212, 1397.911842041330146, 222.1215842506979925 ) ) ;
#69078 = ORIENTED_EDGE ( 'NONE', *, *, #34423, .F. ) ;
#69079 = CARTESIAN_POINT ( 'NONE',  ( -0.0001938387787944162953, 1397.283789131768117, 222.0379186164004466 ) ) ;
#69080 = CARTESIAN_POINT ( 'NONE',  ( 17.04824238339829634, 1423.676546790900147, 228.9394188427949928 ) ) ;
#69081 = CARTESIAN_POINT ( 'NONE',  ( 3.368596972436100234, 1515.551842520359969, 205.3433046317179844 ) ) ;
#69083 = CARTESIAN_POINT ( 'NONE',  ( 8.968501251859999357, 1428.602659895330135, 101.8807690336980016 ) ) ;
#69082 = CARTESIAN_POINT ( 'NONE',  ( 16.01295443681960151, 1422.119564716039804, 191.1690555812749892 ) ) ;
#69084 = CARTESIAN_POINT ( 'NONE',  ( 18.08856701439330195, 1498.113134534269875, 229.9575450159010188 ) ) ;
#69085 = CARTESIAN_POINT ( 'NONE',  ( 2.458572921189999594, 1507.640305379429947, 181.2872115462979821 ) ) ;
#69086 = CARTESIAN_POINT ( 'NONE',  ( 2.770834604750000096, 1467.540123119690179, 218.8375473850189792 ) ) ;
#69087 = CARTESIAN_POINT ( 'NONE',  ( 2.942029629868560203, 1512.314860014990018, 217.0136234555809835 ) ) ;
#69088 = CARTESIAN_POINT ( 'NONE',  ( 3.462620818104999998, 1516.938330505699923, 211.6001527901769919 ) ) ;
#69089 = CARTESIAN_POINT ( 'NONE',  ( 36.51516363007900168, 1436.208852635709945, 134.0999999969979797 ) ) ;
#69090 = CARTESIAN_POINT ( 'NONE',  ( 11.86176063160000105, 1432.032830640380098, 149.9745659136979725 ) ) ;
#69091 = CARTESIAN_POINT ( 'NONE',  ( 7.382751547855000318, 1511.929989569679947, 202.5109750345870054 ) ) ;
#69092 = ORIENTED_EDGE ( 'NONE', *, *, #17874, .F. ) ;
#69093 = CARTESIAN_POINT ( 'NONE',  ( 14.06744947489100106, 1435.197734885789941, 149.3372217745049966 ) ) ;
#69094 = CARTESIAN_POINT ( 'NONE',  ( -0.2691619379491070330, 1432.197445330879873, 200.7020891982060107 ) ) ;
#69095 = VERTEX_POINT ( 'NONE', #15023 ) ;
#69096 = ORIENTED_EDGE ( 'NONE', *, *, #13827, .F. ) ;
#69097 = CARTESIAN_POINT ( 'NONE',  ( 12.64457216002790574, 1445.030948195889323, 169.4649751935023119 ) ) ;
#69098 = CARTESIAN_POINT ( 'NONE',  ( -1.296202833079999950, 1464.946618178429844, 237.1878767853979753 ) ) ;
#69099 = CARTESIAN_POINT ( 'NONE',  ( -5.559835380637566438, 1475.920404062059333, 200.3847495419848030 ) ) ;
#69100 = CARTESIAN_POINT ( 'NONE',  ( 1.708092266164999984, 1516.523379810429788, 216.8305916180169959 ) ) ;
#69101 = CARTESIAN_POINT ( 'NONE',  ( -1.991394312995570015, 1465.005291665100003, 198.2980544129180203 ) ) ;
#69102 = PRODUCT_DEFINITION_FORMATION_WITH_SPECIFIED_SOURCE ( 'ANY', '', #54500, .NOT_KNOWN. ) ;
#69103 = CARTESIAN_POINT ( 'NONE',  ( 11.66548674282380027, 1421.980630269289804, 209.5620691455910105 ) ) ;
#69104 = CARTESIAN_POINT ( 'NONE',  ( -60.03054239385676993, 1379.724805969880208, 261.4558930067639722 ) ) ;
#69105 = CARTESIAN_POINT ( 'NONE',  ( 2.773997830410000365, 1465.987719246390043, 198.8503135595989875 ) ) ;
#69106 = CARTESIAN_POINT ( 'NONE',  ( 0.8957163599030000256, 1507.375187373130075, 237.2105928541979836 ) ) ;
#69107 = EDGE_LOOP ( 'NONE', ( #71073, #30315, #4025, #24637 ) ) ;
#69108 = CARTESIAN_POINT ( 'NONE',  ( -2.493073867885000183, 1516.826109302209943, 206.2575198447970024 ) ) ;
#69109 = ORIENTED_EDGE ( 'NONE', *, *, #64845, .T. ) ;
#69110 = CARTESIAN_POINT ( 'NONE',  ( 19.42500282749999840, 1440.913060387330006, 212.4633492400480179 ) ) ;
#69111 = CARTESIAN_POINT ( 'NONE',  ( -20.17745077670000242, 1509.606869791130066, 230.6312312576980048 ) ) ;
#69112 = ORIENTED_EDGE ( 'NONE', *, *, #102190, .T. ) ;
#69113 = CARTESIAN_POINT ( 'NONE',  ( -9.153149079460000337, 1409.735973916530156, 188.2996874139979866 ) ) ;
#69114 = LINE ( 'NONE', #66904, #23068 ) ;
#69116 = ORIENTED_EDGE ( 'NONE', *, *, #88550, .T. ) ;
#69115 = CARTESIAN_POINT ( 'NONE',  ( -9.380124768717641004, 1428.163396101657781, 137.0999999980979851 ) ) ;
#69117 = CARTESIAN_POINT ( 'NONE',  ( 24.50256053759999730, 1438.051362122639830, 212.5740290884979800 ) ) ;
#69118 = CARTESIAN_POINT ( 'NONE',  ( -18.13023266204549699, 1508.551704408389924, 210.4115160111289811 ) ) ;
#69119 = CARTESIAN_POINT ( 'NONE',  ( -4.038582000520636761, 1515.598601297060668, 208.8111433043314946 ) ) ;
#69120 = CARTESIAN_POINT ( 'NONE',  ( -111.2060435952740676, 1379.913060387289988, 303.0232821107484824 ) ) ;
#69121 = CARTESIAN_POINT ( 'NONE',  ( -2.287084308194999860, 1517.068517094990057, 214.1351209316169957 ) ) ;
#69122 = CARTESIAN_POINT ( 'NONE',  ( -2.710325452122229972, 1429.081471984569816, 200.1517093420179947 ) ) ;
#69123 = CIRCLE ( 'NONE', #4680, 2.000000000000000000 ) ;
#69124 = CARTESIAN_POINT ( 'NONE',  ( -21.92423686380000092, 1509.678671609130106, 190.3411753256980035 ) ) ;
#69125 = CIRCLE ( 'NONE', #11877, 2.000079904907770434 ) ;
#69126 = CARTESIAN_POINT ( 'NONE',  ( -16.90742456150000095, 1442.831169986189934, 162.4348202098979925 ) ) ;
#69127 = CARTESIAN_POINT ( 'NONE',  ( 1.136547584984999970, 1516.839862955080207, 211.5998212856970042 ) ) ;
#69128 = CARTESIAN_POINT ( 'NONE',  ( 15.01814799273499901, 1514.214451716350140, 223.8476172842669882 ) ) ;
#69129 = CARTESIAN_POINT ( 'NONE',  ( 30.38265071698929276, 1524.478200376951008, 221.8419858056983571 ) ) ;
#69131 = VERTEX_POINT ( 'NONE', #34605 ) ;
#69130 = CARTESIAN_POINT ( 'NONE',  ( -102.9162786870000019, 1389.260382295949967, 308.6471719622589944 ) ) ;
#69132 = CARTESIAN_POINT ( 'NONE',  ( 35.93745672850000261, 1447.859703060729998, 254.6053128065979934 ) ) ;
#69133 = CARTESIAN_POINT ( 'NONE',  ( 3.490272952469018364, 1450.862712094549352, 184.0573294561584134 ) ) ;
#69134 = CARTESIAN_POINT ( 'NONE',  ( -28.74419454077009917, 1509.916829779089994, 215.0463914455240229 ) ) ;
#69136 = AXIS2_PLACEMENT_3D ( 'NONE', #20302, #54506, #73490 ) ;
#69135 = CARTESIAN_POINT ( 'NONE',  ( -8.326540575840001068, 1507.918730918930123, 235.2420017123980074 ) ) ;
#69137 = CARTESIAN_POINT ( 'NONE',  ( 7.348570800660000124, 1422.803073198840139, 195.5677875354990078 ) ) ;
#69139 = CARTESIAN_POINT ( 'NONE',  ( 19.09164403609999994, 1456.344937430229947, 226.3477507761979837 ) ) ;
#69138 = CARTESIAN_POINT ( 'NONE',  ( 11.57592109439999994, 1432.301060653729792, 151.1967999008980144 ) ) ;
#69140 = CARTESIAN_POINT ( 'NONE',  ( -10.37115945647730086, 1448.032435977620025, 209.0451274022370001 ) ) ;
#69141 = CARTESIAN_POINT ( 'NONE',  ( -107.2549441997609989, 1382.093684753940124, 310.1063884366330399 ) ) ;
#69142 = ORIENTED_EDGE ( 'NONE', *, *, #29916, .T. ) ;
#69143 = CARTESIAN_POINT ( 'NONE',  ( -7.334328310795000583, 1517.005755693489846, 204.1179978101270081 ) ) ;
#69144 = CARTESIAN_POINT ( 'NONE',  ( 3.780309398849999084E-14, 1406.777728848529932, 269.6500679732980075 ) ) ;
#69145 = CARTESIAN_POINT ( 'NONE',  ( 27.72858359559999997, 1508.599279870730015, 207.6849852067780091 ) ) ;
#69146 = CARTESIAN_POINT ( 'NONE',  ( 24.59137937210000047, 1442.248894770099923, 213.3251317051179967 ) ) ;
#69147 = CARTESIAN_POINT ( 'NONE',  ( 5.386093888109999561, 1432.347042751149957, 154.6076556448980170 ) ) ;
#69148 = CARTESIAN_POINT ( 'NONE',  ( 3.432220944640000049, 1466.863758737489889, 218.8549222279790172 ) ) ;
#69149 = CARTESIAN_POINT ( 'NONE',  ( 0.000000000000000000, 1526.382868172863937, 209.1218459616979999 ) ) ;
#69150 = CARTESIAN_POINT ( 'NONE',  ( 26.80760470685860142, 1436.328554475559940, 136.7304320938700073 ) ) ;
#69151 = CARTESIAN_POINT ( 'NONE',  ( 34.60210436545990120, 1450.378017727679890, 136.2318747066630067 ) ) ;
#69152 = CARTESIAN_POINT ( 'NONE',  ( -34.13334863075944270, 1463.712688128719037, 269.2713322011451851 ) ) ;
#69153 = CARTESIAN_POINT ( 'NONE',  ( -2.123092008920000051, 1429.895782721190017, 200.6928439449890220 ) ) ;
#69154 = EDGE_CURVE ( 'NONE', #9541, #69447, #83901, .T. ) ;
#69155 = CARTESIAN_POINT ( 'NONE',  ( 10.43348778195679927, 1481.587817364219973, 210.8845854110620053 ) ) ;
#69156 = CARTESIAN_POINT ( 'NONE',  ( 3.826065771026290196, 1507.355962757600082, 220.1845845182679966 ) ) ;
#69157 = CARTESIAN_POINT ( 'NONE',  ( -42.06231930236405248, 1442.702167343311658, 269.6487547253948378 ) ) ;
#69158 = EDGE_LOOP ( 'NONE', ( #109000, #34616, #29798, #13710, #92237 ) ) ;
#69159 = CARTESIAN_POINT ( 'NONE',  ( -17.07488731192356823, 1522.051704408389924, 212.8400904445188075 ) ) ;
#69160 = CARTESIAN_POINT ( 'NONE',  ( 13.50151513640000189, 1434.968987195889895, 146.5972134562979932 ) ) ;
#69161 = CARTESIAN_POINT ( 'NONE',  ( -22.08327125186962192, 1523.604703353109699, 184.4267662568474009 ) ) ;
#69162 = DIRECTION ( 'NONE',  ( -1.836970198721029688E-16, -1.000000000000000000, 0.000000000000000000 ) ) ;
#69163 = CARTESIAN_POINT ( 'NONE',  ( 11.44665326297827335, 1425.798162341591706, 139.1345266541928538 ) ) ;
#69165 = CARTESIAN_POINT ( 'NONE',  ( 32.41382812665797530, 1525.581535527371216, 197.9832485531609905 ) ) ;
#69164 = CARTESIAN_POINT ( 'NONE',  ( 11.57530253989999913, 1501.342159807790040, 208.5271154974659851 ) ) ;
#69166 = CARTESIAN_POINT ( 'NONE',  ( 19.26928223589375833, 1455.917628554740986, 225.9370567887913808 ) ) ;
#69167 = CARTESIAN_POINT ( 'NONE',  ( 8.214113159060000058, 1423.929736563989991, 211.6354375824689953 ) ) ;
#69168 = CARTESIAN_POINT ( 'NONE',  ( -14.27824533756169956, 1384.878970200230015, 219.2940513638699827 ) ) ;
#69169 = AXIS2_PLACEMENT_3D ( 'NONE', #81380, #56762, #90900 ) ;
#69170 = DIRECTION ( 'NONE',  ( 0.000000000000000000, 1.000000000000000000, 0.000000000000000000 ) ) ;
#69171 = CARTESIAN_POINT ( 'NONE',  ( -18.45314936670000350, 1415.553739809529816, 207.8952753008079810 ) ) ;
#69172 = CARTESIAN_POINT ( 'NONE',  ( -5.192564606620000411, 1483.459670744789946, 199.8090169432990137 ) ) ;
#69173 = CARTESIAN_POINT ( 'NONE',  ( 25.79054002703109916, 1435.417905869039942, 135.6747449796359888 ) ) ;
#69174 = CARTESIAN_POINT ( 'NONE',  ( -13.51610093808349866, 1443.887577857937458, 169.3501091255429856 ) ) ;
#69175 = ORIENTED_EDGE ( 'NONE', *, *, #69995, .T. ) ;
#69176 = CARTESIAN_POINT ( 'NONE',  ( -16.39775370592910164, 1409.510809139110052, 225.2343662999429910 ) ) ;
#69177 = CARTESIAN_POINT ( 'NONE',  ( 9.771922359260001301, 1440.444625599219989, 148.8200729295979841 ) ) ;
#69178 = EDGE_LOOP ( 'NONE', ( #28471, #79709, #52222, #3240 ) ) ;
#69179 = VERTEX_POINT ( 'NONE', #50864 ) ;
#69180 = CARTESIAN_POINT ( 'NONE',  ( 0.3839115268003259751, 1435.761583004419890, 227.5864344777720021 ) ) ;
#69181 = CARTESIAN_POINT ( 'NONE',  ( -14.89207660494735386, 1416.116151593460017, 205.0818956363123675 ) ) ;
#69183 = CARTESIAN_POINT ( 'NONE',  ( -0.4823735185300109807, 1457.129037944750053, 219.7424419883419944 ) ) ;
#69182 = CARTESIAN_POINT ( 'NONE',  ( 10.03329442769999957, 1425.203965949929852, 96.53732743869790056 ) ) ;
#69184 = DIRECTION ( 'NONE',  ( 0.9846671174924281900, -0.1149361401860498344, -0.1312263365650570279 ) ) ;
#69185 = CARTESIAN_POINT ( 'NONE',  ( 4.350626057107779054, 1425.642856625690001, 185.4477024701949972 ) ) ;
#69186 = EDGE_CURVE ( 'NONE', #8260, #54763, #103540, .T. ) ;
#69187 = CARTESIAN_POINT ( 'NONE',  ( -2.901771220848202937, 1419.574541655020312, 186.1989676290672264 ) ) ;
#69188 = CARTESIAN_POINT ( 'NONE',  ( 7.894362808210001248, 1424.028044848189893, 212.1595859666189767 ) ) ;
#69189 = CARTESIAN_POINT ( 'NONE',  ( -8.627754863869999014, 1437.492696374190018, 228.3379673428989918 ) ) ;
#69190 = CARTESIAN_POINT ( 'NONE',  ( 7.925631312170001053, 1509.190094470230179, 180.8627748357979783 ) ) ;
#69191 = CARTESIAN_POINT ( 'NONE',  ( 2.531379128109999765, 1449.143641694869984, 182.8453065789979917 ) ) ;
#69192 = CARTESIAN_POINT ( 'NONE',  ( 8.972728618379855803, 1365.192543519359333, 207.6218459616988241 ) ) ;
#69194 = ORIENTED_EDGE ( 'NONE', *, *, #46086, .F. ) ;
#69193 = DIRECTION ( 'NONE',  ( -1.755985294532469921E-16, 1.000000000000000000, -1.338183447452831989E-16 ) ) ;
#69195 = ORIENTED_EDGE ( 'NONE', *, *, #83, .T. ) ;
#69196 = CARTESIAN_POINT ( 'NONE',  ( -41.66194525459999909, 1443.744937001919880, 136.1277553619979699 ) ) ;
#69197 = CARTESIAN_POINT ( 'NONE',  ( 7.477233242777599820, 1510.784366252118843, 202.9987894833095652 ) ) ;
#69198 = CARTESIAN_POINT ( 'NONE',  ( -3.056877442999999861, 1471.506820614530170, 269.6159236013979807 ) ) ;
#69199 = CARTESIAN_POINT ( 'NONE',  ( 12.74692502376422176, 1434.633369486244646, 147.1384066575065219 ) ) ;
#69200 = CARTESIAN_POINT ( 'NONE',  ( 0.1420983796599999682, 1486.103412518930099, 181.9585633641979996 ) ) ;
#69201 = CARTESIAN_POINT ( 'NONE',  ( 21.00523825079999796, 1507.839072599329711, 190.5229776796980161 ) ) ;
#69202 = CARTESIAN_POINT ( 'NONE',  ( -9.116411868360000170, 1384.545094513749746, 199.9660485183590026 ) ) ;
#69203 = CARTESIAN_POINT ( 'NONE',  ( -36.39519410782710196, 1451.404435322049949, 135.1209920990980038 ) ) ;
#69204 = CARTESIAN_POINT ( 'NONE',  ( -11.60004869885203682, -0.000000000000000000, 137.0999999980979851 ) ) ;
#69205 = CARTESIAN_POINT ( 'NONE',  ( 38.62863167664609421, 1444.143249097809985, 137.1666610355499927 ) ) ;
#69206 = CARTESIAN_POINT ( 'NONE',  ( 9.979564351426096991, 1368.671368999377137, 209.6218459617033432 ) ) ;
#69207 = CARTESIAN_POINT ( 'NONE',  ( 8.993528449059150276, 1407.583683456149856, 198.9375600053470237 ) ) ;
#69208 = CARTESIAN_POINT ( 'NONE',  ( -20.64901375512450343, 1409.367826505309949, 267.6706922366469712 ) ) ;
#69209 = CARTESIAN_POINT ( 'NONE',  ( -13.86043986179080001, 1435.008531462659903, 148.8737775447249874 ) ) ;
#69210 = ORIENTED_EDGE ( 'NONE', *, *, #70737, .F. ) ;
#69211 = CARTESIAN_POINT ( 'NONE',  ( -11.30175580989999951, 1432.339690393880119, 151.5220148440980097 ) ) ;
#69212 = CARTESIAN_POINT ( 'NONE',  ( 13.28241350259999898, 1445.641312562420126, 188.6965274455980079 ) ) ;
#69213 = ORIENTED_EDGE ( 'NONE', *, *, #47656, .T. ) ;
#69214 = ORIENTED_EDGE ( 'NONE', *, *, #94562, .F. ) ;
#69215 = PLANE ( 'NONE',  #62706 ) ;
#69216 = CARTESIAN_POINT ( 'NONE',  ( -3.787329988085039734, 1369.092969256092601, 207.6218459616989946 ) ) ;
#69217 = CIRCLE ( 'NONE', #29866, 17.26401014167801762 ) ;
#69218 = CARTESIAN_POINT ( 'NONE',  ( 0.01322035751810150123, 1516.939819969850078, 213.1588969678170145 ) ) ;
#69219 = CARTESIAN_POINT ( 'NONE',  ( -16.02210698220000040, 1470.468178375529988, 188.3958660763979935 ) ) ;
#69220 = ORIENTED_EDGE ( 'NONE', *, *, #94766, .F. ) ;
#69221 = DIRECTION ( 'NONE',  ( 0.4978433412588729179, 0.000000000000000000, 0.8672669759446635096 ) ) ;
#69222 = EDGE_CURVE ( 'NONE', #103324, #36366, #16646, .T. ) ;
#69223 = EDGE_CURVE ( 'NONE', #91400, #29545, #96819, .T. ) ;
#69224 = EDGE_CURVE ( 'NONE', #82445, #92620, #7746, .T. ) ;
#69225 = CARTESIAN_POINT ( 'NONE',  ( 9.626138668350000316, 1415.087974640030097, 223.7831235720980203 ) ) ;
#69226 = CARTESIAN_POINT ( 'NONE',  ( 4.032397901875000024, 1516.981965530290154, 203.3362630185569913 ) ) ;
#69227 = CARTESIAN_POINT ( 'NONE',  ( -29.35556035689999987, 1509.949879406430000, 205.5028565010079831 ) ) ;
#69228 = EDGE_CURVE ( 'NONE', #7587, #86208, #34136, .T. ) ;
#69229 = CARTESIAN_POINT ( 'NONE',  ( 1.436979206307143375, 1507.073228327747302, 236.7831034515724014 ) ) ;
#69230 = CIRCLE ( 'NONE', #83502, 1.000000000000000888 ) ;
#69232 = ADVANCED_FACE ( 'NONE', ( #21499 ), #78833, .F. ) ;
#69231 = CARTESIAN_POINT ( 'NONE',  ( -79.49322724790000905, 1384.792572819600082, 282.9493281527590511 ) ) ;
#69233 = CARTESIAN_POINT ( 'NONE',  ( -58.69053996021689557, 1384.665059837310082, 241.2311621880149914 ) ) ;
#69234 = CARTESIAN_POINT ( 'NONE',  ( -1.286178515069999806, 1407.887987576529895, 195.9343300142979842 ) ) ;
#69235 = CARTESIAN_POINT ( 'NONE',  ( -12.38733338750000179, 1409.511671407230097, 227.5189851686980091 ) ) ;
#69237 = ORIENTED_EDGE ( 'NONE', *, *, #6835, .T. ) ;
#69236 = CARTESIAN_POINT ( 'NONE',  ( -4.164625339459999687, 1446.237990885560066, 183.4551341185980107 ) ) ;
#69238 = CARTESIAN_POINT ( 'NONE',  ( 19.33081166079999846, 1455.566665276290223, 210.0606673158609965 ) ) ;
#69239 = CARTESIAN_POINT ( 'NONE',  ( 27.53546928359999768, 1508.129852616029893, 212.9718660772680039 ) ) ;
#69240 = EDGE_CURVE ( 'NONE', #72815, #3729, #67480, .T. ) ;
#69241 = DIRECTION ( 'NONE',  ( 0.000000000000000000, 1.000000000000000000, 0.000000000000000000 ) ) ;
#69242 = CARTESIAN_POINT ( 'NONE',  ( -24.72639760740000270, 1435.360974979420007, 136.0074239971980035 ) ) ;
#69243 = CARTESIAN_POINT ( 'NONE',  ( 0.01327253640020150012, 1516.940252185109784, 211.9957649727570015 ) ) ;
#69244 = CARTESIAN_POINT ( 'NONE',  ( -68.36039621120001186, 1379.746991223579926, 279.2258544646589939 ) ) ;
#69245 = CIRCLE ( 'NONE', #15562, 1.000000000000000888 ) ;
#69246 = CARTESIAN_POINT ( 'NONE',  ( -6.068033889650000567, 1450.398953434090117, 208.9968551374399794 ) ) ;
#69247 = CARTESIAN_POINT ( 'NONE',  ( -29.91208173166754847, 1525.042337199239910, 222.1821013135304668 ) ) ;
#69248 = CARTESIAN_POINT ( 'NONE',  ( 6.556850996575000146, 1516.939568781210028, 209.1101343261499892 ) ) ;
#69249 = EDGE_LOOP ( 'NONE', ( #104377, #96633, #155, #106143 ) ) ;
#69250 = LINE ( 'NONE', #9870, #90229 ) ;
#69252 = EDGE_CURVE ( 'NONE', #25299, #49915, #31350, .T. ) ;
#69251 = CARTESIAN_POINT ( 'NONE',  ( 5.401672926506360106, 1440.924418278400026, 154.8182599678980012 ) ) ;
#69253 = CARTESIAN_POINT ( 'NONE',  ( -32.10879564089999860, 1385.224147136040074, 229.9470470709589733 ) ) ;
#69254 = ORIENTED_EDGE ( 'NONE', *, *, #93787, .T. ) ;
#69255 = CARTESIAN_POINT ( 'NONE',  ( -105.1514435807109180, 1379.134842035547763, 304.0347158685106024 ) ) ;
#69256 = LINE ( 'NONE', #103363, #92405 ) ;
#69257 = CARTESIAN_POINT ( 'NONE',  ( 12.23184522910000105, 1434.618918689169959, 150.6553485564980122 ) ) ;
#69258 = CARTESIAN_POINT ( 'NONE',  ( 16.24562813123679561, 1478.707530004980072, 230.1287771015380201 ) ) ;
#69259 = ADVANCED_FACE ( 'NONE', ( #79383 ), #64109, .F. ) ;
#69260 = DIRECTION ( 'NONE',  ( -0.6768489701308448847, 0.6839977328998089190, 0.2720708970484284062 ) ) ;
#69261 = CARTESIAN_POINT ( 'NONE',  ( -1.408971986799999909, 1408.962262773329940, 187.0389398893979944 ) ) ;
#69262 = EDGE_CURVE ( 'NONE', #82048, #52413, #51389, .T. ) ;
#69263 = CARTESIAN_POINT ( 'NONE',  ( 0.4354997668961430035, 1517.051704408389924, 201.4383102929800202 ) ) ;
#69264 = LINE ( 'NONE', #103370, #107711 ) ;
#69266 = CARTESIAN_POINT ( 'NONE',  ( 11.55221588404359956, 1480.217597516799970, 211.4789165460060190 ) ) ;
#69265 = CARTESIAN_POINT ( 'NONE',  ( -4.030514550714999977, 1516.901952101700090, 213.7446888144170032 ) ) ;
#69267 = CARTESIAN_POINT ( 'NONE',  ( 19.63615699109999824, 1508.568590227029972, 188.6353561189980041 ) ) ;
#69268 = CARTESIAN_POINT ( 'NONE',  ( 6.942344691835000248, 1516.810037859429940, 216.8380980232070101 ) ) ;
#69269 = TOROIDAL_SURFACE ( 'NONE', #12020, 12.73448142120000171, 1.000000000000000000 ) ;
#69270 = ORIENTED_EDGE ( 'NONE', *, *, #36956, .T. ) ;
#69271 = CARTESIAN_POINT ( 'NONE',  ( 3.454172615424999648, 1517.122088787240045, 201.3974225380069925 ) ) ;
#69272 = CARTESIAN_POINT ( 'NONE',  ( -20.34835314180000054, 1499.713795797229977, 189.8114522981980201 ) ) ;
#69273 = VERTEX_POINT ( 'NONE', #27311 ) ;
#69274 = ADVANCED_FACE ( 'NONE', ( #95622 ), #77676, .T. ) ;
#69275 = CARTESIAN_POINT ( 'NONE',  ( 3.521117552959999841, 1421.670602369330027, 184.1604385248979838 ) ) ;
#69276 = SURFACE_STYLE_FILL_AREA ( #110149 ) ;
#69277 = CARTESIAN_POINT ( 'NONE',  ( 2.999854733669999884, 1441.831681250090014, 217.8331532265690100 ) ) ;
#69278 = CARTESIAN_POINT ( 'NONE',  ( -33.28034951413770415, 1522.644714754858114, 200.8029765415151928 ) ) ;
#69279 = CARTESIAN_POINT ( 'NONE',  ( -3.819157230050550598E-10, 1415.320034473050100, 235.4381035424730158 ) ) ;
#69280 = B_SPLINE_CURVE_WITH_KNOTS ( 'NONE', 5,
 ( #13722, #47907, #82615, #48477, #82043, #56867 ),
 .UNSPECIFIED., .F., .F.,
 ( 6, 6 ),
 ( -1.468559632160000072, -1.438859269287107168E-06 ),
 .UNSPECIFIED. ) ;
#69281 = CARTESIAN_POINT ( 'NONE',  ( -4.283010808509999379, 1446.850643219170024, 156.0812219214980132 ) ) ;
#69282 = CARTESIAN_POINT ( 'NONE',  ( 15.87566767260028833, 1507.597642236632055, 231.8003891413981421 ) ) ;
#69283 = CARTESIAN_POINT ( 'NONE',  ( 8.820344574085469347, 1461.063527266820074, 204.9905474934919880 ) ) ;
#69284 = DIRECTION ( 'NONE',  ( 0.7074300731457748848, -0.02470400237811459093, 0.7063514733300028103 ) ) ;
#69285 = CARTESIAN_POINT ( 'NONE',  ( 17.01771828639999740, 1416.204137079330167, 191.6576494061979758 ) ) ;
#69287 = CARTESIAN_POINT ( 'NONE',  ( 0.5987183461865049905, 1507.212886145319999, 186.4932301926239688 ) ) ;
#69286 = CARTESIAN_POINT ( 'NONE',  ( -9.141596155196140217, 1420.494364209170044, 195.3822545821539904 ) ) ;
#69288 = CARTESIAN_POINT ( 'NONE',  ( 10.96946812545280103, 1432.347663862999980, 151.7701354189910035 ) ) ;
#69289 = ORIENTED_EDGE ( 'NONE', *, *, #96325, .T. ) ;
#69290 = CARTESIAN_POINT ( 'NONE',  ( 1.553484637916519917, 1415.542389211330146, 190.7873441232580092 ) ) ;
#69291 = B_SPLINE_CURVE_WITH_KNOTS ( 'NONE', 3,
 ( #75092, #100276, #23556, #109780 ),
 .UNSPECIFIED., .F., .F.,
 ( 4, 4 ),
 ( 0.000000000000000000, 0.0002220129587134779374 ),
 .UNSPECIFIED. ) ;
#69292 = CARTESIAN_POINT ( 'NONE',  ( 26.86204974310000182, 1508.007394749430205, 206.2315949334080187 ) ) ;
#69293 = AXIS2_PLACEMENT_3D ( 'NONE', #77121, #96109, #427 ) ;
#69294 = CARTESIAN_POINT ( 'NONE',  ( -1.435939366445312615, 1526.382868172863937, 178.7444848717731531 ) ) ;
#69295 = CARTESIAN_POINT ( 'NONE',  ( 9.651066088509999474, 1425.440658930580184, 195.4941615409990163 ) ) ;
#69296 = CARTESIAN_POINT ( 'NONE',  ( -10.51265743563710053, 1480.030739721740019, 208.9489006321179829 ) ) ;
#69297 = CARTESIAN_POINT ( 'NONE',  ( -3.549608351769999892, 1507.276797637930031, 180.9704965309979912 ) ) ;
#69298 = CARTESIAN_POINT ( 'NONE',  ( 3.968827104744170331, 1521.951704408389787, 188.7040005449509863 ) ) ;
#69299 = EDGE_CURVE ( 'NONE', #43306, #52400, #33028, .T. ) ;
#69300 = CARTESIAN_POINT ( 'NONE',  ( -3.895893481806210090, 1487.443163804099868, 219.7113992567399805 ) ) ;
#69301 = CARTESIAN_POINT ( 'NONE',  ( 18.28863238269999769, 1430.119121229389975, 201.0315571599689974 ) ) ;
#69302 = CARTESIAN_POINT ( 'NONE',  ( -55.50846133737319832, 1383.803145790959888, 272.4221409317659663 ) ) ;
#69303 = CARTESIAN_POINT ( 'NONE',  ( 19.97872766260000077, 1452.215387843930102, 143.5714034319979930 ) ) ;
#69304 = EDGE_CURVE ( 'NONE', #22078, #13046, #59543, .T. ) ;
#69305 = CARTESIAN_POINT ( 'NONE',  ( -15.37090796494357825, 1506.446781329460464, 224.8527620067033297 ) ) ;
#69306 = CARTESIAN_POINT ( 'NONE',  ( -1.902812991693870082, 1516.533218713809902, 201.4128426435650283 ) ) ;
#69308 = VERTEX_POINT ( 'NONE', #58258 ) ;
#69307 = CARTESIAN_POINT ( 'NONE',  ( 24.27343742149999883, 1509.087597399430024, 195.8036337447979918 ) ) ;
#69309 = CARTESIAN_POINT ( 'NONE',  ( -18.38172408721423068, 1459.016642225524038, 227.7444303527029774 ) ) ;
#69310 = CARTESIAN_POINT ( 'NONE',  ( -84.13119167140000343, 1384.814165098149942, 288.0554183306589948 ) ) ;
#69311 = CARTESIAN_POINT ( 'NONE',  ( 30.31643683089993857, 1523.530935881284904, 222.4932308532203820 ) ) ;
#69312 = VERTEX_POINT ( 'NONE', #65005 ) ;
#69313 = ORIENTED_EDGE ( 'NONE', *, *, #92146, .F. ) ;
#69314 = CARTESIAN_POINT ( 'NONE',  ( 13.63158477449999850, 1446.168541001489984, 189.0290012264979964 ) ) ;
#69315 = CARTESIAN_POINT ( 'NONE',  ( 30.30078187369536380, 1526.189899547014420, 201.5450365910303390 ) ) ;
#69316 = CARTESIAN_POINT ( 'NONE',  ( -31.81407709660785699, 1522.382868172863937, 196.2902540610632229 ) ) ;
#69318 = CARTESIAN_POINT ( 'NONE',  ( -33.67852042730000761, 1460.266105628030118, 261.9077679340980467 ) ) ;
#69317 = CARTESIAN_POINT ( 'NONE',  ( 19.03312855989999974, 1434.814457747880169, 209.2860607477259975 ) ) ;
#69319 = DIRECTION ( 'NONE',  ( -0.5877852522924802425, 0.000000000000000000, -0.8090169943749422332 ) ) ;
#69320 = AXIS2_PLACEMENT_3D ( 'NONE', #28348, #54681, #3727 ) ;
#69321 = CARTESIAN_POINT ( 'NONE',  ( -107.8318265130000100, 1381.795387502540052, 298.2715083548590087 ) ) ;
#69322 = ADVANCED_FACE ( 'NONE', ( #110294 ), #73954, .F. ) ;
#69323 = CARTESIAN_POINT ( 'NONE',  ( -12.45548913970438853, 1435.744143842510539, 150.9793205285649265 ) ) ;
#69324 = CARTESIAN_POINT ( 'NONE',  ( -18.49631469930000094, 1416.851343894929869, 208.7101585479910000 ) ) ;
#69325 = CARTESIAN_POINT ( 'NONE',  ( 4.237847613999999652, 1409.564918727129907, 186.3248662794979964 ) ) ;
#69326 = CARTESIAN_POINT ( 'NONE',  ( 4.363111636370000213, 1423.854804604630090, 183.5697630181979889 ) ) ;
#69327 = CARTESIAN_POINT ( 'NONE',  ( -9.836119169070000723, 1438.961854973259960, 152.9388125716980085 ) ) ;
#69328 = CARTESIAN_POINT ( 'NONE',  ( 10.37614134790000087, 1435.190621590189949, 152.2457780280979875 ) ) ;
#69329 = DIRECTION ( 'NONE',  ( -0.6736849260863839728, 0.000000000000000000, 0.7390186874254150995 ) ) ;
#69330 = AXIS2_PLACEMENT_3D ( 'NONE', #88348, #69921, #18908 ) ;
#69331 = CARTESIAN_POINT ( 'NONE',  ( -9.270813479730000140, 1452.444632404429967, 152.0931890696979849 ) ) ;
#69332 = DIRECTION ( 'NONE',  ( -0.9158452764874773777, 0.3011522798863591199, -0.2655837605254210976 ) ) ;
#69333 = ORIENTED_EDGE ( 'NONE', *, *, #65330, .F. ) ;
#69334 = CARTESIAN_POINT ( 'NONE',  ( -3.747824384279149879, 1508.879013859839915, 213.3683195021539802 ) ) ;
#69335 = CARTESIAN_POINT ( 'NONE',  ( -13.43693033329999764, 1470.316141799590014, 192.0299142216990163 ) ) ;
#69336 = CARTESIAN_POINT ( 'NONE',  ( -44.70563246039999683, 1440.913062630770128, 269.9105894055979888 ) ) ;
#69337 = DIRECTION ( 'NONE',  ( 0.9483721503360844629, -0.1343667288060120535, 0.2872905265700261279 ) ) ;
#69338 = CARTESIAN_POINT ( 'NONE',  ( 17.41030305009999779, 1410.018619230629838, 223.8936866133980175 ) ) ;
#69339 = EDGE_CURVE ( 'NONE', #69349, #39470, #107509, .T. ) ;
#69340 = PLANE ( 'NONE',  #71591 ) ;
#69341 = CARTESIAN_POINT ( 'NONE',  ( 2.897498764350990186, 1409.458680991969914, 231.2323409181370266 ) ) ;
#69342 = CARTESIAN_POINT ( 'NONE',  ( -2.131219751997940115, 1421.405227258459945, 193.6669010562050062 ) ) ;
#69343 = CARTESIAN_POINT ( 'NONE',  ( -7.560007814519999592, 1417.633148021330044, 231.2533292727980268 ) ) ;
#69344 = CARTESIAN_POINT ( 'NONE',  ( -8.555194285240508734, 1511.487508625139981, 214.6892046000639880 ) ) ;
#69345 = CARTESIAN_POINT ( 'NONE',  ( -5.986709854369999917, 1361.264879806939916, 207.6218459616989946 ) ) ;
#69346 = CARTESIAN_POINT ( 'NONE',  ( -46.16525872307749978, 1438.439294611029709, 267.5933863983919991 ) ) ;
#69347 = CARTESIAN_POINT ( 'NONE',  ( 17.17241001986506177, 1523.382868172864164, 238.6251415217915053 ) ) ;
#69348 = EDGE_CURVE ( 'NONE', #93667, #107006, #62131, .T. ) ;
#69349 = VERTEX_POINT ( 'NONE', #702 ) ;
#69350 = CARTESIAN_POINT ( 'NONE',  ( -8.205225261000000714, 1424.128567649279830, 209.5451383975179738 ) ) ;
#69351 = EDGE_LOOP ( 'NONE', ( #24123, #51562, #52710, #9180 ) ) ;
#69352 = CARTESIAN_POINT ( 'NONE',  ( 5.786847739675000213, 1517.104497701820037, 209.8595134730280165 ) ) ;
#69353 = CARTESIAN_POINT ( 'NONE',  ( -1.984413551915469975, 1517.051704408389924, 219.3307686695569885 ) ) ;
#69354 = TOROIDAL_SURFACE ( 'NONE', #1397, 8.000000000000000000, 2.000000000000000000 ) ;
#69355 = DIRECTION ( 'NONE',  ( 0.3363363966051478027, 0.9417419117351976121, -2.812289527534883684E-09 ) ) ;
#69356 = CARTESIAN_POINT ( 'NONE',  ( 7.527384429723530168, 1425.477955340190192, 212.1953674759300270 ) ) ;
#69357 = CARTESIAN_POINT ( 'NONE',  ( -25.74067306890999873, 1452.014159533350039, 135.1052487677340253 ) ) ;
#69358 = ORIENTED_EDGE ( 'NONE', *, *, #72068, .F. ) ;
#69359 = CARTESIAN_POINT ( 'NONE',  ( -17.33016184879966204, 1410.462515310626713, 225.7401866622987541 ) ) ;
#69361 = CARTESIAN_POINT ( 'NONE',  ( -15.30573755027229943, 1512.900351074050150, 222.8919101910120162 ) ) ;
#69360 = CARTESIAN_POINT ( 'NONE',  ( -2.389876875773859322, 1525.253972588464876, 176.1934926369094399 ) ) ;
#69362 = ADVANCED_FACE ( 'NONE', ( #52213 ), #102567, .F. ) ;
#69363 =( BOUNDED_CURVE ( )  B_SPLINE_CURVE ( 3, ( #86788, #72619, #68918, #18452 ),
 .UNSPECIFIED., .F., .F. ) 
 B_SPLINE_CURVE_WITH_KNOTS ( ( 4, 4 ),
 ( 3.284991966284695142, 3.571871965064760346 ),
 .UNSPECIFIED. ) 
 CURVE ( )  GEOMETRIC_REPRESENTATION_ITEM ( )  RATIONAL_B_SPLINE_CURVE ( ( 1.000000000000000000, 0.9931534066853130449, 0.9931534066853130449, 1.000000000000000000 ) ) 
 REPRESENTATION_ITEM ( '' )  );
#69364 = CARTESIAN_POINT ( 'NONE',  ( -10.96966273854589957, 1432.359729197300112, 151.7701366752919796 ) ) ;
#69365 = CARTESIAN_POINT ( 'NONE',  ( -18.89253822837050123, 1508.457456783149837, 210.4078925326670060 ) ) ;
#69366 = EDGE_CURVE ( 'NONE', #66058, #102270, #7429, .T. ) ;
#69367 = CARTESIAN_POINT ( 'NONE',  ( 16.66936639845652834, 1523.382868172864164, 237.7608804993219280 ) ) ;
#69368 = CARTESIAN_POINT ( 'NONE',  ( 20.92767404034497147, 1512.187213306747481, 182.8548762971663848 ) ) ;
#69369 = ORIENTED_EDGE ( 'NONE', *, *, #75380, .T. ) ;
#69370 = CARTESIAN_POINT ( 'NONE',  ( -4.172734005785669886, 1410.537251115530125, 269.3368119707569690 ) ) ;
#69371 = CARTESIAN_POINT ( 'NONE',  ( 4.028611221114998919, 1516.744381837270112, 207.9874879615069858 ) ) ;
#69372 = CARTESIAN_POINT ( 'NONE',  ( 7.957816838496420964, 1418.901444373749882, 232.5320780446629954 ) ) ;
#69373 = CARTESIAN_POINT ( 'NONE',  ( -0.4599830242969941141, 1508.922867521862145, 238.6015126468603569 ) ) ;
#69375 = EDGE_LOOP ( 'NONE', ( #47065, #7810, #33433, #104456 ) ) ;
#69374 = CARTESIAN_POINT ( 'NONE',  ( -9.351945459745801159, 1366.519103298168147, 210.6218459616987957 ) ) ;
#69376 = EDGE_LOOP ( 'NONE', ( #77770, #44058, #36680, #55710, #51853, #3809, #79908, #109618 ) ) ;
#69377 = CARTESIAN_POINT ( 'NONE',  ( -23.06575186558750090, 1409.834430086540124, 209.8350140253269842 ) ) ;
#69378 = ADVANCED_FACE ( 'NONE', ( #33173 ), #88468, .F. ) ;
#69379 = CARTESIAN_POINT ( 'NONE',  ( -1.137698304267330096, 1410.327606596320265, 185.3853181447140059 ) ) ;
#69380 = CARTESIAN_POINT ( 'NONE',  ( 3.727927280429065515, 1425.399814015164338, 185.1578063585167513 ) ) ;
#69381 = CIRCLE ( 'NONE', #24629, 0.9999999999999995559 ) ;
#69382 = CARTESIAN_POINT ( 'NONE',  ( -8.363327067911551893, 1406.549745658205438, 266.9340124281022213 ) ) ;
#69383 = EDGE_CURVE ( 'NONE', #54175, #18252, #74976, .T. ) ;
#69384 = CARTESIAN_POINT ( 'NONE',  ( -18.75340623979260002, 1434.970300145230112, 194.4886870813739961 ) ) ;
#69385 = CARTESIAN_POINT ( 'NONE',  ( -21.83928577469999865, 1430.785017815930132, 218.7203724610579911 ) ) ;
#69386 = CARTESIAN_POINT ( 'NONE',  ( 22.48834728391410209, 1471.669847397150079, 266.7671210210439767 ) ) ;
#69387 = CARTESIAN_POINT ( 'NONE',  ( -6.430339621037643560, 1466.008313631039528, 233.9307461128825878 ) ) ;
#69388 = CARTESIAN_POINT ( 'NONE',  ( -3.670436692600000050, 1428.951561624590113, 201.2856071730990095 ) ) ;
#69389 = CARTESIAN_POINT ( 'NONE',  ( -1.135185082175000026, 1516.778853242349896, 205.6747174714770097 ) ) ;
#69390 = VERTEX_POINT ( 'NONE', #53888 ) ;
#69391 = CARTESIAN_POINT ( 'NONE',  ( 21.70910712195382430, 1411.031551472956380, 216.7158344536642574 ) ) ;
#69392 = CARTESIAN_POINT ( 'NONE',  ( -4.181771660003004598, 1516.718258641743432, 202.8911374329507282 ) ) ;
#69393 = CARTESIAN_POINT ( 'NONE',  ( 23.57286938940000098, 1410.708643128529957, 207.8716802985080108 ) ) ;
#69394 = EDGE_LOOP ( 'NONE', ( #57127, #65320, #53251, #104878 ) ) ;
#69395 = CARTESIAN_POINT ( 'NONE',  ( 4.487249753905000027, 1509.038615934169911, 212.6094383991670043 ) ) ;
#69396 = CARTESIAN_POINT ( 'NONE',  ( 26.31673506719999978, 1451.748965920229921, 135.8560917224979789 ) ) ;
#69397 = CARTESIAN_POINT ( 'NONE',  ( -8.456465142934460388, 1522.051704408389924, 195.1434824822571841 ) ) ;
#69398 = CARTESIAN_POINT ( 'NONE',  ( -13.98236733160000078, 1389.833769007690080, 215.1277130629090095 ) ) ;
#69399 = CARTESIAN_POINT ( 'NONE',  ( 7.065869263262089639, 1517.051704406860154, 213.1971559965600136 ) ) ;
#69400 = CARTESIAN_POINT ( 'NONE',  ( 18.31811527990000243, 1410.915650460429788, 194.0164629065979796 ) ) ;
#69401 = CARTESIAN_POINT ( 'NONE',  ( -4.164270815259999203, 1497.128533180889917, 198.6585142336989804 ) ) ;
#69402 = CARTESIAN_POINT ( 'NONE',  ( 2.789113515896739948, 1439.662583475943393, 183.8117166454382811 ) ) ;
#69404 = CARTESIAN_POINT ( 'NONE',  ( -18.67702562490066498, 1424.502089277812502, 224.7510542254474331 ) ) ;
#69403 = CARTESIAN_POINT ( 'NONE',  ( -1.073559340110749938, 1444.993510080170154, 218.0402162255370229 ) ) ;
#69405 = TOROIDAL_SURFACE ( 'NONE', #21073, 2.000000000000000000, 1.000000000000000000 ) ;
#69406 = DIRECTION ( 'NONE',  ( -1.000000000000000000, 0.000000000000000000, 0.000000000000000000 ) ) ;
#69407 = CARTESIAN_POINT ( 'NONE',  ( -0.2751659207381170202, 1506.798305148240161, 231.4088083080649767 ) ) ;
#69408 = CARTESIAN_POINT ( 'NONE',  ( 28.59841869927651103, 1509.911739174257491, 206.6816370879510316 ) ) ;
#69409 = AXIS2_PLACEMENT_3D ( 'NONE', #88025, #98037, #2378 ) ;
#69410 = EDGE_CURVE ( 'NONE', #36343, #72135, #19460, .T. ) ;
#69411 = CARTESIAN_POINT ( 'NONE',  ( 4.087631528831106920, 1417.919639086681173, 234.1544686792272785 ) ) ;
#69412 = EDGE_LOOP ( 'NONE', ( #105079, #80582, #42745, #13875, #65088, #33262, #57108, #88744 ) ) ;
#69413 = CARTESIAN_POINT ( 'NONE',  ( 12.86029672966080106, 1416.218865267220053, 221.6945511805459716 ) ) ;
#69414 = DIRECTION ( 'NONE',  ( -5.980589973904019347E-17, 1.000000000000000000, -1.736889445713099699E-16 ) ) ;
#69415 = VECTOR ( 'NONE', #77405, 1000.000000000000000 ) ;
#69416 = CARTESIAN_POINT ( 'NONE',  ( -8.668122330615428695, 1484.012669316429992, 200.9602178716519916 ) ) ;
#69417 = CIRCLE ( 'NONE', #106937, 1.500287545630077490 ) ;
#69418 = CARTESIAN_POINT ( 'NONE',  ( -20.05314457115955307, 1508.136158586383772, 209.6329359176547484 ) ) ;
#69419 = CARTESIAN_POINT ( 'NONE',  ( 2.799112436247476854, 1421.785673600051723, 193.9260731165295226 ) ) ;
#69420 = CARTESIAN_POINT ( 'NONE',  ( -10.73398234689440045, 1462.915869440839970, 206.4721582478690038 ) ) ;
#69421 = CARTESIAN_POINT ( 'NONE',  ( -21.37693747720000204, 1440.913060387330006, 224.8635562088979896 ) ) ;
#69422 = CARTESIAN_POINT ( 'NONE',  ( 10.62380629660010101, 1475.245810864669011, 266.9323113450542451 ) ) ;
#69423 = CARTESIAN_POINT ( 'NONE',  ( 11.69923102470000131, 1433.280222705429878, 150.9071057001980023 ) ) ;
#69424 = CARTESIAN_POINT ( 'NONE',  ( 19.62446893450000118, 1440.913060387330006, 214.3676144200779845 ) ) ;
#69425 = CARTESIAN_POINT ( 'NONE',  ( -9.642181709647690724, 1460.678695209409852, 208.4214907479299939 ) ) ;
#69426 = CARTESIAN_POINT ( 'NONE',  ( -9.198431329101820708, 1421.868764589120246, 192.2153590489439807 ) ) ;
#69427 = CARTESIAN_POINT ( 'NONE',  ( 10.00923256885409884, 1425.484835869890048, 195.7305245570549914 ) ) ;
#69428 = CARTESIAN_POINT ( 'NONE',  ( 10.36623042182900178, 1462.084445524129933, 211.0499476876460108 ) ) ;
#69429 = CARTESIAN_POINT ( 'NONE',  ( -5.797154954569999852, 1485.993502122029895, 182.5750687759980337 ) ) ;
#69430 = CARTESIAN_POINT ( 'NONE',  ( 11.17483157899774859, 1398.244322891364391, 215.7730490302998874 ) ) ;
#69431 = CARTESIAN_POINT ( 'NONE',  ( -109.1320112420000044, 1384.953741877089897, 311.2644403302589353 ) ) ;
#69432 = CIRCLE ( 'NONE', #1478, 95.87906057922711511 ) ;
#69433 = CARTESIAN_POINT ( 'NONE',  ( 24.57539793370000325, 1430.358747812230149, 211.0346440933479926 ) ) ;
#69434 = CARTESIAN_POINT ( 'NONE',  ( 4.222531898828509433, 1446.229786520979815, 170.5365406785500113 ) ) ;
#69435 = CARTESIAN_POINT ( 'NONE',  ( 25.73763176173297396, 1436.650863761621849, 137.0965057394066378 ) ) ;
#69436 = CARTESIAN_POINT ( 'NONE',  ( -13.49764385317659965, 1383.859966380460037, 218.9859143532220003 ) ) ;
#69437 = CARTESIAN_POINT ( 'NONE',  ( -13.32684193225579961, 1469.522593795099965, 191.9925906374970168 ) ) ;
#69438 = CARTESIAN_POINT ( 'NONE',  ( 6.559798056295000457, 1516.987478262539980, 213.7368632980669929 ) ) ;
#69439 = CARTESIAN_POINT ( 'NONE',  ( -13.19880346797889992, 1421.769212956930232, 206.7699246856669788 ) ) ;
#69440 = CARTESIAN_POINT ( 'NONE',  ( 0.1651937675056289745, 1483.163554816820124, 181.9584872145249790 ) ) ;
#69442 = ORIENTED_EDGE ( 'NONE', *, *, #63186, .T. ) ;
#69441 = DIRECTION ( 'NONE',  ( 0.000000000000000000, 1.000000000000000000, 0.000000000000000000 ) ) ;
#69443 = CARTESIAN_POINT ( 'NONE',  ( -18.29245442332561566, 1445.052233488289403, 161.2175811807110506 ) ) ;
#69444 = CARTESIAN_POINT ( 'NONE',  ( -3.148024555753120272E-16, 1383.870885931430166, 218.4497379877689980 ) ) ;
#69445 = CARTESIAN_POINT ( 'NONE',  ( -4.293363079010000583, 1475.442267412990077, 199.5995467683989943 ) ) ;
#69447 = VERTEX_POINT ( 'NONE', #71798 ) ;
#69446 = CARTESIAN_POINT ( 'NONE',  ( -31.65140982495776711, 1525.320827368861046, 216.1854560261664631 ) ) ;
#69448 = CARTESIAN_POINT ( 'NONE',  ( -3.406331129536729563, 1508.551704408389924, 219.9476367669959984 ) ) ;
#69449 = VERTEX_POINT ( 'NONE', #104802 ) ;
#69450 = CARTESIAN_POINT ( 'NONE',  ( -5.789140635075550101, 1391.897372272190069, 203.1891863557009970 ) ) ;
#69451 = CARTESIAN_POINT ( 'NONE',  ( -14.47059702760379984, 1380.054458738409949, 208.7831629986500275 ) ) ;
#69452 = CARTESIAN_POINT ( 'NONE',  ( -13.83520620040000004, 1414.913060387329779, 218.3795407500680312 ) ) ;
#69453 = CARTESIAN_POINT ( 'NONE',  ( 11.60004869885205459, 1426.267709371766387, 138.3562380925339994 ) ) ;
#69454 = CARTESIAN_POINT ( 'NONE',  ( -2.967054383202428536, 1368.722141705661670, 210.5451987844712107 ) ) ;
#69455 = EDGE_CURVE ( 'NONE', #99393, #80494, #103696, .T. ) ;
#69456 = CONICAL_SURFACE ( 'NONE', #15764, 0.9999999999999836797, 0.7853981633970000820 ) ;
#69457 = CARTESIAN_POINT ( 'NONE',  ( 11.75869035456349998, 1521.951704408389787, 227.2994842691620079 ) ) ;
#69458 = CARTESIAN_POINT ( 'NONE',  ( -10.57308237661970018, 1471.786795378390025, 206.9537732482530146 ) ) ;
#69459 = DIRECTION ( 'NONE',  ( 4.057416247971030182E-16, 1.000000000000000000, -4.440892098500000003E-16 ) ) ;
#69460 = CARTESIAN_POINT ( 'NONE',  ( -10.81222349729999976, 1391.793768475530214, 204.0084625770589923 ) ) ;
#69461 = CARTESIAN_POINT ( 'NONE',  ( -86.45172696223220044, 1385.181189174330257, 290.0270867646340207 ) ) ;
#69462 = CARTESIAN_POINT ( 'NONE',  ( -17.70224057689999952, 1414.004052165529856, 192.9401193470979763 ) ) ;
#69463 = DIRECTION ( 'NONE',  ( -0.000000000000000000, -1.000000000000000000, -0.000000000000000000 ) ) ;
#69464 = ORIENTED_EDGE ( 'NONE', *, *, #80331, .F. ) ;
#69465 = CARTESIAN_POINT ( 'NONE',  ( 13.31869796660000027, 1443.086052842849995, 169.3753098992980028 ) ) ;
#69467 = EDGE_LOOP ( 'NONE', ( #88392, #52316, #64366, #73703 ) ) ;
#69466 = DIRECTION ( 'NONE',  ( -9.500914144214121536E-47, 1.000000000000000000, -1.836970198721029688E-16 ) ) ;
#69468 = CARTESIAN_POINT ( 'NONE',  ( 6.030521501068090373, 1467.020543277260003, 217.0291475865519999 ) ) ;
#69469 = EDGE_LOOP ( 'NONE', ( #73742, #23109, #37010, #9256 ) ) ;
#69470 = CARTESIAN_POINT ( 'NONE',  ( 6.055110513760000757, 1450.647404142589949, 209.2214892968010247 ) ) ;
#69471 = CARTESIAN_POINT ( 'NONE',  ( -8.082564370840000123, 1362.241991287400197, 207.6218459616989946 ) ) ;
#69472 = CARTESIAN_POINT ( 'NONE',  ( -10.05915832670000043, 1494.201315354589951, 204.1613691274089888 ) ) ;
#69473 = EDGE_CURVE ( 'NONE', #32914, #51052, #71490, .T. ) ;
#69474 = CARTESIAN_POINT ( 'NONE',  ( 30.77169378701360003, 1461.664014259019268, 269.4792440743883617 ) ) ;
#69475 = CARTESIAN_POINT ( 'NONE',  ( -31.97743984922245275, 1525.878013734321485, 220.1676294520837303 ) ) ;
#69476 = CARTESIAN_POINT ( 'NONE',  ( 18.74698803448425366, 1436.847809687247036, 213.8123656996561408 ) ) ;
#69477 = CARTESIAN_POINT ( 'NONE',  ( -3.669386717783980068, 1517.051704642929963, 215.6629163041010031 ) ) ;
#69478 = CARTESIAN_POINT ( 'NONE',  ( -106.6287828259400357, 1306.483669372789791, 305.9508215967690603 ) ) ;
#69479 = CARTESIAN_POINT ( 'NONE',  ( -9.351945459739999578, 1366.519103298159735, 207.6218459616989946 ) ) ;
#69480 = CARTESIAN_POINT ( 'NONE',  ( 1.269526426719999934, 1457.689347263989930, 199.6687966702490087 ) ) ;
#69481 = CARTESIAN_POINT ( 'NONE',  ( 1.118104729594999958, 1516.965971551240045, 206.8221779662269739 ) ) ;
#69482 = AXIS2_PLACEMENT_3D ( 'NONE', #7441, #101474, #50008 ) ;
#69483 = CARTESIAN_POINT ( 'NONE',  ( -2.485536261606702269, 1523.919934424249959, 175.4381607306359570 ) ) ;
#69484 = CARTESIAN_POINT ( 'NONE',  ( -0.0002840614181677549835, 1443.913060387330006, 126.7977857662820043 ) ) ;
#69485 = CARTESIAN_POINT ( 'NONE',  ( -2.021380015520000129, 1496.949193287590106, 197.9094991689989911 ) ) ;
#69488 = EDGE_LOOP ( 'NONE', ( #79024, #38493, #83748, #67282, #6622 ) ) ;
#69487 = CARTESIAN_POINT ( 'NONE',  ( -68.75534438227138878, 1379.747886361640212, 280.3294090916749610 ) ) ;
#69486 = CIRCLE ( 'NONE', #74913, 2.000000020766222075 ) ;
#69489 = LINE ( 'NONE', #42605, #18724 ) ;
#69490 = ORIENTED_EDGE ( 'NONE', *, *, #80331, .T. ) ;
#69491 = AXIS2_PLACEMENT_3D ( 'NONE', #89193, #78595, #79712 ) ;
#69492 = CARTESIAN_POINT ( 'NONE',  ( 30.10637292080000194, 1413.645514435030009, 266.8104572860979715 ) ) ;
#69493 = CARTESIAN_POINT ( 'NONE',  ( -24.75581127569999751, 1430.360917255730101, 207.9708729454779927 ) ) ;
#69495 = CARTESIAN_POINT ( 'NONE',  ( 16.16892249492000033, 1409.485760428959793, 192.9099775984909968 ) ) ;
#69494 = CARTESIAN_POINT ( 'NONE',  ( -11.30596056951389983, 1425.565231672570008, 135.2551855802589955 ) ) ;
#69496 = CARTESIAN_POINT ( 'NONE',  ( 0.7574259850960020080, 1516.837969789639828, 212.3776558342370038 ) ) ;
#69497 = CARTESIAN_POINT ( 'NONE',  ( 29.03576926601821029, 1510.037895104773270, 201.5770025554943459 ) ) ;
#69498 = CARTESIAN_POINT ( 'NONE',  ( -22.95227133490000071, 1507.624369720630057, 208.0069050751279747 ) ) ;
#69499 = CARTESIAN_POINT ( 'NONE',  ( -43.15848075010000429, 1435.559015939599931, 263.9122388061979905 ) ) ;
#69500 = CARTESIAN_POINT ( 'NONE',  ( 19.18955701931950131, 1509.607256104009821, 231.7035876696010064 ) ) ;
#69502 = EDGE_CURVE ( 'NONE', #109440, #23969, #56472, .T. ) ;
#69501 = CARTESIAN_POINT ( 'NONE',  ( 17.39313975581298521, 1460.068489132931745, 228.4728633170865351 ) ) ;
#69503 = CARTESIAN_POINT ( 'NONE',  ( -5.093521796410000135, 1391.866579497489965, 214.5262673350590035 ) ) ;
#69504 = CARTESIAN_POINT ( 'NONE',  ( -37.00411130546480365, 1437.912636928700067, 136.5589373068169721 ) ) ;
#69505 = ORIENTED_EDGE ( 'NONE', *, *, #4527, .F. ) ;
#69506 = CARTESIAN_POINT ( 'NONE',  ( 11.64773666870840074, 1396.497100933559750, 213.5793525411820042 ) ) ;
#69507 = CARTESIAN_POINT ( 'NONE',  ( 9.226870674553810048, 1461.939016979510143, 206.0483255767620108 ) ) ;
#69508 = ADVANCED_FACE ( 'NONE', ( #88563 ), #13882, .F. ) ;
#69509 = CARTESIAN_POINT ( 'NONE',  ( -17.59666625160000208, 1458.100482827429914, 230.0625289195980088 ) ) ;
#69510 = ORIENTED_EDGE ( 'NONE', *, *, #65971, .F. ) ;
#69511 = ORIENTED_EDGE ( 'NONE', *, *, #42085, .F. ) ;
#69512 = CARTESIAN_POINT ( 'NONE',  ( -2.446787376320000096, 1432.353341358199941, 150.2884730787980061 ) ) ;
#69513 = CARTESIAN_POINT ( 'NONE',  ( -11.81421925085510161, 1428.091866732929930, 150.2203729037190101 ) ) ;
#69514 = EDGE_CURVE ( 'NONE', #91380, #72816, #23142, .T. ) ;
#69515 = ORIENTED_EDGE ( 'NONE', *, *, #27283, .T. ) ;
#69516 = CARTESIAN_POINT ( 'NONE',  ( 0.2232360794380000291, 1421.820066533229920, 227.4074839354979929 ) ) ;
#69517 = AXIS2_PLACEMENT_3D ( 'NONE', #88207, #13116, #81423 ) ;
#69518 = CARTESIAN_POINT ( 'NONE',  ( -14.73770141384289900, 1508.451171878049990, 209.7916384116149970 ) ) ;
#69519 = CARTESIAN_POINT ( 'NONE',  ( 3.448830483803570157, 1523.382868172864164, 175.1594891075192493 ) ) ;
#69520 = ADVANCED_FACE ( 'NONE', ( #96964 ), #42795, .T. ) ;
#69521 = CARTESIAN_POINT ( 'NONE',  ( 27.44229968044188439, 1509.334241250234754, 206.1596417527201197 ) ) ;
#69522 = CARTESIAN_POINT ( 'NONE',  ( 1.597238071469150089, 1420.983502555679934, 183.0619176556710102 ) ) ;
#69523 = CARTESIAN_POINT ( 'NONE',  ( 9.248740396683809095, 1450.941274981350034, 208.9745031941699835 ) ) ;
#69524 = CARTESIAN_POINT ( 'NONE',  ( -11.97707799540000018, 1391.854779651599983, 210.9632173721890069 ) ) ;
#69525 = CARTESIAN_POINT ( 'NONE',  ( -95.05970678514869121, 1384.857596447410060, 294.9623361036900064 ) ) ;
#69526 = EDGE_LOOP ( 'NONE', ( #82673, #27519, #76558, #93779 ) ) ;
#69527 = CARTESIAN_POINT ( 'NONE',  ( -4.618749106614999711, 1516.729202374750002, 202.5720834851169911 ) ) ;
#69528 = CARTESIAN_POINT ( 'NONE',  ( 6.944466742375000834, 1516.939530130779985, 209.1105810159089913 ) ) ;
#69529 = VERTEX_POINT ( 'NONE', #101193 ) ;
#69530 = CARTESIAN_POINT ( 'NONE',  ( 11.86506748840099945, 1432.263814426909903, 149.9818949723999992 ) ) ;
#69531 = CARTESIAN_POINT ( 'NONE',  ( -19.37374569213905318, 1524.382868172863937, 234.3668155954421479 ) ) ;
#69532 = ORIENTED_EDGE ( 'NONE', *, *, #63153, .F. ) ;
#69533 = CARTESIAN_POINT ( 'NONE',  ( 29.73378234562457934, 1526.349684470114653, 201.0212898931769985 ) ) ;
#69534 = CARTESIAN_POINT ( 'NONE',  ( -17.22623662315568893, 1443.501467202830781, 162.9225832754749490 ) ) ;
#69535 = CARTESIAN_POINT ( 'NONE',  ( 11.24596261149999954, 1509.248420230330112, 235.4555975505980143 ) ) ;
#69536 = CARTESIAN_POINT ( 'NONE',  ( -9.042214778654647844, 1490.548019693297647, 215.3561743177068308 ) ) ;
#69537 = CARTESIAN_POINT ( 'NONE',  ( -5.273497523000000520, 1420.712481594430074, 186.5671558910979968 ) ) ;
#69538 = CARTESIAN_POINT ( 'NONE',  ( 3.549205703259999733, 1408.030536462830014, 270.2903253923980174 ) ) ;
#69539 = CARTESIAN_POINT ( 'NONE',  ( -17.69507376891250416, 1519.551704408389924, 216.2288492090537488 ) ) ;
#69540 = CARTESIAN_POINT ( 'NONE',  ( -6.325873692910000123, 1474.305489392889967, 200.4708573935690197 ) ) ;
#69541 = CARTESIAN_POINT ( 'NONE',  ( 11.41833521740000101, 1492.743966703789738, 212.4764450907990181 ) ) ;
#69542 = CARTESIAN_POINT ( 'NONE',  ( -1.331958139231829923E-15, 1375.413060387289988, 209.1218459616989946 ) ) ;
#69543 = CARTESIAN_POINT ( 'NONE',  ( -3.500000000000000000, 1409.663060387330006, 146.1721969590979882 ) ) ;
#69545 = CARTESIAN_POINT ( 'NONE',  ( 9.607386820528988736, 1468.930745809150039, 203.2606402744570175 ) ) ;
#69544 = CARTESIAN_POINT ( 'NONE',  ( -20.79256037440000071, 1505.243615344689943, 209.5690373176560115 ) ) ;
#69546 = CARTESIAN_POINT ( 'NONE',  ( -4.619247800516277813, 1423.719106761370995, 184.4314750194308488 ) ) ;
#69547 = CARTESIAN_POINT ( 'NONE',  ( 17.68653785626990071, 1413.495428231110054, 224.8840759871750095 ) ) ;
#69548 = EDGE_CURVE ( 'NONE', #43965, #75409, #97143, .T. ) ;
#69549 = CARTESIAN_POINT ( 'NONE',  ( -6.252266492314999979, 1511.741868877540128, 200.3335294429169835 ) ) ;
#69550 = ORIENTED_EDGE ( 'NONE', *, *, #45218, .F. ) ;
#69551 = CARTESIAN_POINT ( 'NONE',  ( 18.02578551396119977, 1424.483936704789812, 224.5809757487189984 ) ) ;
#69552 = B_SPLINE_SURFACE_WITH_KNOTS ( 'NONE', 5, 5, ( 
 ( #80352, #53511, #3669, #55169, #89294, #12590 ),
 ( #4731, #98239, #45115, #46769, #80899, #64118 ),
 ( #21510, #55722, #38875, #104440, #61922, #2567 ),
 ( #70883, #104996, #96038, #19309, #28286, #15323 ),
 ( #66875, #74170, #49517, #6396, #5851, #23177 ),
 ( #47846, #100985, #107196, #99326, #41093, #108299 ),
 ( #74717, #75272, #84195, #98791, #99878, #57378 ),
 ( #83641, #39992, #32144, #31584, #32695, #109419 ),
 ( #65762, #23731, #66331, #64673, #73054, #91504 ) ),
 .UNSPECIFIED., .F., .F., .F.,
 ( 6, 3, 6 ),
 ( 6, 6 ),
 ( 13.48398407686089939, 16.53063851469999790, 19.57724985460000156 ),
 ( -9.649567376679359532E-06, 2.000042901542320006 ),
 .UNSPECIFIED. ) ;
#69553 = CARTESIAN_POINT ( 'NONE',  ( -19.07966196791950608, 1524.244163922423695, 179.2412984082268679 ) ) ;
#69554 = CARTESIAN_POINT ( 'NONE',  ( -2.983004277789705228, 1485.615614723739100, 182.7116838820144267 ) ) ;
#69555 = ADVANCED_FACE ( 'NONE', ( #39664 ), #48070, .F. ) ;
#69556 = LINE ( 'NONE', #25839, #6236 ) ;
#69558 = VERTEX_POINT ( 'NONE', #73832 ) ;
#69557 = CARTESIAN_POINT ( 'NONE',  ( 1.403832663128229852, 1515.079617817420058, 204.7927853908689997 ) ) ;
#69559 = CARTESIAN_POINT ( 'NONE',  ( -15.76868314863217080, 1415.798507515539768, 209.6929715414478039 ) ) ;
#69561 = B_SPLINE_CURVE_WITH_KNOTS ( 'NONE', 5,
 ( #87089, #28287, #2009, #36689, #19310, #17645 ),
 .UNSPECIFIED., .F., .F.,
 ( 6, 6 ),
 ( -22.82719364450599997, -6.734755223259998758 ),
 .UNSPECIFIED. ) ;
#69560 = CARTESIAN_POINT ( 'NONE',  ( -2.446787376320000096, 1432.353341358199941, 150.2884730787980061 ) ) ;
#69562 = CARTESIAN_POINT ( 'NONE',  ( -11.54804583780000193, 1430.179206417029945, 150.8480334790980066 ) ) ;
#69563 = CARTESIAN_POINT ( 'NONE',  ( -10.96946876072200006, 1432.347663854339999, 151.7701362700559855 ) ) ;
#69564 = LINE ( 'NONE', #43239, #41975 ) ;
#69565 = CARTESIAN_POINT ( 'NONE',  ( 1.190307662709999936E-15, 1432.413060387330006, 146.1721969590979882 ) ) ;
#69566 = CARTESIAN_POINT ( 'NONE',  ( -2.188078410709979771, 1508.020976590390092, 220.9453026643990086 ) ) ;
#69567 = CARTESIAN_POINT ( 'NONE',  ( -14.72577135216500110, 1514.214451716350140, 224.1399939629670257 ) ) ;
#69568 = CARTESIAN_POINT ( 'NONE',  ( 16.49337488880000180, 1410.410615523229808, 226.5881202531979852 ) ) ;
#69569 = CARTESIAN_POINT ( 'NONE',  ( -8.131139148520000859, 1477.102955269890117, 215.8146692214089910 ) ) ;
#69570 = CARTESIAN_POINT ( 'NONE',  ( -16.61244015609999991, 1459.967035441530015, 228.4924331886979871 ) ) ;
#69572 = VECTOR ( 'NONE', #78688, 1000.000000000000000 ) ;
#69571 = CARTESIAN_POINT ( 'NONE',  ( -6.563254928984999736, 1517.139039350860003, 206.6385234782069915 ) ) ;
#69573 = CARTESIAN_POINT ( 'NONE',  ( 35.72701205430000471, 1418.844138006729963, 266.4694652101980523 ) ) ;
#69574 = CARTESIAN_POINT ( 'NONE',  ( 22.68396052030000121, 1435.289475021379985, 139.2169948456979967 ) ) ;
#69575 = CIRCLE ( 'NONE', #6866, 27.48039236454309275 ) ;
#69576 = CARTESIAN_POINT ( 'NONE',  ( 23.44272364520000096, 1430.296227159529963, 206.5262785095279696 ) ) ;
#69577 = CARTESIAN_POINT ( 'NONE',  ( -22.43751286540000223, 1431.503785808020211, 216.9270791274780095 ) ) ;
#69578 = CIRCLE ( 'NONE', #21222, 28.99999999999999645 ) ;
#69579 = DIRECTION ( 'NONE',  ( -0.7074300732239336975, -0.02470400246746228684, -0.7063514732485997039 ) ) ;
#69580 = CARTESIAN_POINT ( 'NONE',  ( 3.827327205999999649, 1409.546157813730133, 126.8043280305979863 ) ) ;
#69581 = CARTESIAN_POINT ( 'NONE',  ( -1.464544818259999825, 1451.650746978230018, 183.9079519998980174 ) ) ;
#69582 = DIRECTION ( 'NONE',  ( 0.02307773700814929468, -0.7475172611785151355, -0.6638413683213441052 ) ) ;
#69583 = DIRECTION ( 'NONE',  ( 1.224646799147353454E-16, 0.000000000000000000, -1.000000000000000000 ) ) ;
#69584 = CARTESIAN_POINT ( 'NONE',  ( -12.28185623160000084, 1441.208366488439879, 187.9047578019979881 ) ) ;
#69585 = CARTESIAN_POINT ( 'NONE',  ( -15.29461995089999959, 1453.313060387329870, 223.0352892562980003 ) ) ;
#69586 = CARTESIAN_POINT ( 'NONE',  ( -30.20925992649999969, 1436.447313216129942, 136.6262449664980068 ) ) ;
#69587 = CARTESIAN_POINT ( 'NONE',  ( -8.178650747341842830, 1456.230684632761040, 227.1998168167369840 ) ) ;
#69588 = ORIENTED_EDGE ( 'NONE', *, *, #58846, .F. ) ;
#69589 = CARTESIAN_POINT ( 'NONE',  ( -2.830985251735000485, 1512.320675624280057, 201.3411128641770063 ) ) ;
#69590 = CARTESIAN_POINT ( 'NONE',  ( -14.20386470660680089, 1409.409070272629833, 204.4985088955900210 ) ) ;
#69591 = ORIENTED_EDGE ( 'NONE', *, *, #27476, .T. ) ;
#69592 = CARTESIAN_POINT ( 'NONE',  ( -12.96253978517979988, 1508.551708299209849, 210.0000646660610073 ) ) ;
#69593 = CARTESIAN_POINT ( 'NONE',  ( -21.24668275234344250, 1409.655010898162118, 211.0876053273857735 ) ) ;
#69594 = CARTESIAN_POINT ( 'NONE',  ( -21.91923426869999858, 1471.782736223630081, 267.0360668916979989 ) ) ;
#69595 = CARTESIAN_POINT ( 'NONE',  ( -31.16641183314643015, 1524.201816949778276, 196.3723131635786672 ) ) ;
#69596 = CARTESIAN_POINT ( 'NONE',  ( 0.2081566899150210093, 1419.757203975580069, 184.2452808931809898 ) ) ;
#69597 = CARTESIAN_POINT ( 'NONE',  ( -24.19977663905823562, 1444.537531331827950, 211.5031488161932032 ) ) ;
#69598 = CARTESIAN_POINT ( 'NONE',  ( -73.71138866091139619, 1384.652804003510028, 298.8779072345359964 ) ) ;
#69599 = CARTESIAN_POINT ( 'NONE',  ( -22.04486723005910065, 1384.954349268969963, 202.2380667361449866 ) ) ;
#69600 = CARTESIAN_POINT ( 'NONE',  ( 16.82531969527569871, 1423.253125815850126, 227.2938718802809888 ) ) ;
#69601 = CARTESIAN_POINT ( 'NONE',  ( 14.59411311889999929, 1414.913060387329779, 216.7687570508280146 ) ) ;
#69602 = CARTESIAN_POINT ( 'NONE',  ( -28.25086642335310216, 1508.135711581739997, 208.8579954535609886 ) ) ;
#69603 = B_SPLINE_CURVE_WITH_KNOTS ( 'NONE', 3,
 ( #73919, #91256, #6697, #101840, #101279, #100210, #85049, #15077, #34104, #91799, #24023, #8339, #84507, #93447, #24575, #25134, #59337, #42503, #41962, #76116 ),
 .UNSPECIFIED., .F., .F.,
 ( 4, 2, 2, 2, 1, 1, 1, 1, 2, 2, 2, 4 ),
 ( 0.000000000000000000, 0.2500000000006933898, 0.3750000000010487722, 0.4375000000012101986, 0.4687500000012878587, 0.4843750000013154478, 0.4921875000013438695, 0.4960937500013579138, 0.4980468750013504198, 0.5000000000013429258, 0.7500000000006714629, 1.000000000000000000 ),
 .UNSPECIFIED. ) ;
#69604 = CARTESIAN_POINT ( 'NONE',  ( -9.687216859550042969, 1494.456727822050880, 203.5511929442279779 ) ) ;
#69605 = CARTESIAN_POINT ( 'NONE',  ( 4.091781189549999809, 1515.531881637889910, 208.0020576612490117 ) ) ;
#69606 = CARTESIAN_POINT ( 'NONE',  ( -8.156530043329999202, 1384.922241695169760, 199.6468276065789667 ) ) ;
#69607 = CARTESIAN_POINT ( 'NONE',  ( -22.72436476140000039, 1409.706612691029704, 207.2124451185780174 ) ) ;
#69608 = FACE_OUTER_BOUND ( 'NONE', #58943, .T. ) ;
#69609 = CARTESIAN_POINT ( 'NONE',  ( 5.161034791280000533, 1485.814572579490005, 218.5690567784690188 ) ) ;
#69610 = CARTESIAN_POINT ( 'NONE',  ( 10.85852436008239863, 1479.618465607619783, 207.8019171430970005 ) ) ;
#69611 = CARTESIAN_POINT ( 'NONE',  ( 0.8182520991989999937, 1433.447543843880112, 150.4377610267980003 ) ) ;
#69612 = CARTESIAN_POINT ( 'NONE',  ( 10.41726918004940039, 1452.895226299490105, 190.0448634872510354 ) ) ;
#69613 = CARTESIAN_POINT ( 'NONE',  ( -5.513199828441160300, 1509.038617475689989, 216.6345962050160097 ) ) ;
#69614 = CARTESIAN_POINT ( 'NONE',  ( -21.51339057085170126, 1505.551704407249872, 209.1218459615049881 ) ) ;
#69616 = CARTESIAN_POINT ( 'NONE',  ( -8.515407867320000435, 1383.766919741620086, 199.9370010572289971 ) ) ;
#69615 = CARTESIAN_POINT ( 'NONE',  ( -9.638115897709079505, 1516.551188146539971, 203.7504991310609910 ) ) ;
#69617 = CARTESIAN_POINT ( 'NONE',  ( -4.994992779129999505, 1391.721842640289879, 203.5951896846190152 ) ) ;
#69618 = DIRECTION ( 'NONE',  ( 0.2803360189751119558, -0.4513760013199308863, -0.8471548984085587319 ) ) ;
#69619 = CARTESIAN_POINT ( 'NONE',  ( -10.84352170600000242, 1490.621361297190106, 211.6123805837090117 ) ) ;
#69620 = CARTESIAN_POINT ( 'NONE',  ( -22.98095509850000084, 1420.941332502029809, 212.0408358815379870 ) ) ;
#69621 = CARTESIAN_POINT ( 'NONE',  ( -7.450033292409999675, 1367.931913175459840, 210.6218459616991936 ) ) ;
#69622 = CARTESIAN_POINT ( 'NONE',  ( -4.621267922064999922, 1516.830644417779922, 204.1223895416970038 ) ) ;
#69623 = CARTESIAN_POINT ( 'NONE',  ( 0.000000000000000000, 1399.332476024090056, 209.1218459616989946 ) ) ;
#69624 = SURFACE_SIDE_STYLE ('',( #77991 ) ) ;
#69625 = FACE_BOUND ( 'NONE', #42900, .T. ) ;
#69626 = CARTESIAN_POINT ( 'NONE',  ( -17.84734352359999932, 1410.892954231429940, 195.0519780797979763 ) ) ;
#69627 = CARTESIAN_POINT ( 'NONE',  ( 6.687607498646199744, 1504.526125536900054, 220.0428038810069893 ) ) ;
#69628 = AXIS2_PLACEMENT_3D ( 'NONE', #102662, #25405, #17555 ) ;
#69629 = CARTESIAN_POINT ( 'NONE',  ( 38.26972034215779672, 1449.715126992240130, 136.0601146782780120 ) ) ;
#69631 = ORIENTED_EDGE ( 'NONE', *, *, #47977, .T. ) ;
#69630 = CARTESIAN_POINT ( 'NONE',  ( -65.86034991249999848, 1379.747388898590089, 276.1189993382589591 ) ) ;
#69632 = ORIENTED_EDGE ( 'NONE', *, *, #21409, .F. ) ;
#69633 = CARTESIAN_POINT ( 'NONE',  ( 11.94173468258579973, 1433.516563288440011, 150.0939282449400025 ) ) ;
#69634 = CARTESIAN_POINT ( 'NONE',  ( 21.39303731107166939, 1524.776010967693765, 184.2561860187820741 ) ) ;
#69635 = ORIENTED_EDGE ( 'NONE', *, *, #71060, .T. ) ;
#69636 = CARTESIAN_POINT ( 'NONE',  ( 0.7518804359284473326, 1457.963929617798613, 199.6002294408864088 ) ) ;
#69637 = CARTESIAN_POINT ( 'NONE',  ( -10.23096445512489971, 1448.798712686370209, 207.3500612127919851 ) ) ;
#69638 = CARTESIAN_POINT ( 'NONE',  ( -7.769002550049999734, 1384.928845206309916, 218.9178303808890007 ) ) ;
#69640 = CARTESIAN_POINT ( 'NONE',  ( 9.253402716490001012, 1428.330636036430178, 123.0297916884979941 ) ) ;
#69639 = CARTESIAN_POINT ( 'NONE',  ( 16.08972158192780100, 1424.754442430379868, 191.0877091364910143 ) ) ;
#69641 = CARTESIAN_POINT ( 'NONE',  ( 19.21540365814130169, 1507.816561716200113, 229.6838698100480087 ) ) ;
#69642 = CIRCLE ( 'NONE', #46373, 1.999999999999997780 ) ;
#69643 = CARTESIAN_POINT ( 'NONE',  ( 3.826470069039999977, 1488.170811478430096, 182.4750432301979970 ) ) ;
#69644 = CARTESIAN_POINT ( 'NONE',  ( 2.995626829160000337, 1468.394067435089937, 218.6771455671389788 ) ) ;
#69645 = CARTESIAN_POINT ( 'NONE',  ( 16.57640676229999954, 1409.993768047430194, 226.3203803305979704 ) ) ;
#69646 = EDGE_CURVE ( 'NONE', #102504, #76431, #87526, .T. ) ;
#69647 = B_SPLINE_SURFACE_WITH_KNOTS ( 'NONE', 5, 5, ( 
 ( #84766, #33265, #84221, #41120, #101010, #34382 ),
 ( #50635, #24309, #68555, #75299, #8064, #110531 ),
 ( #9187, #60150, #51749, #42234, #50094, #75839 ),
 ( #76382, #77497, #33816, #25399, #94841, #51185 ),
 ( #85314, #68010, #16985, #69113, #83669, #102120 ),
 ( #59592, #43349, #85884, #109443, #32723, #18117 ),
 ( #797, #58490, #25955, #17547, #8609, #66903 ),
 ( #59049, #67454, #102655, #6966, #15894, #41679 ),
 ( #92617, #7520, #101554, #24846, #93170, #16440 ),
 ( #42786, #34926, #76946, #94271, #103214, #26522 ),
 ( #60719, #97604, #20325, #95399, #53409, #28744 ),
 ( #54530, #45573, #96501, #1344, #104900, #18662 ),
 ( #45021, #3570, #37144, #71341, #19207, #37694 ),
 ( #79715, #103799, #27639, #52861, #63485, #70788 ),
 ( #19781, #78598, #2474, #28189, #1916, #35483 ),
 ( #29289, #86988, #11942, #71897, #10277, #62375 ),
 ( #44454, #43892, #27098, #95947, #87560, #70239 ),
 ( #53982, #46123, #52313, #78036, #10849, #104346 ),
 ( #105455, #3022, #62949, #97060, #88116, #79166 ),
 ( #36052, #9727, #61824, #88664, #61283, #36591 ),
 ( #11405, #80252, #106013, #69677, #86436, #98136 ),
 ( #65113, #99224, #108748, #108192, #99779, #21953 ),
 ( #12489, #40437, #56146, #90282, #98693, #106549 ),
 ( #55621, #46672, #80804, #107095, #38234, #29837 ),
 ( #81329, #5187, #13563, #4644, #39342, #4110 ),
 ( #23071, #64023, #47749, #31481, #89197, #22502 ),
 ( #20874, #81884, #21412, #56703, #90839, #14124 ) ),
 .UNSPECIFIED., .F., .F., .F.,
 ( 6, 3, 3, 3, 3, 3, 3, 3, 6 ),
 ( 6, 6 ),
 ( 10.40199318109999993, 19.90315615969999996, 23.28476991740000202, 24.97557679630000038, 25.82098023580000046, 26.66638367519999875, 26.99360131220000270, 28.03535140669999848, 29.40431913829999999 ),
 ( 0.000000000000000000, 1.455169987240000129 ),
 .UNSPECIFIED. ) ;
#69648 = CARTESIAN_POINT ( 'NONE',  ( 0.01323701367210150005, 1516.939658295650133, 211.6080660720070341 ) ) ;
#69649 = CARTESIAN_POINT ( 'NONE',  ( 14.17422268772769911, 1415.724942525210054, 197.1424870051829998 ) ) ;
#69650 = CARTESIAN_POINT ( 'NONE',  ( -7.022715574297880181, 1424.820957301160206, 207.8595816151610336 ) ) ;
#69651 = CARTESIAN_POINT ( 'NONE',  ( 7.163002496964999466, 1512.132770473880100, 202.2540665605069705 ) ) ;
#69652 = ORIENTED_EDGE ( 'NONE', *, *, #28887, .F. ) ;
#69653 = CARTESIAN_POINT ( 'NONE',  ( 14.19348081423260055, 1435.301921962149891, 149.4341381306140022 ) ) ;
#69654 = CARTESIAN_POINT ( 'NONE',  ( -5.013380061527799469, 1375.424024322329842, 203.5256954671220058 ) ) ;
#69655 = ORIENTED_EDGE ( 'NONE', *, *, #94079, .T. ) ;
#69656 = ORIENTED_EDGE ( 'NONE', *, *, #40545, .F. ) ;
#69657 = CARTESIAN_POINT ( 'NONE',  ( -6.964055617815001042, 1512.881909847370025, 216.3028661151370216 ) ) ;
#69658 = DIRECTION ( 'NONE',  ( 0.000000000000000000, -0.7071067811865474617, -0.7071067811865474617 ) ) ;
#69659 = CARTESIAN_POINT ( 'NONE',  ( 21.13734888319999783, 1496.938803861589804, 209.1218459616989946 ) ) ;
#69660 = CARTESIAN_POINT ( 'NONE',  ( 5.779603100124999671, 1516.738222552470233, 216.8362174732170047 ) ) ;
#69661 = CARTESIAN_POINT ( 'NONE',  ( -0.4364796396607459328, 1465.308788633660015, 198.1255561066119810 ) ) ;
#69662 = CONICAL_SURFACE ( 'NONE', #24835, 0.9999999999999956701, 0.7853981633970000820 ) ;
#69663 = CARTESIAN_POINT ( 'NONE',  ( 11.51161966288469962, 1422.036711861869890, 209.8677670191129891 ) ) ;
#69664 = CARTESIAN_POINT ( 'NONE',  ( -35.67105607187449579, 1379.642165080909763, 218.6247323468043646 ) ) ;
#69665 = CARTESIAN_POINT ( 'NONE',  ( 4.265655661611780225, 1446.644466445230137, 158.6693615694720165 ) ) ;
#69666 = EDGE_CURVE ( 'NONE', #104566, #18861, #90042, .T. ) ;
#69667 = AXIS2_PLACEMENT_3D ( 'NONE', #109380, #41615, #60086 ) ;
#69668 = CARTESIAN_POINT ( 'NONE',  ( 0.6067091484059999873, 1507.391323370129840, 237.3179893959980120 ) ) ;
#69669 = ORIENTED_EDGE ( 'NONE', *, *, #35083, .F. ) ;
#69670 = CARTESIAN_POINT ( 'NONE',  ( 2.283570633165000086, 1516.909589401870107, 206.2402975076569760 ) ) ;
#69671 = ORIENTED_EDGE ( 'NONE', *, *, #97914, .F. ) ;
#69672 = CARTESIAN_POINT ( 'NONE',  ( -103.9221348808119956, 1379.919223396519783, 305.0512315340399709 ) ) ;
#69673 = CARTESIAN_POINT ( 'NONE',  ( -19.35070331030000190, 1509.010601545330019, 230.0701437765980018 ) ) ;
#69674 = ORIENTED_EDGE ( 'NONE', *, *, #8299, .T. ) ;
#69675 = CARTESIAN_POINT ( 'NONE',  ( -5.513203988984379578, 1508.884118749120262, 201.6131408764620119 ) ) ;
#69676 = EDGE_CURVE ( 'NONE', #66886, #75744, #88690, .T. ) ;
#69677 = CARTESIAN_POINT ( 'NONE',  ( -15.29119482810000008, 1409.948801712029990, 191.1498944753979856 ) ) ;
#69678 = CARTESIAN_POINT ( 'NONE',  ( -24.49292865060000324, 1441.580045819019915, 211.0188571790179992 ) ) ;
#69679 = CARTESIAN_POINT ( 'NONE',  ( 2.727717259937589844, 1423.594114422599887, 192.7156380009489851 ) ) ;
#69680 = CARTESIAN_POINT ( 'NONE',  ( 0.005666290841312040041, 1455.183973234658879, 218.5515631892139083 ) ) ;
#69681 = DIRECTION ( 'NONE',  ( -0.4632728134665660691, -0.8857936774813760517, -0.02734705170200765062 ) ) ;
#69682 = CARTESIAN_POINT ( 'NONE',  ( -106.4218829409999927, 1384.032086002479900, 311.2287423822589858 ) ) ;
#69683 = DIRECTION ( 'NONE',  ( -0.9236849191514725499, -0.3806575521132582463, -0.04365773873301222185 ) ) ;
#69685 = CARTESIAN_POINT ( 'NONE',  ( 0.3722769099684289928, 1457.826255237599980, 228.9731060096619899 ) ) ;
#69684 = CARTESIAN_POINT ( 'NONE',  ( -24.04659120089169733, 1444.796772349889807, 212.0316830080810178 ) ) ;
#69686 = VECTOR ( 'NONE', #82596, 1000.000000000000000 ) ;
#69687 = B_SPLINE_SURFACE_WITH_KNOTS ( 'NONE', 5, 5, ( 
 ( #52120, #86248, #16267, #94652, #51559, #59424 ),
 ( #9539, #43162, #1169, #84593, #44271, #77317 ),
 ( #67821, #35300, #101933, #25220, #93536, #615 ),
 ( #16807, #34747, #69485, #51009, #85142, #8430 ),
 ( #26907, #61096, #42600, #76756, #105264, #97950 ),
 ( #45925, #54338, #4471, #10664, #71713, #78985 ),
 ( #87933, #3934, #54880, #2288, #38599, #21218 ),
 ( #29651, #45385, #72779, #63295, #106366, #80618 ),
 ( #3381, #38061, #105831, #37509, #104707, #36946 ) ),
 .UNSPECIFIED., .F., .F., .F.,
 ( 6, 3, 6 ),
 ( 6, 6 ),
 ( 4.164915011539999767, 8.224269361119999289, 13.59025040360000069 ),
 ( 0.000000000000000000, 2.000000000000000000 ),
 .UNSPECIFIED. ) ;
#69688 = CARTESIAN_POINT ( 'NONE',  ( 5.782749401605000727, 1516.858301627840092, 214.8983370654769942 ) ) ;
#69689 = CARTESIAN_POINT ( 'NONE',  ( 24.02347744240000083, 1410.714002832030019, 209.6150577782879907 ) ) ;
#69690 = CARTESIAN_POINT ( 'NONE',  ( 6.099947970667409791, 1511.445028088800200, 216.7805665003349986 ) ) ;
#69691 = CARTESIAN_POINT ( 'NONE',  ( 28.83249087089999918, 1509.587594255930071, 208.9222957011619997 ) ) ;
#69692 = CARTESIAN_POINT ( 'NONE',  ( 3.462620818104999998, 1516.938330505699923, 211.6001527901769919 ) ) ;
#69693 = CARTESIAN_POINT ( 'NONE',  ( -11.84714928711539983, 1482.159292582530043, 208.0957396826470074 ) ) ;
#69694 = EDGE_CURVE ( 'NONE', #98048, #53402, #46446, .T. ) ;
#69695 = FACE_OUTER_BOUND ( 'NONE', #69249, .T. ) ;
#69697 = VERTEX_POINT ( 'NONE', #82764 ) ;
#69696 = CARTESIAN_POINT ( 'NONE',  ( -90.54195131439999500, 1389.308449918279848, 306.1970171789590154 ) ) ;
#69698 = AXIS2_PLACEMENT_3D ( 'NONE', #42161, #25884, #76313 ) ;
#69699 = CARTESIAN_POINT ( 'NONE',  ( 26.00754374179999928, 1454.033399689230009, 240.2274373035980091 ) ) ;
#69700 = DIRECTION ( 'NONE',  ( 0.02616798426500965835, -0.9993150019883683122, -0.02616798426500960631 ) ) ;
#69701 = DIRECTION ( 'NONE',  ( 5.590778865670909642E-17, 1.000000000000000000, 0.000000000000000000 ) ) ;
#69702 = CARTESIAN_POINT ( 'NONE',  ( -7.988150404321079812, 1508.679516143240107, 235.8900466699099923 ) ) ;
#69703 = CARTESIAN_POINT ( 'NONE',  ( -18.92998585080000140, 1456.923645639730012, 227.1748017144979883 ) ) ;
#69705 = CARTESIAN_POINT ( 'NONE',  ( 17.79684371365149786, 1410.125370365290109, 222.8164932182040161 ) ) ;
#69704 = CARTESIAN_POINT ( 'NONE',  ( 11.86547437279999961, 1432.299053485889999, 150.3973020406980083 ) ) ;
#69706 = CARTESIAN_POINT ( 'NONE',  ( -0.3753211829319999526, 1470.816980702529918, 188.7016457681980057 ) ) ;
#69707 = CARTESIAN_POINT ( 'NONE',  ( -108.0462788022180121, 1381.309336268219795, 310.1032626428960270 ) ) ;
#69708 = ORIENTED_EDGE ( 'NONE', *, *, #69990, .F. ) ;
#69709 = CARTESIAN_POINT ( 'NONE',  ( 4.030514512585000375, 1516.901952101700090, 204.4990030879170320 ) ) ;
#69710 = CARTESIAN_POINT ( 'NONE',  ( 0.2126091594639999971, 1406.777959006730043, 269.6500587044980648 ) ) ;
#69711 = CARTESIAN_POINT ( 'NONE',  ( 28.73878200240000069, 1509.916640768729849, 206.8280204061180143 ) ) ;
#69712 = CARTESIAN_POINT ( 'NONE',  ( 12.45702690739999952, 1416.837177099529754, 223.4766769987980126 ) ) ;
#69713 = CARTESIAN_POINT ( 'NONE',  ( 2.478650075360000038, 1436.419591246580012, 157.6446810035980093 ) ) ;
#69714 =( BOUNDED_CURVE ( )  B_SPLINE_CURVE ( 3, ( #98010, #72835, #65544, #108065 ),
 .UNSPECIFIED., .F., .T. ) 
 B_SPLINE_CURVE_WITH_KNOTS ( ( 4, 4 ),
 ( 4.212388980384758952, 4.712388980384758952 ),
 .UNSPECIFIED. ) 
 CURVE ( )  GEOMETRIC_REPRESENTATION_ITEM ( )  RATIONAL_B_SPLINE_CURVE ( ( 1.000000000000000000, 0.9792749478070963409, 0.9792749478070963409, 1.000000000000000000 ) ) 
 REPRESENTATION_ITEM ( '' )  );
#69715 = CARTESIAN_POINT ( 'NONE',  ( -19.80095844739999933, 1467.038543526389958, 210.3340861277090141 ) ) ;
#69716 = CARTESIAN_POINT ( 'NONE',  ( 0.4151546846821903003, 1512.187213306747481, 242.9330574173806951 ) ) ;
#69717 = CARTESIAN_POINT ( 'NONE',  ( -41.89974302683250329, 1440.913060410779963, 261.8273974356069971 ) ) ;
#69718 = AXIS2_PLACEMENT_3D ( 'NONE', #76046, #110190, #10350 ) ;
#69719 = CARTESIAN_POINT ( 'NONE',  ( -25.71518287839999672, 1448.115169621710038, 138.0481613422979876 ) ) ;
#69720 = CARTESIAN_POINT ( 'NONE',  ( 28.84710513917680075, 1507.919203931609900, 206.0039949767749761 ) ) ;
#69721 = CARTESIAN_POINT ( 'NONE',  ( 0.8853928803100010736, 1430.729413004489970, 199.7003955947189979 ) ) ;
#69722 = CARTESIAN_POINT ( 'NONE',  ( 10.94008111561099916, 1480.254962643290128, 209.9041328597590166 ) ) ;
#69723 = CARTESIAN_POINT ( 'NONE',  ( 2.705175745250000041, 1507.754439583389967, 220.5492045685990092 ) ) ;
#69724 = CARTESIAN_POINT ( 'NONE',  ( -38.87775330991500766, 1452.503265736994535, 269.5910503552404975 ) ) ;
#69725 = ORIENTED_EDGE ( 'NONE', *, *, #17197, .T. ) ;
#69726 = CARTESIAN_POINT ( 'NONE',  ( 19.36857742237545210, 1526.335487865669620, 185.3207153282587285 ) ) ;
#69727 = B_SPLINE_CURVE_WITH_KNOTS ( 'NONE', 5,
 ( #101861, #553, #40873, #67751, #24595, #100235, #93466, #25155, #59358 ),
 .UNSPECIFIED., .F., .F.,
 ( 6, 3, 6 ),
 ( -157.7108139780000045, -153.2961530439999933, -140.3375013407610084 ),
 .UNSPECIFIED. ) ;
#69728 = CARTESIAN_POINT ( 'NONE',  ( 0.000000000000000000, 1523.382868172864164, 209.1218459616979999 ) ) ;
#69729 = CARTESIAN_POINT ( 'NONE',  ( 9.817221195247329391, 1469.134009909099859, 205.3197251424940077 ) ) ;
#69730 = CARTESIAN_POINT ( 'NONE',  ( -0.3788211479479999810, 1416.124142285029848, 233.5244129845979728 ) ) ;
#69731 = CARTESIAN_POINT ( 'NONE',  ( 11.47878270300000025, 1502.051335001390044, 209.2507985867119942 ) ) ;
#69732 = CARTESIAN_POINT ( 'NONE',  ( -31.76119286153750920, 1522.906363951597314, 196.2959455099806121 ) ) ;
#69733 = CARTESIAN_POINT ( 'NONE',  ( 7.503281267020000200, 1424.102137712849981, 212.3377160795290024 ) ) ;
#69734 = DIRECTION ( 'NONE',  ( 0.1403901404440096035, 0.9900962622220685905, 0.000000000000000000 ) ) ;
#69735 = VECTOR ( 'NONE', #103953, 1000.000000000000000 ) ;
#69736 = CARTESIAN_POINT ( 'NONE',  ( -17.85311748929999709, 1415.140114704729967, 207.6665950678980153 ) ) ;
#69737 = CARTESIAN_POINT ( 'NONE',  ( -10.06499266109999979, 1481.481387821690078, 205.8730048975889986 ) ) ;
#69738 = CARTESIAN_POINT ( 'NONE',  ( 7.887696381483615404, 1512.266332053796077, 206.1838970189314750 ) ) ;
#69739 = CARTESIAN_POINT ( 'NONE',  ( -10.47578755381780091, 1396.278882950810157, 205.5458655290329943 ) ) ;
#69740 = ORIENTED_EDGE ( 'NONE', *, *, #53428, .T. ) ;
#69741 = CARTESIAN_POINT ( 'NONE',  ( -16.35908613486439833, 1409.492693367569927, 225.1152296089470042 ) ) ;
#69742 = CARTESIAN_POINT ( 'NONE',  ( 7.333237907140000900, 1433.447543843880112, 149.5704065546979962 ) ) ;
#69743 = ORIENTED_EDGE ( 'NONE', *, *, #103785, .T. ) ;
#69744 = ORIENTED_EDGE ( 'NONE', *, *, #106995, .T. ) ;
#69745 = CARTESIAN_POINT ( 'NONE',  ( -20.59684415639999955, 1507.762623716630060, 208.9176257130860108 ) ) ;
#69746 = CARTESIAN_POINT ( 'NONE',  ( 7.102869657934872905, 1516.552937176199521, 206.7109580197294463 ) ) ;
#69748 = CARTESIAN_POINT ( 'NONE',  ( 0.5343213467924259330, 1456.848408503409928, 219.7312664301520044 ) ) ;
#69747 = CARTESIAN_POINT ( 'NONE',  ( 10.88730574250000060, 1426.101986003629918, 91.15062687669779962 ) ) ;
#69749 = CARTESIAN_POINT ( 'NONE',  ( 3.348648543330357441, 1523.530935881284904, 176.1572159930114196 ) ) ;
#69750 = CARTESIAN_POINT ( 'NONE',  ( -11.46220264589999971, 1433.073555843209988, 151.3007702552979765 ) ) ;
#69751 = AXIS2_PLACEMENT_3D ( 'NONE', #59960, #94075, #43691 ) ;
#69752 = CARTESIAN_POINT ( 'NONE',  ( -2.866286648406546345, 1419.680164975547541, 186.1825321117389933 ) ) ;
#69753 = CARTESIAN_POINT ( 'NONE',  ( 7.724069020439999989, 1425.270033306300093, 211.8061983222289939 ) ) ;
#69754 = CARTESIAN_POINT ( 'NONE',  ( 0.9103409915569969924, 1462.760008604990162, 230.5111369474990113 ) ) ;
#69756 = CARTESIAN_POINT ( 'NONE',  ( 7.466351093540000150, 1508.652853213030085, 182.1636783160980144 ) ) ;
#69755 = B_SPLINE_CURVE_WITH_KNOTS ( 'NONE', 3,
 ( #44403, #85264, #52255, #76892, #43294, #202, #77442, #34325, #77985, #18603, #25348, #103739, #94217, #16936, #52803, #78545, #17492, #103163, #69062, #42181, #1291, #27040, #35431, #35994, #70184 ),
 .UNSPECIFIED., .F., .F.,
 ( 4, 3, 3, 3, 3, 3, 3, 3, 4 ),
 ( -14.84821972146360025, -14.69753164292139935, -14.02977699588210037, -13.36301733525779945, -12.71109731192579950, -12.40463753468570118, -11.81983018498929994, -11.09617899401849961, -10.57397516620000033 ),
 .UNSPECIFIED. ) ;
#69757 = CARTESIAN_POINT ( 'NONE',  ( 2.500000726750000180, 1448.905931065010009, 182.6097889574979831 ) ) ;
#69758 = B_SPLINE_SURFACE_WITH_KNOTS ( 'NONE', 5, 5, ( 
 ( #59325, #32450, #50369, #75570, #101264, #109703, #49261, #92891, #6685, #100197, #24563, #84495, #50907, #91243, #100727, #91786, #7785, #16705, #41951, #48713, #22909 ),
 ( #6127, #33517, #40283, #108597, #31885, #92333, #110243, #24011, #66072, #23480, #40840, #15605, #44731, #18375, #60985, #59867, #94540, #103495, #17259, #68830, #62091 ),
 ( #95110, #77219, #51450, #17814, #34646, #43060, #86155, #52570, #521, #8878, #45283, #85583, #86704, #95661, #9997, #27347, #87836, #70495, #9446, #93994, #53695 ),
 ( #104613, #18928, #102392, #52013, #61532, #69941, #27907, #1070, #102931, #44168, #36855, #43611, #77761, #11124, #53126, #96216, #78305, #1621, #25675, #87263, #35757 ),
 ( #78881, #35198, #10557, #79424, #69385, #19492, #104055, #2185, #26797, #36300, #26234, #2734, #60423, #106804, #98954, #21680, #38502, #81597, #105734, #97851, #105171 ),
 ( #37415, #48021, #54780, #20047, #30660, #71614, #12759, #106267, #13283, #55332, #90006, #13836, #96777, #29553, #55887, #21126, #29018, #3840, #82158, #71048, #54242 ) ),
 .UNSPECIFIED., .F., .F., .F.,
 ( 6, 6 ),
 ( 6, 3, 3, 3, 3, 3, 6 ),
 ( 2.177956466309999950, 27.10020543639999957 ),
 ( 27.90569345569999982, 34.29022120999999856, 36.66164856079999623, 37.84736223619999862, 39.03307591160000101, 39.85391243800000183, 40.67474896430000086 ),
 .UNSPECIFIED. ) ;
#69759 = CARTESIAN_POINT ( 'NONE',  ( 9.704582620010000937, 1366.001145740639913, 207.6218459616989946 ) ) ;
#69761 = ORIENTED_EDGE ( 'NONE', *, *, #97339, .T. ) ;
#69760 = CARTESIAN_POINT ( 'NONE',  ( 7.333575610579999626, 1455.004670275590115, 216.8632114976190053 ) ) ;
#69762 = ORIENTED_EDGE ( 'NONE', *, *, #19247, .T. ) ;
#69763 = CARTESIAN_POINT ( 'NONE',  ( -41.14066536589999856, 1444.183253557760054, 136.8991340996980171 ) ) ;
#69764 = DIRECTION ( 'NONE',  ( -0.6736849260863841948, 0.000000000000000000, 0.7390186874254148774 ) ) ;
#69765 = CARTESIAN_POINT ( 'NONE',  ( -0.9556612664140000657, 1472.040204376429983, 270.0714134045979904 ) ) ;
#69766 = LINE ( 'NONE', #1429, #101636 ) ;
#69767 = CARTESIAN_POINT ( 'NONE',  ( -0.9862637779436296270, 1410.322815402584638, 185.2948817930962662 ) ) ;
#69768 = CARTESIAN_POINT ( 'NONE',  ( -32.38114538885259464, 1523.604703353109926, 202.1233279672533172 ) ) ;
#69769 = DIRECTION ( 'NONE',  ( 9.500914144214121536E-47, -1.000000000000000000, 1.836970198721029688E-16 ) ) ;
#69770 = CARTESIAN_POINT ( 'NONE',  ( -33.93389154554730425, 1451.270658457710169, 135.9469627738999975 ) ) ;
#69771 = FILL_AREA_STYLE ('',( #26621 ) ) ;
#69772 = CARTESIAN_POINT ( 'NONE',  ( -2.500000000000000000, 1448.210448412289907, 170.5244215879980061 ) ) ;
#69773 = CARTESIAN_POINT ( 'NONE',  ( 9.271894271600004345, 1369.053083489915252, 208.3718459617010978 ) ) ;
#69774 = CARTESIAN_POINT ( 'NONE',  ( 12.31782521489999915, 1408.309306176930022, 215.8722587012880183 ) ) ;
#69775 = CARTESIAN_POINT ( 'NONE',  ( -1.532158170363220107, 1405.788062017090169, 268.4831340189729758 ) ) ;
#69776 = CARTESIAN_POINT ( 'NONE',  ( -13.71232569032570048, 1434.975555795949958, 148.7451008170540092 ) ) ;
#69777 = ORIENTED_EDGE ( 'NONE', *, *, #34575, .T. ) ;
#69778 = CARTESIAN_POINT ( 'NONE',  ( -11.86529746090000081, 1432.285507951989985, 150.3971901167980150 ) ) ;
#69779 = CARTESIAN_POINT ( 'NONE',  ( 13.52955335139999882, 1444.423027347819925, 188.5011656169979801 ) ) ;
#69780 = ORIENTED_EDGE ( 'NONE', *, *, #74301, .T. ) ;
#69781 = ORIENTED_EDGE ( 'NONE', *, *, #94287, .T. ) ;
#69782 = FACE_OUTER_BOUND ( 'NONE', #103196, .T. ) ;
#69783 = CARTESIAN_POINT ( 'NONE',  ( -9.977700672470000143, 1365.292605733890014, 207.6218459616989946 ) ) ;
#69784 = CARTESIAN_POINT ( 'NONE',  ( 4.621897824414999967, 1516.858533673840157, 213.7337256555570093 ) ) ;
#69785 = CARTESIAN_POINT ( 'NONE',  ( 3.167889818784999978, 1511.297452611750032, 216.7408386441069865 ) ) ;
#69786 = ORIENTED_EDGE ( 'NONE', *, *, #37831, .F. ) ;
#69787 = CARTESIAN_POINT ( 'NONE',  ( -62.88186284109999491, 1379.821258372850025, 270.0876510056589836 ) ) ;
#69788 = CARTESIAN_POINT ( 'NONE',  ( 11.60080558210000135, 1414.971439108430104, 222.3644924952979807 ) ) ;
#69789 = CARTESIAN_POINT ( 'NONE',  ( -4.621267922064999922, 1516.830644417779922, 204.1223895416970038 ) ) ;
#69790 = CIRCLE ( 'NONE', #62621, 1.999999999999998668 ) ;
#69791 = CARTESIAN_POINT ( 'NONE',  ( -28.52408420809999967, 1509.909458608030263, 201.9849479314579810 ) ) ;
#69792 = B_SPLINE_SURFACE_WITH_KNOTS ( 'NONE', 5, 5, ( 
 ( #68488, #69047, #41616, #109381, #60644, #6896 ),
 ( #66835, #100945, #58422, #92548, #15816, #44389 ),
 ( #19139, #3496, #1277, #61751, #54457, #103723 ),
 ( #80181, #77970, #35417, #95874, #69605, #96994 ),
 ( #35978, #86921, #27025, #62310, #62882, #104831 ),
 ( #53344, #20257, #78532, #61213, #36523, #37623 ) ),
 .UNSPECIFIED., .F., .F., .F.,
 ( 6, 6 ),
 ( 6, 6 ),
 ( 4.991132198209999871, 7.657648704760000591 ),
 ( 0.000000000000000000, 0.5000000000000000000 ),
 .UNSPECIFIED. ) ;
#69793 = CARTESIAN_POINT ( 'NONE',  ( -1.114940899219999837, 1507.624369749730022, 232.0741173169980129 ) ) ;
#69794 = CARTESIAN_POINT ( 'NONE',  ( -41.29476677764731818, 1435.144711064243438, 269.6341300601254147 ) ) ;
#69795 = CARTESIAN_POINT ( 'NONE',  ( -64.59470153520619817, 1384.702257275750071, 254.1534755538610284 ) ) ;
#69796 = CARTESIAN_POINT ( 'NONE',  ( 2.485205649205000089, 1517.181921232829836, 201.3958557702769951 ) ) ;
#69797 = CARTESIAN_POINT ( 'NONE',  ( -24.91457825792770109, 1430.518871130359912, 208.6748305930140077 ) ) ;
#69798 = AXIS2_PLACEMENT_3D ( 'NONE', #53647, #27867, #44127 ) ;
#69800 = ORIENTED_EDGE ( 'NONE', *, *, #52901, .F. ) ;
#69799 = CARTESIAN_POINT ( 'NONE',  ( -5.865704164809999455, 1445.996979593550122, 183.7573955461979835 ) ) ;
#69801 = CARTESIAN_POINT ( 'NONE',  ( 33.91369968912619726, 1451.728767897860052, 134.7155302171979940 ) ) ;
#69802 = CARTESIAN_POINT ( 'NONE',  ( -24.41186848580399982, 1440.913060429360030, 212.0284777848129920 ) ) ;
#69803 = CARTESIAN_POINT ( 'NONE',  ( 19.65495273042400370, 1477.253990450800075, 226.3277939041599893 ) ) ;
#69804 = CARTESIAN_POINT ( 'NONE',  ( -25.30535122030000039, 1436.307508284910227, 137.3140542664980046 ) ) ;
#69806 = CARTESIAN_POINT ( 'NONE',  ( -1.118353254094999860, 1516.977201124959947, 211.6155430111569729 ) ) ;
#69805 = AXIS2_PLACEMENT_3D ( 'NONE', #21326, #22422, #14039 ) ;
#69807 = CARTESIAN_POINT ( 'NONE',  ( -68.69258099389999472, 1379.747741134600119, 279.9541405716590248 ) ) ;
#69808 = B_SPLINE_CURVE_WITH_KNOTS ( 'NONE', 3,
 ( #4334, #39005, #21644, #38465, #73182, #37934, #100016, #22737, #89428, #55851, #31160, #12164, #56387, #106767, #54749, #13245, #46902, #22189, #47979, #82118, #5972, #48544, #89971, #56941, #81025, #4860, #40117, #106229, #64249, #98372, #82682, #65899, #65351, #81559, #29513, #72114, #91069, #88879, #107328, #3802, #46354, #80485, #63705, #99459, #5419, #64810 ),
 .UNSPECIFIED., .F., .F.,
 ( 4, 3, 3, 3, 3, 3, 3, 3, 3, 3, 3, 3, 3, 3, 3, 4 ),
 ( -2.000000000000000000, -1.940228845006789937, -1.806436809266960042, -1.670720477943769877, -1.533764895268459938, -1.394888271458489815, -1.254958854399230050, -1.114243059651710110, -0.9730594466478950100, -0.8263536533118798211, -0.6856755233809810335, -0.5458629076362540022, -0.4072070084870209605, -0.2699245238820009440, -0.1341607992937359217, 0.000000000000000000 ),
 .UNSPECIFIED. ) ;
#69809 = CARTESIAN_POINT ( 'NONE',  ( -14.69695073940000007, 1415.591872390730032, 226.9139971760980075 ) ) ;
#69810 = PLANE ( 'NONE',  #28868 ) ;
#69811 = CARTESIAN_POINT ( 'NONE',  ( -115.0902741230411692, 1305.913060387289988, 309.2469088860785860 ) ) ;
#69812 = CARTESIAN_POINT ( 'NONE',  ( 2.286472886424999906, 1516.883361325900069, 208.3638615500849767 ) ) ;
#69813 = VERTEX_POINT ( 'NONE', #6056 ) ;
#69814 = CARTESIAN_POINT ( 'NONE',  ( 2.500000000000000000, 1439.002693873140061, 157.7215435580980056 ) ) ;
#69815 = CARTESIAN_POINT ( 'NONE',  ( -3.621823104480000222, 1410.301613452430047, 232.3323923370979855 ) ) ;
#69816 = CARTESIAN_POINT ( 'NONE',  ( -36.12389091449999512, 1385.203813137380166, 235.4649545851590062 ) ) ;
#69817 = EDGE_LOOP ( 'NONE', ( #54577, #24078, #34708, #38619, #7499, #76207, #66377 ) ) ;
#69818 = CARTESIAN_POINT ( 'NONE',  ( -13.54997464361210113, 1385.299760518590119, 219.1450828324119868 ) ) ;
#69819 = DIRECTION ( 'NONE',  ( 0.000000000000000000, -1.000000000000000000, 0.000000000000000000 ) ) ;
#69820 = CARTESIAN_POINT ( 'NONE',  ( 12.11419479737319804, 1434.101768081229920, 150.3426090226449787 ) ) ;
#69821 = CARTESIAN_POINT ( 'NONE',  ( 15.93672166378249777, 1469.005798317469953, 229.8246201197470100 ) ) ;
#69822 = CARTESIAN_POINT ( 'NONE',  ( -23.28153440269690222, 1507.876989814209992, 223.8845409149209900 ) ) ;
#69823 = CARTESIAN_POINT ( 'NONE',  ( -1.984533605359999564, 1410.356878505129998, 186.2308698998980105 ) ) ;
#69824 = CARTESIAN_POINT ( 'NONE',  ( 0.1600673621120000112, 1410.295025425230051, 233.2191648330980058 ) ) ;
#69825 = CARTESIAN_POINT ( 'NONE',  ( -13.58268883541719951, 1416.851343898680170, 221.9096085506480165 ) ) ;
#69826 = EDGE_CURVE ( 'NONE', #8681, #41836, #70693, .T. ) ;
#69828 = CARTESIAN_POINT ( 'NONE',  ( -4.363122371700000279, 1421.971318377230091, 184.5104922129979741 ) ) ;
#69827 = CARTESIAN_POINT ( 'NONE',  ( 1.710004548794999968, 1516.557392317769882, 215.6678473207969944 ) ) ;
#69829 = CARTESIAN_POINT ( 'NONE',  ( 19.21159273369999809, 1509.355098208629897, 187.6258791606980196 ) ) ;
#69830 = CARTESIAN_POINT ( 'NONE',  ( -0.7403206051589980019, 1517.139320148880188, 216.8467205834170102 ) ) ;
#69831 = VERTEX_POINT ( 'NONE', #23935 ) ;
#69832 = CARTESIAN_POINT ( 'NONE',  ( -12.18581614772419996, 1415.088012641449950, 197.3189512858170076 ) ) ;
#69833 = DIRECTION ( 'NONE',  ( 0.000000000000000000, 0.07593562622321022026, -0.9971127221483482295 ) ) ;
#69834 = VERTEX_POINT ( 'NONE', #50289 ) ;
#69835 = CARTESIAN_POINT ( 'NONE',  ( 0.2612772751870610088, 1416.851343895820037, 190.7759414009450154 ) ) ;
#69836 = CARTESIAN_POINT ( 'NONE',  ( 9.833393186232900263, 1522.051704408389924, 205.7359371553449989 ) ) ;
#69837 = CARTESIAN_POINT ( 'NONE',  ( 4.814474515349520090, 1424.592626270299888, 191.7967880341639955 ) ) ;
#69838 = CARTESIAN_POINT ( 'NONE',  ( -33.23421991949620491, 1522.906363951597314, 200.8294566360699491 ) ) ;
#69839 = B_SPLINE_CURVE_WITH_KNOTS ( 'NONE', 3,
 ( #31275, #97377, #40228, #74411, #20649, #54851 ),
 .UNSPECIFIED., .F., .F.,
 ( 4, 2, 4 ),
 ( -0.1904887807602000105, -0.09529849760486289179, -1.010125272010720110E-06 ),
 .UNSPECIFIED. ) ;
#69840 = CIRCLE ( 'NONE', #12587, 6.500000000000000000 ) ;
#69841 = CARTESIAN_POINT ( 'NONE',  ( 17.83233393729999960, 1415.128105759529944, 210.4741431536880043 ) ) ;
#69842 = CARTESIAN_POINT ( 'NONE',  ( -18.78018960140000360, 1425.453421275130040, 226.8344281414980230 ) ) ;
#69843 = CARTESIAN_POINT ( 'NONE',  ( -21.31715047099999794, 1436.055628343680155, 143.9063927194979726 ) ) ;
#69844 = CARTESIAN_POINT ( 'NONE',  ( -11.97724519069999971, 1441.600846913620217, 147.6096801420980000 ) ) ;
#69845 = DIRECTION ( 'NONE',  ( -5.980589973904019347E-17, 1.000000000000000000, -1.736889445713099699E-16 ) ) ;
#69847 = CARTESIAN_POINT ( 'NONE',  ( -5.007591594161714177, 1391.741091803201698, 203.5445219108341632 ) ) ;
#69846 = CARTESIAN_POINT ( 'NONE',  ( 5.823572337359999906, 1487.975078907890065, 198.5964445195989754 ) ) ;
#69848 = CARTESIAN_POINT ( 'NONE',  ( 11.81532904971749254, 1433.677431381189763, 150.7649965429154406 ) ) ;
#69849 = ORIENTED_EDGE ( 'NONE', *, *, #1753, .T. ) ;
#69850 = CARTESIAN_POINT ( 'NONE',  ( 12.91878488757420129, 1430.070686061380002, 195.6857951094069961 ) ) ;
#69851 = CARTESIAN_POINT ( 'NONE',  ( -4.679791067032079255, 1508.610720099250102, 212.2979123687669869 ) ) ;
#69852 = CARTESIAN_POINT ( 'NONE',  ( -11.90002773584334683, 1434.916176828660127, 147.6452132258590382 ) ) ;
#69853 = CARTESIAN_POINT ( 'NONE',  ( 13.86092937120069912, 1410.765486813650114, 191.1266627561969926 ) ) ;
#69854 = FACE_OUTER_BOUND ( 'NONE', #62545, .T. ) ;
#69855 = CARTESIAN_POINT ( 'NONE',  ( 29.36670733772781361, 1526.000688113810384, 220.9053709889059576 ) ) ;
#69856 = CARTESIAN_POINT ( 'NONE',  ( 1.925297169133120212, 1521.951704408389787, 230.6853930764029883 ) ) ;
#69857 = CARTESIAN_POINT ( 'NONE',  ( -10.27696724499340064, 1491.210326720090052, 213.0881471566560208 ) ) ;
#69858 = CARTESIAN_POINT ( 'NONE',  ( 13.40958072579999971, 1414.996442553730049, 197.9133052342980079 ) ) ;
#69859 = CARTESIAN_POINT ( 'NONE',  ( -99.18220428064979899, 1383.764529278820191, 310.5488099629289991 ) ) ;
#69860 = EDGE_CURVE ( 'NONE', #91513, #85568, #7703, .T. ) ;
#69861 = ADVANCED_FACE ( 'NONE', ( #108515 ), #43511, .F. ) ;
#69862 = CARTESIAN_POINT ( 'NONE',  ( -7.628773448420000491, 1416.913060387330006, 216.7506196533379921 ) ) ;
#69863 = PLANE ( 'NONE',  #82189 ) ;
#69864 = CARTESIAN_POINT ( 'NONE',  ( -2.431784208376569723, 1516.533929790709863, 201.4128240233619920 ) ) ;
#69866 = VERTEX_POINT ( 'NONE', #35666 ) ;
#69865 = CARTESIAN_POINT ( 'NONE',  ( 22.98967036120000174, 1508.444085606630097, 193.7320087538980147 ) ) ;
#69867 = CARTESIAN_POINT ( 'NONE',  ( -1.547463840030000037, 1414.913060387329779, 225.9340782259980074 ) ) ;
#69868 = AXIS2_PLACEMENT_3D ( 'NONE', #52407, #79258, #86532 ) ;
#69869 = CARTESIAN_POINT ( 'NONE',  ( -75.43085291519999203, 1383.276795896440035, 276.7272104215589934 ) ) ;
#69870 = EDGE_CURVE ( 'NONE', #41661, #75670, #51342, .T. ) ;
#69871 = CARTESIAN_POINT ( 'NONE',  ( -14.81767606095329981, 1417.858166622450199, 213.3262279172620026 ) ) ;
#69872 = ORIENTED_EDGE ( 'NONE', *, *, #55761, .F. ) ;
#69873 = ORIENTED_EDGE ( 'NONE', *, *, #9305, .T. ) ;
#69874 = CARTESIAN_POINT ( 'NONE',  ( 33.91369120165509798, 1451.728768194249824, 134.0999999980979851 ) ) ;
#69875 = DIRECTION ( 'NONE',  ( 0.000000000000000000, 1.000000000000000000, 0.000000000000000000 ) ) ;
#69876 = CARTESIAN_POINT ( 'NONE',  ( 40.26850195192459836, 1443.374941825310088, 137.0885199844659894 ) ) ;
#69878 = CARTESIAN_POINT ( 'NONE',  ( -18.32011812489999869, 1469.450906033330057, 259.8063372729980074 ) ) ;
#69877 = CARTESIAN_POINT ( 'NONE',  ( 21.25073931209999856, 1488.812149332829904, 209.0329839582499858 ) ) ;
#69879 = FACE_OUTER_BOUND ( 'NONE', #101388, .T. ) ;
#69880 = CARTESIAN_POINT ( 'NONE',  ( -107.5397600339999968, 1382.037659314800067, 298.2264582646590725 ) ) ;
#69881 = CARTESIAN_POINT ( 'NONE',  ( 24.93047652359999944, 1508.532778672029963, 197.8716724273980105 ) ) ;
#69882 = CARTESIAN_POINT ( 'NONE',  ( -20.45667992530000134, 1485.851243504329886, 191.2933074961979969 ) ) ;
#69883 = CARTESIAN_POINT ( 'NONE',  ( 2.104012799200000394, 1408.986534133630130, 186.4985688927979766 ) ) ;
#69884 = CARTESIAN_POINT ( 'NONE',  ( 6.313072733930000346, 1422.316561012229840, 186.3238498068980107 ) ) ;
#69885 = CARTESIAN_POINT ( 'NONE',  ( -11.83477905770000049, 1434.684743416989932, 151.1661213938980097 ) ) ;
#69886 = CARTESIAN_POINT ( 'NONE',  ( -9.147922398094991081, 1449.650533038000049, 209.9742684363969829 ) ) ;
#69887 = CARTESIAN_POINT ( 'NONE',  ( -10.30332664446770075, 1423.841252421040053, 204.4542459073049940 ) ) ;
#69888 = AXIS2_PLACEMENT_3D ( 'NONE', #22612, #82570, #48428 ) ;
#69889 = CARTESIAN_POINT ( 'NONE',  ( 3.351006924987864455, 1524.082582765195411, 242.0157322279995071 ) ) ;
#69890 = CARTESIAN_POINT ( 'NONE',  ( 2.125574643609999814, 1472.895346367389948, 219.1091941688290206 ) ) ;
#69891 = ORIENTED_EDGE ( 'NONE', *, *, #54816, .T. ) ;
#69892 = CARTESIAN_POINT ( 'NONE',  ( -2.393268998928310687, 1426.806556743500096, 139.9374969045731518 ) ) ;
#69893 = CARTESIAN_POINT ( 'NONE',  ( 22.18328064218600204, 1474.773901063470021, 209.9706487204360030 ) ) ;
#69895 = ADVANCED_FACE ( 'NONE', ( #69854 ), #39215, .T. ) ;
#69894 = CARTESIAN_POINT ( 'NONE',  ( -40.64494809139999631, 1449.406402974629827, 269.6215796247980165 ) ) ;
#69896 = DIRECTION ( 'NONE',  ( -0.9702683578407158560, 7.674209871302701496E-33, 0.2420316379589265432 ) ) ;
#69897 = CARTESIAN_POINT ( 'NONE',  ( 1.110223024629999949E-15, 1434.541756592460160, 155.4759165859979930 ) ) ;
#69898 = B_SPLINE_CURVE_WITH_KNOTS ( 'NONE', 3,
 ( #71116, #37482, #2803, #61598, #10631, #18439, #45899, #52639, #71685, #44238 ),
 .UNSPECIFIED., .F., .F.,
 ( 4, 2, 2, 2, 4 ),
 ( 0.000000000000000000, 0.2500000000000000000, 0.5000000000000000000, 0.7500000000000000000, 1.000000000000000000 ),
 .UNSPECIFIED. ) ;
#69899 = DIRECTION ( 'NONE',  ( -0.9455185755993178454, 0.000000000000000000, 0.3255681544571537578 ) ) ;
#69900 = CARTESIAN_POINT ( 'NONE',  ( -20.59725329420000151, 1484.571939645490147, 210.1086304389179986 ) ) ;
#69901 = DIRECTION ( 'NONE',  ( 0.000000000000000000, 0.000000000000000000, 1.000000000000000000 ) ) ;
#69902 = CARTESIAN_POINT ( 'NONE',  ( -3.349453590340000009, 1417.674249932829980, 234.8202870076979991 ) ) ;
#69903 = EDGE_CURVE ( 'NONE', #93900, #22042, #59342, .T. ) ;
#69904 = VECTOR ( 'NONE', #19728, 999.9999999999998863 ) ;
#69905 = CARTESIAN_POINT ( 'NONE',  ( -1.258566612072725688, 1484.609298652428606, 182.2899128876086081 ) ) ;
#69906 = CARTESIAN_POINT ( 'NONE',  ( -7.173827098674079750, 1361.757975858879945, 210.6218459616991936 ) ) ;
#69907 = CARTESIAN_POINT ( 'NONE',  ( -45.72953638603589610, 1436.732522043369954, 266.6874787479000020 ) ) ;
#69908 = DIRECTION ( 'NONE',  ( 0.000000000000000000, -1.000000000000000000, -0.000000000000000000 ) ) ;
#69909 = ORIENTED_EDGE ( 'NONE', *, *, #88612, .F. ) ;
#69910 = CARTESIAN_POINT ( 'NONE',  ( 23.84671661830000033, 1435.330256084430175, 136.8235927701979904 ) ) ;
#69911 = EDGE_CURVE ( 'NONE', #76345, #28393, #53042, .T. ) ;
#69912 = VERTEX_POINT ( 'NONE', #61452 ) ;
#69913 = CARTESIAN_POINT ( 'NONE',  ( 4.044319887224999910, 1517.073005577650065, 210.2423896678870108 ) ) ;
#69914 = TOROIDAL_SURFACE ( 'NONE', #75249, 24.00000000000000000, 1.000000000000000000 ) ;
#69915 = CARTESIAN_POINT ( 'NONE',  ( -9.041223454946500482, 1447.413830056329971, 212.1276203665690048 ) ) ;
#69916 = CARTESIAN_POINT ( 'NONE',  ( -6.777304992429280084, 1470.983459794990495, 216.6342898665807297 ) ) ;
#69917 = CARTESIAN_POINT ( 'NONE',  ( -16.34177352999999755, 1410.409901485429828, 191.5622047604979912 ) ) ;
#69918 = CARTESIAN_POINT ( 'NONE',  ( -2.842752294796690116, 1497.021273686229961, 221.1752333403379964 ) ) ;
#69919 = VERTEX_POINT ( 'NONE', #95027 ) ;
#69920 = CARTESIAN_POINT ( 'NONE',  ( 22.57734580500000021, 1433.084083961730130, 213.0699815576180072 ) ) ;
#69922 = CARTESIAN_POINT ( 'NONE',  ( 13.57457166070000021, 1434.814457747740107, 195.7795090784979948 ) ) ;
#69921 = DIRECTION ( 'NONE',  ( 0.8672669759446700599, 0.000000000000000000, 0.4978433412588614271 ) ) ;
#69923 = CARTESIAN_POINT ( 'NONE',  ( 3.959152859930000101, 1428.396642669490120, 216.3690266601789745 ) ) ;
#69924 = CIRCLE ( 'NONE', #66399, 2.000006071546453157 ) ;
#69925 = CARTESIAN_POINT ( 'NONE',  ( -17.26078256985329773, 1508.541932187329849, 212.5336323307500095 ) ) ;
#69926 = DIRECTION ( 'NONE',  ( -1.755985294532469921E-16, 1.000000000000000000, -1.338183447452831989E-16 ) ) ;
#69927 = CARTESIAN_POINT ( 'NONE',  ( -8.769340852563940913, 1438.886933218489958, 207.8278986470189977 ) ) ;
#69928 = VERTEX_POINT ( 'NONE', #18297 ) ;
#69929 = CARTESIAN_POINT ( 'NONE',  ( -1.875969534053839816, 1407.674994227130128, 270.1370502786999737 ) ) ;
#69930 = CARTESIAN_POINT ( 'NONE',  ( 4.612671339784999880, 1516.783665406140017, 208.3654117178780041 ) ) ;
#69931 = CARTESIAN_POINT ( 'NONE',  ( 7.876066647220000938, 1417.703921191229938, 230.9570592481979929 ) ) ;
#69932 = CARTESIAN_POINT ( 'NONE',  ( -7.460636202991704380, 1509.035273820330531, 215.1586052621513545 ) ) ;
#69934 = ORIENTED_EDGE ( 'NONE', *, *, #109828, .F. ) ;
#69933 = CARTESIAN_POINT ( 'NONE',  ( -8.232155009519999567, 1367.485244382299925, 207.6218459616989946 ) ) ;
#69935 = VERTEX_POINT ( 'NONE', #52490 ) ;
#69936 = CARTESIAN_POINT ( 'NONE',  ( 13.40958089240390017, 1414.996442620800053, 197.9133050684260127 ) ) ;
#69937 = CARTESIAN_POINT ( 'NONE',  ( -0.003606333971295369849, 1409.082051554400095, 185.5805092309179827 ) ) ;
#69938 = CARTESIAN_POINT ( 'NONE',  ( 3.664318114120971970, 1425.064796927145153, 184.9869177022372639 ) ) ;
#69939 = CARTESIAN_POINT ( 'NONE',  ( -3.448830483803561719, 1523.382868172864164, 175.1594891075192209 ) ) ;
#69940 = CARTESIAN_POINT ( 'NONE',  ( -18.51001488987260046, 1427.198549858980186, 194.7363669604100096 ) ) ;
#69941 = CARTESIAN_POINT ( 'NONE',  ( -20.83663208060000116, 1425.807880000829982, 220.5952949419979916 ) ) ;
#69942 = CARTESIAN_POINT ( 'NONE',  ( 28.54163408408160052, 1468.582989030339832, 267.1922970806700732 ) ) ;
#69943 = CARTESIAN_POINT ( 'NONE',  ( -11.39275159694039985, 1391.913060387289988, 207.2216192889670197 ) ) ;
#69944 = CARTESIAN_POINT ( 'NONE',  ( 3.887502411549999870, 1447.985170383209834, 184.3007615236979859 ) ) ;
#69945 = CARTESIAN_POINT ( 'NONE',  ( 7.709681268295000223, 1516.559109716219837, 206.2491454149069909 ) ) ;
#69946 = ORIENTED_EDGE ( 'NONE', *, *, #97295, .F. ) ;
#69947 = CARTESIAN_POINT ( 'NONE',  ( -13.62133678120479985, 1452.879579795280051, 223.2680741433150047 ) ) ;
#69948 = CARTESIAN_POINT ( 'NONE',  ( -4.327793213831197860, 1516.734711358231152, 202.9907106567216601 ) ) ;
#69949 = CARTESIAN_POINT ( 'NONE',  ( 22.86785504970000105, 1409.720132996430038, 208.8870272755499968 ) ) ;
#69950 = EDGE_LOOP ( 'NONE', ( #18272, #2056, #5725, #12329 ) ) ;
#69951 = CARTESIAN_POINT ( 'NONE',  ( 3.892696960845567045, 1515.551704300027950, 207.5713754906064707 ) ) ;
#69952 = CARTESIAN_POINT ( 'NONE',  ( 26.21289084844420003, 1451.932721288379980, 135.4906490382789741 ) ) ;
#69953 = CARTESIAN_POINT ( 'NONE',  ( -14.77824381598609982, 1473.184986518139794, 194.8749861038550080 ) ) ;
#69954 = CARTESIAN_POINT ( 'NONE',  ( -8.976689669389999793, 1389.857300751820048, 214.6605541070490233 ) ) ;
#69955 = CARTESIAN_POINT ( 'NONE',  ( -33.35590117750204087, 1523.678648413191695, 201.9126545693505648 ) ) ;
#69956 = CARTESIAN_POINT ( 'NONE',  ( 17.56784546119999746, 1409.526543069129957, 195.5982376816980093 ) ) ;
#69957 = CARTESIAN_POINT ( 'NONE',  ( -3.786785403780000170, 1495.627531097190058, 197.8060809205989869 ) ) ;
#69958 = CARTESIAN_POINT ( 'NONE',  ( 2.500000000000039968, 1439.615672328189930, 182.7715275322960053 ) ) ;
#69960 = CARTESIAN_POINT ( 'NONE',  ( -18.77412637462996159, 1424.630488750686936, 224.5960567574681193 ) ) ;
#69959 = CARTESIAN_POINT ( 'NONE',  ( 0.2946311075390000145, 1417.347637901529879, 235.5671102051979915 ) ) ;
#69961 = CARTESIAN_POINT ( 'NONE',  ( 0.7128917335112240350, 1452.003216656849872, 183.1721099556629895 ) ) ;
#69962 = EDGE_CURVE ( 'NONE', #68439, #50075, #44665, .T. ) ;
#69963 = CARTESIAN_POINT ( 'NONE',  ( -0.2751659207381170202, 1506.798305148240161, 231.4088083080649767 ) ) ;
#69964 = CARTESIAN_POINT ( 'NONE',  ( -9.153278953699999221, 1381.244387431579980, 217.5834349994690058 ) ) ;
#69965 = ADVANCED_FACE ( 'NONE', ( #105651 ), #77845, .F. ) ;
#69966 = CARTESIAN_POINT ( 'NONE',  ( 4.039897278065000208, 1516.787536375099990, 214.1203611275269907 ) ) ;
#69967 = CARTESIAN_POINT ( 'NONE',  ( 2.494564929293782818, 1524.201670966335769, 242.7027287329880210 ) ) ;
#69968 = ORIENTED_EDGE ( 'NONE', *, *, #100788, .F. ) ;
#69969 = DIRECTION ( 'NONE',  ( 0.9786619618251627406, 0.000000000000000000, 0.2054769195713317953 ) ) ;
#69970 = CARTESIAN_POINT ( 'NONE',  ( 20.60985939166236491, 1525.581535527370988, 236.5072125268897025 ) ) ;
#69971 = CARTESIAN_POINT ( 'NONE',  ( -8.270734047218098794, 1484.136534094920080, 200.5535876571919971 ) ) ;
#69972 = DIRECTION ( 'NONE',  ( -0.8090169943749419001, 0.000000000000000000, 0.5877852522924809087 ) ) ;
#69973 = CARTESIAN_POINT ( 'NONE',  ( 12.50011566148209852, 1426.394375987810236, 202.7337349580159866 ) ) ;
#69974 = AXIS2_PLACEMENT_3D ( 'NONE', #44130, #86664, #78265 ) ;
#69975 = CARTESIAN_POINT ( 'NONE',  ( -4.327012391429009952, 1515.157834657069998, 208.9940569023019918 ) ) ;
#69976 = CARTESIAN_POINT ( 'NONE',  ( -28.02005515429999960, 1444.132106999520147, 248.0989693021979861 ) ) ;
#69977 = EDGE_CURVE ( 'NONE', #25667, #70841, #82082, .T. ) ;
#69978 = CARTESIAN_POINT ( 'NONE',  ( 45.67177335919998171, 1441.839097175249435, 266.1885934058977909 ) ) ;
#69979 = CARTESIAN_POINT ( 'NONE',  ( 11.06154325740000033, 1433.015924775339954, 151.7088343760979967 ) ) ;
#69980 = CARTESIAN_POINT ( 'NONE',  ( 4.290289619920000241, 1461.407663422529822, 243.9198229428980085 ) ) ;
#69981 = CARTESIAN_POINT ( 'NONE',  ( 27.02044944551220240, 1440.913060390540068, 226.9243301018659906 ) ) ;
#69982 = CARTESIAN_POINT ( 'NONE',  ( -16.83566772702310033, 1418.884435451930131, 201.2565165529269962 ) ) ;
#69983 = CARTESIAN_POINT ( 'NONE',  ( 0.000000000000000000, 1414.421228241719973, 209.1218459616989946 ) ) ;
#69984 = CARTESIAN_POINT ( 'NONE',  ( 14.22937790979999839, 1463.546440309030004, 223.7319135734979909 ) ) ;
#69985 = CARTESIAN_POINT ( 'NONE',  ( -4.642927288299999233, 1485.993600593529891, 182.3621085484980142 ) ) ;
#69986 =( REPRESENTATION_RELATIONSHIP ('NONE','NONE', #14372, #22211 ) REPRESENTATION_RELATIONSHIP_WITH_TRANSFORMATION ( #16823 )SHAPE_REPRESENTATION_RELATIONSHIP( ) );
#69987 = CIRCLE ( 'NONE', #3815, 1.999999999999982458 ) ;
#69988 = CARTESIAN_POINT ( 'NONE',  ( -0.9161335898489990637, 1443.103187093389806, 200.2678566797989959 ) ) ;
#69989 = CARTESIAN_POINT ( 'NONE',  ( -28.86589449839050303, 1509.921079635449814, 200.7492878960630094 ) ) ;
#69990 = EDGE_CURVE ( 'NONE', #49802, #29937, #11029, .T. ) ;
#69991 = CARTESIAN_POINT ( 'NONE',  ( 25.67898337129999931, 1449.805023455629907, 209.8444692255790187 ) ) ;
#69992 = CARTESIAN_POINT ( 'NONE',  ( -16.98954224973644145, 1419.974429067340452, 207.7469223126931297 ) ) ;
#69993 = CARTESIAN_POINT ( 'NONE',  ( -38.70772189830101695, 1437.296230298083174, 135.0862444309819921 ) ) ;
#69994 = CARTESIAN_POINT ( 'NONE',  ( -25.46281358831500086, 1383.847540614680156, 223.8241380845890092 ) ) ;
#69995 = EDGE_CURVE ( 'NONE', #61056, #39980, #104732, .T. ) ;
#69996 = CARTESIAN_POINT ( 'NONE',  ( 9.738317455238711062, 1493.400073354660208, 188.2659979897460119 ) ) ;
#69997 = CARTESIAN_POINT ( 'NONE',  ( -7.323974644434999348, 1516.647924054489977, 213.1579656147470132 ) ) ;
#69998 = CARTESIAN_POINT ( 'NONE',  ( 9.176228414599330918, 1450.984694443030094, 210.2421773183669984 ) ) ;
#69999 = EDGE_CURVE ( 'NONE', #107054, #100575, #13876, .T. ) ;
#70001 = EDGE_LOOP ( 'NONE', ( #53255, #39166, #50899, #63196 ) ) ;
#70000 = CARTESIAN_POINT ( 'NONE',  ( 5.246794622849999534, 1436.700339732089788, 207.6218553049789932 ) ) ;
#70002 = CARTESIAN_POINT ( 'NONE',  ( 16.11867488194040732, 1414.913060387329779, 209.5777220539784480 ) ) ;
#70003 = AXIS2_PLACEMENT_3D ( 'NONE', #47492, #107380, #64863 ) ;
#70004 = CARTESIAN_POINT ( 'NONE',  ( -9.920431381559678741, 1389.497472067758736, 201.7143931154362235 ) ) ;
#70005 = CARTESIAN_POINT ( 'NONE',  ( -4.352858573179999802, 1475.884254538489813, 199.7486192038290085 ) ) ;
#70007 = ORIENTED_EDGE ( 'NONE', *, *, #95289, .F. ) ;
#70006 = CARTESIAN_POINT ( 'NONE',  ( -36.91977620350599665, 1451.033275236189866, 134.0999999987079718 ) ) ;
#70008 = CARTESIAN_POINT ( 'NONE',  ( -7.055342795364590636, 1508.551704404470001, 219.1733338826510078 ) ) ;
#70009 = EDGE_LOOP ( 'NONE', ( #103015, #103001, #1390, #62760, #26663 ) ) ;
#70010 = AXIS2_PLACEMENT_3D ( 'NONE', #110154, #49166, #16608 ) ;
#70011 = CARTESIAN_POINT ( 'NONE',  ( -14.38501648843540082, 1380.276608459779936, 209.4261068465210087 ) ) ;
#70012 = CARTESIAN_POINT ( 'NONE',  ( -15.47006972390000001, 1415.932617990029939, 219.1087698475380137 ) ) ;
#70013 = DIRECTION ( 'NONE',  ( -0.2720708970484284062, 0.6839977328998089190, -0.6768489701308448847 ) ) ;
#70015 = EDGE_CURVE ( 'NONE', #46489, #98890, #80751, .T. ) ;
#70014 = CARTESIAN_POINT ( 'NONE',  ( -2.850903925664035832, 1367.902980992500716, 209.8767901781862690 ) ) ;
#70016 = CARTESIAN_POINT ( 'NONE',  ( 0.9870939535439990919, 1430.542140937089926, 217.5404060487589959 ) ) ;
#70017 = FACE_OUTER_BOUND ( 'NONE', #102470, .T. ) ;
#70018 = CARTESIAN_POINT ( 'NONE',  ( 12.67571009042330132, 1409.355705931530110, 217.0370738725129911 ) ) ;
#70019 = CARTESIAN_POINT ( 'NONE',  ( -12.25663671779999930, 1391.732016969049937, 208.2029345092809933 ) ) ;
#70020 = CARTESIAN_POINT ( 'NONE',  ( -87.98538269667260181, 1385.186294664909838, 291.2263267895870058 ) ) ;
#70021 = CARTESIAN_POINT ( 'NONE',  ( -17.81762806769999941, 1417.741547129829996, 192.8330553043980160 ) ) ;
#70022 = CARTESIAN_POINT ( 'NONE',  ( 11.34606461758039941, 1422.095439081570021, 210.1857495716350002 ) ) ;
#70023 = ORIENTED_EDGE ( 'NONE', *, *, #6434, .T. ) ;
#70024 = VECTOR ( 'NONE', #432, 1000.000000000000114 ) ;
#70025 = EDGE_CURVE ( 'NONE', #22340, #4524, #79362, .T. ) ;
#70026 = CARTESIAN_POINT ( 'NONE',  ( 11.62672742097220002, 1491.248664925870116, 206.9181316795630039 ) ) ;
#70028 = ORIENTED_EDGE ( 'NONE', *, *, #31840, .F. ) ;
#70027 = CARTESIAN_POINT ( 'NONE',  ( -1.556099498820364024, 1414.941240534605186, 226.3359606419509760 ) ) ;
#70029 = CARTESIAN_POINT ( 'NONE',  ( 8.495474403110010897, 1465.434214291670060, 214.1564210924720157 ) ) ;
#70030 = VERTEX_POINT ( 'NONE', #31672 ) ;
#70031 =( BOUNDED_CURVE ( )  B_SPLINE_CURVE ( 3, ( #6606, #73830, #31803, #107404 ),
 .UNSPECIFIED., .F., .F. ) 
 B_SPLINE_CURVE_WITH_KNOTS ( ( 4, 4 ),
 ( 6.031750335428980314, 6.430153915118459906 ),
 .UNSPECIFIED. ) 
 CURVE ( )  GEOMETRIC_REPRESENTATION_ITEM ( )  RATIONAL_B_SPLINE_CURVE ( ( 1.000000000000000000, 0.9868165636548378306, 0.9868165636548378306, 1.000000000000000000 ) ) 
 REPRESENTATION_ITEM ( '' )  );
#70032 = CARTESIAN_POINT ( 'NONE',  ( 26.37683526749999885, 1508.582706265930028, 216.7137036938680126 ) ) ;
#70033 = CARTESIAN_POINT ( 'NONE',  ( -7.674634134560755605, 1364.272616766665806, 208.3718459617061285 ) ) ;
#70034 = CARTESIAN_POINT ( 'NONE',  ( -0.3263949288959780426, 1496.478667861620124, 196.7673131782539997 ) ) ;
#70035 = CARTESIAN_POINT ( 'NONE',  ( 17.16188218510789909, 1468.758169019195520, 269.3744713492412188 ) ) ;
#70036 = CARTESIAN_POINT ( 'NONE',  ( -30.29630067237475188, 1526.329757971584741, 221.7900933993811066 ) ) ;
#70037 = CARTESIAN_POINT ( 'NONE',  ( 3.841758412219999475, 1398.027797085529983, 221.6465661679980030 ) ) ;
#70038 = CARTESIAN_POINT ( 'NONE',  ( 32.32092748916883096, 1524.075132568165600, 202.1437887561546347 ) ) ;
#70039 = CARTESIAN_POINT ( 'NONE',  ( 0.000000000000000000, 1526.382868172863937, 209.1218459616979999 ) ) ;
#70040 = CARTESIAN_POINT ( 'NONE',  ( -1.443364724160000057, 1457.295863107529840, 183.6403006915980143 ) ) ;
#70041 = CARTESIAN_POINT ( 'NONE',  ( -4.120923335396738274, 1371.066854469031114, 209.6218459617033432 ) ) ;
#70042 = CARTESIAN_POINT ( 'NONE',  ( -8.680963252626170856, 1511.446089069276695, 214.5904756146348689 ) ) ;
#70043 = EDGE_CURVE ( 'NONE', #35617, #56560, #8532, .T. ) ;
#70044 = CARTESIAN_POINT ( 'NONE',  ( 3.439931081351653042, 1448.290196154458272, 184.1542931849176910 ) ) ;
#70045 = CARTESIAN_POINT ( 'NONE',  ( -0.01319654689839849966, 1516.941178807709775, 206.8296289214069930 ) ) ;
#70046 = CARTESIAN_POINT ( 'NONE',  ( -13.01309165946850044, 1435.753263066840191, 150.6599531705490165 ) ) ;
#70047 = EDGE_CURVE ( 'NONE', #87539, #1077, #85736, .T. ) ;
#70048 = CARTESIAN_POINT ( 'NONE',  ( -7.228663065755881689, 1511.163060387329779, 183.1074954935087646 ) ) ;
#70049 = CARTESIAN_POINT ( 'NONE',  ( 13.79555441699999996, 1416.822694190629818, 196.3351662185980047 ) ) ;
#70051 = ORIENTED_EDGE ( 'NONE', *, *, #81129, .T. ) ;
#70050 = CARTESIAN_POINT ( 'NONE',  ( -3.148245054199999782, 1496.969444965490084, 220.6920657697990009 ) ) ;
#70052 = CARTESIAN_POINT ( 'NONE',  ( 40.43746183755959578, 1444.189944152170028, 137.0849278640690159 ) ) ;
#70053 = ORIENTED_EDGE ( 'NONE', *, *, #63708, .F. ) ;
#70054 = CARTESIAN_POINT ( 'NONE',  ( 8.537822598675001373, 1517.051704408389924, 212.5465662711270056 ) ) ;
#70055 = CARTESIAN_POINT ( 'NONE',  ( -27.33420534970000304, 1488.691127167430068, 208.3487218773969971 ) ) ;
#70057 = CARTESIAN_POINT ( 'NONE',  ( 16.19082947937390315, 1409.478451820400096, 193.2334330245300009 ) ) ;
#70056 = CARTESIAN_POINT ( 'NONE',  ( -10.55446544952580012, 1425.080811231209964, 127.8430071859979762 ) ) ;
#70058 = CARTESIAN_POINT ( 'NONE',  ( -7.322105105754999954, 1516.572193931679976, 211.9951753309869957 ) ) ;
#70059 = AXIS2_PLACEMENT_3D ( 'NONE', #82160, #13838, #5459 ) ;
#70060 = CARTESIAN_POINT ( 'NONE',  ( 32.28466283162156714, 1522.382868172863937, 219.1752493337713190 ) ) ;
#70061 = CARTESIAN_POINT ( 'NONE',  ( -12.45246057309999976, 1410.452083772230026, 259.9009997819980526 ) ) ;
#70062 = CARTESIAN_POINT ( 'NONE',  ( 18.83404400785749999, 1509.591035207039795, 231.9679584295540167 ) ) ;
#70063 = CARTESIAN_POINT ( 'NONE',  ( 28.25550469550829646, 1508.223393718089937, 209.3894320226199852 ) ) ;
#70064 = CARTESIAN_POINT ( 'NONE',  ( -4.992349863779999453, 1391.620913471789891, 214.4932724168290008 ) ) ;
#70065 = CARTESIAN_POINT ( 'NONE',  ( 32.74960465840000268, 1450.908762451789926, 136.2057699161979940 ) ) ;
#70066 = ORIENTED_EDGE ( 'NONE', *, *, #46601, .F. ) ;
#70067 = CARTESIAN_POINT ( 'NONE',  ( 6.170308677738740144, 1397.182086642849981, 220.3579607364119681 ) ) ;
#70068 = CARTESIAN_POINT ( 'NONE',  ( 10.41193553163299867, 1460.804056526489831, 207.7426899176469988 ) ) ;
#70069 = CARTESIAN_POINT ( 'NONE',  ( -17.95620059730000051, 1457.813590052430072, 229.1786308768979836 ) ) ;
#70070 = ORIENTED_EDGE ( 'NONE', *, *, #49688, .T. ) ;
#70071 = EDGE_LOOP ( 'NONE', ( #26020, #31608, #71018, #100227 ) ) ;
#70072 = CARTESIAN_POINT ( 'NONE',  ( -2.409586283469999923, 1426.663880916129983, 144.1938086916980239 ) ) ;
#70073 = CARTESIAN_POINT ( 'NONE',  ( 8.079271929000000796, 1423.284668454760094, 195.9721669254989820 ) ) ;
#70074 = ORIENTED_EDGE ( 'NONE', *, *, #78879, .T. ) ;
#70075 = AXIS2_PLACEMENT_3D ( 'NONE', #76724, #92966, #52092 ) ;
#70076 = CARTESIAN_POINT ( 'NONE',  ( -0.7199630763800000111, 1415.645607075230146, 184.8796628268980271 ) ) ;
#70077 = SPHERICAL_SURFACE ( 'NONE', #67087, 2.000000000000000000 ) ;
#70078 = CARTESIAN_POINT ( 'NONE',  ( 3.500000000000000000, 1409.663060387330006, 146.1721969590979882 ) ) ;
#70079 = CARTESIAN_POINT ( 'NONE',  ( 27.42787240605195009, 1509.319615610296296, 206.1613560982198692 ) ) ;
#70080 = CARTESIAN_POINT ( 'NONE',  ( 1.991789202884729715, 1421.124413674059952, 183.1574783845820207 ) ) ;
#70081 = CARTESIAN_POINT ( 'NONE',  ( 9.922915408476299604, 1451.489621189869695, 207.3832923455570096 ) ) ;
#70082 = CARTESIAN_POINT ( 'NONE',  ( 2.835697453489999909, 1501.613331751589840, 230.3199997588990016 ) ) ;
#70083 = CARTESIAN_POINT ( 'NONE',  ( 14.91384436259999902, 1485.716867147530138, 224.8720064076979952 ) ) ;
#70084 = VERTEX_POINT ( 'NONE', #75359 ) ;
#70085 = CARTESIAN_POINT ( 'NONE',  ( 6.551643386774999023, 1516.807958722750072, 203.3403553877570005 ) ) ;
#70086 = CARTESIAN_POINT ( 'NONE',  ( -5.000330033664999618, 1516.770163853809890, 209.8779366980180328 ) ) ;
#70087 = ORIENTED_EDGE ( 'NONE', *, *, #39174, .F. ) ;
#70088 = CARTESIAN_POINT ( 'NONE',  ( 11.86098062413520005, 1431.978481139299902, 149.9706316993390089 ) ) ;
#70089 = VECTOR ( 'NONE', #49167, 1000.000000000000000 ) ;
#70090 = CARTESIAN_POINT ( 'NONE',  ( 13.20674952220708143, 1444.700630393524307, 187.3249437680643723 ) ) ;
#70091 = ORIENTED_EDGE ( 'NONE', *, *, #399, .F. ) ;
#70092 = DIRECTION ( 'NONE',  ( 0.000000000000000000, 1.000000000000000000, 0.000000000000000000 ) ) ;
#70093 = CARTESIAN_POINT ( 'NONE',  ( -7.744919283042880132, 1508.476290139939920, 219.4107736818559999 ) ) ;
#70094 = CARTESIAN_POINT ( 'NONE',  ( 23.61230825720000226, 1435.322028862560046, 137.2857987807979896 ) ) ;
#70095 = CARTESIAN_POINT ( 'NONE',  ( -9.120463652338420601, 1471.255923615639858, 213.5777534691339952 ) ) ;
#70096 = CARTESIAN_POINT ( 'NONE',  ( -6.220537627200000586, 1424.583777295530126, 186.6152486391980005 ) ) ;
#70097 = CARTESIAN_POINT ( 'NONE',  ( 3.422118110653599832, 1410.133528635409903, 269.8663509809509833 ) ) ;
#70098 = CARTESIAN_POINT ( 'NONE',  ( -1.122592899216370017E-16, 1388.079727053959914, 209.1218459616989946 ) ) ;
#70099 = DIRECTION ( 'NONE',  ( 0.02616798426500960631, -0.9993150019883682011, 0.02616798426500970345 ) ) ;
#70100 = CARTESIAN_POINT ( 'NONE',  ( -2.465027318521849864, 1422.346290854769904, 192.7050527383619851 ) ) ;
#70101 = CARTESIAN_POINT ( 'NONE',  ( -25.94889933050000153, 1379.671554933049947, 211.6347087375590093 ) ) ;
#70102 = DIRECTION ( 'NONE',  ( -0.4794255386042018952, 0.000000000000000000, 0.8775825618903733139 ) ) ;
#70104 = FACE_OUTER_BOUND ( 'NONE', #108120, .T. ) ;
#70103 = CARTESIAN_POINT ( 'NONE',  ( -14.90880384090000099, 1503.968912916589943, 208.7967653244450048 ) ) ;
#70105 = CARTESIAN_POINT ( 'NONE',  ( -5.023809873749912391, 1422.821914202444304, 184.8408105619813568 ) ) ;
#70106 = EDGE_CURVE ( 'NONE', #48574, #110694, #15955, .T. ) ;
#70107 = CARTESIAN_POINT ( 'NONE',  ( 17.79886040655730284, 1417.133647275629983, 224.9897512113339815 ) ) ;
#70108 = CARTESIAN_POINT ( 'NONE',  ( -6.115766451680039850, 1497.554681153639876, 215.1697308089790113 ) ) ;
#70109 = ORIENTED_EDGE ( 'NONE', *, *, #85776, .F. ) ;
#70110 = CARTESIAN_POINT ( 'NONE',  ( 38.34143788450000301, 1440.913060387330006, 265.6112250856980381 ) ) ;
#70111 = AXIS2_PLACEMENT_3D ( 'NONE', #38808, #12519, #46697 ) ;
#70112 = CARTESIAN_POINT ( 'NONE',  ( 13.80546151116429954, 1434.979654507460054, 148.5370226032280243 ) ) ;
#70113 = CARTESIAN_POINT ( 'NONE',  ( -20.37381179411481469, 1524.397344074318880, 180.2832293763214864 ) ) ;
#70114 = CARTESIAN_POINT ( 'NONE',  ( 3.837812054080000035, 1506.875571340089891, 220.1607364553989896 ) ) ;
#70115 = DIRECTION ( 'NONE',  ( 0.000000000000000000, 0.000000000000000000, -1.000000000000000000 ) ) ;
#70116 = AXIS2_PLACEMENT_3D ( 'NONE', #70731, #107590, #8834 ) ;
#70118 = ORIENTED_EDGE ( 'NONE', *, *, #106265, .F. ) ;
#70117 = CARTESIAN_POINT ( 'NONE',  ( 1.364625987975899735, 1515.082030188910039, 204.7928485609430140 ) ) ;
#70119 = CARTESIAN_POINT ( 'NONE',  ( -15.68073676374516445, 1415.733564152250437, 209.6599020335900150 ) ) ;
#70120 = B_SPLINE_CURVE_WITH_KNOTS ( 'NONE', 3,
 ( #27490, #79571, #10142, #96916, #61678, #95801, #19069, #53273, #87412, #10707, #44878 ),
 .UNSPECIFIED., .F., .F.,
 ( 4, 2, 1, 2, 2, 4 ),
 ( 0.000000000000000000, 0.2499999999997352118, 0.3749999999995330957, 0.4374999999994320654, 0.4999999999993309796, 1.000000000000000000 ),
 .UNSPECIFIED. ) ;
#70121 = CARTESIAN_POINT ( 'NONE',  ( -7.544964944700390141, 1384.904325550069871, 219.0876571251629912 ) ) ;
#70122 = ADVANCED_FACE ( 'NONE', ( #82642 ), #35667, .F. ) ;
#70123 = CARTESIAN_POINT ( 'NONE',  ( -10.81519956420000028, 1424.921090988229935, 144.1714224092980032 ) ) ;
#70124 = CARTESIAN_POINT ( 'NONE',  ( -14.62342645192239843, 1422.162688039920113, 221.5608089125659887 ) ) ;
#70125 = CARTESIAN_POINT ( 'NONE',  ( 0.8076263318534745439, 1444.250888050305093, 218.0378284561443820 ) ) ;
#70126 = CARTESIAN_POINT ( 'NONE',  ( 4.456500632703686016, 1370.468720332280100, 209.2823377659277924 ) ) ;
#70127 = EDGE_CURVE ( 'NONE', #93336, #84761, #41856, .T. ) ;
#70128 = DIRECTION ( 'NONE',  ( 0.8775825618903763115, 0.000000000000000000, -0.4794255386041963996 ) ) ;
#70129 = CARTESIAN_POINT ( 'NONE',  ( -13.22806383169999833, 1431.113060387329824, 222.3499097936980036 ) ) ;
#70130 = CARTESIAN_POINT ( 'NONE',  ( 13.26154391220000051, 1415.081125743829944, 228.6222406189980063 ) ) ;
#70131 = CARTESIAN_POINT ( 'NONE',  ( -10.37617513340000031, 1479.403831781789904, 210.6295454589389919 ) ) ;
#70132 = CARTESIAN_POINT ( 'NONE',  ( -16.96734216822699892, 1460.582103501581969, 228.2620883328710022 ) ) ;
#70133 = CARTESIAN_POINT ( 'NONE',  ( -2.493073867885000183, 1516.826109302209943, 206.2575198447970024 ) ) ;
#70134 = CARTESIAN_POINT ( 'NONE',  ( 18.39250288750000095, 1408.568853042730098, 268.3412086706979949 ) ) ;
#70135 = CARTESIAN_POINT ( 'NONE',  ( -34.68852446352570951, 1522.861859112239244, 218.2490599185902624 ) ) ;
#70136 = CARTESIAN_POINT ( 'NONE',  ( 24.71638692850000396, 1435.786853257239954, 137.7886294928979964 ) ) ;
#70137 = CARTESIAN_POINT ( 'NONE',  ( 19.52745459059999789, 1469.160779044030050, 191.2963237270979846 ) ) ;
#70138 = CARTESIAN_POINT ( 'NONE',  ( -23.49218588160000110, 1435.195132014040155, 213.3092087416680158 ) ) ;
#70139 = CARTESIAN_POINT ( 'NONE',  ( 27.43355929049999986, 1507.980920698529872, 207.4175378521480013 ) ) ;
#70140 = CARTESIAN_POINT ( 'NONE',  ( -15.61594006588599903, 1418.240309429660101, 203.0222030835800240 ) ) ;
#70141 = CARTESIAN_POINT ( 'NONE',  ( 32.02808312589916540, 1512.187213306747481, 198.2787714533495489 ) ) ;
#70142 = CARTESIAN_POINT ( 'NONE',  ( -22.33217205817994255, 1507.117986396238166, 204.9771641880283823 ) ) ;
#70143 = CARTESIAN_POINT ( 'NONE',  ( -16.61533299009999709, 1414.913060387329779, 205.7754145581380101 ) ) ;
#70144 = CARTESIAN_POINT ( 'NONE',  ( -13.95628782549999869, 1442.683319114259803, 188.5952711372979991 ) ) ;
#70145 = EDGE_CURVE ( 'NONE', #18900, #63032, #8665, .T. ) ;
#70146 = CARTESIAN_POINT ( 'NONE',  ( -27.78452750130110260, 1508.000976266860107, 210.4681927182890036 ) ) ;
#70147 = CARTESIAN_POINT ( 'NONE',  ( -33.54529832459999739, 1435.829277014980107, 135.9561275551980088 ) ) ;
#70148 = CARTESIAN_POINT ( 'NONE',  ( 18.51436573157358723, 1512.187213306747481, 181.1015051776552696 ) ) ;
#70149 = ORIENTED_EDGE ( 'NONE', *, *, #15321, .T. ) ;
#70150 = ADVANCED_FACE ( 'NONE', ( #42286 ), #85692, .T. ) ;
#70151 = CARTESIAN_POINT ( 'NONE',  ( -2.822464128215000034, 1512.205735116489905, 201.3478245270569857 ) ) ;
#70152 = CARTESIAN_POINT ( 'NONE',  ( -12.86297904326220021, 1409.362245513460039, 201.5229356212220182 ) ) ;
#70153 = ORIENTED_EDGE ( 'NONE', *, *, #67288, .F. ) ;
#70155 = EDGE_CURVE ( 'NONE', #35724, #66359, #74007, .T. ) ;
#70154 = CARTESIAN_POINT ( 'NONE',  ( 8.060344786502357195, 1436.149655876709176, 226.2159421968783022 ) ) ;
#70156 = CARTESIAN_POINT ( 'NONE',  ( -38.70127719692458612, 1443.501467202840104, 136.9798462687442679 ) ) ;
#70157 = VECTOR ( 'NONE', #62484, 1000.000000000000000 ) ;
#70158 = CARTESIAN_POINT ( 'NONE',  ( -46.16778036140000552, 1446.056973084060019, 266.9714954301979901 ) ) ;
#70159 = CARTESIAN_POINT ( 'NONE',  ( -29.53442096303453823, 1525.651285554135484, 196.5125176505563900 ) ) ;
#70160 = CARTESIAN_POINT ( 'NONE',  ( -14.45750500688560081, 1416.828039245989885, 221.3916439204320170 ) ) ;
#70161 = CARTESIAN_POINT ( 'NONE',  ( -25.63704141100000200, 1507.963169804229892, 218.3319399335480000 ) ) ;
#70162 = CARTESIAN_POINT ( 'NONE',  ( -75.37878430945180241, 1384.648787239799958, 300.3730460693899431 ) ) ;
#70163 = CARTESIAN_POINT ( 'NONE',  ( -23.31512350511849974, 1384.956600135750023, 202.6507508542970015 ) ) ;
#70164 = CARTESIAN_POINT ( 'NONE',  ( 18.41238929687650128, 1425.273680578170115, 226.4426435738229770 ) ) ;
#70165 = CARTESIAN_POINT ( 'NONE',  ( 20.85881780809999952, 1508.960366401729971, 227.7807767123979943 ) ) ;
#70166 = CARTESIAN_POINT ( 'NONE',  ( 15.22899453930000035, 1495.924838334530023, 224.5915237618979745 ) ) ;
#70167 = EDGE_CURVE ( 'NONE', #19615, #59795, #12520, .T. ) ;
#70168 = DIRECTION ( 'NONE',  ( -0.9533478951374150245, 0.2986798387784170283, 0.04379662937212339818 ) ) ;
#70169 = CARTESIAN_POINT ( 'NONE',  ( -5.432410439650000811, 1391.426148861440197, 214.9021618825790085 ) ) ;
#70170 = CARTESIAN_POINT ( 'NONE',  ( -9.837454594919998740, 1508.005995996430102, 182.3419145424980172 ) ) ;
#70171 = CARTESIAN_POINT ( 'NONE',  ( -23.49882790210000394, 1410.228905210230096, 207.0913801706779793 ) ) ;
#70172 = CARTESIAN_POINT ( 'NONE',  ( 17.84204423069999734, 1415.932840167130053, 208.7775004867189921 ) ) ;
#70173 = CARTESIAN_POINT ( 'NONE',  ( 5.034012500299999360, 1484.257038904289857, 219.3935155832990063 ) ) ;
#70174 = CARTESIAN_POINT ( 'NONE',  ( 10.65098579914269905, 1480.263159560079885, 208.4913410984459858 ) ) ;
#70175 = CARTESIAN_POINT ( 'NONE',  ( -106.4081690619180023, 1391.913060387289988, 304.4390516697600333 ) ) ;
#70176 = CARTESIAN_POINT ( 'NONE',  ( 10.68098866639740052, 1451.528505696489901, 190.2751307916069834 ) ) ;
#70177 = CARTESIAN_POINT ( 'NONE',  ( -6.725623931370599884, 1508.728101229370168, 216.3255547359810009 ) ) ;
#70178 = CARTESIAN_POINT ( 'NONE',  ( 17.60627569411529691, 1410.895669416499913, 224.1775087544040161 ) ) ;
#70179 =( BOUNDED_CURVE ( )  B_SPLINE_CURVE ( 3, ( #18430, #45347, #18987, #37472 ),
 .UNSPECIFIED., .F., .T. ) 
 B_SPLINE_CURVE_WITH_KNOTS ( ( 4, 4 ),
 ( 3.108823480124809802, 3.416777941171309951 ),
 .UNSPECIFIED. ) 
 CURVE ( )  GEOMETRIC_REPRESENTATION_ITEM ( )  RATIONAL_B_SPLINE_CURVE ( ( 1.000000000000000000, 0.9921126061611611480, 0.9921126061611611480, 1.000000000000000000 ) ) 
 REPRESENTATION_ITEM ( '' )  );
#70180 = B_SPLINE_CURVE_WITH_KNOTS ( 'NONE', 5,
 ( #90214, #21889, #28681, #21344, #20261, #55550, #54461, #89133, #12959, #80739, #47141, #88599, #46054, #38716, #4047, #81267, #13499, #3503, #4582, #72891, #107032 ),
 .UNSPECIFIED., .F., .F.,
 ( 6, 3, 3, 3, 3, 3, 6 ),
 ( -36.02199544990000390, -35.70255572539999633, -35.38311600090000297, -30.91096027220000053, -15.58155506210000141, -15.15568292920000104, -14.73068219289999803 ),
 .UNSPECIFIED. ) ;
#70182 = CARTESIAN_POINT ( 'NONE',  ( -12.28864222183389998, 1378.254430273839944, 210.0761076775810068 ) ) ;
#70181 = DIRECTION ( 'NONE',  ( 0.1751037286923191050, 0.3726097680845921745, -0.9113180810924323971 ) ) ;
#70183 = CARTESIAN_POINT ( 'NONE',  ( -0.1019954133980000149, 1415.740983310430011, 233.4942065637980306 ) ) ;
#70184 = CARTESIAN_POINT ( 'NONE',  ( 9.788553136239070085, 1435.243871060430138, 208.4607419252359932 ) ) ;
#70185 = CARTESIAN_POINT ( 'NONE',  ( -11.32899621019999969, 1490.498838803789795, 210.5081409889190240 ) ) ;
#70186 = EDGE_CURVE ( 'NONE', #24399, #29251, #36304, .T. ) ;
#70187 = CARTESIAN_POINT ( 'NONE',  ( -23.31536538260000313, 1425.877123410529975, 211.5352558136579830 ) ) ;
#70188 = CARTESIAN_POINT ( 'NONE',  ( -1.780436306985229811, 1421.048930496699995, 183.4850363039900003 ) ) ;
#70189 = CARTESIAN_POINT ( 'NONE',  ( -3.264778817514999876, 1516.727068157269969, 204.1245957781970048 ) ) ;
#70190 = CARTESIAN_POINT ( 'NONE',  ( 15.62010807923499911, 1514.600163677630007, 193.7548396194670204 ) ) ;
#70191 = CARTESIAN_POINT ( 'NONE',  ( -15.55317322349129938, 1485.870500728060051, 186.9405944658579983 ) ) ;
#70192 = CARTESIAN_POINT ( 'NONE',  ( -19.52959706730000278, 1468.975338568629923, 192.9635188021979957 ) ) ;
#70193 = EDGE_CURVE ( 'NONE', #39961, #42280, #96469, .T. ) ;
#70194 = CIRCLE ( 'NONE', #5815, 1.999999999999999556 ) ;
#70195 = CARTESIAN_POINT ( 'NONE',  ( 10.99927853205480055, 1502.537208110279835, 214.7972864508199962 ) ) ;
#70196 = CARTESIAN_POINT ( 'NONE',  ( -9.617736285228385640, 1422.771253444837839, 210.6923910180071857 ) ) ;
#70198 = ORIENTED_EDGE ( 'NONE', *, *, #101461, .F. ) ;
#70197 = CARTESIAN_POINT ( 'NONE',  ( -60.20344105345110108, 1379.728587437710075, 265.9570968973860090 ) ) ;
#70199 = ORIENTED_EDGE ( 'NONE', *, *, #5619, .T. ) ;
#70200 = CARTESIAN_POINT ( 'NONE',  ( 11.95465844686730073, 1433.562513212249996, 150.0837927613160048 ) ) ;
#70201 = CARTESIAN_POINT ( 'NONE',  ( 20.53760542139772838, 1525.821544997590991, 184.7213720461152775 ) ) ;
#70202 = EDGE_LOOP ( 'NONE', ( #45288, #13217, #13083, #50639 ) ) ;
#70203 = CARTESIAN_POINT ( 'NONE',  ( -105.2302759960000031, 1379.130298687069853, 305.2168657121590059 ) ) ;
#70204 = CARTESIAN_POINT ( 'NONE',  ( -109.4839102970000084, 1384.920889589209992, 311.2841191852589873 ) ) ;
#70207 = EDGE_CURVE ( 'NONE', #108404, #83875, #68665, .T. ) ;
#70206 = CARTESIAN_POINT ( 'NONE',  ( -0.1042373741590000014, 1508.844537587730201, 179.8773204004980073 ) ) ;
#70205 = LINE ( 'NONE', #104311, #71171 ) ;
#70208 = DIRECTION ( 'NONE',  ( -1.000000000000000000, 0.000000000000000000, -2.775557561562891351E-14 ) ) ;
#70209 = CARTESIAN_POINT ( 'NONE',  ( 3.328378719390000295, 1488.171522112329967, 182.3487599890979993 ) ) ;
#70210 = CARTESIAN_POINT ( 'NONE',  ( -105.7924919010939959, 1378.913060387289988, 304.1383837694310159 ) ) ;
#70211 = CARTESIAN_POINT ( 'NONE',  ( -24.06822806131540204, 1444.795745940579991, 211.8976761515809812 ) ) ;
#70212 = FILL_AREA_STYLE ('',( #89168 ) ) ;
#70213 = CARTESIAN_POINT ( 'NONE',  ( -3.446329813785000251, 1516.812046502680005, 212.0014881234369852 ) ) ;
#70214 = CARTESIAN_POINT ( 'NONE',  ( 37.83686684571890169, 1436.862236043870098, 134.0999999968879877 ) ) ;
#70215 = CARTESIAN_POINT ( 'NONE',  ( -3.497059220858349526, 1428.107238701659981, 208.0505560005599932 ) ) ;
#70216 = CARTESIAN_POINT ( 'NONE',  ( -12.54761498111694884, 1509.351232781885074, 235.8718500083220704 ) ) ;
#70217 = ORIENTED_EDGE ( 'NONE', *, *, #37814, .F. ) ;
#70218 = CARTESIAN_POINT ( 'NONE',  ( 13.64250267370000103, 1435.175725784029964, 149.6291831842980287 ) ) ;
#70219 = DIRECTION ( 'NONE',  ( 0.9510565162951518658, 0.000000000000000000, -0.3090169943749528914 ) ) ;
#70220 = ORIENTED_EDGE ( 'NONE', *, *, #30943, .T. ) ;
#70221 = ORIENTED_EDGE ( 'NONE', *, *, #92897, .F. ) ;
#70222 = VERTEX_POINT ( 'NONE', #84013 ) ;
#70223 = CARTESIAN_POINT ( 'NONE',  ( -8.473068926205000295, 1511.778199792620171, 215.2106786806170078 ) ) ;
#70224 = CARTESIAN_POINT ( 'NONE',  ( -2.975604897060000198, 1464.763624779529891, 236.8058159536980156 ) ) ;
#70225 = CARTESIAN_POINT ( 'NONE',  ( 17.33396934321472926, 1451.072800439867706, 148.0459263477291074 ) ) ;
#70226 = CARTESIAN_POINT ( 'NONE',  ( -8.580820927359999573, 1384.944142096140013, 218.6694753803189997 ) ) ;
#70227 = CARTESIAN_POINT ( 'NONE',  ( -1.353007460168119902, 1465.121494863239832, 198.2016196216069943 ) ) ;
#70228 = CARTESIAN_POINT ( 'NONE',  ( -19.06540802248403565, 1442.452554616592579, 210.7014195594630905 ) ) ;
#70229 = CARTESIAN_POINT ( 'NONE',  ( -53.08802174891025061, 1379.700056302278199, 245.9205172436845146 ) ) ;
#70230 = CARTESIAN_POINT ( 'NONE',  ( 4.238698726834749131, 1446.369305975439829, 163.0897191397669985 ) ) ;
#70231 = CARTESIAN_POINT ( 'NONE',  ( -0.008809588698450001101, 1507.869595074230119, 237.5091932035980165 ) ) ;
#70232 = ORIENTED_EDGE ( 'NONE', *, *, #76427, .T. ) ;
#70233 = CARTESIAN_POINT ( 'NONE',  ( -3.462620856235000044, 1516.938330505699923, 206.6435391121569864 ) ) ;
#70234 = ORIENTED_EDGE ( 'NONE', *, *, #24097, .F. ) ;
#70235 = CARTESIAN_POINT ( 'NONE',  ( 32.84806791407179816, 1440.913060387330006, 257.4303453130210073 ) ) ;
#70236 = CARTESIAN_POINT ( 'NONE',  ( -20.65862993740000064, 1509.573542409829997, 188.2595545114980098 ) ) ;
#70237 = EDGE_LOOP ( 'NONE', ( #90118, #73304, #108836, #10395 ) ) ;
#70238 = CARTESIAN_POINT ( 'NONE',  ( -7.260552783093170426, 1508.878902882709781, 202.3557464436360078 ) ) ;
#70239 = CARTESIAN_POINT ( 'NONE',  ( -14.78404272899999938, 1410.801860023729887, 190.6280328239980122 ) ) ;
#70240 = CARTESIAN_POINT ( 'NONE',  ( -43.49718241125740548, 1379.669396352335298, 234.1649366570986217 ) ) ;
#70241 = CARTESIAN_POINT ( 'NONE',  ( -24.33264312739999724, 1442.481256506720001, 211.4417695029279685 ) ) ;
#70242 = CARTESIAN_POINT ( 'NONE',  ( -3.563323249086690403, 1433.447251056540154, 218.0070131686250079 ) ) ;
#70243 = CARTESIAN_POINT ( 'NONE',  ( -3.530668216773314118E-09, 1395.913060387170844, 197.9004239563262217 ) ) ;
#70244 = CARTESIAN_POINT ( 'NONE',  ( 6.646318662569973057, 1377.913060387289988, 209.1218459647943746 ) ) ;
#70245 = CARTESIAN_POINT ( 'NONE',  ( -12.91279240200000089, 1434.774393157829991, 149.9807649780979943 ) ) ;
#70246 = CARTESIAN_POINT ( 'NONE',  ( -2.188078410700000198, 1508.020976590390092, 220.9453026643990086 ) ) ;
#70247 = CARTESIAN_POINT ( 'NONE',  ( -25.19798387652940264, 1470.611580667020007, 212.0227933820560224 ) ) ;
#70248 = CARTESIAN_POINT ( 'NONE',  ( -1.123101616545000070, 1517.157901477309906, 214.9105372957470195 ) ) ;
#70249 = CARTESIAN_POINT ( 'NONE',  ( -2.923984041130000211, 1463.321251604189911, 228.6078422769990084 ) ) ;
#70250 = CARTESIAN_POINT ( 'NONE',  ( 5.586203231419629489, 1511.461696079649982, 217.8427964110400126 ) ) ;
#70251 = DIRECTION ( 'NONE',  ( -1.755985294532469921E-16, 1.000000000000000000, -1.338183447452831989E-16 ) ) ;
#70252 = CARTESIAN_POINT ( 'NONE',  ( -3.253141175365000137, 1516.858171774179937, 212.3894494859370070 ) ) ;
#70253 = CARTESIAN_POINT ( 'NONE',  ( -11.70289210622340192, 1482.471125327160053, 206.9498061491099747 ) ) ;
#70254 = CARTESIAN_POINT ( 'NONE',  ( -17.92791450389482222, 1486.167514923851513, 188.4156298903135962 ) ) ;
#70256 = ORIENTED_EDGE ( 'NONE', *, *, #3599, .F. ) ;
#70255 = CARTESIAN_POINT ( 'NONE',  ( -85.09270623130001354, 1390.599118280639914, 298.7241002662590290 ) ) ;
#70257 = CARTESIAN_POINT ( 'NONE',  ( -16.99777429700792553, 1524.964158026965606, 237.0504674185739873 ) ) ;
#70258 = CARTESIAN_POINT ( 'NONE',  ( 14.01630619350000018, 1463.409576321530039, 240.3753821329979985 ) ) ;
#70259 = CARTESIAN_POINT ( 'NONE',  ( 30.45769963430792515, 1526.208281990539263, 217.1507671409962370 ) ) ;
#70260 = DIRECTION ( 'NONE',  ( 0.02616798426500960631, 0.9993150019883683122, 0.02616798426500945712 ) ) ;
#70261 = CARTESIAN_POINT ( 'NONE',  ( -7.349614982530000340, 1507.875248142329838, 235.6215898391979806 ) ) ;
#70262 = CARTESIAN_POINT ( 'NONE',  ( 7.443246446248299009, 1423.092341332710021, 195.6161848952980051 ) ) ;
#70263 = B_SPLINE_CURVE_WITH_KNOTS ( 'NONE', 5,
 ( #25725, #59925, #109754, #84545, #60474, #59375 ),
 .UNSPECIFIED., .F., .F.,
 ( 6, 6 ),
 ( -2.000000000000000000, -2.311399205368047660E-08 ),
 .UNSPECIFIED. ) ;
#70265 = CARTESIAN_POINT ( 'NONE',  ( 19.08933866519999967, 1456.280081694130104, 226.1031454244979955 ) ) ;
#70264 = CARTESIAN_POINT ( 'NONE',  ( 11.87124599549999893, 1432.722052905369992, 149.9814473066979872 ) ) ;
#70266 = CARTESIAN_POINT ( 'NONE',  ( -9.191350345563439106, 1450.447642638940124, 208.3545562163980094 ) ) ;
#70267 = CARTESIAN_POINT ( 'NONE',  ( -106.8792834639999967, 1379.710674565020099, 308.6693595243589812 ) ) ;
#70268 = ORIENTED_EDGE ( 'NONE', *, *, #48922, .T. ) ;
#70269 = CARTESIAN_POINT ( 'NONE',  ( 5.775236792744999903, 1516.804776704140068, 204.1142572851869943 ) ) ;
#70270 = CARTESIAN_POINT ( 'NONE',  ( -10.49942725105620056, 1508.438008077390123, 218.5529879601039909 ) ) ;
#70271 = CARTESIAN_POINT ( 'NONE',  ( 11.21032122953132770, 1522.051704408389924, 188.3716648695481695 ) ) ;
#70272 = CARTESIAN_POINT ( 'NONE',  ( 12.83854459959200156, 1470.906649396920102, 269.8736685321649702 ) ) ;
#70273 = CARTESIAN_POINT ( 'NONE',  ( 2.478743724850000163, 1435.404071181940026, 157.6105368136979905 ) ) ;
#70274 = CARTESIAN_POINT ( 'NONE',  ( 20.89240899049999811, 1496.462831935489930, 205.9570778813589982 ) ) ;
#70275 = CARTESIAN_POINT ( 'NONE',  ( 1.090037377353519974E-11, 1406.777728848529932, 269.6500679732980075 ) ) ;
#70276 = B_SPLINE_CURVE_WITH_KNOTS ( 'NONE', 3,
 ( #46267, #3709, #18250, #44034, #78171, #87131, #10420, #56849, #14822, #55768, #40034, #4771, #56295, #90981 ),
 .UNSPECIFIED., .F., .F.,
 ( 4, 2, 2, 2, 2, 2, 4 ),
 ( 0.000000000000000000, 0.001069581499410647389, 0.001604372249115970867, 0.002139162998821294778, 0.003208744498231351060, 0.003743535247936652637, 0.004278325997641954648 ),
 .UNSPECIFIED. ) ;
#70277 = EDGE_CURVE ( 'NONE', #21233, #68144, #101788, .T. ) ;
#70278 = CARTESIAN_POINT ( 'NONE',  ( -38.86154762539019458, 1440.913060394929971, 257.6231068593190230 ) ) ;
#70279 = CARTESIAN_POINT ( 'NONE',  ( 34.16143226917030518, 1450.427616041969941, 136.2389182185960124 ) ) ;
#70280 = CARTESIAN_POINT ( 'NONE',  ( 2.497446428329765489, 1449.075933931984537, 154.5437254066351329 ) ) ;
#70281 = CARTESIAN_POINT ( 'NONE',  ( 1.372954253770000133, 1432.414673090790075, 200.7998073325189807 ) ) ;
#70282 = ADVANCED_FACE ( 'NONE', ( #49880 ), #7314, .T. ) ;
#70283 = CARTESIAN_POINT ( 'NONE',  ( -1.433829657236012523, 1450.688199284849816, 182.8043069926514193 ) ) ;
#70284 = CARTESIAN_POINT ( 'NONE',  ( -0.3534431153210010335, 1507.725504649390132, 220.9869073979990048 ) ) ;
#70285 = LINE ( 'NONE', #106055, #1443 ) ;
#70286 = ORIENTED_EDGE ( 'NONE', *, *, #58250, .T. ) ;
#70287 = CARTESIAN_POINT ( 'NONE',  ( -38.34143788450000301, 1436.524347981669962, 265.6112249940979950 ) ) ;
#70288 = CARTESIAN_POINT ( 'NONE',  ( -0.5697963391879999895, 1450.893162800530263, 181.2886238165980046 ) ) ;
#70289 = CARTESIAN_POINT ( 'NONE',  ( 4.449801743544099963, 1466.569988769939982, 199.3372086498600027 ) ) ;
#70290 = CARTESIAN_POINT ( 'NONE',  ( -0.5500088493020000024, 1475.046162849929942, 269.6499792952980101 ) ) ;
#70291 = FACE_OUTER_BOUND ( 'NONE', #79696, .T. ) ;
#70292 = CARTESIAN_POINT ( 'NONE',  ( -30.29630067237287250, 1526.329757971584968, 196.4535985240159448 ) ) ;
#70293 = CARTESIAN_POINT ( 'NONE',  ( 9.461346545499999650, 1428.170031190390091, 212.4970399571089956 ) ) ;
#70294 = CARTESIAN_POINT ( 'NONE',  ( -20.70560609375029770, 1384.860107662629844, 221.2521089292840202 ) ) ;
#70295 = CARTESIAN_POINT ( 'NONE',  ( -18.96271086799999850, 1416.819756528530206, 208.0003800946280137 ) ) ;
#70296 = CARTESIAN_POINT ( 'NONE',  ( 11.86774696298919984, 1432.458695464179982, 149.9821701094620039 ) ) ;
#70297 = CARTESIAN_POINT ( 'NONE',  ( 7.887474265800920037, 1512.146734774960350, 206.1643637411737302 ) ) ;
#70298 = CARTESIAN_POINT ( 'NONE',  ( -13.48132209962330030, 1443.611916072062741, 169.3589951324157710 ) ) ;
#70299 = ORIENTED_EDGE ( 'NONE', *, *, #108978, .F. ) ;
#70300 = CARTESIAN_POINT ( 'NONE',  ( 4.408870434958439333, 1425.824683284920184, 185.4670092970000042 ) ) ;
#70301 = CARTESIAN_POINT ( 'NONE',  ( 11.98890328080000067, 1442.756953654919926, 147.5994355510979688 ) ) ;
#70302 = ORIENTED_EDGE ( 'NONE', *, *, #20671, .T. ) ;
#70303 = CARTESIAN_POINT ( 'NONE',  ( -11.36959371680000075, 1503.847165134090119, 207.0750569533189775 ) ) ;
#70304 = CARTESIAN_POINT ( 'NONE',  ( 2.242229686229999963, 1409.158574056130192, 231.2133334487979823 ) ) ;
#70305 = CARTESIAN_POINT ( 'NONE',  ( -1.642047857909999964, 1448.524332027589935, 190.1362812327990071 ) ) ;
#70307 = CARTESIAN_POINT ( 'NONE',  ( -1.955601760757490037, 1457.577163455510117, 219.5947542298710005 ) ) ;
#70306 = CARTESIAN_POINT ( 'NONE',  ( 10.74293569890000022, 1425.684509311930242, 97.29932836569790311 ) ) ;
#70308 = CARTESIAN_POINT ( 'NONE',  ( -2.170628023513319516, 1485.611815822959898, 197.4219878149299916 ) ) ;
#70309 = CARTESIAN_POINT ( 'NONE',  ( -9.114100666540000617, 1450.438723326089985, 204.6615263125590047 ) ) ;
#70310 = CARTESIAN_POINT ( 'NONE',  ( 6.554778533645000849, 1516.929962200689943, 201.4024535497269994 ) ) ;
#70311 = CARTESIAN_POINT ( 'NONE',  ( 7.389162030640000545, 1425.109552474849806, 212.4764166173689830 ) ) ;
#70312 = CARTESIAN_POINT ( 'NONE',  ( 11.69992624430000028, 1435.514532378290141, 225.6365414701989778 ) ) ;
#70313 = FACE_BOUND ( 'NONE', #97456, .T. ) ;
#70314 = CARTESIAN_POINT ( 'NONE',  ( 7.583791906034999641, 1511.751588929339960, 206.7961148284170179 ) ) ;
#70315 = CARTESIAN_POINT ( 'NONE',  ( 2.541163892419999737, 1448.917481751670039, 182.8661774463979839 ) ) ;
#70316 = EDGE_CURVE ( 'NONE', #56560, #11116, #93520, .T. ) ;
#70317 = CARTESIAN_POINT ( 'NONE',  ( 8.120855199716963568, 1364.859655959927750, 208.3718459617061285 ) ) ;
#70319 = EDGE_LOOP ( 'NONE', ( #45349, #63355, #12063, #72910 ) ) ;
#70318 = CARTESIAN_POINT ( 'NONE',  ( -0.6774325393469999845, 1465.095555782530027, 238.0673157071979915 ) ) ;
#70320 = VERTEX_POINT ( 'NONE', #33056 ) ;
#70321 = CARTESIAN_POINT ( 'NONE',  ( -40.27186325100000630, 1443.842159933049970, 137.1351494573980005 ) ) ;
#70322 = CARTESIAN_POINT ( 'NONE',  ( 0.02607543431880000179, 1466.687777830830100, 235.6591783243979989 ) ) ;
#70323 = FACE_OUTER_BOUND ( 'NONE', #54633, .T. ) ;
#70324 = CARTESIAN_POINT ( 'NONE',  ( 3.272667022753710242, 1517.151704408390060, 229.2073556998901438 ) ) ;
#70326 = EDGE_CURVE ( 'NONE', #32377, #5789, #101338, .T. ) ;
#70325 = CARTESIAN_POINT ( 'NONE',  ( 12.53380499169999851, 1442.773887286369927, 177.9435428178979919 ) ) ;
#70327 = CARTESIAN_POINT ( 'NONE',  ( -3.665756888920000289, 1508.551704408389924, 214.1089243971590008 ) ) ;
#70328 = CARTESIAN_POINT ( 'NONE',  ( 14.59277107062129986, 1436.244837967300100, 149.8707660814949918 ) ) ;
#70329 = CARTESIAN_POINT ( 'NONE',  ( -36.21674782232960155, 1450.969262370170100, 135.9186764936750080 ) ) ;
#70330 = CARTESIAN_POINT ( 'NONE',  ( 33.93525398028069873, 1436.160849851710054, 136.3001642050429894 ) ) ;
#70331 = CARTESIAN_POINT ( 'NONE',  ( 9.646161636302020170, 1396.249911776859790, 214.5408828654969966 ) ) ;
#70332 = CARTESIAN_POINT ( 'NONE',  ( 13.93304799769729918, 1408.881101324619976, 204.4086770006200027 ) ) ;
#70333 = CARTESIAN_POINT ( 'NONE',  ( -5.337764340897860116, 1406.291602267970120, 269.0345653378449811 ) ) ;
#70334 = CARTESIAN_POINT ( 'NONE',  ( -14.20723507282459863, 1435.348451359640194, 149.4979282535020104 ) ) ;
#70335 = ORIENTED_EDGE ( 'NONE', *, *, #31801, .F. ) ;
#70336 = CARTESIAN_POINT ( 'NONE',  ( 3.902542322860000024, 1426.015650169130140, 185.2953858070979720 ) ) ;
#70337 = CARTESIAN_POINT ( 'NONE',  ( 20.85167060786188742, 1525.730671948510462, 234.0535507870877439 ) ) ;
#70338 = ORIENTED_EDGE ( 'NONE', *, *, #25998, .T. ) ;
#70339 = ORIENTED_EDGE ( 'NONE', *, *, #29001, .F. ) ;
#70340 = CARTESIAN_POINT ( 'NONE',  ( -4.023353920839999986, 1454.320588500490203, 200.2248028819489889 ) ) ;
#70341 = CARTESIAN_POINT ( 'NONE',  ( -3.034926079678273325, 1369.200812461397618, 207.6218459616989946 ) ) ;
#70342 = CARTESIAN_POINT ( 'NONE',  ( 3.264778779384999829, 1516.727068157269969, 214.1190961241369735 ) ) ;
#70343 = CARTESIAN_POINT ( 'NONE',  ( 4.820945208375000846, 1510.984078637139874, 216.7915721300269638 ) ) ;
#70344 = B_SPLINE_SURFACE_WITH_KNOTS ( 'NONE', 5, 5, ( 
 ( #20641, #1681, #71108, #27966, #79486, #88967 ),
 ( #43670, #2793, #35260, #77822, #96841, #44790 ),
 ( #78942, #95722, #28521, #1130, #70553, #52630 ),
 ( #26864, #70005, #69445, #62720, #35822, #104119 ),
 ( #104672, #27406, #62150, #96277, #65452, #13897 ),
 ( #5521, #55390, #23413, #99560, #46448, #57050 ),
 ( #38558, #98467, #89520, #97909, #21180, #4432 ),
 ( #12258, #12812, #107418, #22285, #72204, #46992 ),
 ( #64900, #81115, #106327, #73281, #66008, #72737 ) ),
 .UNSPECIFIED., .F., .F., .F.,
 ( 6, 3, 6 ),
 ( 6, 6 ),
 ( 20.66572445029999727, 22.33923004749999919, 24.01273564469999755 ),
 ( 0.000000000000000000, 2.000000000000000000 ),
 .UNSPECIFIED. ) ;
#70345 = ORIENTED_EDGE ( 'NONE', *, *, #17243, .T. ) ;
#70346 = CARTESIAN_POINT ( 'NONE',  ( -71.62432531729999141, 1374.712643070490230, 285.2199721836589674 ) ) ;
#70347 = CARTESIAN_POINT ( 'NONE',  ( 7.191822421769999529, 1414.913060387229962, 224.1599105121979960 ) ) ;
#70348 = CARTESIAN_POINT ( 'NONE',  ( 5.776491095245000373, 1516.858301627840092, 203.3390965304970166 ) ) ;
#70349 = CARTESIAN_POINT ( 'NONE',  ( -4.363122647530000009, 1407.471318475729959, 146.1721969590979882 ) ) ;
#70350 = CARTESIAN_POINT ( 'NONE',  ( 10603.70820181224371, 2837.742859962505918, -4739.672918854301315 ) ) ;
#70351 = CARTESIAN_POINT ( 'NONE',  ( 11.79467588633447583, 1433.007546482180260, 150.6262872999809019 ) ) ;
#70352 = CARTESIAN_POINT ( 'NONE',  ( -50.99365685415219929, 1384.624155639869969, 226.8516233277449885 ) ) ;
#70353 = CARTESIAN_POINT ( 'NONE',  ( 5.779627054084999216, 1516.977993847330026, 201.4011957967969977 ) ) ;
#70354 = CARTESIAN_POINT ( 'NONE',  ( -10.15115807179999941, 1410.198279941630062, 229.5434800901979884 ) ) ;
#70356 = ORIENTED_EDGE ( 'NONE', *, *, #28932, .F. ) ;
#70355 = CARTESIAN_POINT ( 'NONE',  ( -10.93884247429999945, 1445.278210069279794, 184.9723926117980284 ) ) ;
#70357 = LINE ( 'NONE', #97724, #33258 ) ;
#70358 = CARTESIAN_POINT ( 'NONE',  ( -24.49816830492780184, 1440.913060440859908, 212.6606737188390071 ) ) ;
#70359 = CARTESIAN_POINT ( 'NONE',  ( -1.385482440409720093E-15, 1384.214058746219962, 218.5641289260389897 ) ) ;
#70360 = SPHERICAL_SURFACE ( 'NONE', #67763, 2.000000000000000000 ) ;
#70361 = CARTESIAN_POINT ( 'NONE',  ( -24.89417918259999851, 1435.865321316010295, 137.4102906330980147 ) ) ;
#70362 = CARTESIAN_POINT ( 'NONE',  ( 6.950214933285000285, 1517.129577905929864, 211.9934263588270085 ) ) ;
#70363 = CARTESIAN_POINT ( 'NONE',  ( -65.30777065759998834, 1379.749275567730137, 273.2377066393590326 ) ) ;
#70364 = CARTESIAN_POINT ( 'NONE',  ( 0.009483596459017473723, 1508.335432445508786, 237.8375765388574337 ) ) ;
#70365 = CARTESIAN_POINT ( 'NONE',  ( -29.86283313086175539, 1525.137881624895272, 222.1297143728456263 ) ) ;
#70366 = CARTESIAN_POINT ( 'NONE',  ( 24.04366655069240366, 1494.655546942339924, 207.1744041867209773 ) ) ;
#70367 = CARTESIAN_POINT ( 'NONE',  ( 5.006259848694999626, 1516.939723362869927, 209.1089481433290018 ) ) ;
#70368 = ORIENTED_EDGE ( 'NONE', *, *, #22749, .T. ) ;
#70369 = CARTESIAN_POINT ( 'NONE',  ( 2.500000000000000000, 1435.788807054279914, 157.6019689661980010 ) ) ;
#70370 = CARTESIAN_POINT ( 'NONE',  ( -14.02792940870000038, 1415.367714275730123, 227.2463639653980181 ) ) ;
#70371 =( BOUNDED_CURVE ( )  B_SPLINE_CURVE ( 3, ( #10490, #44661, #68765, #26165 ),
 .UNSPECIFIED., .F., .F. ) 
 B_SPLINE_CURVE_WITH_KNOTS ( ( 4, 4 ),
 ( 0.000000000000000000, 0.7048113239778103223 ),
 .UNSPECIFIED. ) 
 CURVE ( )  GEOMETRIC_REPRESENTATION_ITEM ( )  RATIONAL_B_SPLINE_CURVE ( ( 1.000000000000000000, 0.9590300661663088144, 0.9590300661663088144, 1.000000000000000000 ) ) 
 REPRESENTATION_ITEM ( '' )  );
#70372 = CARTESIAN_POINT ( 'NONE',  ( -47.37385164190000353, 1385.009681923870176, 256.2782761542590038 ) ) ;
#70373 = ORIENTED_EDGE ( 'NONE', *, *, #87314, .T. ) ;
#70374 = CARTESIAN_POINT ( 'NONE',  ( -14.54965318006719954, 1385.296335759480144, 219.3214808617400138 ) ) ;
#70375 = DIRECTION ( 'NONE',  ( 0.01398399491000389475, 0.01017778245426219710, -0.9998504191281166742 ) ) ;
#70376 = CARTESIAN_POINT ( 'NONE',  ( 12.12836356214739908, 1434.009854529710083, 150.0535883806440154 ) ) ;
#70377 = CARTESIAN_POINT ( 'NONE',  ( 14.13280191679420028, 1478.704388969779984, 231.2915111619190043 ) ) ;
#70378 = CARTESIAN_POINT ( 'NONE',  ( -22.35377295150689747, 1508.960832111700029, 226.0627451311750065 ) ) ;
#70379 = CARTESIAN_POINT ( 'NONE',  ( 3.511588562210000042, 1485.920069248189975, 198.9399334953989751 ) ) ;
#70380 = CARTESIAN_POINT ( 'NONE',  ( 33.93019615848946557, 1512.187213306747481, 197.6607374645996060 ) ) ;
#70381 = CARTESIAN_POINT ( 'NONE',  ( 0.02113572768988940254, 1420.444438332730215, 182.6732129553429900 ) ) ;
#70383 = CARTESIAN_POINT ( 'NONE',  ( -3.959162678200000229, 1419.915783653529843, 186.3511350151979968 ) ) ;
#70382 = CARTESIAN_POINT ( 'NONE',  ( 7.719392382375000139, 1516.929962200689943, 215.6766245038770080 ) ) ;
#70384 = CARTESIAN_POINT ( 'NONE',  ( -5.607667144112699731, 1391.799625134960024, 214.9775039132319705 ) ) ;
#70385 = CARTESIAN_POINT ( 'NONE',  ( 18.42577555256999844, 1424.509265906519886, 223.4215472205989954 ) ) ;
#70386 = ORIENTED_EDGE ( 'NONE', *, *, #43461, .T. ) ;
#70387 = CARTESIAN_POINT ( 'NONE',  ( -12.44185449472369953, 1415.426561690380140, 196.8128181430920165 ) ) ;
#70388 = FACE_OUTER_BOUND ( 'NONE', #43166, .T. ) ;
#70389 = ORIENTED_EDGE ( 'NONE', *, *, #37285, .T. ) ;
#70390 = DIRECTION ( 'NONE',  ( -0.6205445805634668410, -0.7071067811868649855, -0.3390050494208925458 ) ) ;
#70391 = CARTESIAN_POINT ( 'NONE',  ( 4.865303301610000908, 1425.588844564269948, 210.1313439721089935 ) ) ;
#70392 = DIRECTION ( 'NONE',  ( 1.755985294532464991E-16, -1.000000000000000000, 1.338183447452830017E-16 ) ) ;
#70393 = UNCERTAINTY_MEASURE_WITH_UNIT (LENGTH_MEASURE( 1.000000000000000082E-05 ), #14654, 'distance_accuracy_value', 'NONE');
#70394 = CARTESIAN_POINT ( 'NONE',  ( 2.735388290130000399, 1441.676293522389869, 218.2628663559290203 ) ) ;
#70395 = CARTESIAN_POINT ( 'NONE',  ( -26.35475552313950232, 1507.985742420310089, 201.5462045797129917 ) ) ;
#70396 = CARTESIAN_POINT ( 'NONE',  ( -3.129590240750207641, 1508.089762839850664, 220.8354442735884788 ) ) ;
#70397 = CARTESIAN_POINT ( 'NONE',  ( -2.499999998559999881, 1448.104721231620033, 157.8850639176980337 ) ) ;
#70398 = CARTESIAN_POINT ( 'NONE',  ( -28.96739426325758870, 1526.189892541618974, 220.8024485780730686 ) ) ;
#70399 = CARTESIAN_POINT ( 'NONE',  ( -21.65324558190000204, 1435.253471290910056, 140.9571069649979904 ) ) ;
#70400 = CARTESIAN_POINT ( 'NONE',  ( -7.333237907140000900, 1433.447543843880112, 149.5704065546979962 ) ) ;
#70401 = CARTESIAN_POINT ( 'NONE',  ( 16.72731342339999827, 1418.990981506430217, 191.3670037215980244 ) ) ;
#70403 = CARTESIAN_POINT ( 'NONE',  ( -19.00997723749662427, 1439.581593688745215, 210.0041471448513732 ) ) ;
#70402 = CARTESIAN_POINT ( 'NONE',  ( 4.253777714910000007, 1442.471859903390168, 216.9083338397390150 ) ) ;
#70404 = CARTESIAN_POINT ( 'NONE',  ( -26.79413315976150045, 1435.433175095809929, 135.2874648155150226 ) ) ;
#70405 = ORIENTED_EDGE ( 'NONE', *, *, #36890, .T. ) ;
#70406 = CYLINDRICAL_SURFACE ( 'NONE', #78585, 0.9999999999999988898 ) ;
#70407 = CARTESIAN_POINT ( 'NONE',  ( 24.38386427640000065, 1449.838343677799912, 206.7258738186879725 ) ) ;
#70408 = CARTESIAN_POINT ( 'NONE',  ( -24.04833748900000145, 1437.594120219370097, 211.5101582450080002 ) ) ;
#70409 = CARTESIAN_POINT ( 'NONE',  ( -2.461679514290000537, 1485.354438815590129, 197.8976887413989800 ) ) ;
#70410 = CARTESIAN_POINT ( 'NONE',  ( -4.646147325060000277, 1378.399971913189802, 203.6922293430689876 ) ) ;
#70411 = CARTESIAN_POINT ( 'NONE',  ( -10.47307406344970104, 1479.706635250730187, 209.8500660232109851 ) ) ;
#70412 = CARTESIAN_POINT ( 'NONE',  ( -12.53380499169999851, 1442.773887286369927, 169.4755105685979970 ) ) ;
#70413 = CARTESIAN_POINT ( 'NONE',  ( -11.37556622210709811, 1470.595267410999895, 209.8768689712920263 ) ) ;
#70414 = CARTESIAN_POINT ( 'NONE',  ( -8.150407651345240367, 1489.695318043820180, 216.4961765964640108 ) ) ;
#70415 = CARTESIAN_POINT ( 'NONE',  ( -19.58883746862870012, 1465.811302608600045, 204.1485295717249926 ) ) ;
#70417 = EDGE_CURVE ( 'NONE', #36273, #23739, #108695, .T. ) ;
#70416 = CARTESIAN_POINT ( 'NONE',  ( -83.41305439239448560, 1383.774604776039951, 305.6893928593270289 ) ) ;
#70418 = B_SPLINE_CURVE_WITH_KNOTS ( 'NONE', 5,
 ( #64687, #13670, #67442, #18101, #25387, #33802, #59580, #103200, #76370, #26506, #68543, #1328 ),
 .UNSPECIFIED., .F., .F.,
 ( 6, 3, 3, 6 ),
 ( 0.000000000000000000, 0.2278800823983170021, 0.5900544727611899409, 1.000000000000000000 ),
 .UNSPECIFIED. ) ;
#70419 = CARTESIAN_POINT ( 'NONE',  ( -109.7131932503749994, 1383.420641160820196, 311.2779527788660516 ) ) ;
#70420 = CARTESIAN_POINT ( 'NONE',  ( -32.37018134260411983, 1512.187213306747481, 200.1723992780599986 ) ) ;
#70421 = CARTESIAN_POINT ( 'NONE',  ( -22.83134035751703905, 1409.745587068702889, 209.7110239188152150 ) ) ;
#70423 = ORIENTED_EDGE ( 'NONE', *, *, #106847, .T. ) ;
#70422 = CARTESIAN_POINT ( 'NONE',  ( 10.57119421182350116, 1452.454795556669978, 209.2037162487509931 ) ) ;
#70424 = CARTESIAN_POINT ( 'NONE',  ( -18.57177926220356667, 1458.612650609036109, 227.5361665883615387 ) ) ;
#70425 = CARTESIAN_POINT ( 'NONE',  ( -87.68417812469999717, 1381.021699689639945, 305.9844954027590234 ) ) ;
#70426 = CARTESIAN_POINT ( 'NONE',  ( 19.98048820006079751, 1508.975598045479956, 229.6642444245289880 ) ) ;
#70427 = ADVANCED_FACE ( 'NONE', ( #94063 ), #44642, .T. ) ;
#70428 = ORIENTED_EDGE ( 'NONE', *, *, #42847, .T. ) ;
#70429 = ORIENTED_EDGE ( 'NONE', *, *, #74117, .F. ) ;
#70430 = CARTESIAN_POINT ( 'NONE',  ( 31.81407709660777527, 1522.382868172863937, 221.9534378623329758 ) ) ;
#70431 = CARTESIAN_POINT ( 'NONE',  ( 18.28847123799999963, 1425.325025442230071, 225.4709929694980133 ) ) ;
#70432 = CARTESIAN_POINT ( 'NONE',  ( 6.824596843277944913, 1424.786834349993342, 213.4892281956427098 ) ) ;
#70434 = CARTESIAN_POINT ( 'NONE',  ( -41.56052291270000154, 1440.913060434399995, 261.5689799299980223 ) ) ;
#70433 = CARTESIAN_POINT ( 'NONE',  ( 20.42020019299999944, 1470.816980701229795, 208.7465247758109967 ) ) ;
#70435 = CARTESIAN_POINT ( 'NONE',  ( -4.214198108440539770, 1495.305865917009896, 197.5356767487029970 ) ) ;
#70436 = CARTESIAN_POINT ( 'NONE',  ( -11.92876349830000038, 1433.442608765759815, 149.9100308696980051 ) ) ;
#70437 = CARTESIAN_POINT ( 'NONE',  ( 24.69949309869999965, 1509.552011340129866, 195.6045197258980011 ) ) ;
#70438 = CARTESIAN_POINT ( 'NONE',  ( -20.27111778190000280, 1485.538628530129927, 191.5000650964979911 ) ) ;
#70439 = CARTESIAN_POINT ( 'NONE',  ( 10.14794430829999961, 1410.198169809130150, 188.6983266523980092 ) ) ;
#70440 = CARTESIAN_POINT ( 'NONE',  ( 4.455748556580000574, 1421.964143777330037, 184.5555025332980108 ) ) ;
#70441 = CARTESIAN_POINT ( 'NONE',  ( -1.768532852147479906, 1515.064792882589927, 213.4512947377390049 ) ) ;
#70442 = CARTESIAN_POINT ( 'NONE',  ( 10.15459887489999957, 1436.277524974660082, 152.4140740738980071 ) ) ;
#70443 = CARTESIAN_POINT ( 'NONE',  ( -3.144306714850350293, 1440.618978642349930, 155.9524017610649764 ) ) ;
#70444 = CARTESIAN_POINT ( 'NONE',  ( -6.348459599079999904, 1451.445385983630104, 153.6738296132980111 ) ) ;
#70445 = CARTESIAN_POINT ( 'NONE',  ( 1.594477343619999932, 1465.161209020629940, 235.7125686318980229 ) ) ;
#70446 = VERTEX_POINT ( 'NONE', #45358 ) ;
#70447 = CARTESIAN_POINT ( 'NONE',  ( -2.487924076119420125, 1508.884228858900087, 213.6131300271670170 ) ) ;
#70448 = CARTESIAN_POINT ( 'NONE',  ( -17.60826646697100273, 1487.424402488250053, 195.0120373652249839 ) ) ;
#70449 = CARTESIAN_POINT ( 'NONE',  ( -42.54899908119999452, 1440.913084212150125, 270.0692079169979820 ) ) ;
#70450 = CARTESIAN_POINT ( 'NONE',  ( -23.89984773989923639, 1435.936556201614849, 211.3273771066375843 ) ) ;
#70451 = CARTESIAN_POINT ( 'NONE',  ( 9.663014860980000620, 1442.759804623820173, 153.0865865510980086 ) ) ;
#70452 = FACE_OUTER_BOUND ( 'NONE', #107493, .T. ) ;
#70453 = CARTESIAN_POINT ( 'NONE',  ( 4.360582346120001063, 1431.113060387329824, 190.2999270487979970 ) ) ;
#70454 = CARTESIAN_POINT ( 'NONE',  ( 2.831208615256320282, 1409.103140891420026, 230.6980589985730035 ) ) ;
#70455 = CARTESIAN_POINT ( 'NONE',  ( -1.149035020100000137, 1415.140114695929924, 226.8980037389979998 ) ) ;
#70456 = CARTESIAN_POINT ( 'NONE',  ( -7.703814818310000589, 1418.732955197130195, 232.4505356538980152 ) ) ;
#70457 = CARTESIAN_POINT ( 'NONE',  ( -9.659668702359999415, 1460.930246203189881, 210.9154259863990148 ) ) ;
#70458 = CARTESIAN_POINT ( 'NONE',  ( 9.060746519232587559, 1361.466900052261508, 210.6218459617030021 ) ) ;
#70459 = CARTESIAN_POINT ( 'NONE',  ( -45.28153491675919895, 1434.439803511990021, 266.7022297949800418 ) ) ;
#70460 = CARTESIAN_POINT ( 'NONE',  ( -3.086273611079999757, 1434.212532904980208, 185.3571854654980200 ) ) ;
#70461 = EDGE_LOOP ( 'NONE', ( #5159, #13825, #60977, #83393, #108532, #16422 ) ) ;
#70462 = CARTESIAN_POINT ( 'NONE',  ( -8.769605281700000532, 1423.161328079120040, 210.3743386932289923 ) ) ;
#70463 = ORIENTED_EDGE ( 'NONE', *, *, #19919, .F. ) ;
#70464 = CARTESIAN_POINT ( 'NONE',  ( 2.297629621054999571, 1516.970035769810011, 209.8568691683980205 ) ) ;
#70465 = DIRECTION ( 'NONE',  ( -8.117787186050000125E-15, -2.786659791809999935E-14, -1.000000000000000000 ) ) ;
#70466 = CARTESIAN_POINT ( 'NONE',  ( -2.470168521978398424, 1523.382868172864164, 242.8787258963054683 ) ) ;
#70467 = CARTESIAN_POINT ( 'NONE',  ( 7.112947187247390168, 1426.630951286630079, 213.1637636118960017 ) ) ;
#70468 = AXIS2_PLACEMENT_3D ( 'NONE', #47940, #82075, #14316 ) ;
#70469 = CARTESIAN_POINT ( 'NONE',  ( 1.553494589745609833, 1495.825222316409963, 221.3635534445299982 ) ) ;
#70470 = B_SPLINE_SURFACE_WITH_KNOTS ( 'NONE', 5, 5, ( 
 ( #11402, #45017, #106010, #29286, #1912, #45570 ),
 ( #3018, #10274, #105452, #63482, #80249, #104343 ),
 ( #46669, #28741, #37141, #95395, #62946, #97057 ),
 ( #79163, #52858, #36049, #61821, #36588, #61280 ),
 ( #44451, #19204, #20321, #12486, #3567, #72415 ),
 ( #54527, #70236, #2471, #86985, #53406, #10846 ) ),
 .UNSPECIFIED., .F., .F., .F.,
 ( 6, 6 ),
 ( 6, 6 ),
 ( 26.92148545460000264, 41.10482460869999954 ),
 ( 0.000000000000000000, 2.000000000000000000 ),
 .UNSPECIFIED. ) ;
#70471 = EDGE_LOOP ( 'NONE', ( #25628, #89572 ) ) ;
#70472 = CARTESIAN_POINT ( 'NONE',  ( -15.72497962059999921, 1506.810797420529980, 193.7296588674980171 ) ) ;
#70474 = CARTESIAN_POINT ( 'NONE',  ( 13.17272844760000083, 1434.822352678270136, 195.6302333700980114 ) ) ;
#70473 = CARTESIAN_POINT ( 'NONE',  ( 0.3570154777189999962, 1451.680777065829943, 183.0662967611979752 ) ) ;
#70475 = CARTESIAN_POINT ( 'NONE',  ( 11.60004869885203860, 1424.621825572507532, 136.2521570335653678 ) ) ;
#70476 = CARTESIAN_POINT ( 'NONE',  ( -16.93034130587640007, 1508.454808519469907, 213.3837835212590051 ) ) ;
#70477 = DIRECTION ( 'NONE',  ( -0.6906235816661250304, 0.2466512791670444904, 0.6798545542481230219 ) ) ;
#70478 = CARTESIAN_POINT ( 'NONE',  ( -8.588755023577968828, 1437.818823225090000, 207.9413749079909906 ) ) ;
#70479 = ORIENTED_EDGE ( 'NONE', *, *, #55265, .F. ) ;
#70480 = CARTESIAN_POINT ( 'NONE',  ( -16.50783381592070143, 1412.114139793179902, 270.0842635278900161 ) ) ;
#70481 = CARTESIAN_POINT ( 'NONE',  ( -6.564578723344999922, 1517.199196846569976, 207.4137433428170141 ) ) ;
#70482 = AXIS2_PLACEMENT_3D ( 'NONE', #12867, #3950, #81171 ) ;
#70483 = CARTESIAN_POINT ( 'NONE',  ( 4.249559015328859601, 1418.026146675719929, 233.7825626454939822 ) ) ;
#70484 = CARTESIAN_POINT ( 'NONE',  ( 8.435534112686301711, 1435.555565619180015, 206.9221676573980062 ) ) ;
#70486 = ORIENTED_EDGE ( 'NONE', *, *, #3750, .T. ) ;
#70485 = CARTESIAN_POINT ( 'NONE',  ( -7.324900043384086956, 1366.863774163400876, 207.6218459616988241 ) ) ;
#70487 = ORIENTED_EDGE ( 'NONE', *, *, #93867, .T. ) ;
#70488 = B_SPLINE_CURVE_WITH_KNOTS ( 'NONE', 3,
 ( #6243, #75669, #31998, #76209, #74570, #65625, #109813, #83490, #48272, #14642, #92994, #65069, #74017, #24124, #91363, #84596, #100306, #5710, #56665, #49361, #49914, #108706, #48828, #15175, #66186, #82951, #40393, #33092, #24663, #14082, #67281, #23591, #110354, #7887, #99185, #99738, #57780, #66732, #23030, #22464, #6785 ),
 .UNSPECIFIED., .F., .F.,
 ( 4, 2, 2, 1, 1, 2, 2, 2, 1, 1, 1, 2, 2, 2, 1, 1, 2, 2, 2, 2, 2, 2, 2, 4 ),
 ( 0.000000000000000000, 0.06250000000013367085, 0.09375000000022679081, 0.1093750000002732536, 0.1171875000002964018, 0.1210937500003325812, 0.1250000000003687606, 0.1875000000003629319, 0.2187500000003601286, 0.2343750000003837208, 0.2421875000003934908, 0.2460937500003762823, 0.2500000000003590461, 0.3125000000004938272, 0.3437500000005588308, 0.3593750000005890288, 0.3671875000005865308, 0.3750000000005840328, 0.5000000000004931611, 0.6250000000004023448, 0.6875000000003569367, 0.7187500000003310685, 0.7500000000003052003, 1.000000000000000000 ),
 .UNSPECIFIED. ) ;
#70489 = CARTESIAN_POINT ( 'NONE',  ( 45.47623103552137991, 1443.785048864438522, 268.9791838446159318 ) ) ;
#70490 = CARTESIAN_POINT ( 'NONE',  ( -0.3788414990293429985, 1408.926289824029936, 186.6322569618010050 ) ) ;
#70491 = CARTESIAN_POINT ( 'NONE',  ( -10.72663399029027964, 1438.657822394603727, 152.4853033122590773 ) ) ;
#70492 = CARTESIAN_POINT ( 'NONE',  ( 2.472529913803022783, 1523.678648413191695, 175.3762130535718597 ) ) ;
#70493 = AXIS2_PLACEMENT_3D ( 'NONE', #82696, #48560, #66475 ) ;
#70494 = CARTESIAN_POINT ( 'NONE',  ( -17.48716113793120286, 1415.020374539339855, 207.5653286189619848 ) ) ;
#70495 = CARTESIAN_POINT ( 'NONE',  ( -17.92118525700000120, 1420.840642511729811, 225.6991564338980254 ) ) ;
#70496 = CARTESIAN_POINT ( 'NONE',  ( 15.87316543544599945, 1474.349515721750095, 267.7599166360050162 ) ) ;
#70497 = ADVANCED_FACE ( 'NONE', ( #37483 ), #36922, .F. ) ;
#70498 = CARTESIAN_POINT ( 'NONE',  ( -8.771379158800783671, 1465.168284390142617, 232.9278865296558365 ) ) ;
#70499 = CARTESIAN_POINT ( 'NONE',  ( 10.31307702720000030, 1447.342907605319851, 186.9095413067980189 ) ) ;
#70500 = CARTESIAN_POINT ( 'NONE',  ( -5.788097265284999793, 1517.099836525840146, 206.6397780718770036 ) ) ;
#70501 = ORIENTED_EDGE ( 'NONE', *, *, #3914, .F. ) ;
#70502 = CARTESIAN_POINT ( 'NONE',  ( 20.38176113183206439, 1410.985889941965070, 219.3306597827873077 ) ) ;
#70503 = CARTESIAN_POINT ( 'NONE',  ( 1.487297559325930107, 1473.104910899560082, 182.5967061028410114 ) ) ;
#70504 = VERTEX_POINT ( 'NONE', #18996 ) ;
#70505 = CARTESIAN_POINT ( 'NONE',  ( 2.487924076119540029, 1508.884228858900087, 204.6305618962310007 ) ) ;
#70506 = EDGE_CURVE ( 'NONE', #2790, #41237, #17831, .T. ) ;
#70507 = CARTESIAN_POINT ( 'NONE',  ( 24.45310709153400097, 1452.054032404549844, 136.2426869603699799 ) ) ;
#70508 = EDGE_CURVE ( 'NONE', #52184, #17927, #71362, .T. ) ;
#70509 = CARTESIAN_POINT ( 'NONE',  ( -23.10442739037580040, 1411.095127590459924, 210.9251608898400150 ) ) ;
#70510 = CARTESIAN_POINT ( 'NONE',  ( -36.52015904620000697, 1388.283625214549829, 211.0401408952490101 ) ) ;
#70511 = FACE_OUTER_BOUND ( 'NONE', #27742, .T. ) ;
#70512 = CARTESIAN_POINT ( 'NONE',  ( 17.81467328779999804, 1409.700101153729975, 194.2398719659980202 ) ) ;
#70513 = CARTESIAN_POINT ( 'NONE',  ( -3.403509591720000227, 1496.471358393389892, 198.2852398950990107 ) ) ;
#70514 = CARTESIAN_POINT ( 'NONE',  ( 2.688983237145497363, 1439.653997274290305, 183.6213077983770461 ) ) ;
#70516 = CARTESIAN_POINT ( 'NONE',  ( -18.83596995908460059, 1424.713049970400107, 224.4964886877786512 ) ) ;
#70515 = CARTESIAN_POINT ( 'NONE',  ( 0.5934285380220000183, 1417.359862721729996, 235.5294838487980087 ) ) ;
#70517 = DIRECTION ( 'NONE',  ( 0.4794255386042031719, 0.000000000000000000, 0.8775825618903726477 ) ) ;
#70518 = CARTESIAN_POINT ( 'NONE',  ( -8.836665542129999551, 1381.997304831789961, 217.9968222378790017 ) ) ;
#70519 = CARTESIAN_POINT ( 'NONE',  ( -7.323974644434999348, 1516.647924054489977, 213.1579656147470132 ) ) ;
#70520 = CARTESIAN_POINT ( 'NONE',  ( 27.74428279426650334, 1446.393444133639832, 137.1635631392660173 ) ) ;
#70521 = ORIENTED_EDGE ( 'NONE', *, *, #110431, .T. ) ;
#70522 = CARTESIAN_POINT ( 'NONE',  ( 19.63722818192610120, 1519.551704408389924, 218.2362632616380154 ) ) ;
#70523 = DIRECTION ( 'NONE',  ( -1.755985294532469921E-16, 1.000000000000000000, -1.338183447452831989E-16 ) ) ;
#70524 = CARTESIAN_POINT ( 'NONE',  ( -8.061508288203871331, 1484.198171600520254, 200.3613286617199947 ) ) ;
#70525 = CARTESIAN_POINT ( 'NONE',  ( -8576.261851439176098, 2833.596074015790236, -10892.29874055330765 ) ) ;
#70526 = CARTESIAN_POINT ( 'NONE',  ( -34.87559606798220813, 1450.334017323499893, 136.2297881972530149 ) ) ;
#70527 = CARTESIAN_POINT ( 'NONE',  ( -6.759474677965349620, 1416.948096802409964, 218.8894228273509839 ) ) ;
#70528 = CARTESIAN_POINT ( 'NONE',  ( -3.114882401860000094, 1454.846680951630105, 214.3676144192479853 ) ) ;
#70529 = CARTESIAN_POINT ( 'NONE',  ( 45.63117166579991135, 1442.771140612856243, 266.1897092273976568 ) ) ;
#70530 = CARTESIAN_POINT ( 'NONE',  ( 10.98577627829999948, 1433.173240417669831, 151.7674451195979941 ) ) ;
#70531 = DIRECTION ( 'NONE',  ( -9.439841191556039654E-47, 1.000000000000000000, -1.836970198721029688E-16 ) ) ;
#70532 = CARTESIAN_POINT ( 'NONE',  ( 26.21990212871559933, 1440.913060396030005, 223.0271923088249935 ) ) ;
#70533 = CARTESIAN_POINT ( 'NONE',  ( 3.122055633242120098, 1424.574844735749821, 188.9232701594920059 ) ) ;
#70534 = EDGE_LOOP ( 'NONE', ( #36160, #251, #98227, #4283 ) ) ;
#70535 = CARTESIAN_POINT ( 'NONE',  ( -28.15442807850000051, 1509.896234805130007, 200.8410251444579728 ) ) ;
#70536 = AXIS2_PLACEMENT_3D ( 'NONE', #829, #26555, #286 ) ;
#70537 = CARTESIAN_POINT ( 'NONE',  ( 10.78168260516119936, 1461.896513113439823, 211.1674540152700104 ) ) ;
#70538 = CARTESIAN_POINT ( 'NONE',  ( -9.656302321220000096, 1486.131777580530070, 183.4210019581979907 ) ) ;
#70539 = CARTESIAN_POINT ( 'NONE',  ( -1.590879946456773775, 1526.333389947990099, 239.8456008596675133 ) ) ;
#70540 = CARTESIAN_POINT ( 'NONE',  ( -8.778933807423072722, 1427.705008372408884, 144.1938086916980524 ) ) ;
#70541 = CARTESIAN_POINT ( 'NONE',  ( 25.80166435820000004, 1469.242112528930193, 212.9326132565380192 ) ) ;
#70542 = CARTESIAN_POINT ( 'NONE',  ( -16.08688390367190379, 1420.213695813531103, 209.4851459447380080 ) ) ;
#70543 = CARTESIAN_POINT ( 'NONE',  ( -13.70965915470000063, 1507.817784722230044, 232.5379316308980151 ) ) ;
#70544 = CARTESIAN_POINT ( 'NONE',  ( -29.50517310080210365, 1383.842696339350141, 227.2997455133179869 ) ) ;
#70545 = CARTESIAN_POINT ( 'NONE',  ( -25.62237252300000279, 1435.677407238350042, 212.3102753037179866 ) ) ;
#70546 = CARTESIAN_POINT ( 'NONE',  ( 18.64588652299999794, 1416.828040475229955, 209.6843149956849857 ) ) ;
#70547 = FACE_OUTER_BOUND ( 'NONE', #16547, .T. ) ;
#70548 = CARTESIAN_POINT ( 'NONE',  ( 0.1618819747345350002, 1485.136375146799764, 181.8737203127180067 ) ) ;
#70550 = EDGE_LOOP ( 'NONE', ( #17182, #70637, #110787, #71321 ) ) ;
#70549 = CARTESIAN_POINT ( 'NONE',  ( 3.074703527060000052, 1441.333178254290033, 218.5515148082390056 ) ) ;
#70551 = CARTESIAN_POINT ( 'NONE',  ( -0.4299350981030000129, 1451.092099702930000, 182.2245401378979750 ) ) ;
#70552 = CARTESIAN_POINT ( 'NONE',  ( -8.601711843582590333, 1387.512598758959939, 200.1433781083956660 ) ) ;
#70553 = CARTESIAN_POINT ( 'NONE',  ( -4.557053783849999817, 1474.667304043090098, 199.0764274286989917 ) ) ;
#70554 = EDGE_CURVE ( 'NONE', #42052, #35207, #99020, .T. ) ;
#70556 = ORIENTED_EDGE ( 'NONE', *, *, #26068, .F. ) ;
#70555 = CARTESIAN_POINT ( 'NONE',  ( -32.54480841269623426, 1524.547873515804895, 217.0832791832422686 ) ) ;
#70557 = CARTESIAN_POINT ( 'NONE',  ( -6.059217065147319836, 1508.551704408389924, 219.4267866760630170 ) ) ;
#70558 = VERTEX_POINT ( 'NONE', #49206 ) ;
#70559 = B_SPLINE_SURFACE_WITH_KNOTS ( 'NONE', 5, 5, ( 
 ( #611, #84040, #76748, #51005, #7338, #67815 ),
 ( #16261, #50464, #60, #49353, #59971, #68375 ),
 ( #83481, #42048, #66722, #94086, #84588, #51553 ),
 ( #17356, #67271, #85688, #41502, #8985, #75116 ),
 ( #24114, #34741, #76200, #6775, #25216, #75661 ),
 ( #59420, #109803, #109263, #43157, #100297, #58305 ),
 ( #92427, #33082, #35295, #38467, #72644, #26902 ),
 ( #1165, #61624, #103602, #81027, #52114, #44266 ),
 ( #95756, #69480, #64251, #61091, #95206, #94645 ) ),
 .UNSPECIFIED., .F., .F., .F.,
 ( 6, 3, 6 ),
 ( 6, 6 ),
 ( 3.966463181890000023, 7.853302612130000249, 13.00030988960000045 ),
 ( 0.000000000000000000, 2.000000000000000000 ),
 .UNSPECIFIED. ) ;
#70560 = CARTESIAN_POINT ( 'NONE',  ( -13.49218435975080155, 1390.354837178909975, 211.7086340214200106 ) ) ;
#70561 = CARTESIAN_POINT ( 'NONE',  ( 12.27010794681469008, 1416.835807157242016, 223.5795575599114500 ) ) ;
#70562 = CARTESIAN_POINT ( 'NONE',  ( -3.034926079678273325, 1369.200812461397618, 207.6218459616989946 ) ) ;
#70563 = CARTESIAN_POINT ( 'NONE',  ( -2.265697975220000160, 1431.525679395089810, 217.2185296630090079 ) ) ;
#70564 = CARTESIAN_POINT ( 'NONE',  ( -10.24672469099380123, 1472.256837706050192, 207.1292450579819899 ) ) ;
#70565 = CARTESIAN_POINT ( 'NONE',  ( 14.89108873512989994, 1409.433068664470056, 210.2543917981890047 ) ) ;
#70566 = CARTESIAN_POINT ( 'NONE',  ( 6.763640255447179445E-10, 1465.118916387369836, 238.1343321182859825 ) ) ;
#70567 = CARTESIAN_POINT ( 'NONE',  ( -96.20702463676329330, 1385.210891181070110, 295.3517524571470290 ) ) ;
#70568 = CARTESIAN_POINT ( 'NONE',  ( -17.30242272219999933, 1430.613991027629936, 191.1830775443980031 ) ) ;
#70569 = CARTESIAN_POINT ( 'NONE',  ( 9.612801490498689816, 1424.761641057829820, 208.8539646045889810 ) ) ;
#70570 = ORIENTED_EDGE ( 'NONE', *, *, #88439, .T. ) ;
#70571 = DIRECTION ( 'NONE',  ( 0.9810655946269050132, 0.06469995582470079720, 0.1825492118735090041 ) ) ;
#70573 = EDGE_LOOP ( 'NONE', ( #76639, #69725 ) ) ;
#70572 = CARTESIAN_POINT ( 'NONE',  ( -2.370970874524634286, 1427.002265528474027, 134.0999999980979567 ) ) ;
#70574 = VERTEX_POINT ( 'NONE', #39686 ) ;
#70576 = CIRCLE ( 'NONE', #65212, 2.000000000029146907 ) ;
#70575 = CARTESIAN_POINT ( 'NONE',  ( 7.443246446248299009, 1423.092341332710021, 195.6161848952980051 ) ) ;
#70577 = CARTESIAN_POINT ( 'NONE',  ( -5.403726144051158364, 1363.053751466317181, 208.3718459617061285 ) ) ;
#70578 = CARTESIAN_POINT ( 'NONE',  ( -0.9569096709085479491, 1496.314324137450058, 196.8078323967840220 ) ) ;
#70579 = CARTESIAN_POINT ( 'NONE',  ( 5.512104717576124635, 1471.237629144492075, 269.3375989710273188 ) ) ;
#70580 = CARTESIAN_POINT ( 'NONE',  ( -30.31404213106216972, 1524.330813522192102, 221.7920027509183001 ) ) ;
#70581 = CARTESIAN_POINT ( 'NONE',  ( -14.55278341820000065, 1420.461940006850000, 213.8336615198890058 ) ) ;
#70582 = CARTESIAN_POINT ( 'NONE',  ( 32.22536377336272295, 1523.621879633028584, 201.4085774011528542 ) ) ;
#70583 = CARTESIAN_POINT ( 'NONE',  ( 4.353674023710000007, 1446.914190579090018, 199.8745573264090183 ) ) ;
#70584 = CARTESIAN_POINT ( 'NONE',  ( 0.1857455191719999954, 1471.145214114130113, 182.4746948879979982 ) ) ;
#70585 = CARTESIAN_POINT ( 'NONE',  ( -6.711617847637158185, 1369.367247958655753, 207.6218459616987673 ) ) ;
#70586 = DIRECTION ( 'NONE',  ( 0.7414773880254614813, 0.000000000000000000, -0.6709778558543786353 ) ) ;
#70587 = ADVANCED_FACE ( 'NONE', ( #40231 ), #22296, .F. ) ;
#70588 = CARTESIAN_POINT ( 'NONE',  ( -1.136547623115000016, 1516.839862955080207, 206.6438706166370025 ) ) ;
#70589 = LINE ( 'NONE', #53794, #37602 ) ;
#70590 = B_SPLINE_SURFACE_WITH_KNOTS ( 'NONE', 5, 5, ( 
 ( #14890, #48529, #58579, #75917, #5960, #109524, #40105, #83763, #7604 ),
 ( #23292, #49081, #108417, #50716, #41215, #110069, #83216, #23837, #84845 ),
 ( #91613, #84312, #108975, #74287, #59139, #6505, #101640, #40659, #93261 ),
 ( #16525, #76467, #110619, #66984, #31701, #68097, #92707, #56924, #50186 ),
 ( #91054, #74832, #100557, #58029, #92164, #7060, #1996, #77579, #78117 ),
 ( #26038, #96026, #27174, #19297, #79244, #9270, #35561, #102742, #61908 ),
 ( #51833, #43430, #69191, #25490, #340, #42876, #52939, #59681, #68642 ),
 ( #10361, #60801, #87076, #36131, #78679, #8695, #17628, #2552, #60231 ),
 ( #93793, #69757, #70315, #102210, #94350, #85970, #887, #35010, #87642 ) ),
 .UNSPECIFIED., .F., .F., .F.,
 ( 6, 3, 6 ),
 ( 6, 3, 6 ),
 ( 4.947986407769999317, 8.870455474829999076, 10.02594095490000115 ),
 ( 0.000000000000000000, 1.000000000000000000, 2.000000000000000000 ),
 .UNSPECIFIED. ) ;
#70591 = CARTESIAN_POINT ( 'NONE',  ( 3.550311703873260096E-15, 1384.899971913130003, 209.1218459572589836 ) ) ;
#70592 = FACE_OUTER_BOUND ( 'NONE', #83664, .T. ) ;
#70593 = CARTESIAN_POINT ( 'NONE',  ( -2.667618532240000118, 1496.805265767590072, 220.8079931561990179 ) ) ;
#70594 = CARTESIAN_POINT ( 'NONE',  ( -103.5801209296959939, 1379.883073482990085, 303.9981235976169955 ) ) ;
#70595 = ORIENTED_EDGE ( 'NONE', *, *, #85022, .T. ) ;
#70596 = CARTESIAN_POINT ( 'NONE',  ( 27.41410076250000216, 1415.612337104729932, 262.1295773258979693 ) ) ;
#70597 = CARTESIAN_POINT ( 'NONE',  ( -25.66628087289999982, 1469.241412583229931, 204.8365099310479991 ) ) ;
#70599 = CARTESIAN_POINT ( 'NONE',  ( 17.21791179325979826, 1410.146180600570005, 192.5803812474509868 ) ) ;
#70598 = CARTESIAN_POINT ( 'NONE',  ( -10.89878236088929953, 1426.095048252110246, 91.95250234051970040 ) ) ;
#70600 = CARTESIAN_POINT ( 'NONE',  ( 3.268235720634999897, 1516.890356958860139, 211.9874346545169885 ) ) ;
#70601 = CARTESIAN_POINT ( 'NONE',  ( 16.83374205149999980, 1433.582731286290027, 217.5197046195389987 ) ) ;
#70602 = DIRECTION ( 'NONE',  ( -1.000000000000000000, -2.220446049250313081E-13, 0.000000000000000000 ) ) ;
#70603 = CARTESIAN_POINT ( 'NONE',  ( -27.90885395119999757, 1424.419860134829833, 250.2249407852980028 ) ) ;
#70604 = CARTESIAN_POINT ( 'NONE',  ( 20.55662018261149981, 1509.675015189930036, 230.6199700381970104 ) ) ;
#70605 = CARTESIAN_POINT ( 'NONE',  ( 29.21489664454900037, 1509.775817163060083, 209.5928712634359954 ) ) ;
#70606 = CARTESIAN_POINT ( 'NONE',  ( -5.032977198260000229, 1391.805267112089950, 214.4361776263990009 ) ) ;
#70607 = CARTESIAN_POINT ( 'NONE',  ( -22.70509189929999749, 1409.705932116229860, 208.9454376012710100 ) ) ;
#70608 = ORIENTED_EDGE ( 'NONE', *, *, #103466, .F. ) ;
#70609 = CARTESIAN_POINT ( 'NONE',  ( 7.793403662019999345, 1494.414358568890066, 218.7662867540790046 ) ) ;
#70610 = CARTESIAN_POINT ( 'NONE',  ( 15.09731849065486387, 1514.821748426677459, 225.1372258183207862 ) ) ;
#70611 = CARTESIAN_POINT ( 'NONE',  ( -16.64514777280000146, 1458.767275973729966, 229.9812677959979794 ) ) ;
#70612 = ORIENTED_EDGE ( 'NONE', *, *, #57263, .T. ) ;
#70613 = ORIENTED_EDGE ( 'NONE', *, *, #52925, .F. ) ;
#70614 = AXIS2_PLACEMENT_3D ( 'NONE', #96242, #36325, #18401 ) ;
#70615 = CARTESIAN_POINT ( 'NONE',  ( 8.972797426533400511, 1452.010477424879809, 211.5435742291749932 ) ) ;
#70616 = DIRECTION ( 'NONE',  ( 0.9510565162951566398, 0.000000000000000000, -0.3090169943749382919 ) ) ;
#70617 = ORIENTED_EDGE ( 'NONE', *, *, #34951, .F. ) ;
#70618 = CARTESIAN_POINT ( 'NONE',  ( -0.7271388932819999873, 1419.324264331729864, 184.7252148951980075 ) ) ;
#70619 = CARTESIAN_POINT ( 'NONE',  ( -6.488391801617740207, 1419.348173448909165, 195.1544855266193395 ) ) ;
#70620 = AXIS2_PLACEMENT_3D ( 'NONE', #87436, #1795, #70115 ) ;
#70621 = DIRECTION ( 'NONE',  ( -1.755985294532469921E-16, 1.000000000000000000, -1.338183447452831989E-16 ) ) ;
#70622 = AXIS2_PLACEMENT_3D ( 'NONE', #82641, #41185, #21603 ) ;
#70623 = CARTESIAN_POINT ( 'NONE',  ( 27.27513885906573776, 1509.144913387980750, 206.1795252833925929 ) ) ;
#70624 = CARTESIAN_POINT ( 'NONE',  ( 1.410687896538389996, 1420.916877493199991, 183.0185646639909862 ) ) ;
#70625 = EDGE_CURVE ( 'NONE', #106056, #98544, #95425, .T. ) ;
#70626 = CARTESIAN_POINT ( 'NONE',  ( 9.370963865242019963, 1451.172249539200038, 208.3746166689639949 ) ) ;
#70627 = EDGE_CURVE ( 'NONE', #70893, #66058, #52589, .T. ) ;
#70628 = FACE_OUTER_BOUND ( 'NONE', #77491, .T. ) ;
#70629 = CARTESIAN_POINT ( 'NONE',  ( 13.75454463520000026, 1463.783809604629823, 225.0383857723980157 ) ) ;
#70630 = ORIENTED_EDGE ( 'NONE', *, *, #59619, .F. ) ;
#70631 = CARTESIAN_POINT ( 'NONE',  ( -4.036748876935000396, 1516.667393516340098, 202.1854475764570225 ) ) ;
#70632 = CARTESIAN_POINT ( 'NONE',  ( -6.550870182235000172, 1516.727502608469877, 209.8762341530540141 ) ) ;
#70633 = VERTEX_POINT ( 'NONE', #13908 ) ;
#70635 = ADVANCED_FACE ( 'NONE', ( #31829 ), #58979, .T. ) ;
#70634 = CARTESIAN_POINT ( 'NONE',  ( 11.86610049460949945, 1432.336025080309810, 149.9824239092829998 ) ) ;
#70636 = CYLINDRICAL_SURFACE ( 'NONE', #24750, 0.5000000000000005551 ) ;
#70637 = ORIENTED_EDGE ( 'NONE', *, *, #67475, .T. ) ;
#70638 = CARTESIAN_POINT ( 'NONE',  ( 9.908006808964964662, 1424.402993806118047, 139.1388889620660052 ) ) ;
#70639 = EDGE_CURVE ( 'NONE', #32152, #81044, #110760, .T. ) ;
#70640 = CARTESIAN_POINT ( 'NONE',  ( -7.679361995703810173, 1508.551704408399928, 219.1247835820369971 ) ) ;
#70641 = CARTESIAN_POINT ( 'NONE',  ( -17.06003757377249741, 1420.270326980760046, 204.0766453804359912 ) ) ;
#70642 = ADVANCED_FACE ( 'NONE', ( #66016 ), #31278, .T. ) ;
#70643 = CARTESIAN_POINT ( 'NONE',  ( -2.130647964720339793, 1467.954295551920040, 220.0452685800179893 ) ) ;
#70644 = CARTESIAN_POINT ( 'NONE',  ( 21.97362714515480064, 1452.145724418900045, 140.5458991228840091 ) ) ;
#70645 = CARTESIAN_POINT ( 'NONE',  ( 4.128048954824370398, 1410.178378922490083, 269.8667681920509835 ) ) ;
#70646 = CARTESIAN_POINT ( 'NONE',  ( -3.897009771321176874, 1517.051704408389924, 187.2231132109079113 ) ) ;
#70647 = CARTESIAN_POINT ( 'NONE',  ( -110.0494255671617054, 1384.394578747806008, 296.9720231736403662 ) ) ;
#70648 = CARTESIAN_POINT ( 'NONE',  ( 7.882820024130000824, 1493.775712921889863, 217.5949005480990195 ) ) ;
#70649 = CARTESIAN_POINT ( 'NONE',  ( -30.44593040359999847, 1379.623838566320273, 214.2479615521790208 ) ) ;
#70650 = DIRECTION ( 'NONE',  ( -0.9417419115949053898, -0.3363363969979660806, -9.559255346349042767E-16 ) ) ;
#70651 = EDGE_CURVE ( 'NONE', #56488, #101252, #12821, .T. ) ;
#70653 = DIRECTION ( 'NONE',  ( 1.000000000000000000, 2.249639673992789970E-32, 1.224646799147350002E-16 ) ) ;
#70652 = CARTESIAN_POINT ( 'NONE',  ( -18.26060618049999817, 1504.473730909189953, 209.2482098315410042 ) ) ;
#70654 = CARTESIAN_POINT ( 'NONE',  ( -21.80201530938867549, 1379.715454459142848, 213.3549729146243976 ) ) ;
#70655 = APPLICATION_CONTEXT ( 'automotive_design' ) ;
#70656 = CARTESIAN_POINT ( 'NONE',  ( -9.920924821321568388, 1439.719005343529943, 207.8524026893080077 ) ) ;
#70657 = CARTESIAN_POINT ( 'NONE',  ( -7.213837406734999291, 1512.784460098840100, 202.2559763233970216 ) ) ;
#70658 = EDGE_LOOP ( 'NONE', ( #34378, #85515, #47603, #74568, #42337 ) ) ;
#70659 = CARTESIAN_POINT ( 'NONE',  ( 11.06589456070000033, 1424.668795903030286, 234.3916895905979629 ) ) ;
#70660 = CARTESIAN_POINT ( 'NONE',  ( 40.27308693906149273, 1443.611999474700042, 137.1163322506119755 ) ) ;
#70661 = CARTESIAN_POINT ( 'NONE',  ( -56.62033099439780415, 1385.083666504650182, 274.9067868046199692 ) ) ;
#70662 = B_SPLINE_CURVE_WITH_KNOTS ( 'NONE', 5,
 ( #108796, #32087, #89241, #12537, #46716, #80846, #98184, #4150, #38277, #106590, #59510, #91989, #33726, #67918, #24218 ),
 .UNSPECIFIED., .F., .F.,
 ( 6, 3, 3, 3, 6 ),
 ( 0.000000000000000000, 0.1200153949226330508, 0.2400307898452661015, 0.4800615796854195150, 1.000000000000000000 ),
 .UNSPECIFIED. ) ;
#70663 = CARTESIAN_POINT ( 'NONE',  ( -21.11882185303258908, 1525.651285554113201, 233.3142527378166164 ) ) ;
#70664 = AXIS2_PLACEMENT_3D ( 'NONE', #38218, #71881, #47731 ) ;
#70665 = CARTESIAN_POINT ( 'NONE',  ( 3.725765543819999692, 1506.045642329989960, 220.5640007132990092 ) ) ;
#70666 = CARTESIAN_POINT ( 'NONE',  ( -15.10310828839999964, 1416.172775391969935, 212.2626019875489760 ) ) ;
#70667 = EDGE_CURVE ( 'NONE', #74815, #48606, #21746, .T. ) ;
#70669 = ORIENTED_EDGE ( 'NONE', *, *, #48875, .F. ) ;
#70668 = CARTESIAN_POINT ( 'NONE',  ( 1.621556534070299982, 1515.068963820189992, 204.7925064057230031 ) ) ;
#70670 = CARTESIAN_POINT ( 'NONE',  ( -17.16683859837399950, 1418.026022597180145, 204.8288321923220110 ) ) ;
#70671 = DIRECTION ( 'NONE',  ( 0.000000000000000000, 1.000000000000000000, -1.836970198721029688E-16 ) ) ;
#70672 = CARTESIAN_POINT ( 'NONE',  ( -15.85592065860000055, 1415.880107938199899, 209.4912318213870037 ) ) ;
#70673 = CARTESIAN_POINT ( 'NONE',  ( 11.35635713053500062, 1512.376261820769969, 225.3263167562670048 ) ) ;
#70674 = CARTESIAN_POINT ( 'NONE',  ( 1.804213505530000150, 1410.351307731129964, 232.1928988982980115 ) ) ;
#70675 = EDGE_CURVE ( 'NONE', #9501, #77376, #55372, .T. ) ;
#70676 = CARTESIAN_POINT ( 'NONE',  ( 13.05502264250409894, 1509.382255964980004, 181.3091698393539843 ) ) ;
#70677 = CARTESIAN_POINT ( 'NONE',  ( 13.73040296012064587, 1519.551704408389924, 227.6346699041483816 ) ) ;
#70678 = CARTESIAN_POINT ( 'NONE',  ( -4.561655832029999580, 1453.313060387329870, 228.9334036006980000 ) ) ;
#70679 = ADVANCED_FACE ( 'NONE', ( #93382 ), #34745, .T. ) ;
#70680 = CARTESIAN_POINT ( 'NONE',  ( 4.387294391120000192, 1412.734080688830090, 231.5195920807979917 ) ) ;
#70681 = CARTESIAN_POINT ( 'NONE',  ( -4.772433264290000032, 1461.586210710390105, 228.1254610687989839 ) ) ;
#70682 = CARTESIAN_POINT ( 'NONE',  ( -16.16546996768000000, 1459.158286300486225, 229.6201364928280100 ) ) ;
#70683 = CARTESIAN_POINT ( 'NONE',  ( 7.709032137684999952, 1516.534320418310244, 206.6366287381669906 ) ) ;
#70684 = CARTESIAN_POINT ( 'NONE',  ( 39.36363609779999706, 1422.502404882930023, 266.6143061720980540 ) ) ;
#70685 = CARTESIAN_POINT ( 'NONE',  ( -30.99338347248342629, 1526.382868172863937, 218.3719692838073740 ) ) ;
#70686 = CARTESIAN_POINT ( 'NONE',  ( 20.76830133009999813, 1436.454188401799911, 144.6138742496980001 ) ) ;
#70687 = EDGE_CURVE ( 'NONE', #81018, #36007, #21792, .T. ) ;
#70688 = CARTESIAN_POINT ( 'NONE',  ( 25.79183385109999804, 1488.578147155629949, 204.4850554393780158 ) ) ;
#70689 = CARTESIAN_POINT ( 'NONE',  ( 29.64936652346687040, 1509.975957225338334, 207.7724523241800227 ) ) ;
#70690 = DIRECTION ( 'NONE',  ( 1.755985294532464991E-16, -1.000000000000000000, 1.338183447452830017E-16 ) ) ;
#70691 = CARTESIAN_POINT ( 'NONE',  ( 12.73048906530000046, 1416.839648764230105, 223.1309759826980041 ) ) ;
#70692 = CARTESIAN_POINT ( 'NONE',  ( -9.269106418329268848, 1384.253990364469928, 197.9928380864789972 ) ) ;
#70693 =( BOUNDED_CURVE ( )  B_SPLINE_CURVE ( 3, ( #31805, #16084, #14986, #65994 ),
 .UNSPECIFIED., .F., .F. ) 
 B_SPLINE_CURVE_WITH_KNOTS ( ( 4, 4 ),
 ( 2.436781329611986457, 3.141592653589793116 ),
 .UNSPECIFIED. ) 
 CURVE ( )  GEOMETRIC_REPRESENTATION_ITEM ( )  RATIONAL_B_SPLINE_CURVE ( ( 1.000000000000000000, 0.9590300661663091475, 0.9590300661663091475, 1.000000000000000000 ) ) 
 REPRESENTATION_ITEM ( '' )  );
#70694 = CARTESIAN_POINT ( 'NONE',  ( -33.92723575372020406, 1435.682266284350135, 135.5036441057579850 ) ) ;
#70695 = CARTESIAN_POINT ( 'NONE',  ( -6.232532107092660034, 1407.162969920749902, 197.7132727041200155 ) ) ;
#70696 = CARTESIAN_POINT ( 'NONE',  ( -16.32914645889999861, 1414.913060387329779, 205.8850555510879872 ) ) ;
#70697 = CARTESIAN_POINT ( 'NONE',  ( -14.11670454040000067, 1442.569783380919944, 188.7198005640980227 ) ) ;
#70698 = CARTESIAN_POINT ( 'NONE',  ( -27.82104174381949946, 1508.416260427059797, 210.5121804756579991 ) ) ;
#70699 = CARTESIAN_POINT ( 'NONE',  ( -32.75718130879999990, 1436.536627606989896, 136.5459210844979907 ) ) ;
#70700 = DIRECTION ( 'NONE',  ( 0.6709778558543747495, 0.000000000000000000, 0.7414773880254650340 ) ) ;
#70701 = ORIENTED_EDGE ( 'NONE', *, *, #39094, .F. ) ;
#70702 = CARTESIAN_POINT ( 'NONE',  ( -2.701540413345000058, 1511.422242621320265, 201.5466790130070081 ) ) ;
#70703 = CARTESIAN_POINT ( 'NONE',  ( -11.51995628840010077, 1409.315346125450105, 218.6443785118009941 ) ) ;
#70704 = CARTESIAN_POINT ( 'NONE',  ( -13.27281985135759967, 1508.551708237569983, 210.0518082456389948 ) ) ;
#70705 = CARTESIAN_POINT ( 'NONE',  ( -4.785434006952626440, 1421.795252747364430, 137.9170229470215077 ) ) ;
#70706 = CARTESIAN_POINT ( 'NONE',  ( -45.88373572799999778, 1440.913038273419943, 266.4124089069979391 ) ) ;
#70707 = CARTESIAN_POINT ( 'NONE',  ( -12.87561223598270033, 1428.667272998819954, 222.5140706137790119 ) ) ;
#70708 = CARTESIAN_POINT ( 'NONE',  ( 0.3028733268543740142, 1419.325029753159924, 184.5281611957330199 ) ) ;
#70709 = CARTESIAN_POINT ( 'NONE',  ( 20.21716934225403506, 1526.104292489126237, 233.6939662645254430 ) ) ;
#70710 = CARTESIAN_POINT ( 'NONE',  ( -78.31511690615438681, 1384.642162581499861, 302.6921158508910139 ) ) ;
#70711 = CARTESIAN_POINT ( 'NONE',  ( -45.64952612643359231, 1385.004992914349941, 219.1277060083630204 ) ) ;
#70712 = CARTESIAN_POINT ( 'NONE',  ( 17.30207205515339908, 1423.280328764439901, 226.7191613964260171 ) ) ;
#70713 = CARTESIAN_POINT ( 'NONE',  ( 20.59646478119999813, 1507.764133386629965, 227.7125276174979831 ) ) ;
#70714 = CARTESIAN_POINT ( 'NONE',  ( 13.88564761750000009, 1452.412735684230029, 223.2422962839980016 ) ) ;
#70715 = EDGE_CURVE ( 'NONE', #237, #65949, #78668, .T. ) ;
#70716 = CARTESIAN_POINT ( 'NONE',  ( -26.87108745762090223, 1495.338653855599887, 210.8366527536690000 ) ) ;
#70717 = CARTESIAN_POINT ( 'NONE',  ( 4.363122683464830232, 1421.971318488559973, 183.8271341761570170 ) ) ;
#70718 = CARTESIAN_POINT ( 'NONE',  ( -8.371048524560000814, 1384.932744135109942, 199.7749417901490006 ) ) ;
#70720 = CARTESIAN_POINT ( 'NONE',  ( -3.657993755839999750, 1474.872004365689918, 218.7367895275489786 ) ) ;
#70719 = CIRCLE ( 'NONE', #27751, 1.000000000000003553 ) ;
#70721 = ADVANCED_FACE ( 'NONE', ( #25617 ), #7095, .F. ) ;
#70722 = CARTESIAN_POINT ( 'NONE',  ( 12.97490827640000077, 1414.913060387329779, 197.6684973124980047 ) ) ;
#70723 = CARTESIAN_POINT ( 'NONE',  ( -12.77426335350000031, 1416.547221146729953, 195.3312399645980122 ) ) ;
#70724 = CARTESIAN_POINT ( 'NONE',  ( 1.918627788879999851, 1422.032892955219950, 193.7879044333990066 ) ) ;
#70725 = CARTESIAN_POINT ( 'NONE',  ( 22.50049573229999922, 1409.698795012430082, 211.8242440451179789 ) ) ;
#70726 = B_SPLINE_SURFACE_WITH_KNOTS ( 'NONE', 5, 5, ( 
 ( #2490, #55088, #89216, #72435, #106029, #63502 ),
 ( #37166, #38252, #87578, #98156, #89761, #95963 ),
 ( #71361, #53431, #80820, #13032, #88132, #104921 ),
 ( #46144, #46689, #88681, #47220, #20890, #29853 ),
 ( #81346, #11958, #36068, #19224, #105474, #37712 ),
 ( #28762, #97622, #10866, #79183, #28206, #4127 ) ),
 .UNSPECIFIED., .F., .F., .F.,
 ( 6, 6 ),
 ( 6, 6 ),
 ( 30.32814665369999929, 157.7108139869999945 ),
 ( -1.942890293099999814E-16, 1.000000000000000000 ),
 .UNSPECIFIED. ) ;
#70727 = CARTESIAN_POINT ( 'NONE',  ( -12.89608512423069975, 1434.724840024559853, 149.2206170422699927 ) ) ;
#70728 = CARTESIAN_POINT ( 'NONE',  ( 8.204285602689999735, 1462.106119291689993, 228.8664411563990200 ) ) ;
#70729 = CARTESIAN_POINT ( 'NONE',  ( -5.360152366205530150, 1422.242722016050038, 144.1549655170190078 ) ) ;
#70731 = CARTESIAN_POINT ( 'NONE',  ( -21.62164173326539895, 1517.051704408389924, 210.2163513712909833 ) ) ;
#70730 = CARTESIAN_POINT ( 'NONE',  ( -11.30788591870000204, 1432.727006032190047, 151.5212569347980036 ) ) ;
#70732 = CARTESIAN_POINT ( 'NONE',  ( 1.069243730569999995, 1410.308942135029838, 232.9260189513979924 ) ) ;
#70733 = FACE_OUTER_BOUND ( 'NONE', #32063, .T. ) ;
#70734 = CARTESIAN_POINT ( 'NONE',  ( -12.21915924449999835, 1490.155271298389835, 209.9311082064550078 ) ) ;
#70735 = CARTESIAN_POINT ( 'NONE',  ( -23.09493868299999875, 1420.935639543630032, 211.5389171420879961 ) ) ;
#70736 = CARTESIAN_POINT ( 'NONE',  ( -9.328535443860001664, 1363.278783432129785, 210.6218459616991936 ) ) ;
#70737 = EDGE_CURVE ( 'NONE', #345, #25915, #16110, .T. ) ;
#70738 = CARTESIAN_POINT ( 'NONE',  ( 6.936398355645000180, 1516.667393516340098, 205.0850970932970085 ) ) ;
#70740 = CARTESIAN_POINT ( 'NONE',  ( -21.78276816909999880, 1430.096355600930110, 220.5348153272979914 ) ) ;
#70739 = B_SPLINE_CURVE_WITH_KNOTS ( 'NONE', 5,
 ( #56627, #21874, #65586, #30854, #82374, #21331 ),
 .UNSPECIFIED., .F., .F.,
 ( 6, 6 ),
 ( 0.000000000000000000, 1.000000000000000000 ),
 .UNSPECIFIED. ) ;
#70741 = CARTESIAN_POINT ( 'NONE',  ( -19.06789788857610191, 1485.490801430430110, 189.6154567045299757 ) ) ;
#70742 = CARTESIAN_POINT ( 'NONE',  ( -4.255035861773739825, 1441.293950967729870, 160.2601193279770087 ) ) ;
#70744 = ORIENTED_EDGE ( 'NONE', *, *, #16871, .T. ) ;
#70743 = CARTESIAN_POINT ( 'NONE',  ( -67.12659018946959577, 1379.744665315070051, 278.1807872282039966 ) ) ;
#70745 = ORIENTED_EDGE ( 'NONE', *, *, #99362, .F. ) ;
#70746 = CARTESIAN_POINT ( 'NONE',  ( 11.93532877116399860, 1433.536986264360166, 150.1921723446900216 ) ) ;
#70747 = CARTESIAN_POINT ( 'NONE',  ( 26.60746491089999921, 1509.169831192730044, 216.8088406937480102 ) ) ;
#70748 = ORIENTED_EDGE ( 'NONE', *, *, #29551, .T. ) ;
#70749 = CARTESIAN_POINT ( 'NONE',  ( -105.2954588910000098, 1379.016081903610029, 304.6073168026589997 ) ) ;
#70750 = CARTESIAN_POINT ( 'NONE',  ( 11.16012950169999840, 1500.726265256889974, 206.0864327037589874 ) ) ;
#70752 = CARTESIAN_POINT ( 'NONE',  ( 13.79159911834929986, 1453.017954755449864, 224.3209708394340112 ) ) ;
#70751 = CARTESIAN_POINT ( 'NONE',  ( -22.96901158596647008, 1519.551704408389924, 211.6943887467578236 ) ) ;
#70753 = CARTESIAN_POINT ( 'NONE',  ( 11.91321771470000002, 1435.943783413959864, 147.6429393588979906 ) ) ;
#70754 = B_SPLINE_CURVE_WITH_KNOTS ( 'NONE', 5,
 ( #4869, #39012, #73190, #59702, #100576, #93814, #84868, #110092, #84334 ),
 .UNSPECIFIED., .F., .F.,
 ( 6, 3, 6 ),
 ( 0.000000000000000000, 0.5677246447800281537, 1.000000000000000000 ),
 .UNSPECIFIED. ) ;
#70755 = EDGE_CURVE ( 'NONE', #98379, #42497, #93929, .T. ) ;
#70756 = CARTESIAN_POINT ( 'NONE',  ( -24.29770167611630072, 1452.000795570500031, 137.1838091970490154 ) ) ;
#70757 = CARTESIAN_POINT ( 'NONE',  ( 10.65455282579233298, 1438.738895160811580, 152.5347921806118734 ) ) ;
#70758 = CARTESIAN_POINT ( 'NONE',  ( 14.78239737450000035, 1410.801796610830252, 227.6257754451980020 ) ) ;
#70759 = CARTESIAN_POINT ( 'NONE',  ( 5.011678838024999472, 1516.989560013210166, 212.3778133565769792 ) ) ;
#70761 = AXIS2_PLACEMENT_3D ( 'NONE', #110649, #92744, #101129 ) ;
#70760 = CARTESIAN_POINT ( 'NONE',  ( 40.71250048023939883, 1447.497876396469792, 134.0999999984609872 ) ) ;
#70762 = CARTESIAN_POINT ( 'NONE',  ( -4.993214567250789493, 1391.653935164599716, 214.7089805434449943 ) ) ;
#70763 = CARTESIAN_POINT ( 'NONE',  ( 5425.877333011740120, 54.28084071072822780, 8448.741457639642249 ) ) ;
#70764 = ORIENTED_EDGE ( 'NONE', *, *, #10421, .F. ) ;
#70765 = CARTESIAN_POINT ( 'NONE',  ( 13.90749792064180035, 1435.812708943650023, 150.1213536925990297 ) ) ;
#70766 = EDGE_CURVE ( 'NONE', #110254, #78256, #1335, .T. ) ;
#70767 = CARTESIAN_POINT ( 'NONE',  ( 32.28466283162151029, 1501.977400791986611, 199.0684425896244250 ) ) ;
#70768 = VERTEX_POINT ( 'NONE', #50846 ) ;
#70769 = VERTEX_POINT ( 'NONE', #110743 ) ;
#70770 = ORIENTED_EDGE ( 'NONE', *, *, #83601, .T. ) ;
#70771 = CARTESIAN_POINT ( 'NONE',  ( -7.503873141484999287, 1512.035910181040208, 215.6868223634869821 ) ) ;
#70772 = CARTESIAN_POINT ( 'NONE',  ( -0.6774325393469999845, 1465.095555782530027, 238.0673157071979915 ) ) ;
#70773 = CARTESIAN_POINT ( 'NONE',  ( -13.74310390781900004, 1522.051704408389924, 201.1531303618569950 ) ) ;
#70774 = CARTESIAN_POINT ( 'NONE',  ( -8.023236032950000762, 1384.902848640620050, 218.7875340078090005 ) ) ;
#70775 = CARTESIAN_POINT ( 'NONE',  ( 10.14286467640000033, 1461.576202403990010, 208.9373515736710090 ) ) ;
#70776 = DIRECTION ( 'NONE',  ( -0.000000000000000000, 1.000000000000000000, -0.000000000000000000 ) ) ;
#70777 = CARTESIAN_POINT ( 'NONE',  ( -59.10983982511428536, 1379.721706864959515, 259.3694688010850200 ) ) ;
#70778 = CARTESIAN_POINT ( 'NONE',  ( 4.222531898828509433, 1446.229786520979815, 170.5365406785500113 ) ) ;
#70779 = ADVANCED_FACE ( 'NONE', ( #67664 ), #62855, .F. ) ;
#70780 = CARTESIAN_POINT ( 'NONE',  ( 12.42529224677512900, 1517.151704408390060, 202.6823640254548309 ) ) ;
#70781 = CARTESIAN_POINT ( 'NONE',  ( -0.7579844201469989606, 1516.883361325900069, 206.8353730456769881 ) ) ;
#70782 = ORIENTED_EDGE ( 'NONE', *, *, #97665, .F. ) ;
#70783 = CARTESIAN_POINT ( 'NONE',  ( 23.65006834624189835, 1440.913060387330006, 234.3338484623149895 ) ) ;
#70784 = CARTESIAN_POINT ( 'NONE',  ( -8.586954633810537876E-06, 1452.913060687297275, 152.6867136803564335 ) ) ;
#70785 = ADVANCED_FACE ( 'NONE', ( #1986 ), #23959, .F. ) ;
#70786 = EDGE_LOOP ( 'NONE', ( #53152, #76036 ) ) ;
#70787 = CARTESIAN_POINT ( 'NONE',  ( 26.10257120823780141, 1450.811424229450040, 136.5821829170589865 ) ) ;
#70788 = CARTESIAN_POINT ( 'NONE',  ( -14.27637756340000053, 1410.784304046130046, 190.3513780643979771 ) ) ;
#70789 = CARTESIAN_POINT ( 'NONE',  ( -57.28523240820543805, 1379.717557217216381, 260.4048635326923886 ) ) ;
#70791 = FACE_OUTER_BOUND ( 'NONE', #78214, .T. ) ;
#70790 = CARTESIAN_POINT ( 'NONE',  ( -24.67346689489999889, 1441.307773655729761, 210.6971997129480201 ) ) ;
#70792 = CARTESIAN_POINT ( 'NONE',  ( -1.673997294314879980, 1422.546829072329956, 192.5753128275750043 ) ) ;
#70793 = CARTESIAN_POINT ( 'NONE',  ( -18.89959486414000267, 1416.839692127460012, 207.5749783441650038 ) ) ;
#70794 = CARTESIAN_POINT ( 'NONE',  ( 10.79528402730720060, 1489.628194868570063, 207.4012257063180016 ) ) ;
#70795 = CARTESIAN_POINT ( 'NONE',  ( -11.94116563470000081, 1433.615379977029988, 149.2721031343980087 ) ) ;
#70796 = CARTESIAN_POINT ( 'NONE',  ( -2.360319324340000247, 1507.471933479789868, 221.3436898553990204 ) ) ;
#70797 = ADVANCED_FACE ( 'NONE', ( #81395 ), #58903, .T. ) ;
#70799 = CARTESIAN_POINT ( 'NONE',  ( 0.4156989469490010025, 1498.844189599989932, 200.5557808060589764 ) ) ;
#70798 = CARTESIAN_POINT ( 'NONE',  ( 4.561144869889999676, 1466.058506330530008, 233.9063445751979771 ) ) ;
#70800 = CARTESIAN_POINT ( 'NONE',  ( 3.261635932824999973, 1516.613881697390070, 216.0569793506570022 ) ) ;
#70801 = EDGE_CURVE ( 'NONE', #3002, #79909, #83977, .T. ) ;
#70802 = CARTESIAN_POINT ( 'NONE',  ( -31.93052144186258445, 1525.394057003703438, 217.0185065382337655 ) ) ;
#70803 = ADVANCED_FACE ( 'NONE', ( #4707 ), #84775, .T. ) ;
#70804 = CARTESIAN_POINT ( 'NONE',  ( 5.689538361743419870, 1510.689985724130111, 216.6800952772849769 ) ) ;
#70805 = CARTESIAN_POINT ( 'NONE',  ( -3.487592467065000257, 1509.038615934169911, 213.6090957241370063 ) ) ;
#70806 = CARTESIAN_POINT ( 'NONE',  ( -7.322105105754999954, 1516.572193931679976, 211.9951753309869957 ) ) ;
#70807 = CIRCLE ( 'NONE', #77945, 1.999999999999998446 ) ;
#70808 = CARTESIAN_POINT ( 'NONE',  ( -14.44303134326499993, 1516.995662938509895, 225.7915129991669971 ) ) ;
#70809 = CARTESIAN_POINT ( 'NONE',  ( 30.12442103006196348, 1524.524650307242382, 222.3821565184462372 ) ) ;
#70811 = ORIENTED_EDGE ( 'NONE', *, *, #65090, .F. ) ;
#70810 = CARTESIAN_POINT ( 'NONE',  ( -102.7371261779999969, 1386.485993092710032, 311.2182069122590065 ) ) ;
#70812 = CARTESIAN_POINT ( 'NONE',  ( -16.48400364723607936, 1525.790286462510494, 236.4799666439590169 ) ) ;
#70813 = CARTESIAN_POINT ( 'NONE',  ( 31.95512683039999757, 1440.913060382470121, 244.1805851198980122 ) ) ;
#70814 = CARTESIAN_POINT ( 'NONE',  ( -11.71397076299980000, 1489.483175994190105, 212.5377881273170146 ) ) ;
#70815 = CARTESIAN_POINT ( 'NONE',  ( -15.29584542989999996, 1415.909343553620147, 206.6854934211490047 ) ) ;
#70816 = CARTESIAN_POINT ( 'NONE',  ( 2.921131793919999886, 1415.930151872029910, 231.8786077231980016 ) ) ;
#70817 = ADVANCED_FACE ( 'NONE', ( #63018 ), #9737, .T. ) ;
#70818 = CARTESIAN_POINT ( 'NONE',  ( -19.22340757710000148, 1456.313295594730107, 227.1916260328980002 ) ) ;
#70820 = CARTESIAN_POINT ( 'NONE',  ( 19.24165877509999945, 1455.917582588630239, 226.0685302825979761 ) ) ;
#70819 = CARTESIAN_POINT ( 'NONE',  ( 11.87111128170000107, 1432.721370721239964, 150.3961584458980099 ) ) ;
#70821 = CARTESIAN_POINT ( 'NONE',  ( 0.04599154778319999859, 1434.818091166349859, 190.1711483882980076 ) ) ;
#70822 = CARTESIAN_POINT ( 'NONE',  ( -105.6030581432469972, 1377.982187984739994, 305.0819089094490550 ) ) ;
#70823 = ORIENTED_EDGE ( 'NONE', *, *, #87834, .T. ) ;
#70824 = CARTESIAN_POINT ( 'NONE',  ( -6.557909920764999789, 1516.908489800550115, 203.3441005368270282 ) ) ;
#70825 = CARTESIAN_POINT ( 'NONE',  ( 1.333571497619999935, 1405.789322411930016, 268.4830616106980301 ) ) ;
#70826 = EDGE_CURVE ( 'NONE', #72142, #1895, #24887, .T. ) ;
#70827 = CARTESIAN_POINT ( 'NONE',  ( 1.842963895390000273, 1515.551704166990021, 213.1059277586890062 ) ) ;
#70828 = AXIS2_PLACEMENT_3D ( 'NONE', #52908, #10327, #44500 ) ;
#70829 = CARTESIAN_POINT ( 'NONE',  ( 30.41063212992060372, 1463.807241927210043, 269.9433037886050215 ) ) ;
#70830 = CARTESIAN_POINT ( 'NONE',  ( 5.388168580889999504, 1432.635621093390000, 154.6140392605979912 ) ) ;
#70831 = CARTESIAN_POINT ( 'NONE',  ( 3.159263275979999896, 1466.676511794390080, 219.3004963912989922 ) ) ;
#70832 = CARTESIAN_POINT ( 'NONE',  ( -36.99862439799500180, 1440.913060387569885, 254.6224166283950296 ) ) ;
#70833 = CARTESIAN_POINT ( 'NONE',  ( 36.42198593292390285, 1449.840865744850134, 136.2602280137270157 ) ) ;
#70834 = CARTESIAN_POINT ( 'NONE',  ( 2.397204011594943118, 1449.532271010019485, 154.4508081864954647 ) ) ;
#70835 = CARTESIAN_POINT ( 'NONE',  ( 1.180525396009999950, 1431.432006926090253, 200.4326319868589792 ) ) ;
#70836 = CARTESIAN_POINT ( 'NONE',  ( -15.92610956699463642, 1415.966321813838249, 209.5991204954336524 ) ) ;
#70837 = CARTESIAN_POINT ( 'NONE',  ( 25.00977876991279913, 1436.598012848749931, 137.9330263815630246 ) ) ;
#70838 = CARTESIAN_POINT ( 'NONE',  ( -18.75625549219999755, 1442.404531551690070, 208.2016858895329960 ) ) ;
#70839 = AXIS2_PLACEMENT_3D ( 'NONE', #74491, #57694, #109723 ) ;
#70840 =( BOUNDED_CURVE ( )  B_SPLINE_CURVE ( 3, ( #38566, #97919, #90067, #73851 ),
 .UNSPECIFIED., .F., .T. ) 
 B_SPLINE_CURVE_WITH_KNOTS ( ( 4, 4 ),
 ( 0.000000000000000000, 0.7048113239778113215 ),
 .UNSPECIFIED. ) 
 CURVE ( )  GEOMETRIC_REPRESENTATION_ITEM ( )  RATIONAL_B_SPLINE_CURVE ( ( 1.000000000000000000, 0.9590300661663084814, 0.9590300661663084814, 1.000000000000000000 ) ) 
 REPRESENTATION_ITEM ( '' )  );
#70841 = VERTEX_POINT ( 'NONE', #53486 ) ;
#70842 = CARTESIAN_POINT ( 'NONE',  ( 18.66420869458043796, 1526.382868172863937, 185.4599087859680537 ) ) ;
#70843 = CARTESIAN_POINT ( 'NONE',  ( 3.415182420970000354, 1486.712733516890239, 198.4695609272989998 ) ) ;
#70844 = LINE ( 'NONE', #104953, #88498 ) ;
#70845 = CARTESIAN_POINT ( 'NONE',  ( -0.2162292962460000134, 1476.076401974029977, 267.5371521268979791 ) ) ;
#70846 = CARTESIAN_POINT ( 'NONE',  ( 10.85845406881951192, 1424.793774302243946, 138.1921923613813590 ) ) ;
#70847 = CARTESIAN_POINT ( 'NONE',  ( 15.05358514859999985, 1410.831827802429871, 191.5175413050980069 ) ) ;
#70848 = CARTESIAN_POINT ( 'NONE',  ( -3.012147942673290224, 1448.270564837731172, 184.4771857188410138 ) ) ;
#70849 = CARTESIAN_POINT ( 'NONE',  ( -12.73211671072519913, 1384.883120266560127, 219.0473556928539836 ) ) ;
#70850 = CARTESIAN_POINT ( 'NONE',  ( -17.39559652730000039, 1414.988017874730076, 207.6227087713480159 ) ) ;
#70851 = CARTESIAN_POINT ( 'NONE',  ( 32.02808312589916540, 1512.187213306747481, 197.2787714533495489 ) ) ;
#70852 = CARTESIAN_POINT ( 'NONE',  ( 26.60255046156829906, 1435.426458939230088, 135.2844108396259912 ) ) ;
#70853 = CARTESIAN_POINT ( 'NONE',  ( -10.98175438394980041, 1396.296551700780128, 210.5364588383239948 ) ) ;
#70854 = CARTESIAN_POINT ( 'NONE',  ( -15.97230427090000049, 1420.722880863429964, 227.0315165930979902 ) ) ;
#70855 = CARTESIAN_POINT ( 'NONE',  ( -16.48341284556989805, 1409.589363928740113, 225.5757014958979880 ) ) ;
#70856 = CARTESIAN_POINT ( 'NONE',  ( 9.675350337739999418, 1433.447543843880112, 148.7453054530979841 ) ) ;
#70857 = ORIENTED_EDGE ( 'NONE', *, *, #89633, .F. ) ;
#70858 = CARTESIAN_POINT ( 'NONE',  ( -11.34054827985558944, 1501.996627661553475, 207.3924314934697293 ) ) ;
#70859 = CARTESIAN_POINT ( 'NONE',  ( 1.899651985450000025, 1408.979397696429942, 230.3912746812980004 ) ) ;
#70860 = CARTESIAN_POINT ( 'NONE',  ( -5.350997755189996319, 1484.262300443630920, 183.6825286484975095 ) ) ;
#70862 = CARTESIAN_POINT ( 'NONE',  ( -9.881667340448540671, 1438.678908226070007, 210.2323064812840130 ) ) ;
#70861 = CARTESIAN_POINT ( 'NONE',  ( 10.51778671589999803, 1425.368423570830146, 103.4445267086979925 ) ) ;
#70863 = CARTESIAN_POINT ( 'NONE',  ( -15.99169327979993405, 1409.471481020725832, 225.2129679076976174 ) ) ;
#70864 = CARTESIAN_POINT ( 'NONE',  ( -9.173748801299998590, 1450.559996510189876, 208.1432996479669839 ) ) ;
#70865 = CARTESIAN_POINT ( 'NONE',  ( 4.616899834755000320, 1517.050041317280147, 201.3993091674070115 ) ) ;
#70866 = CARTESIAN_POINT ( 'NONE',  ( 7.601709514279999524, 1425.061887899960084, 212.0249446704789875 ) ) ;
#70867 = CARTESIAN_POINT ( 'NONE',  ( 5.140094423509999011, 1436.845494339190054, 228.7442485628990028 ) ) ;
#70868 = CARTESIAN_POINT ( 'NONE',  ( 5.496790702980000276, 1508.067699050229976, 181.8679897695980117 ) ) ;
#70869 = CARTESIAN_POINT ( 'NONE',  ( 7.513264357029996177, 1375.413060387289988, 209.1218459572589836 ) ) ;
#70870 = CARTESIAN_POINT ( 'NONE',  ( -55.15136628130240837, 1379.936376804820156, 253.2598006625759695 ) ) ;
#70871 = CARTESIAN_POINT ( 'NONE',  ( 9.532517564019999057, 1366.286862064870093, 207.6218459616989946 ) ) ;
#70873 = ORIENTED_EDGE ( 'NONE', *, *, #13686, .T. ) ;
#70872 = CARTESIAN_POINT ( 'NONE',  ( 8.401749989260000717, 1454.595346029489974, 215.7321778818789824 ) ) ;
#70874 = ORIENTED_EDGE ( 'NONE', *, *, #918, .F. ) ;
#70875 = CIRCLE ( 'NONE', #97618, 28.41070217520000440 ) ;
#70876 = DIRECTION ( 'NONE',  ( 0.000000000000000000, 0.000000000000000000, 1.000000000000000000 ) ) ;
#70877 = CARTESIAN_POINT ( 'NONE',  ( -14.68857900839999964, 1409.425996869029859, 192.2200297474979891 ) ) ;
#70878 = CARTESIAN_POINT ( 'NONE',  ( 3.820260774390000039E-10, 1453.313060387329870, 228.7984261690980077 ) ) ;
#70879 = CARTESIAN_POINT ( 'NONE',  ( -7.853884020855000259, 1511.558654537720031, 212.4889000995470099 ) ) ;
#70881 = CARTESIAN_POINT ( 'NONE',  ( -2.056488256989999819, 1486.374418793230006, 181.7138485504979997 ) ) ;
#70880 = CARTESIAN_POINT ( 'NONE',  ( -7.587808279129999889, 1384.071260043419898, 219.0277729778390210 ) ) ;
#70882 = CARTESIAN_POINT ( 'NONE',  ( -1.997114497637953789, 1521.951704408389787, 229.8748770088220965 ) ) ;
#70883 = CARTESIAN_POINT ( 'NONE',  ( -2.528233502088980345, 1463.070495996789987, 199.6737502978820089 ) ) ;
#70884 = CARTESIAN_POINT ( 'NONE',  ( 22.47142205740000165, 1410.193803466230065, 206.7884343312579745 ) ) ;
#70885 = CARTESIAN_POINT ( 'NONE',  ( 35.07271181893440826, 1436.204584066430016, 136.2659483677949765 ) ) ;
#70886 = CARTESIAN_POINT ( 'NONE',  ( 8.750394133592571677, 1396.218630886179881, 215.8835450990220295 ) ) ;
#70887 = CARTESIAN_POINT ( 'NONE',  ( 12.20862189049999991, 1408.016881114429907, 215.8065031030079979 ) ) ;
#70888 = CARTESIAN_POINT ( 'NONE',  ( 5.741649384740319799E-05, 1405.716795532820015, 267.8539894883900274 ) ) ;
#70889 = CARTESIAN_POINT ( 'NONE',  ( 41.65810716170000205, 1443.954329772089977, 135.6863066689980144 ) ) ;
#70890 = ORIENTED_EDGE ( 'NONE', *, *, #42452, .T. ) ;
#70891 = CARTESIAN_POINT ( 'NONE',  ( -11.57667674939999891, 1432.352206966570066, 151.1966745221979807 ) ) ;
#70892 = CARTESIAN_POINT ( 'NONE',  ( 12.36054334989999859, 1442.536702532669779, 187.4076687437979842 ) ) ;
#70893 = VERTEX_POINT ( 'NONE', #63554 ) ;
#70894 = ORIENTED_EDGE ( 'NONE', *, *, #41795, .T. ) ;
#70895 = CARTESIAN_POINT ( 'NONE',  ( -3.589036755729999584, 1455.442922379190122, 200.3873980026590118 ) ) ;
#70896 = CARTESIAN_POINT ( 'NONE',  ( 1.748848150589999983, 1360.440694539920059, 207.6218459616989946 ) ) ;
#70897 = CARTESIAN_POINT ( 'NONE',  ( 1.132949076425000090, 1516.693851263360102, 214.1195642086070166 ) ) ;
#70898 = CARTESIAN_POINT ( 'NONE',  ( 5.160317800795000132, 1510.729589429620091, 216.6788758775169867 ) ) ;
#70899 = ORIENTED_EDGE ( 'NONE', *, *, #90545, .T. ) ;
#70900 = CARTESIAN_POINT ( 'NONE',  ( 5.440512190109999757, 1424.738065781850082, 191.9794586101990319 ) ) ;
#70901 = CARTESIAN_POINT ( 'NONE',  ( -85.54616801760001010, 1375.529499929939902, 296.2627734727589655 ) ) ;
#70902 = B_SPLINE_CURVE_WITH_KNOTS ( 'NONE', 5,
 ( #76727, #85666, #66157, #15681, #68357, #83460 ),
 .UNSPECIFIED., .F., .F.,
 ( 6, 6 ),
 ( 0.000000000000000000, 1.000000000000000000 ),
 .UNSPECIFIED. ) ;
#70903 = CARTESIAN_POINT ( 'NONE',  ( -105.8501189142269965, 1378.913060387460064, 303.4887780044520014 ) ) ;
#70904 = CARTESIAN_POINT ( 'NONE',  ( 4.029572640705000985, 1516.858649670339901, 205.0803734583570019 ) ) ;
#70905 = CARTESIAN_POINT ( 'NONE',  ( -21.43608950620000186, 1440.913060387330006, 225.1375979974980055 ) ) ;
#70906 = EDGE_CURVE ( 'NONE', #94116, #8387, #105934, .T. ) ;
#70907 = CARTESIAN_POINT ( 'NONE',  ( -94.50912602849999189, 1384.855827234549906, 294.8620370673590401 ) ) ;
#70908 = CARTESIAN_POINT ( 'NONE',  ( -1.128757599205000073, 1516.608208975040043, 201.4108789544669946 ) ) ;
#70909 = CARTESIAN_POINT ( 'NONE',  ( -7.764017288770000746, 1409.184185845429965, 229.1854234257980067 ) ) ;
#70910 = EDGE_CURVE ( 'NONE', #80823, #71507, #48425, .T. ) ;
#70912 = ORIENTED_EDGE ( 'NONE', *, *, #105169, .F. ) ;
#70911 = CARTESIAN_POINT ( 'NONE',  ( -4.219438975460000130, 1446.230224810899927, 183.1418051739979944 ) ) ;
#70913 = CARTESIAN_POINT ( 'NONE',  ( 2.500020115319840031, 1419.382923540379807, 144.1035841389490031 ) ) ;
#70914 = CARTESIAN_POINT ( 'NONE',  ( -25.61448129076210023, 1440.913060494739966, 219.7488153746120076 ) ) ;
#70915 = B_SPLINE_CURVE_WITH_KNOTS ( 'NONE', 5,
 ( #83747, #16511, #100543, #50701, #92693, #25474, #32786, #67525, #15422 ),
 .UNSPECIFIED., .F., .F.,
 ( 6, 3, 6 ),
 ( 0.000000000000000000, 0.4999976322456015643, 1.000000000000000000 ),
 .UNSPECIFIED. ) ;
#70916 = CARTESIAN_POINT ( 'NONE',  ( -2.105916231296855123, 1485.584842600218508, 182.5101088624064403 ) ) ;
#70917 = FACE_OUTER_BOUND ( 'NONE', #9560, .T. ) ;
#70919 = EDGE_CURVE ( 'NONE', #99476, #24021, #93784, .T. ) ;
#70918 = CARTESIAN_POINT ( 'NONE',  ( -25.54523398509999765, 1435.396131125720103, 135.6579912344979846 ) ) ;
#70920 = CARTESIAN_POINT ( 'NONE',  ( 43.61871776674129819, 1431.697620533069994, 269.9278503807960305 ) ) ;
#70921 = CARTESIAN_POINT ( 'NONE',  ( 7.337793712495000342, 1517.145312756229941, 211.9940546803969994 ) ) ;
#70922 = CARTESIAN_POINT ( 'NONE',  ( -65.88578210080000019, 1379.740759783769818, 274.2509442001589832 ) ) ;
#70923 = ADVANCED_FACE ( 'NONE', ( #47272 ), #93717, .F. ) ;
#70924 = CARTESIAN_POINT ( 'NONE',  ( -8.855566472366772857, 1426.236804904744531, 225.2812767048452827 ) ) ;
#70925 = CARTESIAN_POINT ( 'NONE',  ( -31.25789155969114219, 1523.954914175594695, 221.8935806748798711 ) ) ;
#70926 = CARTESIAN_POINT ( 'NONE',  ( -17.84104788077500103, 1489.004184077329910, 195.1797443787960162 ) ) ;
#70927 = CARTESIAN_POINT ( 'NONE',  ( 2.491655725414999800, 1516.977504706749869, 209.8569557413499922 ) ) ;
#70928 = EDGE_LOOP ( 'NONE', ( #5447, #71542, #75007, #50090 ) ) ;
#70929 = DIRECTION ( 'NONE',  ( -1.000000000000000000, 0.000000000000000000, 0.000000000000000000 ) ) ;
#70930 = CARTESIAN_POINT ( 'NONE',  ( -6.530923115290000247, 1417.905666013130030, 231.6298835945980272 ) ) ;
#70931 = CARTESIAN_POINT ( 'NONE',  ( -27.63867464639999838, 1385.244481134689977, 225.6178332698589770 ) ) ;
#70932 = ORIENTED_EDGE ( 'NONE', *, *, #21307, .T. ) ;
#70933 = CARTESIAN_POINT ( 'NONE',  ( -31.27769646076779964, 1385.227575565290181, 229.4193426744380133 ) ) ;
#70934 = FACE_OUTER_BOUND ( 'NONE', #55956, .T. ) ;
#70935 = CARTESIAN_POINT ( 'NONE',  ( 14.75922108689939982, 1469.003854007090240, 230.4826721581509901 ) ) ;
#70936 = CARTESIAN_POINT ( 'NONE',  ( -23.77573081741120120, 1509.051567791879961, 223.4963634714729892 ) ) ;
#70937 = DIRECTION ( 'NONE',  ( 0.000000000000000000, 1.000000000000000000, 0.000000000000000000 ) ) ;
#70938 = CARTESIAN_POINT ( 'NONE',  ( -0.1886782460270000072, 1409.088270590330012, 232.6670924473980051 ) ) ;
#70939 = CARTESIAN_POINT ( 'NONE',  ( 2.797255426280000012, 1417.697071498429978, 234.5789349732979758 ) ) ;
#70941 = CARTESIAN_POINT ( 'NONE',  ( 14.68195088934960069, 1451.730267658390176, 195.2572681451519827 ) ) ;
#70940 = CARTESIAN_POINT ( 'NONE',  ( -0.7376675409259989546, 1517.104497701820037, 214.9086937099069985 ) ) ;
#70942 = CARTESIAN_POINT ( 'NONE',  ( 9.957762540578798394, 1469.139097590099936, 207.8491545737729780 ) ) ;
#70943 = EDGE_LOOP ( 'NONE', ( #39022, #78853, #14323, #65618 ) ) ;
#70944 = CARTESIAN_POINT ( 'NONE',  ( -11.99589392261009912, 1415.088136167450102, 197.0938743475270201 ) ) ;
#70946 = EDGE_CURVE ( 'NONE', #42195, #98535, #89934, .T. ) ;
#70945 = EDGE_CURVE ( 'NONE', #106239, #58739, #37699, .T. ) ;
#70947 = CARTESIAN_POINT ( 'NONE',  ( -19.29371659517392601, 1526.349689584397083, 185.0912979150474200 ) ) ;
#70948 = ORIENTED_EDGE ( 'NONE', *, *, #83, .F. ) ;
#70949 = FACE_OUTER_BOUND ( 'NONE', #60823, .T. ) ;
#70950 = CARTESIAN_POINT ( 'NONE',  ( 18.06315781999999714, 1430.297107959589766, 211.8007709855490077 ) ) ;
#70951 = EDGE_CURVE ( 'NONE', #10343, #88662, #42177, .T. ) ;
#70952 = DIRECTION ( 'NONE',  ( 0.9455185755993178454, 0.000000000000000000, -0.3255681544571537578 ) ) ;
#70953 = CARTESIAN_POINT ( 'NONE',  ( 4.497572334437839103, 1424.519692532310046, 191.7182092258769899 ) ) ;
#70954 = CARTESIAN_POINT ( 'NONE',  ( -34.18677586421046044, 1522.906561336852974, 198.4504086008704746 ) ) ;
#70955 = CARTESIAN_POINT ( 'NONE',  ( -207.7471169361000136, -8387.357407334289746, 2179.761025090469957 ) ) ;
#70956 = DIRECTION ( 'NONE',  ( 0.2768460956572699194, -0.4521313779474797068, -0.8478994376661886934 ) ) ;
#70957 = CARTESIAN_POINT ( 'NONE',  ( 30.51231035492518728, 1526.382868172863937, 200.0858385050239008 ) ) ;
#70958 = CARTESIAN_POINT ( 'NONE',  ( -18.57722710470000038, 1435.146103754619844, 144.7442513582979871 ) ) ;
#70959 = CARTESIAN_POINT ( 'NONE',  ( -2.031883580139580037, 1464.998375551469962, 198.3053770173009980 ) ) ;
#70960 = CARTESIAN_POINT ( 'NONE',  ( -3.171072485709999889, 1451.871858332230204, 182.7750508701979868 ) ) ;
#70962 = CARTESIAN_POINT ( 'NONE',  ( -14.38276615813130022, 1509.537722091349906, 182.7943691049900110 ) ) ;
#70961 = CARTESIAN_POINT ( 'NONE',  ( 1.356545997123550062, 1410.335726221229834, 232.6398861002840022 ) ) ;
#70963 = CARTESIAN_POINT ( 'NONE',  ( -10.05392054895050080, 1472.343305534860065, 210.7099757364429706 ) ) ;
#70964 = ORIENTED_EDGE ( 'NONE', *, *, #68020, .T. ) ;
#70965 = CARTESIAN_POINT ( 'NONE',  ( 1.552473713816009848, 1415.666200589839946, 190.6769660270060172 ) ) ;
#70966 = CARTESIAN_POINT ( 'NONE',  ( 22.65374460030000137, 1411.052683168629983, 206.6971487888179979 ) ) ;
#70967 = CARTESIAN_POINT ( 'NONE',  ( -24.16028618640000047, 1437.513346555010003, 211.1466462160479978 ) ) ;
#70968 = CARTESIAN_POINT ( 'NONE',  ( 30.30080019752885434, 1526.189892541618974, 216.6986470857947609 ) ) ;
#70969 = DIRECTION ( 'NONE',  ( 0.000000000000000000, 0.000000000000000000, -1.000000000000000000 ) ) ;
#70970 = CARTESIAN_POINT ( 'NONE',  ( -2.580627846919146595, 1425.957731743932754, 184.7531624060546562 ) ) ;
#70971 = LINE ( 'NONE', #37335, #3081 ) ;
#70972 = CARTESIAN_POINT ( 'NONE',  ( -24.89623166663279719, 1440.854217278560100, 210.4275088599499952 ) ) ;
#70973 = CARTESIAN_POINT ( 'NONE',  ( -10.97127478134579981, 1470.155385822019980, 212.1066267448319991 ) ) ;
#70975 = VECTOR ( 'NONE', #30336, 1000.000000000000114 ) ;
#70974 = CARTESIAN_POINT ( 'NONE',  ( -8.552474816142620284, 1488.818340932279852, 216.6102650812369745 ) ) ;
#70976 = CARTESIAN_POINT ( 'NONE',  ( -13.90060862545290021, 1502.276468621130107, 227.4029620636050026 ) ) ;
#70977 = CARTESIAN_POINT ( 'NONE',  ( -80.19811966763030853, 1383.776841508610005, 303.7771253361019603 ) ) ;
#70978 = CARTESIAN_POINT ( 'NONE',  ( -109.0351493388839828, 1384.329153919109785, 311.2187254259250153 ) ) ;
#70979 = CARTESIAN_POINT ( 'NONE',  ( -15.20279846676549873, 1514.921193439789931, 193.2119408159660168 ) ) ;
#70980 = CARTESIAN_POINT ( 'NONE',  ( -1.518801255529869998, 1516.566488792059999, 201.4119714359050022 ) ) ;
#70982 = VERTEX_POINT ( 'NONE', #76327 ) ;
#70981 = CARTESIAN_POINT ( 'NONE',  ( 22.33903000980000186, 1509.718431408929973, 189.5993525853980088 ) ) ;
#70983 = CARTESIAN_POINT ( 'NONE',  ( -13.74310390781900004, 1517.151704408390060, 201.1531303618569950 ) ) ;
#70984 = CARTESIAN_POINT ( 'NONE',  ( -74.66787686629999143, 1381.796287462720102, 277.1868353108590100 ) ) ;
#70985 = DIRECTION ( 'NONE',  ( 0.5877852522924634782, 0.000000000000000000, -0.8090169943749544457 ) ) ;
#70986 = ORIENTED_EDGE ( 'NONE', *, *, #47971, .F. ) ;
#70987 = ORIENTED_EDGE ( 'NONE', *, *, #82208, .T. ) ;
#70988 = CARTESIAN_POINT ( 'NONE',  ( 26.51636468996370155, 1480.769270085010021, 207.6884295754969969 ) ) ;
#70989 = CARTESIAN_POINT ( 'NONE',  ( -110.0629862560000021, 1384.919307705380106, 296.9512714754590093 ) ) ;
#70990 = CARTESIAN_POINT ( 'NONE',  ( 12.72540794655758489, 1442.818196233205981, 169.4573749914120526 ) ) ;
#70992 = CARTESIAN_POINT ( 'NONE',  ( -39.71667984149999597, 1440.913060391189902, 259.0958842013980075 ) ) ;
#70991 = CARTESIAN_POINT ( 'NONE',  ( 34.89652595409791047, 1423.938945117018648, 269.5300863509276041 ) ) ;
#70993 = CARTESIAN_POINT ( 'NONE',  ( 8.559827946524409370, 1437.030862833870060, 207.9841999479689889 ) ) ;
#70994 = CARTESIAN_POINT ( 'NONE',  ( -11.11051595620000043, 1433.900636542000029, 151.6798721210980148 ) ) ;
#70995 = CARTESIAN_POINT ( 'NONE',  ( -0.2421828111940010075, 1488.147221623489941, 217.2451007367390048 ) ) ;
#70996 = CARTESIAN_POINT ( 'NONE',  ( -18.99761857140000032, 1485.804004457929977, 189.5282822598980204 ) ) ;
#70997 = CARTESIAN_POINT ( 'NONE',  ( 5.275011299300000012, 1410.472427662630025, 186.4709616624980129 ) ) ;
#70998 = CARTESIAN_POINT ( 'NONE',  ( 5.036045094249999465, 1422.685027075830021, 184.4684357060980062 ) ) ;
#70999 = CARTESIAN_POINT ( 'NONE',  ( -1.621556533595490013, 1515.068963820210001, 213.4511855176750146 ) ) ;
#71000 = CARTESIAN_POINT ( 'NONE',  ( 7.765022045919999449, 1439.035228149790100, 153.8379896983980188 ) ) ;
#71001 = CARTESIAN_POINT ( 'NONE',  ( -15.44414269670690132, 1421.125735695469757, 203.4397924531029958 ) ) ;
#71002 = CARTESIAN_POINT ( 'NONE',  ( 3.059301852550817102, 1525.343727714918259, 241.3958358433001479 ) ) ;
#71003 = CARTESIAN_POINT ( 'NONE',  ( -9.225907677606098645, 1517.151704408390060, 219.6631043460218393 ) ) ;
#71004 = VERTEX_POINT ( 'NONE', #110477 ) ;
#71005 = CARTESIAN_POINT ( 'NONE',  ( -3.273042392791920108, 1508.551704408389924, 214.1089285546999861 ) ) ;
#71006 = CARTESIAN_POINT ( 'NONE',  ( -21.35037659171259961, 1486.708548635719808, 201.9023949429700053 ) ) ;
#71007 = CARTESIAN_POINT ( 'NONE',  ( -13.09237183259999959, 1470.597673365530227, 270.0792996520979727 ) ) ;
#71008 = DIRECTION ( 'NONE',  ( 0.4794255386042031719, 0.000000000000000000, 0.8775825618903726477 ) ) ;
#71009 = CARTESIAN_POINT ( 'NONE',  ( 3.329166574300000292, 1441.604926038239910, 155.7074624611979914 ) ) ;
#71010 = CARTESIAN_POINT ( 'NONE',  ( -15.27799311270000082, 1485.037650874329984, 224.0147209149980085 ) ) ;
#71011 = CARTESIAN_POINT ( 'NONE',  ( 4.328907235665639952, 1515.085473475149911, 210.4350698618210060 ) ) ;
#71012 = CARTESIAN_POINT ( 'NONE',  ( -13.16208950729999927, 1420.370919692029929, 228.2271380253979771 ) ) ;
#71013 = CIRCLE ( 'NONE', #26528, 1.000000000000000888 ) ;
#71014 = CARTESIAN_POINT ( 'NONE',  ( -10.04630323299999972, 1461.008343231690105, 213.6807241916089879 ) ) ;
#71015 = CARTESIAN_POINT ( 'NONE',  ( 8.205855632998520832, 1360.030193506661362, 209.6218459617033432 ) ) ;
#71016 = CARTESIAN_POINT ( 'NONE',  ( -45.31040329346470230, 1436.802911717760026, 268.9839291206840244 ) ) ;
#71017 = CARTESIAN_POINT ( 'NONE',  ( -4.148575093039999828, 1428.755514565529893, 185.9890542076980182 ) ) ;
#71018 = ORIENTED_EDGE ( 'NONE', *, *, #50747, .F. ) ;
#71019 = CARTESIAN_POINT ( 'NONE',  ( -8.080215484499998269, 1424.584971138479887, 209.6516123241690082 ) ) ;
#71020 = ORIENTED_EDGE ( 'NONE', *, *, #62096, .F. ) ;
#71021 = CARTESIAN_POINT ( 'NONE',  ( 7.339107202615000602, 1517.203017563489766, 210.2473558205170150 ) ) ;
#71022 = CARTESIAN_POINT ( 'NONE',  ( -1.925297170580940076, 1517.151704408390060, 187.5582988486569889 ) ) ;
#71023 = CARTESIAN_POINT ( 'NONE',  ( -20.61542114839999940, 1508.364347659730129, 190.3921826406979960 ) ) ;
#71024 = CARTESIAN_POINT ( 'NONE',  ( -13.78890751930000036, 1425.417061756730163, 189.3862953465980183 ) ) ;
#71025 = AXIS2_PLACEMENT_3D ( 'NONE', #7975, #25308, #93618 ) ;
#71026 = CARTESIAN_POINT ( 'NONE',  ( -1.737201087752100026, 1496.680566212609847, 221.3643383344579831 ) ) ;
#71027 = ORIENTED_EDGE ( 'NONE', *, *, #50135, .F. ) ;
#71028 = DIRECTION ( 'NONE',  ( 1.000000000000000000, 0.000000000000000000, 0.000000000000000000 ) ) ;
#71029 =( BOUNDED_CURVE ( )  B_SPLINE_CURVE ( 3, ( #105688, #28970, #82672, #12708 ),
 .UNSPECIFIED., .F., .T. ) 
 B_SPLINE_CURVE_WITH_KNOTS ( ( 4, 4 ),
 ( 1.009769430403854029, 2.131822871348764803 ),
 .UNSPECIFIED. ) 
 CURVE ( )  GEOMETRIC_REPRESENTATION_ITEM ( )  RATIONAL_B_SPLINE_CURVE ( ( 1.000000000000000000, 0.8978061898640717908, 0.8978061898640717908, 1.000000000000000000 ) ) 
 REPRESENTATION_ITEM ( '' )  );
#71030 = B_SPLINE_CURVE_WITH_KNOTS ( 'NONE', 3,
 ( #9823, #71441, #80349, #30482, #20963, #97145, #37795, #88750, #20413, #12586, #28843, #14225, #73617, #29924, #46767, #89291, #81418, #107745, #80897, #12034, #64115, #4729, #98236, #46215, #22598 ),
 .UNSPECIFIED., .F., .F.,
 ( 4, 3, 3, 3, 3, 3, 3, 3, 4 ),
 ( -42.69308751009999980, -41.31664050871439997, -39.51470315257619603, -37.85453691144520150, -36.24168671189359969, -34.73070981842659677, -33.26220518797870085, -31.82994285059310258, -30.44684653110000028 ),
 .UNSPECIFIED. ) ;
#71031 = CARTESIAN_POINT ( 'NONE',  ( 2.276078898794865690, 1487.012333271777834, 219.6970559366252189 ) ) ;
#71032 = CARTESIAN_POINT ( 'NONE',  ( 8.910663374729999475, 1471.585705475490158, 214.3446098367489867 ) ) ;
#71033 = CARTESIAN_POINT ( 'NONE',  ( -9.954813569522620753, 1439.582591239990052, 208.1867998061339904 ) ) ;
#71034 = EDGE_LOOP ( 'NONE', ( #102401, #29078, #75354, #15310, #58901 ) ) ;
#71035 = CARTESIAN_POINT ( 'NONE',  ( -16.97136689889709871, 1410.626141966220075, 270.3495370215860021 ) ) ;
#71036 = CARTESIAN_POINT ( 'NONE',  ( 2.286472886424999906, 1516.883361325900069, 208.3638615500849767 ) ) ;
#71037 = CARTESIAN_POINT ( 'NONE',  ( -0.7904366496569998901, 1426.935925255829943, 133.6118001900980232 ) ) ;
#71038 = DIRECTION ( 'NONE',  ( -5.980589973904019347E-17, 1.000000000000000000, -1.736889445713099699E-16 ) ) ;
#71040 = ORIENTED_EDGE ( 'NONE', *, *, #61177, .F. ) ;
#71039 = CARTESIAN_POINT ( 'NONE',  ( -7.532495872739816356, 1365.665514383497566, 208.3718459617061285 ) ) ;
#71041 = ORIENTED_EDGE ( 'NONE', *, *, #74078, .T. ) ;
#71042 = CARTESIAN_POINT ( 'NONE',  ( 45.63562816159383573, 1441.199288540710768, 268.9747940734181384 ) ) ;
#71043 = CARTESIAN_POINT ( 'NONE',  ( 0.7923714640039719592, 1467.258159185920022, 220.1721432627789738 ) ) ;
#71044 = CARTESIAN_POINT ( 'NONE',  ( -9.066449906558435856, 1440.400147515658091, 153.5443354344916145 ) ) ;
#71045 = CARTESIAN_POINT ( 'NONE',  ( -15.46200339894285847, 1407.981780703992172, 266.8670517912573246 ) ) ;
#71046 = AXIS2_PLACEMENT_3D ( 'NONE', #84226, #59054, #60724 ) ;
#71047 = CARTESIAN_POINT ( 'NONE',  ( -18.45097462037960057, 1415.673583075490114, 207.5694314020479965 ) ) ;
#71048 = CARTESIAN_POINT ( 'NONE',  ( -18.09906091010000040, 1435.779564141970013, 226.5701799449980172 ) ) ;
#71049 = EDGE_CURVE ( 'NONE', #109427, #17632, #33755, .T. ) ;
#71050 = CARTESIAN_POINT ( 'NONE',  ( 15.79251552625780164, 1474.064138637460019, 266.8741674170499891 ) ) ;
#71051 = CARTESIAN_POINT ( 'NONE',  ( 12.07588402680000073, 1415.579607678529783, 223.1679904141980160 ) ) ;
#71052 = CARTESIAN_POINT ( 'NONE',  ( -10.33299300126450149, 1447.717326489380184, 209.8084994042759774 ) ) ;
#71053 = CARTESIAN_POINT ( 'NONE',  ( -1.716392779905000054, 1516.788317650260069, 206.2580580763669786 ) ) ;
#71054 = EDGE_LOOP ( 'NONE', ( #45537, #102385, #92435, #64168, #110037 ) ) ;
#71055 = CARTESIAN_POINT ( 'NONE',  ( 20.68010504029316010, 1410.996119301493081, 218.7905024334752113 ) ) ;
#71056 = CARTESIAN_POINT ( 'NONE',  ( 1.503770822449239875, 1464.070697699469974, 182.9916286601730064 ) ) ;
#71057 = ORIENTED_EDGE ( 'NONE', *, *, #30538, .T. ) ;
#71058 = CARTESIAN_POINT ( 'NONE',  ( 4.678976733710090485, 1508.551704408389924, 205.0635106934799978 ) ) ;
#71060 = EDGE_CURVE ( 'NONE', #41855, #10196, #83111, .T. ) ;
#71059 = CARTESIAN_POINT ( 'NONE',  ( 25.24320764742720158, 1451.875638110379896, 136.2233328636380350 ) ) ;
#71061 = CARTESIAN_POINT ( 'NONE',  ( -4.987078438843339789, 1508.551704408389924, 211.6718637777229901 ) ) ;
#71062 = CARTESIAN_POINT ( 'NONE',  ( -39.76804797110000322, 1384.988983489909742, 212.4493689816489734 ) ) ;
#71063 = CARTESIAN_POINT ( 'NONE',  ( -12.56539978307642791, 1389.228131685772041, 215.4313030480873294 ) ) ;
#71064 = CARTESIAN_POINT ( 'NONE',  ( 17.85287820219999944, 1409.701424983430115, 194.3066436361979754 ) ) ;
#71065 = DIRECTION ( 'NONE',  ( 0.9510565162951561957, 0.000000000000000000, 0.3090169943749392911 ) ) ;
#71066 = CARTESIAN_POINT ( 'NONE',  ( 3.351449279187751262, 1439.689399315149558, 184.4071940306241117 ) ) ;
#71067 = CARTESIAN_POINT ( 'NONE',  ( -19.82422479395705750, 1426.129180672527127, 222.7993382114829046 ) ) ;
#71068 = DIRECTION ( 'NONE',  ( 0.9786619618251657382, 0.000000000000000000, 0.2054769195713179730 ) ) ;
#71069 = CIRCLE ( 'NONE', #103139, 14.91144628110000170 ) ;
#71070 = CARTESIAN_POINT ( 'NONE',  ( -9.599331020219999289, 1381.710107449539919, 217.4672660472789687 ) ) ;
#71071 = CARTESIAN_POINT ( 'NONE',  ( 1.131796810615000037, 1516.659138130710289, 214.8948242487770131 ) ) ;
#71072 = CARTESIAN_POINT ( 'NONE',  ( 2.487421823092354156, 1523.954914175591739, 242.7965504892020192 ) ) ;
#71073 = ORIENTED_EDGE ( 'NONE', *, *, #63601, .T. ) ;
#71074 = CARTESIAN_POINT ( 'NONE',  ( -16.70831018089999986, 1417.149231790749809, 207.3570869115089863 ) ) ;
#71075 = CARTESIAN_POINT ( 'NONE',  ( 4.637787270109999582, 1462.124489585889933, 228.1829287868989979 ) ) ;
#71076 = CARTESIAN_POINT ( 'NONE',  ( -7.416192941597599564, 1484.381854404939986, 199.8094865323589886 ) ) ;
#71077 = CARTESIAN_POINT ( 'NONE',  ( -20.09781860883127536, 1508.119603360660221, 209.6220754275047113 ) ) ;
#71078 = CARTESIAN_POINT ( 'NONE',  ( -37.93102824555499808, 1448.882024444920035, 136.3724781078850015 ) ) ;
#71079 = EDGE_CURVE ( 'NONE', #36663, #23166, #12965, .T. ) ;
#71080 = CARTESIAN_POINT ( 'NONE',  ( -4.329448776040000446, 1515.064792882589927, 207.2788837304390199 ) ) ;
#71081 = CARTESIAN_POINT ( 'NONE',  ( -14.35418281379999961, 1450.996202461129997, 214.3676144195279676 ) ) ;
#71082 = CARTESIAN_POINT ( 'NONE',  ( -28.27139721233055170, 1526.382868172863937, 198.6830693683576214 ) ) ;
#71083 = CARTESIAN_POINT ( 'NONE',  ( 11.85425778610000158, 1433.048935507500119, 150.3174848872980078 ) ) ;
#71084 = CARTESIAN_POINT ( 'NONE',  ( -4.761695837242630347, 1473.992865699130107, 270.1327791948820050 ) ) ;
#71085 = CARTESIAN_POINT ( 'NONE',  ( 25.63907149821320175, 1440.913060399049982, 219.8810537515410033 ) ) ;
#71086 = CARTESIAN_POINT ( 'NONE',  ( -20.33900532369999681, 1508.016036090129774, 228.6619146254979853 ) ) ;
#71087 = CARTESIAN_POINT ( 'NONE',  ( -31.79839622030619495, 1525.159196711359755, 202.0929531505411489 ) ) ;
#71088 = VERTEX_POINT ( 'NONE', #19724 ) ;
#71089 = CARTESIAN_POINT ( 'NONE',  ( -27.59578990780000041, 1509.876726736629962, 201.0523533628679616 ) ) ;
#71090 = CARTESIAN_POINT ( 'NONE',  ( 24.93050294115990795, 1436.289034237693386, 137.8926071792222672 ) ) ;
#71091 = VECTOR ( 'NONE', #93737, 1000.000000000000114 ) ;
#71092 = CARTESIAN_POINT ( 'NONE',  ( 22.71325450959999870, 1409.706218420429877, 209.2588089802279967 ) ) ;
#71093 = CARTESIAN_POINT ( 'NONE',  ( 7.590703170876726524, 1398.138570740227351, 198.5570256807006047 ) ) ;
#71094 = CARTESIAN_POINT ( 'NONE',  ( 2.630527005430000287, 1490.916590196630068, 235.2555692320979972 ) ) ;
#71095 = CARTESIAN_POINT ( 'NONE',  ( 24.85895335929999916, 1430.362482292330014, 209.8091488686460195 ) ) ;
#71096 = VECTOR ( 'NONE', #50309, 1000.000000000000227 ) ;
#71097 = CARTESIAN_POINT ( 'NONE',  ( 29.99620953741496976, 1526.382868172863937, 219.7462484079458704 ) ) ;
#71098 = DIRECTION ( 'NONE',  ( -0.4978433412588703089, 0.000000000000000000, 0.8672669759446649529 ) ) ;
#71099 = CARTESIAN_POINT ( 'NONE',  ( -24.69891064529219804, 1383.848419887520095, 223.2892647768329653 ) ) ;
#71100 = CARTESIAN_POINT ( 'NONE',  ( -3.137380515432329986, 1508.729448924109874, 204.5649393178340176 ) ) ;
#71101 = CARTESIAN_POINT ( 'NONE',  ( 2.499936552876079965, 1420.115363462959976, 90.95688517979088772 ) ) ;
#71102 = CARTESIAN_POINT ( 'NONE',  ( -1732.234191736389675, 11221.53578756870047, -1992.291823225089274 ) ) ;
#71103 = CARTESIAN_POINT ( 'NONE',  ( -2.330134126090000368, 1515.551704408389924, 205.2922258481490303 ) ) ;
#71105 = ORIENTED_EDGE ( 'NONE', *, *, #67624, .T. ) ;
#71104 = CARTESIAN_POINT ( 'NONE',  ( 3.440131352139999876, 1441.985517479789905, 217.4173380492889862 ) ) ;
#71106 = CARTESIAN_POINT ( 'NONE',  ( -0.5623043548920000356, 1416.835809830829930, 227.7680352835980102 ) ) ;
#71107 = CARTESIAN_POINT ( 'NONE',  ( -9.240102488050887075, 1388.574724895332793, 200.8464198674274996 ) ) ;
#71108 = CARTESIAN_POINT ( 'NONE',  ( -4.794939693159999905, 1475.260167711990107, 199.8527928283789947 ) ) ;
#71110 = ORIENTED_EDGE ( 'NONE', *, *, #80164, .F. ) ;
#71109 = CARTESIAN_POINT ( 'NONE',  ( -36.72650137420430383, 1451.114006374390101, 134.0999999987039644 ) ) ;
#71111 = CARTESIAN_POINT ( 'NONE',  ( -3.612392877355159904, 1508.551704408389924, 219.9195952245149783 ) ) ;
#71112 = ORIENTED_EDGE ( 'NONE', *, *, #73287, .F. ) ;
#71113 = CARTESIAN_POINT ( 'NONE',  ( -9.428062662729999488, 1388.903456711819899, 217.2485254379789978 ) ) ;
#71114 = CARTESIAN_POINT ( 'NONE',  ( -17.76192429420000352, 1416.216739748429973, 211.9674486285379942 ) ) ;
#71115 = CARTESIAN_POINT ( 'NONE',  ( 3.269916730896537338, 1485.110870265661788, 219.7892682990461424 ) ) ;
#71116 = CARTESIAN_POINT ( 'NONE',  ( 23.55087631299999984, 1411.110694763729953, 207.7642880164279973 ) ) ;
#71117 = B_SPLINE_CURVE_WITH_KNOTS ( 'NONE', 3,
 ( #84384, #32864, #6578, #22793, #8209, #59206, #23903, #32335, #100618, #7671, #67055, #65404 ),
 .UNSPECIFIED., .F., .F.,
 ( 4, 2, 2, 2, 2, 4 ),
 ( 4.496430354704500113E-15, 9.667223565493732152E-05, 0.0001933444713053782127, 0.0003866889426061961626, 0.0007733778852078835621, 0.001546755770410726451 ),
 .UNSPECIFIED. ) ;
#71118 = CARTESIAN_POINT ( 'NONE',  ( -14.82545538847084110, 1420.108256178820739, 213.3440734001790418 ) ) ;
#71119 = CARTESIAN_POINT ( 'NONE',  ( -12.29983469507761917, 1377.704127499016067, 208.5802176589124031 ) ) ;
#71120 = AXIS2_PLACEMENT_3D ( 'NONE', #85791, #49456, #41031 ) ;
#71121 = CARTESIAN_POINT ( 'NONE',  ( 13.89024821118459840, 1409.398118541669874, 214.6073209033960154 ) ) ;
#71122 = DIRECTION ( 'NONE',  ( 1.000000000000000000, 0.000000000000000000, 0.000000000000000000 ) ) ;
#71123 = CARTESIAN_POINT ( 'NONE',  ( -105.1325957748820059, 1385.233345991170154, 296.9340941069459632 ) ) ;
#71124 = CARTESIAN_POINT ( 'NONE',  ( -17.67056496260000031, 1412.978053172430009, 193.3746425421979893 ) ) ;
#71125 = CARTESIAN_POINT ( 'NONE',  ( -3.378249781281797759, 1476.214897016527402, 219.3461772814387984 ) ) ;
#71126 = CARTESIAN_POINT ( 'NONE',  ( 10.81577661162920023, 1490.127638817409888, 207.3825687807529903 ) ) ;
#71128 = EDGE_LOOP ( 'NONE', ( #46327, #4043, #107624, #96770 ) ) ;
#71127 = CARTESIAN_POINT ( 'NONE',  ( 3.034148894259999896, 1440.440283194090171, 157.2495476715980089 ) ) ;
#71129 = ORIENTED_EDGE ( 'NONE', *, *, #67209, .T. ) ;
#71130 = CARTESIAN_POINT ( 'NONE',  ( -12.25049518321329955, 1416.576002138870081, 194.6830814986430198 ) ) ;
#71131 = CARTESIAN_POINT ( 'NONE',  ( -11.99985923319999870, 1433.681662988860126, 149.8469377335979971 ) ) ;
#71132 = CARTESIAN_POINT ( 'NONE',  ( 16.66598991933063445, 1468.916255155639874, 269.3720935231359022 ) ) ;
#71133 = CARTESIAN_POINT ( 'NONE',  ( 12.45662817246929954, 1427.088122696140090, 206.6493147128259977 ) ) ;
#71134 = CARTESIAN_POINT ( 'NONE',  ( 1.233953280850000001, 1397.950740760129975, 222.1299377637979831 ) ) ;
#71135 = CARTESIAN_POINT ( 'NONE',  ( 31.79806488006812870, 1525.506916460682078, 201.2206263324432030 ) ) ;
#71136 = CARTESIAN_POINT ( 'NONE',  ( -6.729604382136518126, 1516.629170255225063, 212.4376854727360922 ) ) ;
#71137 = CARTESIAN_POINT ( 'NONE',  ( -19.02802488173782081, 1486.252467685796091, 189.3493767970001898 ) ) ;
#71138 = CARTESIAN_POINT ( 'NONE',  ( -11.91708563375230767, 1364.919342642561787, 208.3718459617010978 ) ) ;
#71139 = DIRECTION ( 'NONE',  ( 0.000000000000000000, 0.000000000000000000, 1.000000000000000000 ) ) ;
#71140 = CARTESIAN_POINT ( 'NONE',  ( 6.546302742015000398, 1516.577434278289957, 206.6347425125669872 ) ) ;
#71141 = AXIS2_PLACEMENT_3D ( 'NONE', #109229, #102998, #32513 ) ;
#71142 = CARTESIAN_POINT ( 'NONE',  ( -13.18323158269999951, 1435.197366603820001, 150.1160888488979879 ) ) ;
#71143 = CARTESIAN_POINT ( 'NONE',  ( 18.16369802799999889, 1409.547350699329854, 196.7220820877979861 ) ) ;
#71144 = CARTESIAN_POINT ( 'NONE',  ( -18.70459388414779767, 1509.566239243649989, 231.7064163625079800 ) ) ;
#71145 = CARTESIAN_POINT ( 'NONE',  ( -7.732430556567909896, 1493.472238524849899, 207.1384183514769859 ) ) ;
#71146 = CARTESIAN_POINT ( 'NONE',  ( -109.1848878950000028, 1384.511724394249995, 297.1380044401590226 ) ) ;
#71147 = VERTEX_POINT ( 'NONE', #71284 ) ;
#71148 = CARTESIAN_POINT ( 'NONE',  ( 45.67178420940000194, 1438.126719075119809, 266.1886048709980059 ) ) ;
#71149 = CARTESIAN_POINT ( 'NONE',  ( -21.80621300580000010, 1469.235547604329895, 196.1136359960979973 ) ) ;
#71151 = CARTESIAN_POINT ( 'NONE',  ( 13.56343219680000090, 1416.311719779230089, 196.3989970432979817 ) ) ;
#71150 = CARTESIAN_POINT ( 'NONE',  ( -10.97801989845739890, 1426.061463023469742, 97.52402582803289022 ) ) ;
#71152 = CARTESIAN_POINT ( 'NONE',  ( 0.01327253640020150012, 1516.940252185109784, 211.9957649727570015 ) ) ;
#71153 = DIRECTION ( 'NONE',  ( 0.000000000000000000, 1.000000000000000000, 0.000000000000000000 ) ) ;
#71154 = CARTESIAN_POINT ( 'NONE',  ( -32.79493994580000304, 1434.501496568330140, 248.1152222149979991 ) ) ;
#71155 = CARTESIAN_POINT ( 'NONE',  ( 2.265886247949999710, 1487.020940553290075, 219.7147332017989925 ) ) ;
#71156 = CARTESIAN_POINT ( 'NONE',  ( 3.183012419607803345, 1447.433753094939448, 154.8412150998025538 ) ) ;
#71157 = DIRECTION ( 'NONE',  ( 0.3363363969981663093, 0.6659120918162475533, -0.6659120918163308200 ) ) ;
#71158 = VERTEX_POINT ( 'NONE', #28129 ) ;
#71159 = CARTESIAN_POINT ( 'NONE',  ( -5.385828860609489510, 1432.197383170389912, 154.6045697296559922 ) ) ;
#71160 = CARTESIAN_POINT ( 'NONE',  ( 12.01214636615307185, 1513.042027792501813, 225.7134143163021918 ) ) ;
#71161 = CARTESIAN_POINT ( 'NONE',  ( -15.36439361150980076, 1376.113480921259907, 247.8666525594929908 ) ) ;
#71162 = ORIENTED_EDGE ( 'NONE', *, *, #108264, .T. ) ;
#71163 = VERTEX_POINT ( 'NONE', #98080 ) ;
#71164 = AXIS2_PLACEMENT_3D ( 'NONE', #81246, #59388, #34707 ) ;
#71165 = CARTESIAN_POINT ( 'NONE',  ( 10.44089720877999916, 1453.109204862920024, 211.0141701243190084 ) ) ;
#71166 = CARTESIAN_POINT ( 'NONE',  ( 5.522475241700000481, 1424.154859417280022, 193.8631810266990101 ) ) ;
#71167 = ORIENTED_EDGE ( 'NONE', *, *, #51660, .F. ) ;
#71168 = CARTESIAN_POINT ( 'NONE',  ( -0.1626181647790000129, 1421.812182938429942, 227.5856863222980166 ) ) ;
#71169 = CARTESIAN_POINT ( 'NONE',  ( -9.642223397419670050, 1460.679120766980077, 208.4218084076549928 ) ) ;
#71170 = DIRECTION ( 'NONE',  ( 0.000000000000000000, -1.000000000000000000, 0.000000000000000000 ) ) ;
#71171 = VECTOR ( 'NONE', #222, 1000.000000000000114 ) ;
#71172 = CARTESIAN_POINT ( 'NONE',  ( -0.3264474814539999881, 1470.489006557829953, 235.7562541381980168 ) ) ;
#71173 = CARTESIAN_POINT ( 'NONE',  ( 1.923719469800590165, 1421.100103055099908, 183.1407590705949815 ) ) ;
#71174 = ORIENTED_EDGE ( 'NONE', *, *, #66493, .F. ) ;
#71175 = AXIS2_PLACEMENT_3D ( 'NONE', #71578, #2698, #4862 ) ;
#71176 = CARTESIAN_POINT ( 'NONE',  ( 11.63658410760000095, 1425.864915301529891, 144.1607460163980079 ) ) ;
#71177 = CARTESIAN_POINT ( 'NONE',  ( -2.419927497189999777, 1502.444211376990097, 230.3922731312990209 ) ) ;
#71178 = CARTESIAN_POINT ( 'NONE',  ( 15.59042067260000053, 1507.631725826930051, 225.7583918763980080 ) ) ;
#71179 = ORIENTED_EDGE ( 'NONE', *, *, #34328, .F. ) ;
#71180 = CARTESIAN_POINT ( 'NONE',  ( 3.449149195745000007, 1516.947419719950176, 204.4980579627370219 ) ) ;
#71181 = ORIENTED_EDGE ( 'NONE', *, *, #30146, .F. ) ;
#71182 = CARTESIAN_POINT ( 'NONE',  ( 11.86235724903239941, 1432.074504238270038, 149.9760656271810149 ) ) ;
#71183 = CARTESIAN_POINT ( 'NONE',  ( 5.385523159618170297, 1511.435001054559962, 217.7746220610370074 ) ) ;
#71184 = ORIENTED_EDGE ( 'NONE', *, *, #40774, .F. ) ;
#71185 = VERTEX_POINT ( 'NONE', #62320 ) ;
#71186 = CARTESIAN_POINT ( 'NONE',  ( -1.447759218079930132, 1462.381657541340019, 183.4226446050429900 ) ) ;
#71187 = CARTESIAN_POINT ( 'NONE',  ( -13.51610093809999924, 1443.913060387330006, 169.3501091259980171 ) ) ;
#71188 = CARTESIAN_POINT ( 'NONE',  ( 3.048828140119999919, 1509.019527812029992, 237.9289388369980145 ) ) ;
#71189 = CARTESIAN_POINT ( 'NONE',  ( -9.842736051686820531, 1471.074784007589869, 212.0439963695450274 ) ) ;
#71190 = CARTESIAN_POINT ( 'NONE',  ( -4.363116875470000267, 1423.854803018830125, 184.2545991611980014 ) ) ;
#71191 = CARTESIAN_POINT ( 'NONE',  ( 3.056876074108880292, 1410.319324463180010, 269.6158940089480325 ) ) ;
#71192 = CARTESIAN_POINT ( 'NONE',  ( 32.38114538885255200, 1523.604703353109699, 216.1203639561429100 ) ) ;
#71193 = CARTESIAN_POINT ( 'NONE',  ( -12.77139216734400051, 1502.534344327860026, 209.6059914789669847 ) ) ;
#71194 = CARTESIAN_POINT ( 'NONE',  ( -2.402424516307810176, 1422.211108107479959, 192.9590038495489921 ) ) ;
#71195 = CARTESIAN_POINT ( 'NONE',  ( 11.26937486967429969, 1478.652699849539886, 205.8601904136019982 ) ) ;
#71196 = CARTESIAN_POINT ( 'NONE',  ( 8.343648446271952679, 1424.442999199686028, 195.7429581655293873 ) ) ;
#71198 = CARTESIAN_POINT ( 'NONE',  ( 10.26782831285779984, 1469.378476928209921, 204.4240403020939993 ) ) ;
#71197 = CARTESIAN_POINT ( 'NONE',  ( -14.27911803519999978, 1503.311367094989919, 208.8533501441869760 ) ) ;
#71199 = CARTESIAN_POINT ( 'NONE',  ( 11.93531355930769955, 1421.883139682599904, 207.3300720177520020 ) ) ;
#71200 = CIRCLE ( 'NONE', #62246, 1.000000000000000888 ) ;
#71201 = CARTESIAN_POINT ( 'NONE',  ( -9.962284032283351465, 1439.515202336300035, 208.3475260488820027 ) ) ;
#71202 = CARTESIAN_POINT ( 'NONE',  ( -8.027449309594999249, 1514.605246816799763, 202.6315394120669851 ) ) ;
#71203 = ORIENTED_EDGE ( 'NONE', *, *, #45214, .T. ) ;
#71204 = CARTESIAN_POINT ( 'NONE',  ( 38.34143784940000188, 1436.524347965420020, 265.6112251771979800 ) ) ;
#71205 = B_SPLINE_CURVE_WITH_KNOTS ( 'NONE', 5,
 ( #21113, #31738, #3825, #48567, #22761, #56410 ),
 .UNSPECIFIED., .F., .F.,
 ( 6, 6 ),
 ( 0.000000000000000000, 1.000000000000000000 ),
 .UNSPECIFIED. ) ;
#71206 = CARTESIAN_POINT ( 'NONE',  ( 41.15110440228482958, 1443.645438857304953, 136.9181504661874840 ) ) ;
#71208 = CARTESIAN_POINT ( 'NONE',  ( -66.72509573152139239, 1385.036337219960160, 291.0918609499310037 ) ) ;
#71207 = B_SPLINE_CURVE_WITH_KNOTS ( 'NONE', 3,
 ( #30988, #108247, #56201, #108802, #13613, #56758, #15272, #81936, #91456, #64623, #14178, #5239, #99834, #83586, #48923, #13066, #48365, #98744, #4691 ),
 .UNSPECIFIED., .F., .F.,
 ( 4, 3, 3, 3, 3, 3, 4 ),
 ( -1.403944690730000167, -1.188125015481449998, -0.9636848121176839754, -0.7385352318536739791, -0.5129228707660121733, -0.2865928050055470688, -0.05981740377519995100 ),
 .UNSPECIFIED. ) ;
#71209 = CARTESIAN_POINT ( 'NONE',  ( -17.89234610336760412, 1523.611961620354123, 180.3157245011626912 ) ) ;
#71210 = CARTESIAN_POINT ( 'NONE',  ( 3.554299223149999687, 1505.806595534090093, 220.9721875483989777 ) ) ;
#71211 = CARTESIAN_POINT ( 'NONE',  ( 43.70825229526830213, 1428.337867259879886, 269.0264340981559599 ) ) ;
#71213 = VERTEX_POINT ( 'NONE', #61762 ) ;
#71212 = CARTESIAN_POINT ( 'NONE',  ( -17.81215992105380153, 1419.248216703719891, 206.8919694010189687 ) ) ;
#71214 = CARTESIAN_POINT ( 'NONE',  ( -17.38240445386849942, 1417.772954075339840, 205.8675793474119757 ) ) ;
#71215 = CARTESIAN_POINT ( 'NONE',  ( -24.39954769610000085, 1443.080901239500008, 211.1504982047080148 ) ) ;
#71216 = CARTESIAN_POINT ( 'NONE',  ( -1.600048698852036821, 1411.254281879943164, 135.5999999980979851 ) ) ;
#71217 = CARTESIAN_POINT ( 'NONE',  ( -19.74523735960000081, 1465.054873128789950, 210.0762488071430028 ) ) ;
#71218 = CARTESIAN_POINT ( 'NONE',  ( 11.74940789013500009, 1512.456207068040158, 225.5877689890670013 ) ) ;
#71219 = CARTESIAN_POINT ( 'NONE',  ( -12.10873113499999931, 1442.495059057370099, 187.0567141033980079 ) ) ;
#71220 = CARTESIAN_POINT ( 'NONE',  ( 21.71631475791559751, 1509.710815674639889, 229.8179829200470010 ) ) ;
#71221 = DIRECTION ( 'NONE',  ( 0.000000000000000000, 1.000000000000000000, -1.836970198721029688E-16 ) ) ;
#71222 = CARTESIAN_POINT ( 'NONE',  ( 12.28535814839943541, 1434.206754551802078, 149.6317592098948808 ) ) ;
#71223 = CARTESIAN_POINT ( 'NONE',  ( 14.57860324780000028, 1417.424410125430086, 228.0517902003980169 ) ) ;
#71224 = ADVANCED_FACE ( 'NONE', ( #62894 ), #12425, .F. ) ;
#71225 = CARTESIAN_POINT ( 'NONE',  ( 9.708743359033459086, 1469.923152700759829, 211.7994329600670085 ) ) ;
#71227 = CARTESIAN_POINT ( 'NONE',  ( -16.12699268032000077, 1459.080750933630043, 229.9878372279760015 ) ) ;
#71226 = CIRCLE ( 'NONE', #37226, 1.999999999999957589 ) ;
#71228 = CARTESIAN_POINT ( 'NONE',  ( 6.933587655514999781, 1516.542957540330008, 207.4124872689769745 ) ) ;
#71229 = CARTESIAN_POINT ( 'NONE',  ( 39.35535942429999778, 1422.520539079029959, 268.7089579441980050 ) ) ;
#71230 = CARTESIAN_POINT ( 'NONE',  ( -18.81215439969999892, 1410.493119616930244, 223.2931733231980047 ) ) ;
#71231 = CARTESIAN_POINT ( 'NONE',  ( 17.05308463140000086, 1435.093823673100133, 146.1608047648980175 ) ) ;
#71232 = CARTESIAN_POINT ( 'NONE',  ( 20.43733526010000290, 1469.157605011630039, 192.7233812162979802 ) ) ;
#71233 = CARTESIAN_POINT ( 'NONE',  ( 5.362419220542090414, 1424.201140997230141, 150.5224082514530153 ) ) ;
#71234 = DIRECTION ( 'NONE',  ( 0.000000000000000000, 0.5259463573989414664, 0.8505177418130589473 ) ) ;
#71235 = CARTESIAN_POINT ( 'NONE',  ( -44.47031351537230393, 1451.019434385626482, 266.2216429519685903 ) ) ;
#71237 = B_SPLINE_CURVE_WITH_KNOTS ( 'NONE', 3,
 ( #3881, #79469, #55375, #10042, #105780, #35806, #63778, #61574, #36899, #54287 ),
 .UNSPECIFIED., .F., .F.,
 ( 4, 2, 2, 2, 4 ),
 ( 0.000000000000000000, 0.2500000000000000000, 0.5000000000000000000, 0.7500000000000000000, 1.000000000000000000 ),
 .UNSPECIFIED. ) ;
#71236 = CARTESIAN_POINT ( 'NONE',  ( 32.85805783624312681, 1523.678648413191695, 217.1983043299902931 ) ) ;
#71238 = CARTESIAN_POINT ( 'NONE',  ( -33.93525006893180063, 1435.841462747220021, 135.9408810291510008 ) ) ;
#71239 = B_SPLINE_CURVE_WITH_KNOTS ( 'NONE', 5,
 ( #21116, #55321, #89453, #12746, #89996, #46928, #81046, #30082, #36290, #96765, #54230, #64276 ),
 .UNSPECIFIED., .F., .F.,
 ( 6, 3, 3, 6 ),
 ( 0.000000000000000000, 0.2739007385715113152, 0.6877721063829390635, 1.000000000000000000 ),
 .UNSPECIFIED. ) ;
#71240 = DIRECTION ( 'NONE',  ( 0.000000000000000000, -1.000000000000000000, 0.000000000000000000 ) ) ;
#71241 = CARTESIAN_POINT ( 'NONE',  ( -15.71890336570000102, 1414.913060387229962, 203.5737140920780064 ) ) ;
#71242 = CARTESIAN_POINT ( 'NONE',  ( 22.70509004431190192, 1409.705939603270053, 209.2982552845940063 ) ) ;
#71243 = CARTESIAN_POINT ( 'NONE',  ( -7.765511611824870819, 1383.298095908590085, 218.8630668455809882 ) ) ;
#71244 = CARTESIAN_POINT ( 'NONE',  ( 12.40455451780000118, 1434.419853495000098, 146.4343138086979934 ) ) ;
#71245 = CARTESIAN_POINT ( 'NONE',  ( -30.19569412050000068, 1435.551785849099815, 135.1818641824980034 ) ) ;
#71246 = CARTESIAN_POINT ( 'NONE',  ( -3.827053565004849833, 1515.145425758850251, 209.1218459619010162 ) ) ;
#71247 = ORIENTED_EDGE ( 'NONE', *, *, #20912, .T. ) ;
#71248 = CARTESIAN_POINT ( 'NONE',  ( 5.980914351475993485, 1510.675349056919458, 216.6316662786656764 ) ) ;
#71249 = CARTESIAN_POINT ( 'NONE',  ( 39.87321672109999326, 1440.876652101590025, 136.8077108269980044 ) ) ;
#71250 = CARTESIAN_POINT ( 'NONE',  ( -19.27355791249999939, 1467.813399981289876, 204.3088842694490097 ) ) ;
#71251 = VERTEX_POINT ( 'NONE', #70178 ) ;
#71252 = CIRCLE ( 'NONE', #22900, 1.999999999999999556 ) ;
#71253 = DIRECTION ( 'NONE',  ( 0.000000000000000000, -1.000000000000000000, -2.312964634635740689E-15 ) ) ;
#71254 = CARTESIAN_POINT ( 'NONE',  ( -4.897370105774945692, 1421.905084353634948, 138.0291448931159550 ) ) ;
#71255 = CARTESIAN_POINT ( 'NONE',  ( -37.68243668920000289, 1461.704006605230006, 266.6693340566979487 ) ) ;
#71256 = CARTESIAN_POINT ( 'NONE',  ( -13.42305729488690069, 1429.046643101820109, 222.2861133963140219 ) ) ;
#71257 = VECTOR ( 'NONE', #105952, 1000.000000000000114 ) ;
#71258 = CARTESIAN_POINT ( 'NONE',  ( 0.3556640921540570321, 1419.127793398659833, 184.6118934103729998 ) ) ;
#71259 = FACE_OUTER_BOUND ( 'NONE', #81876, .T. ) ;
#71260 = DIRECTION ( 'NONE',  ( 0.000000000000000000, 0.000000000000000000, -1.000000000000000000 ) ) ;
#71261 = B_SPLINE_SURFACE_WITH_KNOTS ( 'NONE', 5, 5, ( 
 ( #35985, #26456, #60650, #95334, #52246, #18595 ),
 ( #52792, #34315, #86926, #102594, #10217, #79103 ),
 ( #93645, #17483, #44395, #78537, #51129, #27574 ),
 ( #61757, #19144, #87496, #10784, #44956, #2411 ),
 ( #36528, #70724, #47143, #88601, #37630, #105392 ),
 ( #37076, #54463, #11884, #62316, #62890, #46608 ),
 ( #11340, #28684, #53921, #4049, #20263, #45513 ),
 ( #5121, #97000, #81819, #38176, #63421, #79654 ),
 ( #2959, #29232, #46056, #39277, #107034, #38718 ) ),
 .UNSPECIFIED., .F., .F., .F.,
 ( 6, 3, 6 ),
 ( 6, 6 ),
 ( 4.410666364559999941, 8.626592454029999857, 14.48744219459999982 ),
 ( 0.000000000000000000, 2.000000000000000000 ),
 .UNSPECIFIED. ) ;
#71262 = CARTESIAN_POINT ( 'NONE',  ( -44.00405079680249543, 1385.000270709609822, 217.1257494786190136 ) ) ;
#71263 = CARTESIAN_POINT ( 'NONE',  ( -5.013279353751990186, 1375.408587603007163, 214.7179514574215204 ) ) ;
#71264 = CARTESIAN_POINT ( 'NONE',  ( 17.17404474450000151, 1416.216596894529857, 215.3726550198079792 ) ) ;
#71265 = CIRCLE ( 'NONE', #12224, 1.000000000000000888 ) ;
#71266 = CARTESIAN_POINT ( 'NONE',  ( -9.443064477949999258, 1434.540978515130064, 153.1670680800980051 ) ) ;
#71267 = CARTESIAN_POINT ( 'NONE',  ( -10.83190899079038161, 1493.268439024361669, 206.6147278250968213 ) ) ;
#71268 = CARTESIAN_POINT ( 'NONE',  ( -3.200208250563545853, 1370.366478648552174, 206.6667948705140532 ) ) ;
#71269 = CARTESIAN_POINT ( 'NONE',  ( -8.604402833090000868, 1384.931574737560140, 199.8686422932590006 ) ) ;
#71270 = CIRCLE ( 'NONE', #35498, 15.40132948099999943 ) ;
#71271 = EDGE_CURVE ( 'NONE', #54363, #5297, #45849, .T. ) ;
#71272 = CARTESIAN_POINT ( 'NONE',  ( -23.89076775359999871, 1410.242936723630010, 208.6635434592330114 ) ) ;
#71273 = ADVANCED_FACE ( 'NONE', ( #46615 ), #54541, .F. ) ;
#71274 = ADVANCED_FACE ( 'NONE', ( #30874 ), #5126, .T. ) ;
#71275 = CARTESIAN_POINT ( 'NONE',  ( 13.77266209894789917, 1517.051704408389924, 201.2043266506040027 ) ) ;
#71276 = CIRCLE ( 'NONE', #3320, 12.49965726619999984 ) ;
#71277 = CARTESIAN_POINT ( 'NONE',  ( 16.66936639845631873, 1523.456872492435195, 180.4828114240739581 ) ) ;
#71278 = CARTESIAN_POINT ( 'NONE',  ( 2.372478608332516892, 1501.977400791986611, 243.3440112565233449 ) ) ;
#71279 = EDGE_CURVE ( 'NONE', #48668, #45161, #40466, .T. ) ;
#71280 = CARTESIAN_POINT ( 'NONE',  ( 23.45078998690000205, 1410.227208243830091, 211.3297003749379996 ) ) ;
#71281 = CARTESIAN_POINT ( 'NONE',  ( -106.4226887258490137, 1391.913060387289988, 304.6216818903239414 ) ) ;
#71282 = ADVANCED_FACE ( 'NONE', ( #68370 ), #10662, .F. ) ;
#71283 = CARTESIAN_POINT ( 'NONE',  ( -2.515588616550900269, 1448.349620516269852, 188.5842437137009995 ) ) ;
#71284 = CARTESIAN_POINT ( 'NONE',  ( 17.17760792425680094, 1517.051704368240053, 222.7507317666290305 ) ) ;
#71286 = CARTESIAN_POINT ( 'NONE',  ( -14.17772863140000084, 1379.591530680210099, 207.8208987399890191 ) ) ;
#71285 = CARTESIAN_POINT ( 'NONE',  ( -27.43355922089999765, 1507.980920696029898, 210.8261541407979962 ) ) ;
#71287 = CARTESIAN_POINT ( 'NONE',  ( 1.071447408489999864, 1411.670163745530090, 232.9832474924979806 ) ) ;
#71288 = CARTESIAN_POINT ( 'NONE',  ( -123.2094608543013834, 1377.418846546388522, 298.8629130685377504 ) ) ;
#71289 = CARTESIAN_POINT ( 'NONE',  ( 1766.069695707609526, -8382.262153571264207, 2383.103299250912187 ) ) ;
#71290 = CARTESIAN_POINT ( 'NONE',  ( -23.23815859999999844, 1425.880866807129905, 211.7841193188579894 ) ) ;
#71291 = CARTESIAN_POINT ( 'NONE',  ( -1.499738582814070131, 1420.769031529490121, 184.5716992340250044 ) ) ;
#71292 = CARTESIAN_POINT ( 'NONE',  ( -7.721907926364999675, 1517.026025493960105, 204.1173703575669833 ) ) ;
#71293 = CARTESIAN_POINT ( 'NONE',  ( 13.37370059936500155, 1507.528266836789953, 233.0489815920269905 ) ) ;
#71294 = CARTESIAN_POINT ( 'NONE',  ( -16.37199061016699986, 1485.898763490840111, 187.4707436738999888 ) ) ;
#71295 = CARTESIAN_POINT ( 'NONE',  ( 11.46366843843170003, 1502.128415927390051, 212.5217899936770323 ) ) ;
#71296 = CARTESIAN_POINT ( 'NONE',  ( -14.98674809609716263, 1420.597066439330092, 210.5912578852586989 ) ) ;
#71298 = ORIENTED_EDGE ( 'NONE', *, *, #101981, .F. ) ;
#71297 = CARTESIAN_POINT ( 'NONE',  ( -68.28298542711279140, 1379.746875315909847, 279.8596883230670187 ) ) ;
#71299 = EDGE_LOOP ( 'NONE', ( #98666, #70053 ) ) ;
#71300 = CARTESIAN_POINT ( 'NONE',  ( 27.36865155859999987, 1509.161448955630021, 214.5593760264079890 ) ) ;
#71301 = ORIENTED_EDGE ( 'NONE', *, *, #54069, .T. ) ;
#71302 = CARTESIAN_POINT ( 'NONE',  ( 0.02352154200225501854, 1457.675724657883848, 199.5853667110562242 ) ) ;
#71303 = CARTESIAN_POINT ( 'NONE',  ( -109.1314240389999952, 1384.941892907230113, 311.2645748072590095 ) ) ;
#71305 = CARTESIAN_POINT ( 'NONE',  ( 15.76326814482090199, 1409.463407968690035, 192.8551723846009907 ) ) ;
#71304 = CARTESIAN_POINT ( 'NONE',  ( 15.82232452675290091, 1415.565885647649793, 191.3713869796289941 ) ) ;
#71306 = CARTESIAN_POINT ( 'NONE',  ( 11.86716023049999968, 1432.353341358199941, 147.6509521729980179 ) ) ;
#71307 = EDGE_CURVE ( 'NONE', #96609, #100850, #79171, .T. ) ;
#71308 = B_SPLINE_CURVE_WITH_KNOTS ( 'NONE', 3,
 ( #61861, #43384, #95981, #19242, #77532, #33856 ),
 .UNSPECIFIED., .F., .F.,
 ( 4, 2, 4 ),
 ( 0.000000000000000000, 0.5000000000000000000, 1.000000000000000000 ),
 .UNSPECIFIED. ) ;
#71309 = CARTESIAN_POINT ( 'NONE',  ( -25.40499604889999929, 1451.786406054930239, 136.2913176118979948 ) ) ;
#71310 = CARTESIAN_POINT ( 'NONE',  ( -0.7443733913810010039, 1468.219489664089906, 219.4953987198990148 ) ) ;
#71311 = CARTESIAN_POINT ( 'NONE',  ( 15.60951394679999993, 1410.830427143530187, 227.1466297419979696 ) ) ;
#71312 = CARTESIAN_POINT ( 'NONE',  ( 5.011367946795000528, 1516.974592746400049, 212.5716232859570027 ) ) ;
#71313 = EDGE_CURVE ( 'NONE', #44698, #48553, #74267, .T. ) ;
#71314 = CARTESIAN_POINT ( 'NONE',  ( 41.18215094353789851, 1440.963619928870003, 134.0999999980659823 ) ) ;
#71315 = CARTESIAN_POINT ( 'NONE',  ( -10.78881813950000002, 1422.299201281090063, 210.6311831754890136 ) ) ;
#71316 = CARTESIAN_POINT ( 'NONE',  ( -0.5620977654635980203, 1416.851343899799986, 227.7685710128770040 ) ) ;
#71317 = ORIENTED_EDGE ( 'NONE', *, *, #52115, .F. ) ;
#71318 = CARTESIAN_POINT ( 'NONE',  ( -13.97985296220000073, 1420.196174967039951, 195.9955836506989897 ) ) ;
#71319 = CARTESIAN_POINT ( 'NONE',  ( -1.417680259639110041, 1431.646251614470202, 200.8417364822699938 ) ) ;
#71320 = EDGE_LOOP ( 'NONE', ( #76400, #32382, #3951 ) ) ;
#71321 = ORIENTED_EDGE ( 'NONE', *, *, #14450, .F. ) ;
#71322 = ADVANCED_FACE ( 'NONE', ( #78402 ), #12503, .T. ) ;
#71323 = EDGE_LOOP ( 'NONE', ( #23860, #82822, #654, #99500 ) ) ;
#71324 = CARTESIAN_POINT ( 'NONE',  ( -7.777075051915000259, 1512.220794350760116, 215.6496765134470195 ) ) ;
#71325 = CARTESIAN_POINT ( 'NONE',  ( 16.48452149413872547, 1514.266850628232305, 194.7220678386542261 ) ) ;
#71326 = CARTESIAN_POINT ( 'NONE',  ( 19.34610958727051155, 1451.004559698421644, 146.2861324281605278 ) ) ;
#71327 = B_SPLINE_CURVE_WITH_KNOTS ( 'NONE', 5,
 ( #54696, #20486, #87168, #19389, #63650, #28363 ),
 .UNSPECIFIED., .F., .F.,
 ( 6, 6 ),
 ( 0.000000000000000000, 1.000000000000000000 ),
 .UNSPECIFIED. ) ;
#71328 = CARTESIAN_POINT ( 'NONE',  ( -2.896892189909999971, 1484.263391075629897, 183.3160938871980079 ) ) ;
#71329 = CARTESIAN_POINT ( 'NONE',  ( 2.340033977622370198, 1466.009485822560009, 198.3389262314019845 ) ) ;
#71330 = CARTESIAN_POINT ( 'NONE',  ( -13.88298926620000096, 1379.761820614679891, 208.2296881040550147 ) ) ;
#71331 = CARTESIAN_POINT ( 'NONE',  ( -3.827327205999999649, 1409.546157813730133, 146.1721969590979882 ) ) ;
#71332 = CARTESIAN_POINT ( 'NONE',  ( 4.246950514239129504, 1446.447518977580103, 161.6227665976579715 ) ) ;
#71333 = CARTESIAN_POINT ( 'NONE',  ( 0.3572670465939999929, 1508.337857058129885, 237.7796338305979873 ) ) ;
#71334 = ORIENTED_EDGE ( 'NONE', *, *, #106995, .F. ) ;
#71335 = CARTESIAN_POINT ( 'NONE',  ( -0.7579263249019989601, 1516.927039499179955, 207.4176752179770347 ) ) ;
#71336 = ORIENTED_EDGE ( 'NONE', *, *, #30765, .F. ) ;
#71337 = CARTESIAN_POINT ( 'NONE',  ( 32.06566495267949790, 1440.913060387330006, 256.0678710581919972 ) ) ;
#71338 = CARTESIAN_POINT ( 'NONE',  ( 11.76014171143800091, 1479.338753478690023, 208.6264959333659874 ) ) ;
#71339 = ORIENTED_EDGE ( 'NONE', *, *, #1464, .F. ) ;
#71340 = CARTESIAN_POINT ( 'NONE',  ( -33.91369269983620427, 1450.440666099120108, 136.2454419983430114 ) ) ;
#71341 = CARTESIAN_POINT ( 'NONE',  ( -13.97246758180000015, 1409.902985965229846, 190.4217242322980042 ) ) ;
#71342 = DIRECTION ( 'NONE',  ( 0.000000000000000000, 0.000000000000000000, 1.000000000000000000 ) ) ;
#71344 = CARTESIAN_POINT ( 'NONE',  ( 6.826689052339999897, 1469.354294130389917, 209.2233868860279813 ) ) ;
#71343 = CARTESIAN_POINT ( 'NONE',  ( -24.67000125460000248, 1440.968500227289951, 210.6876455135279969 ) ) ;
#71345 = CARTESIAN_POINT ( 'NONE',  ( 22.53427855600670071, 1410.990232248750090, 206.1996399176450154 ) ) ;
#71346 = CARTESIAN_POINT ( 'NONE',  ( -3.286480964850000408, 1456.341185808290220, 218.0120306903490075 ) ) ;
#71347 = CARTESIAN_POINT ( 'NONE',  ( 27.69925877688100258, 1441.434395746940027, 137.3015763641899980 ) ) ;
#71348 = FACE_OUTER_BOUND ( 'NONE', #94844, .T. ) ;
#71349 = CARTESIAN_POINT ( 'NONE',  ( 18.17633956390000094, 1435.132278384110123, 145.0981326318980109 ) ) ;
#71351 = CARTESIAN_POINT ( 'NONE',  ( -16.32163040922650055, 1507.551697810010182, 213.4489835936819873 ) ) ;
#71350 = CARTESIAN_POINT ( 'NONE',  ( 6.314283035290000790, 1463.997681713329939, 235.6565739224980121 ) ) ;
#71352 = B_SPLINE_CURVE_WITH_KNOTS ( 'NONE', 3,
 ( #1669, #95710, #45334, #18976, #53173, #87883, #44779, #71663, #96828, #54831, #10045, #19542, #105221, #70542, #61039, #11706, #72194, #87315, #37461, #29066, #10610, #36350, #62139, #80016, #35810, #104659, #95162, #18419, #62709, #52619, #69992, #20097, #27956, #78929, #44218, #78361 ),
 .UNSPECIFIED., .F., .F.,
 ( 4, 2, 2, 1, 1, 1, 1, 2, 2, 2, 2, 1, 1, 2, 2, 2, 2, 1, 1, 2, 2, 4 ),
 ( 0.000000000000000000, 0.1249999999996103950, 0.1874999999994146627, 0.2187499999993167688, 0.2343749999992800759, 0.2421874999992680855, 0.2460937499992680855, 0.2480468749992686128, 0.2499999999992691957, 0.3749999999996406208, 0.4374999999998094857, 0.4687499999998851474, 0.4843749999999223399, 0.4921874999999306666, 0.4999999999999389377, 0.6249999999998843148, 0.6874999999998553379, 0.7187499999998425704, 0.7343749999998377964, 0.7421874999998345768, 0.7499999999998312461, 1.000000000000000000 ),
 .UNSPECIFIED. ) ;
#71353 = CIRCLE ( 'NONE', #40909, 1.999999999999942935 ) ;
#71354 = CARTESIAN_POINT ( 'NONE',  ( -4.615644842514999624, 1517.009964551830080, 216.0692237534070159 ) ) ;
#71355 = CIRCLE ( 'NONE', #101641, 10.00000000000000888 ) ;
#71356 = CARTESIAN_POINT ( 'NONE',  ( 11.73653109249999993, 1426.280329148629789, 144.1709412064980143 ) ) ;
#71357 = CARTESIAN_POINT ( 'NONE',  ( 6.265221788440870299, 1511.198033794599951, 216.5696572527920125 ) ) ;
#71358 = AXIS2_PLACEMENT_3D ( 'NONE', #67194, #52600, #87862 ) ;
#71359 = CARTESIAN_POINT ( 'NONE',  ( 28.78960601649999873, 1509.588732904530161, 208.4412888571310134 ) ) ;
#71360 = CARTESIAN_POINT ( 'NONE',  ( -2.283570671295000132, 1516.909589401870107, 212.0033943946770023 ) ) ;
#71361 = CARTESIAN_POINT ( 'NONE',  ( -20.71063674839999891, 1470.804162801530083, 208.8514674448739754 ) ) ;
#71362 =( BOUNDED_CURVE ( )  B_SPLINE_CURVE ( 3, ( #4442, #47001, #22854, #57060 ),
 .UNSPECIFIED., .F., .F. ) 
 B_SPLINE_CURVE_WITH_KNOTS ( ( 4, 4 ),
 ( 3.464045754873669836, 3.751191316916064888 ),
 .UNSPECIFIED. ) 
 CURVE ( )  GEOMETRIC_REPRESENTATION_ITEM ( )  RATIONAL_B_SPLINE_CURVE ( ( 1.000000000000000000, 0.9931407469010118394, 0.9931407469010118394, 1.000000000000000000 ) ) 
 REPRESENTATION_ITEM ( '' )  );
#71363 = CARTESIAN_POINT ( 'NONE',  ( 7.622520388263168911, 1452.679533476516099, 191.4523119007226910 ) ) ;
#71365 = ORIENTED_EDGE ( 'NONE', *, *, #4346, .T. ) ;
#71364 = CARTESIAN_POINT ( 'NONE',  ( -94.46405900630000474, 1386.760127987169881, 294.9897091881589972 ) ) ;
#71366 = CARTESIAN_POINT ( 'NONE',  ( -17.53714238134516279, 1524.871836253796346, 237.4423643566621536 ) ) ;
#71367 = CARTESIAN_POINT ( 'NONE',  ( 4.694071664390000009, 1465.143864797330025, 238.2947585048979988 ) ) ;
#71368 = CARTESIAN_POINT ( 'NONE',  ( -9.202353836351246485, 1488.302798331107169, 217.0664070768366969 ) ) ;
#71369 = CARTESIAN_POINT ( 'NONE',  ( -20.11385680769999951, 1487.601373209189887, 204.1067431612489997 ) ) ;
#71370 = CARTESIAN_POINT ( 'NONE',  ( 11.22085813615770000, 1414.913060387329779, 197.6243702374680140 ) ) ;
#71371 = CARTESIAN_POINT ( 'NONE',  ( -20.92345263760000051, 1454.438554760929946, 223.3898966321980026 ) ) ;
#71372 = ADVANCED_FACE ( 'NONE', ( #106892 ), #91202, .T. ) ;
#71374 = CARTESIAN_POINT ( 'NONE',  ( 5.386491384805029980, 1432.359961415570069, 154.6077504147789909 ) ) ;
#71373 = CARTESIAN_POINT ( 'NONE',  ( -21.53807511146743181, 1411.025645835263049, 201.1588749450977218 ) ) ;
#71375 = CARTESIAN_POINT ( 'NONE',  ( -8.972902429201688790, 1449.183751661920041, 211.0003755984220106 ) ) ;
#71376 = CARTESIAN_POINT ( 'NONE',  ( -106.4468452320000011, 1379.239802504850104, 307.9198481384590309 ) ) ;
#71377 = CIRCLE ( 'NONE', #85605, 7.513435694540000043 ) ;
#71378 = ORIENTED_EDGE ( 'NONE', *, *, #46258, .F. ) ;
#71379 = CARTESIAN_POINT ( 'NONE',  ( -3.458526536014999930, 1516.742629295279812, 204.1242721449069961 ) ) ;
#71380 = CARTESIAN_POINT ( 'NONE',  ( 1.749310115339999916, 1406.801363622329973, 269.6491151137980182 ) ) ;
#71381 = EDGE_CURVE ( 'NONE', #83342, #21777, #50027, .T. ) ;
#71382 = CARTESIAN_POINT ( 'NONE',  ( -0.008738962350170510068, 1515.558522550590169, 213.2765912358790104 ) ) ;
#71383 = CARTESIAN_POINT ( 'NONE',  ( 39.57252994079590280, 1456.675038565810155, 270.2586952983279502 ) ) ;
#71384 = CARTESIAN_POINT ( 'NONE',  ( -23.74108753817469974, 1436.296634041249945, 212.5883363871789982 ) ) ;
#71385 = CARTESIAN_POINT ( 'NONE',  ( 20.54534055259999903, 1497.714303034489831, 214.2326470396490095 ) ) ;
#71386 = CARTESIAN_POINT ( 'NONE',  ( -42.90581327332729700, 1440.913060410159915, 263.0724741836789917 ) ) ;
#71387 = ADVANCED_FACE ( 'NONE', ( #99036, #47018 ), #66589, .T. ) ;
#71388 = CARTESIAN_POINT ( 'NONE',  ( -12.53380580351000084, 1442.773887400870080, 185.9733686700720057 ) ) ;
#71389 = CARTESIAN_POINT ( 'NONE',  ( 1.367072583474315595, 1450.698607345994787, 154.2613738994832033 ) ) ;
#71390 = DIRECTION ( 'NONE',  ( -0.09762373801881200908, -0.1163955094263306178, 0.9883934900436258664 ) ) ;
#71391 = CARTESIAN_POINT ( 'NONE',  ( -1.218484030269072260, 1451.352790354969784, 183.4814141672358119 ) ) ;
#71392 = CARTESIAN_POINT ( 'NONE',  ( -21.75649307329753768, 1524.201670966335769, 183.4206095899358218 ) ) ;
#71393 = CARTESIAN_POINT ( 'NONE',  ( -4.138993644310000164, 1515.551749209589843, 209.4962531541799819 ) ) ;
#71394 = EDGE_LOOP ( 'NONE', ( #47314, #49482, #29128, #96710 ) ) ;
#71395 = CARTESIAN_POINT ( 'NONE',  ( -9.019386504720001696, 1419.938649402030023, 248.0989693098979956 ) ) ;
#71396 = CARTESIAN_POINT ( 'NONE',  ( 10.70401247158669911, 1470.123045870449914, 207.0335124537880063 ) ) ;
#71397 = CARTESIAN_POINT ( 'NONE',  ( -1.328227237909999969, 1475.823473844229966, 266.9604901357979543 ) ) ;
#71398 = DIRECTION ( 'NONE',  ( -1.755985294532469921E-16, 1.000000000000000000, -1.338183447452831989E-16 ) ) ;
#71399 = CARTESIAN_POINT ( 'NONE',  ( -28.04656858090000071, 1508.051246290529889, 210.1181873726100093 ) ) ;
#71400 = CARTESIAN_POINT ( 'NONE',  ( -4.487249772970000272, 1509.038615934189920, 209.1218459608020055 ) ) ;
#71401 = CARTESIAN_POINT ( 'NONE',  ( -35.39279618899279711, 1384.807458296239929, 234.7559858425150026 ) ) ;
#71402 = B_SPLINE_SURFACE_WITH_KNOTS ( 'NONE', 5, 1, ( 
 ( #91973, #50540 ),
 ( #41016, #6319 ),
 ( #41584, #66803 ),
 ( #92513, #7964 ),
 ( #76836, #51090 ),
 ( #49982, #33708 ) ),
 .UNSPECIFIED., .F., .F., .F.,
 ( 6, 6 ),
 ( 2, 2 ),
 ( 0.000000000000000000, 3.920049511110000218 ),
 ( 0.000000000000000000, 14.00000000000000000 ),
 .UNSPECIFIED. ) ;
#71403 = CARTESIAN_POINT ( 'NONE',  ( -17.86855543449999928, 1415.163755998629995, 207.5652616391579954 ) ) ;
#71404 = B_SPLINE_CURVE_WITH_KNOTS ( 'NONE', 3,
 ( #68436, #33689, #25830, #75720, #42660, #34804, #84099, #85753, #67883, #76815, #109866, #33143, #49963, #67332, #101430, #93590, #68992, #8486, #59479, #60031, #24721, #15227, #93049, #16866, #51069, #50523, #94149, #51618, #103093, #6837, #86862, #95814, #9595, #69545, #43765, #104217, #26964, #80114, #71198, #2888, #78471, #10720, #104770, #44891, #18532, #96370, #52727, #103666, #53285 ),
 .UNSPECIFIED., .F., .F.,
 ( 4, 3, 3, 3, 3, 3, 3, 3, 3, 3, 3, 3, 3, 3, 3, 3, 4 ),
 ( -28.88939375100000007, -28.35496397148130043, -26.99855305397730021, -25.63863431757279798, -24.27724806815169956, -22.91518329866390147, -21.55400513323160183, -20.19477292252609857, -18.83849860325140213, -17.48889295550879908, -16.74086542361019880, -15.46648022024419866, -14.14486414810110126, -12.80329080502029981, -11.46594563996600158, -10.15626214476240108, -8.883338167809998964 ),
 .UNSPECIFIED. ) ;
#71405 = CARTESIAN_POINT ( 'NONE',  ( -10.91430100039999829, 1483.114603242489920, 204.3199828216889955 ) ) ;
#71406 = CARTESIAN_POINT ( 'NONE',  ( 26.62473440929639779, 1435.447231379140021, 135.5572024620289824 ) ) ;
#71407 = EDGE_CURVE ( 'NONE', #75744, #46325, #13390, .T. ) ;
#71408 = CARTESIAN_POINT ( 'NONE',  ( -11.06075986596750127, 1396.299310633010236, 208.6759994649900136 ) ) ;
#71409 = CARTESIAN_POINT ( 'NONE',  ( -15.64704939853400134, 1421.345936108949900, 227.1284707070510080 ) ) ;
#71410 = VECTOR ( 'NONE', #76148, 1000.000000000000227 ) ;
#71411 = CARTESIAN_POINT ( 'NONE',  ( -16.35500113143990220, 1409.585309854400066, 225.6783689361829772 ) ) ;
#71412 = CARTESIAN_POINT ( 'NONE',  ( -45.49575511559999796, 1438.180874202940004, 268.9785913983979526 ) ) ;
#71413 = CIRCLE ( 'NONE', #57075, 1.999999999999999556 ) ;
#71414 = VERTEX_POINT ( 'NONE', #64923 ) ;
#71415 = CARTESIAN_POINT ( 'NONE',  ( -1.022619748562719977, 1436.061388905930016, 227.5769040188990004 ) ) ;
#71416 = DIRECTION ( 'NONE',  ( -0.4025563316115431389, 0.03449475076686812219, -0.9147450530333514074 ) ) ;
#71417 = CARTESIAN_POINT ( 'NONE',  ( -14.13260639439999977, 1484.576036422829930, 186.6695759715979932 ) ) ;
#71419 = CARTESIAN_POINT ( 'NONE',  ( -12.56945278516500153, 1512.044075975079977, 193.8624433630670012 ) ) ;
#71418 = CARTESIAN_POINT ( 'NONE',  ( 11.41326510949999928, 1425.999523078630091, 128.4892991212979894 ) ) ;
#71420 = CARTESIAN_POINT ( 'NONE',  ( -0.2816376222929999895, 1499.119349190730190, 236.9843354826979862 ) ) ;
#71421 = CARTESIAN_POINT ( 'NONE',  ( -10.22077960920000095, 1448.827726244289806, 207.2905429624990177 ) ) ;
#71422 = EDGE_CURVE ( 'NONE', #90510, #99871, #82251, .T. ) ;
#71423 = CARTESIAN_POINT ( 'NONE',  ( -3.260378293205000055, 1516.582197289609894, 201.4115600944169842 ) ) ;
#71424 = CARTESIAN_POINT ( 'NONE',  ( 7.553999303160000345, 1425.256314220230024, 212.1065527620190210 ) ) ;
#71425 = CARTESIAN_POINT ( 'NONE',  ( -4.882003189570000679, 1430.559178934629927, 150.0077195948979920 ) ) ;
#71426 = CARTESIAN_POINT ( 'NONE',  ( 6.853204512189999598, 1508.129908978229878, 182.3155033407979886 ) ) ;
#71427 = DIRECTION ( 'NONE',  ( 0.07512831052118132402, 0.9801898970463382987, 0.1832580221614370231 ) ) ;
#71428 = CARTESIAN_POINT ( 'NONE',  ( -71.62438411370330016, 1379.712643069029809, 285.2199323073880350 ) ) ;
#71429 = AXIS2_PLACEMENT_3D ( 'NONE', #109196, #59901, #58784 ) ;
#71430 = CARTESIAN_POINT ( 'NONE',  ( 4.901453889304693057, 1367.619533116579305, 210.6218459617142003 ) ) ;
#71431 = EDGE_CURVE ( 'NONE', #66206, #79432, #89850, .T. ) ;
#71433 = VERTEX_POINT ( 'NONE', #57634 ) ;
#71432 = CARTESIAN_POINT ( 'NONE',  ( 6.163562822530000318, 1453.283431879389809, 216.1943447892690244 ) ) ;
#71434 = ORIENTED_EDGE ( 'NONE', *, *, #58534, .T. ) ;
#71435 = CARTESIAN_POINT ( 'NONE',  ( -12.51070046275587266, 1447.046588421757406, 187.7237876303275641 ) ) ;
#71436 = VECTOR ( 'NONE', #21625, 1000.000000000000000 ) ;
#71437 = CARTESIAN_POINT ( 'NONE',  ( -15.94347048536829803, 1409.469818645040050, 192.9752432267480060 ) ) ;
#71438 = DIRECTION ( 'NONE',  ( 0.3741247022715693538, 0.04424963817041901309, -0.9263221236006385917 ) ) ;
#71439 = CARTESIAN_POINT ( 'NONE',  ( 4.304841658572250651, 1499.458000153912508, 198.5863174272942899 ) ) ;
#71441 = CARTESIAN_POINT ( 'NONE',  ( -1.367757481957880161, 1418.999489435819896, 185.2367492338790100 ) ) ;
#71440 = CARTESIAN_POINT ( 'NONE',  ( -9.129808330190000376, 1383.863787716949901, 218.5279287960690056 ) ) ;
#71442 = CARTESIAN_POINT ( 'NONE',  ( 6.200576079530000229, 1429.764427576630169, 185.9200482557980081 ) ) ;
#71443 = DIRECTION ( 'NONE',  ( 0.5877852522924743583, 0.000000000000000000, 0.8090169943749466741 ) ) ;
#71444 = CARTESIAN_POINT ( 'NONE',  ( -110.0634901748029932, 1384.899971912700039, 296.9512050915229793 ) ) ;
#71445 = CARTESIAN_POINT ( 'NONE',  ( -2.500000000000000000, 1448.206577425080013, 168.0218890593559991 ) ) ;
#71446 = CARTESIAN_POINT ( 'NONE',  ( -13.02571899038530567, 1435.353243946824477, 150.4465727419359951 ) ) ;
#71447 = PLANE ( 'NONE',  #12246 ) ;
#71448 = CARTESIAN_POINT ( 'NONE',  ( -11.75869035456349998, 1517.051704408389924, 190.9442076542370046 ) ) ;
#71449 = CARTESIAN_POINT ( 'NONE',  ( 0.000000000000000000, 1405.413060387330006, 209.1218459616979999 ) ) ;
#71450 = VERTEX_POINT ( 'NONE', #98495 ) ;
#71451 = CARTESIAN_POINT ( 'NONE',  ( -16.73628186595857059, 1526.382868172864164, 184.0591879540917546 ) ) ;
#71452 = CARTESIAN_POINT ( 'NONE',  ( 21.45462491533043803, 1525.320849883649316, 233.4406507496946972 ) ) ;
#71453 = ORIENTED_EDGE ( 'NONE', *, *, #51655, .F. ) ;
#71454 = ADVANCED_FACE ( 'NONE', ( #24530 ), #71533, .T. ) ;
#71455 = VERTEX_POINT ( 'NONE', #82050 ) ;
#71456 = CARTESIAN_POINT ( 'NONE',  ( -3.617198352219999968, 1454.554796268290147, 200.0420705370489998 ) ) ;
#71457 = CARTESIAN_POINT ( 'NONE',  ( -8.624710350820000926, 1367.191948709370081, 207.6218459616989946 ) ) ;
#71458 = AXIS2_PLACEMENT_3D ( 'NONE', #99795, #4123, #66244 ) ;
#71459 = EDGE_CURVE ( 'NONE', #92224, #40681, #75132, .T. ) ;
#71460 = CARTESIAN_POINT ( 'NONE',  ( -2.869693497065000098, 1517.070197312179971, 214.9093229647470196 ) ) ;
#71461 = CARTESIAN_POINT ( 'NONE',  ( 2.392017048025000037, 1512.336926113599930, 216.7209653789669801 ) ) ;
#71462 = EDGE_LOOP ( 'NONE', ( #105335, #93156, #46779, #33148, #39293 ) ) ;
#71463 = CARTESIAN_POINT ( 'NONE',  ( 7.904651180169999236, 1423.075284537190100, 213.5785853047590024 ) ) ;
#71464 = CARTESIAN_POINT ( 'NONE',  ( -87.79856897099999458, 1374.577971548089863, 299.2711673883590038 ) ) ;
#71465 = CARTESIAN_POINT ( 'NONE',  ( 12.26986170129999998, 1416.828040559629926, 223.5793159245980064 ) ) ;
#71466 = CARTESIAN_POINT ( 'NONE',  ( -0.7568987378019988999, 1516.805675336850072, 205.0906771642370074 ) ) ;
#71467 = CARTESIAN_POINT ( 'NONE',  ( -39.71894992190000551, 1440.913060387330006, 267.1764892454980327 ) ) ;
#71468 = FACE_OUTER_BOUND ( 'NONE', #100509, .T. ) ;
#71469 = CARTESIAN_POINT ( 'NONE',  ( -4.331002755570000140, 1409.231591811829958, 231.5156777643979922 ) ) ;
#71471 = ORIENTED_EDGE ( 'NONE', *, *, #3817, .T. ) ;
#71470 = CARTESIAN_POINT ( 'NONE',  ( 2.469061732649111107, 1524.816846803860926, 175.8590321262562952 ) ) ;
#71472 = CARTESIAN_POINT ( 'NONE',  ( -27.95545114004499965, 1508.164280454029949, 210.3124796796069802 ) ) ;
#71473 = CARTESIAN_POINT ( 'NONE',  ( 17.66551557756463353, 1517.051704408389924, 217.9010776241849214 ) ) ;
#71474 = CARTESIAN_POINT ( 'NONE',  ( -1.808737572104399227, 1485.212291744892127, 182.6011977422664927 ) ) ;
#71475 = CYLINDRICAL_SURFACE ( 'NONE', #101694, 2.000000000000003553 ) ;
#71476 = CARTESIAN_POINT ( 'NONE',  ( 20.73365673480000027, 1411.792342831829956, 270.3294707265980037 ) ) ;
#71477 = CARTESIAN_POINT ( 'NONE',  ( 4.041472473744999405, 1516.858649670339901, 213.1514186109370144 ) ) ;
#71478 = AXIS2_PLACEMENT_3D ( 'NONE', #51067, #96927, #11810 ) ;
#71479 = CARTESIAN_POINT ( 'NONE',  ( -67.99787016330000711, 1379.746136258720071, 278.4829519276589735 ) ) ;
#71480 = CARTESIAN_POINT ( 'NONE',  ( 0.01553491999268000710, 1507.764438927018546, 237.4914441325955465 ) ) ;
#71481 = CARTESIAN_POINT ( 'NONE',  ( -30.29139619033233544, 1523.843263703803814, 222.4926162074647777 ) ) ;
#71482 = CARTESIAN_POINT ( 'NONE',  ( -21.59687499341919903, 1507.523464219199923, 209.4572686751589856 ) ) ;
#71483 = CARTESIAN_POINT ( 'NONE',  ( 4.618583391875000110, 1516.939762005280045, 209.1087859301640322 ) ) ;
#71484 = ORIENTED_EDGE ( 'NONE', *, *, #3509, .T. ) ;
#71485 = CARTESIAN_POINT ( 'NONE',  ( 4.199282754958249875, 1421.058089936039778, 185.3644816151839905 ) ) ;
#71486 = CARTESIAN_POINT ( 'NONE',  ( -0.9715279139649999340, 1417.917963001030103, 233.3865104881980130 ) ) ;
#71487 = CARTESIAN_POINT ( 'NONE',  ( -96.24131551039999977, 1384.723465092230072, 310.5839496812590141 ) ) ;
#71488 = ORIENTED_EDGE ( 'NONE', *, *, #66667, .T. ) ;
#71489 = CARTESIAN_POINT ( 'NONE',  ( -32.15151909282970877, 1385.223364821960104, 230.4497740801809869 ) ) ;
#71490 = CIRCLE ( 'NONE', #66113, 1.500000000000014433 ) ;
#71491 = FACE_OUTER_BOUND ( 'NONE', #51288, .T. ) ;
#71492 = PRODUCT ( 'Handle Mounting Screw', 'Handle Mounting Screw', '', ( #41524 ) ) ;
#71493 = CARTESIAN_POINT ( 'NONE',  ( 12.81251879674629990, 1488.404633894339895, 232.3873005381080077 ) ) ;
#71494 =( BOUNDED_CURVE ( )  B_SPLINE_CURVE ( 3, ( #90624, #81661, #22293, #6075 ),
 .UNSPECIFIED., .F., .F. ) 
 B_SPLINE_CURVE_WITH_KNOTS ( ( 4, 4 ),
 ( 4.143391436656575166, 5.281615214968810257 ),
 .UNSPECIFIED. ) 
 CURVE ( )  GEOMETRIC_REPRESENTATION_ITEM ( )  RATIONAL_B_SPLINE_CURVE ( ( 1.000000000000000000, 0.8949199307684150284, 0.8949199307684150284, 1.000000000000000000 ) ) 
 REPRESENTATION_ITEM ( '' )  );
#71495 = CARTESIAN_POINT ( 'NONE',  ( 19.28393622879999825, 1507.737928638330004, 188.6540313642980209 ) ) ;
#71496 = DIRECTION ( 'NONE',  ( 0.8090169943749422332, -0.000000000000000000, -0.5877852522924802425 ) ) ;
#71497 = CARTESIAN_POINT ( 'NONE',  ( -18.51436573157398158, 1511.187213306747708, 181.1015051776554969 ) ) ;
#71498 = CARTESIAN_POINT ( 'NONE',  ( 2.715010028530000064, 1417.669881552329798, 234.6652376653979957 ) ) ;
#71499 = EDGE_CURVE ( 'NONE', #56418, #44154, #53648, .T. ) ;
#71501 = CARTESIAN_POINT ( 'NONE',  ( -7.709253412061816135, 1516.542698385629819, 211.7357737058638918 ) ) ;
#71500 = CARTESIAN_POINT ( 'NONE',  ( -7.714371541114999786, 1516.738222552470233, 214.9014490703569891 ) ) ;
#71502 = CARTESIAN_POINT ( 'NONE',  ( -5.433843300390170050, 1391.480867605439926, 214.9027815983120036 ) ) ;
#71503 = CARTESIAN_POINT ( 'NONE',  ( 10.54077562621580100, 1470.446268097909751, 208.9023493837970022 ) ) ;
#71504 = ORIENTED_EDGE ( 'NONE', *, *, #61306, .T. ) ;
#71505 = CARTESIAN_POINT ( 'NONE',  ( -0.01010286742719850028, 1516.939452820819952, 201.4022050290969901 ) ) ;
#71506 = CARTESIAN_POINT ( 'NONE',  ( -11.46637696920000060, 1485.913060386929828, 183.3557477887979985 ) ) ;
#71507 = VERTEX_POINT ( 'NONE', #15392 ) ;
#71508 = TOROIDAL_SURFACE ( 'NONE', #94714, 12.73448142120000171, 1.000000000000000000 ) ;
#71509 = CARTESIAN_POINT ( 'NONE',  ( 3.835404308833624043, 1396.046995657106436, 216.1425064568209677 ) ) ;
#71510 = CARTESIAN_POINT ( 'NONE',  ( 18.20258715539999983, 1429.723789929190161, 209.1218459616989946 ) ) ;
#71511 = CARTESIAN_POINT ( 'NONE',  ( 8.769368648193829330, 1511.501844456730169, 203.3371675829959884 ) ) ;
#71512 = CARTESIAN_POINT ( 'NONE',  ( 2.026941135499999991, 1442.331840242090038, 218.1303087973689969 ) ) ;
#71513 = CARTESIAN_POINT ( 'NONE',  ( -26.45794170912690291, 1508.569471461619969, 201.4995158287420054 ) ) ;
#71514 = ADVANCED_FACE ( 'NONE', ( #40611 ), #104531, .F. ) ;
#71515 = CARTESIAN_POINT ( 'NONE',  ( -2.715357302349999724, 1447.820972450259887, 154.4673902286979796 ) ) ;
#71516 = CARTESIAN_POINT ( 'NONE',  ( -18.35233659730000255, 1424.971321547430080, 225.5691796496979862 ) ) ;
#71517 = CARTESIAN_POINT ( 'NONE',  ( -15.06148604940000091, 1435.839581580419917, 149.4729251189979777 ) ) ;
#71518 = CARTESIAN_POINT ( 'NONE',  ( -0.5845692370331438958, 1467.807727929299972, 230.0158462584300025 ) ) ;
#71519 = CARTESIAN_POINT ( 'NONE',  ( 16.32486700269999957, 1418.999550187130126, 191.2653796169979898 ) ) ;
#71521 = CARTESIAN_POINT ( 'NONE',  ( -18.44100721514212537, 1436.486662365291750, 212.9983258236653683 ) ) ;
#71520 = CARTESIAN_POINT ( 'NONE',  ( 0.1697262053381299873, 1408.918987357010110, 231.7543611685260032 ) ) ;
#71522 = CARTESIAN_POINT ( 'NONE',  ( -10.13169652023110068, 1472.475396586130046, 210.1560152870009688 ) ) ;
#71523 = ORIENTED_EDGE ( 'NONE', *, *, #91702, .T. ) ;
#71524 = CARTESIAN_POINT ( 'NONE',  ( -0.2626388803150430107, 1424.255108698730055, 227.7923674800080107 ) ) ;
#71525 = CARTESIAN_POINT ( 'NONE',  ( -8.256084004110000762, 1508.551704433089981, 218.9904985306490062 ) ) ;
#71526 = DIRECTION ( 'NONE',  ( 0.000000000000000000, -6.123233995736799316E-17, -1.000000000000000000 ) ) ;
#71527 = FACE_OUTER_BOUND ( 'NONE', #42424, .T. ) ;
#71528 = CARTESIAN_POINT ( 'NONE',  ( -2.979329921729999775, 1485.440599754389950, 197.5893634892990178 ) ) ;
#71529 = AXIS2_PLACEMENT_3D ( 'NONE', #32257, #4842, #83758 ) ;
#71530 = CARTESIAN_POINT ( 'NONE',  ( -18.58455358810000035, 1509.562047299329834, 231.7122880195979917 ) ) ;
#71531 = CARTESIAN_POINT ( 'NONE',  ( 11.60004869885203682, 1426.786827912535728, 134.3786173235958472 ) ) ;
#71532 = CARTESIAN_POINT ( 'NONE',  ( 19.68294476550000027, 1431.113060387329824, 210.0974834526720088 ) ) ;
#71533 = B_SPLINE_SURFACE_WITH_KNOTS ( 'NONE', 5, 5, ( 
 ( #76067, #41913, #32941, #59286, #110210, #68794 ),
 ( #7748, #84996, #15569, #101793, #102355, #26193 ),
 ( #58718, #485, #93951, #76613, #50867, #51413 ),
 ( #85545, #33483, #93404, #25083, #77182, #60381 ),
 ( #8291, #8841, #43024, #16669, #92299, #110765 ),
 ( #25638, #50335, #67685, #102894, #42454, #34608 ),
 ( #17218, #84461, #34055, #23976, #92853, #49771 ),
 ( #68247, #59830, #58170, #83902, #16129, #7208 ),
 ( #41364, #75531, #109666, #67131, #101230, #108371 ) ),
 .UNSPECIFIED., .F., .F., .F.,
 ( 6, 3, 6 ),
 ( 6, 6 ),
 ( 3.959746331690000343, 7.829449941020000026, 12.95412177010000043 ),
 ( 0.000000000000000000, 2.000000000000000000 ),
 .UNSPECIFIED. ) ;
#71534 = DIRECTION ( 'NONE',  ( 0.000000000000000000, 1.000000000000000000, 0.000000000000000000 ) ) ;
#71535 = CARTESIAN_POINT ( 'NONE',  ( -14.24649929728060016, 1509.423840198609923, 183.1703963639310189 ) ) ;
#71536 = CARTESIAN_POINT ( 'NONE',  ( -7.889194276409699391, 1488.589073438359947, 217.2869014410679824 ) ) ;
#71537 = CARTESIAN_POINT ( 'NONE',  ( 4.803837674189999518, 1471.771474222590086, 187.6888395837989947 ) ) ;
#71538 = CARTESIAN_POINT ( 'NONE',  ( -79.35849551933969792, 1383.777447801099925, 303.2169598375339774 ) ) ;
#71539 = CARTESIAN_POINT ( 'NONE',  ( -109.6045263617230034, 1384.282720651610134, 311.2785409792999758 ) ) ;
#71540 = CARTESIAN_POINT ( 'NONE',  ( 7.671689734580000142, 1427.928541111089999, 213.1259205237190031 ) ) ;
#71542 = ORIENTED_EDGE ( 'NONE', *, *, #39288, .F. ) ;
#71541 = CARTESIAN_POINT ( 'NONE',  ( -18.35946451589240169, 1443.345020097670158, 213.1741786437940220 ) ) ;
#71543 = VECTOR ( 'NONE', #23690, 1000.000000000000000 ) ;
#71544 = CARTESIAN_POINT ( 'NONE',  ( -81.53378978499999619, 1382.336709067400079, 304.3954627607590169 ) ) ;
#71545 = ADVANCED_FACE ( 'NONE', ( #85352 ), #37507, .T. ) ;
#71546 = CARTESIAN_POINT ( 'NONE',  ( 19.93293359290609956, 1508.855319075360057, 229.5871707258750121 ) ) ;
#71547 = ORIENTED_EDGE ( 'NONE', *, *, #88592, .F. ) ;
#71548 = VERTEX_POINT ( 'NONE', #27131 ) ;
#71549 = CARTESIAN_POINT ( 'NONE',  ( 16.63478241967279914, 1414.913060387399810, 210.4991047624779981 ) ) ;
#71550 = CARTESIAN_POINT ( 'NONE',  ( 13.45333203899999930, 1508.683642288930059, 233.3158433383979968 ) ) ;
#71551 = CARTESIAN_POINT ( 'NONE',  ( 12.60661500655967693, 1442.786586627101997, 169.4683401008484509 ) ) ;
#71553 = CARTESIAN_POINT ( 'NONE',  ( -27.70845756829999829, 1450.383242533360090, 238.1060645626980090 ) ) ;
#71552 = CARTESIAN_POINT ( 'NONE',  ( 41.21166932550332973, 1434.842932742385074, 269.6325636146803504 ) ) ;
#71554 = ADVANCED_FACE ( 'NONE', ( #103251 ), #67493, .T. ) ;
#71555 = CARTESIAN_POINT ( 'NONE',  ( -20.51560685680000162, 1505.131281290129891, 190.1532519183979844 ) ) ;
#71556 = CARTESIAN_POINT ( 'NONE',  ( -11.91229251400000066, 1433.393972783660047, 150.1287693233979894 ) ) ;
#71557 = ADVANCED_FACE ( 'NONE', ( #18155 ), #45584, .F. ) ;
#71558 = CARTESIAN_POINT ( 'NONE',  ( 26.64289581539999929, 1508.595173681330152, 204.0920109017480115 ) ) ;
#71559 = CARTESIAN_POINT ( 'NONE',  ( -19.06270802089999705, 1485.830083011429906, 189.5716758561979987 ) ) ;
#71560 = DIRECTION ( 'NONE',  ( 0.000000000000000000, -1.000000000000000000, 6.123233995736769734E-17 ) ) ;
#71561 = CARTESIAN_POINT ( 'NONE',  ( 5.174241722320000569, 1423.109489784829975, 185.3707530537979835 ) ) ;
#71562 = CARTESIAN_POINT ( 'NONE',  ( -24.39066168639999788, 1440.643119315069953, 211.3250814536579867 ) ) ;
#71563 = CARTESIAN_POINT ( 'NONE',  ( 6.017144064880000087, 1442.258634807139970, 154.7968030183980090 ) ) ;
#71564 = DIRECTION ( 'NONE',  ( -1.985713488479999930E-13, 1.181721098350000151E-14, 1.000000000000000000 ) ) ;
#71565 = ADVANCED_FACE ( 'NONE', ( #16416 ), #67819, .T. ) ;
#71566 = CARTESIAN_POINT ( 'NONE',  ( 0.02089856015480650100, 1507.111761549349922, 237.3522809668369860 ) ) ;
#71568 = ORIENTED_EDGE ( 'NONE', *, *, #98951, .T. ) ;
#71567 = CARTESIAN_POINT ( 'NONE',  ( 2.149988386126029882E-09, 1405.989059316979819, 266.9611530767110139 ) ) ;
#71569 = ORIENTED_EDGE ( 'NONE', *, *, #40687, .T. ) ;
#71570 = CARTESIAN_POINT ( 'NONE',  ( -12.97219746350000058, 1506.894675433090015, 209.2202028069119990 ) ) ;
#71571 = CARTESIAN_POINT ( 'NONE',  ( 16.63319105031239786, 1492.894349348930064, 193.2649508192429835 ) ) ;
#71572 = CARTESIAN_POINT ( 'NONE',  ( -10.49063443250000027, 1470.661302036229699, 269.6264949689979744 ) ) ;
#71573 = CARTESIAN_POINT ( 'NONE',  ( -7.878537825433329367, 1517.051704408389924, 218.1850669711710111 ) ) ;
#71574 = CARTESIAN_POINT ( 'NONE',  ( 2.331468351709999880E-15, 1435.943783413959864, 155.5249316174979981 ) ) ;
#71575 = CARTESIAN_POINT ( 'NONE',  ( -22.79764378385881329, 1411.075395676238713, 211.2310797118794596 ) ) ;
#71576 = CIRCLE ( 'NONE', #23228, 15.09021984820000029 ) ;
#71577 = CARTESIAN_POINT ( 'NONE',  ( 4.328404850859260300, 1515.104658776890119, 210.1767891407040167 ) ) ;
#71578 = CARTESIAN_POINT ( 'NONE',  ( 31.43069643840511773, 1526.748660780343471, 201.6857111062222998 ) ) ;
#71579 = CARTESIAN_POINT ( 'NONE',  ( -1.202518465757487220, 1484.679450086970292, 182.2456923944191374 ) ) ;
#71580 = CARTESIAN_POINT ( 'NONE',  ( 7.340269731167739842, 1361.836778001496214, 210.6218459616991936 ) ) ;
#71581 = CARTESIAN_POINT ( 'NONE',  ( -44.28103615880979760, 1432.290645226539709, 266.2283159212610144 ) ) ;
#71582 = CIRCLE ( 'NONE', #105509, 1.000000000000000888 ) ;
#71583 = EDGE_LOOP ( 'NONE', ( #97836, #4532, #45734, #66100, #23931 ) ) ;
#71584 = DIRECTION ( 'NONE',  ( 0.000000000000000000, 0.000000000000000000, 1.000000000000000000 ) ) ;
#71585 = EDGE_LOOP ( 'NONE', ( #26061, #75321, #73777, #81362 ) ) ;
#71586 = CARTESIAN_POINT ( 'NONE',  ( -2.282301616165000269, 1516.836638729160086, 210.8392784184970026 ) ) ;
#71587 = CARTESIAN_POINT ( 'NONE',  ( -9.299128358382350967, 1447.143969702200138, 212.1393002196799955 ) ) ;
#71588 = EDGE_CURVE ( 'NONE', #21389, #71450, #93148, .T. ) ;
#71589 = CARTESIAN_POINT ( 'NONE',  ( -21.33083225349999879, 1509.431387662330053, 190.3642105689980042 ) ) ;
#71590 = CARTESIAN_POINT ( 'NONE',  ( 7.133777758825489812, 1426.611815516710067, 213.1249336043190112 ) ) ;
#71591 = AXIS2_PLACEMENT_3D ( 'NONE', #78831, #63169, #86661 ) ;
#71592 = LINE ( 'NONE', #62635, #101875 ) ;
#71593 = EDGE_LOOP ( 'NONE', ( #37862, #31247, #42880 ) ) ;
#71594 = CARTESIAN_POINT ( 'NONE',  ( -3.355801963978114255, 1523.843263703804951, 176.1812209933808901 ) ) ;
#71595 = ADVANCED_FACE ( 'NONE', ( #33241 ), #8039, .F. ) ;
#71596 = CARTESIAN_POINT ( 'NONE',  ( 2.484577657225000014, 1517.170512887980067, 201.7834339727070017 ) ) ;
#71597 = CARTESIAN_POINT ( 'NONE',  ( 18.53418652026280000, 1507.620785850910124, 188.5293807599879869 ) ) ;
#71598 = CARTESIAN_POINT ( 'NONE',  ( -8.584430616891150834, 1438.454652122179823, 207.6921544452859791 ) ) ;
#71599 = ORIENTED_EDGE ( 'NONE', *, *, #40017, .T. ) ;
#71600 = CARTESIAN_POINT ( 'NONE',  ( -19.44407063118980261, 1410.830196386340049, 270.0540648103669810 ) ) ;
#71601 = CARTESIAN_POINT ( 'NONE',  ( 2.879318417774999972, 1516.995911393979895, 209.8571825100049750 ) ) ;
#71602 = CARTESIAN_POINT ( 'NONE',  ( 3.561272854136539934, 1416.011968391400160, 231.7883711070729760 ) ) ;
#71603 = CARTESIAN_POINT ( 'NONE',  ( 9.313029624468448731, 1435.254921036249925, 208.0259770765709959 ) ) ;
#71605 = ORIENTED_EDGE ( 'NONE', *, *, #95512, .T. ) ;
#71604 = CARTESIAN_POINT ( 'NONE',  ( -5.732728747552154225, 1366.653013508871254, 208.3718459617061285 ) ) ;
#71606 = ORIENTED_EDGE ( 'NONE', *, *, #81541, .F. ) ;
#71607 = CARTESIAN_POINT ( 'NONE',  ( 42.75061902808843683, 1452.888007040521416, 269.0553722311352658 ) ) ;
#71608 = CARTESIAN_POINT ( 'NONE',  ( 3.235048515759559873, 1466.472015849239824, 219.6884157167970102 ) ) ;
#71609 = CARTESIAN_POINT ( 'NONE',  ( 3.625945072265513769, 1424.652023359415125, 184.6562347036613403 ) ) ;
#71610 = AXIS2_PLACEMENT_3D ( 'NONE', #61888, #20384, #105520 ) ;
#71611 = CARTESIAN_POINT ( 'NONE',  ( 4.989246313819999834, 1471.909539260290103, 189.7082128665990126 ) ) ;
#71612 = B_SPLINE_SURFACE_WITH_KNOTS ( 'NONE', 5, 5, ( 
 ( #52594, #86728, #44188, #78330, #110265, #77241, #542, #68304, #24585 ),
 ( #33542, #8348, #43633, #34666, #68852, #102954, #94561, #9468, #77783 ),
 ( #29570, #3305, #36874, #45853, #2206, #81077, #19512, #4393, #79443 ),
 ( #80543, #97868, #104075, #96236, #37985, #69961, #27370, #53717, #78900 ),
 ( #61552, #27929, #53146, #54260, #54797, #72167, #63223, #95685, #87855 ),
 ( #37435, #106285, #2754, #87285, #62675, #18951, #62111, #45304, #21143 ) ),
 .UNSPECIFIED., .F., .F., .F.,
 ( 6, 6 ),
 ( 6, 3, 6 ),
 ( 3.271539800728220371, 6.921095641200810000 ),
 ( -3.659009177935479380E-05, 1.000000000000000000, 2.000000000000000000 ),
 .UNSPECIFIED. ) ;
#71613 = CARTESIAN_POINT ( 'NONE',  ( -5.614653854145000622, 1512.903985260039917, 216.7358144361969892 ) ) ;
#71614 = CARTESIAN_POINT ( 'NONE',  ( -21.20399697579999909, 1435.766733359059799, 220.8510379581979919 ) ) ;
#71615 = CARTESIAN_POINT ( 'NONE',  ( -14.11290024180000025, 1420.166582371130062, 221.9553848337980071 ) ) ;
#71616 = CARTESIAN_POINT ( 'NONE',  ( -1.697652520239993246, 1466.995205074520072, 235.3380831672032798 ) ) ;
#71617 = CARTESIAN_POINT ( 'NONE',  ( -17.53366249653573306, 1422.926247351624397, 226.4414695557952939 ) ) ;
#71618 = CARTESIAN_POINT ( 'NONE',  ( 6.546039395294999785, 1516.565291103010168, 206.8289057630870218 ) ) ;
#71619 = ORIENTED_EDGE ( 'NONE', *, *, #61025, .F. ) ;
#71620 = CARTESIAN_POINT ( 'NONE',  ( 0.2521604941109990006, 1444.846786543190092, 215.4142079403889909 ) ) ;
#71621 = CARTESIAN_POINT ( 'NONE',  ( -2.282008387128519278, 1516.544479074504125, 201.9748403303481439 ) ) ;
#71622 = EDGE_LOOP ( 'NONE', ( #25607, #108062, #96861, #1706 ) ) ;
#71623 = CARTESIAN_POINT ( 'NONE',  ( 10.13233719373625696, 1455.383656796513833, 226.4959039531065059 ) ) ;
#71624 = CARTESIAN_POINT ( 'NONE',  ( -27.68254001883949655, 1507.989615300039986, 210.5775529569929745 ) ) ;
#71625 = CARTESIAN_POINT ( 'NONE',  ( -9.173749095941850840, 1450.559996438570124, 208.1432995907519796 ) ) ;
#71626 = CARTESIAN_POINT ( 'NONE',  ( -50.84652256599999731, 1385.021217850319999, 226.1755936018590205 ) ) ;
#71627 = B_SPLINE_CURVE_WITH_KNOTS ( 'NONE', 3,
 ( #33044, #32512, #20107, #1129, #20640, #11185, #77820, #2249, #10055, #45346, #79485, #36913, #104671, #70552, #27405, #2792, #11718, #44229, #27965, #105794, #71107, #54300, #53183, #88428, #35259, #87893, #70004, #62149, #104118, #78941, #45889, #103561, #54842, #78373, #3347, #63259 ),
 .UNSPECIFIED., .F., .F.,
 ( 4, 2, 2, 1, 1, 1, 2, 2, 2, 2, 1, 1, 1, 2, 2, 2, 2, 1, 1, 2, 2, 4 ),
 ( 0.000000000000000000, 0.1250000000019153013, 0.1875000000029100888, 0.2187500000034410808, 0.2343750000037066461, 0.2421875000038058723, 0.2460937500038569148, 0.2500000000039079295, 0.3750000000046815885, 0.4375000000050380811, 0.4687500000052188254, 0.4843750000053117510, 0.4921875000053556604, 0.4960937500053528848, 0.5000000000053500537, 0.6250000000040984993, 0.6875000000034486858, 0.7187500000031239455, 0.7343750000029616309, 0.7421875000028802516, 0.7500000000027988722, 1.000000000000000000 ),
 .UNSPECIFIED. ) ;
#71628 = CARTESIAN_POINT ( 'NONE',  ( -6.416973687110000490, 1415.004829294899992, 206.0388214070289905 ) ) ;
#71629 = CARTESIAN_POINT ( 'NONE',  ( 19.40037511790000124, 1410.512935499930109, 196.1053253185980054 ) ) ;
#71630 = CARTESIAN_POINT ( 'NONE',  ( -2.804857515051331074, 1447.114276553103309, 170.5309535041508298 ) ) ;
#71631 = CARTESIAN_POINT ( 'NONE',  ( -24.89775120788979734, 1442.835553621690224, 210.5176540011790109 ) ) ;
#71632 = CARTESIAN_POINT ( 'NONE',  ( -14.08302796437247828, 1379.638023313924123, 211.6372550111867383 ) ) ;
#71633 = DIRECTION ( 'NONE',  ( 0.3790982213344173957, 0.2704758103281632020, 0.8849448426926984634 ) ) ;
#71634 = DIRECTION ( 'NONE',  ( 0.9510565162951561957, 0.000000000000000000, 0.3090169943749392911 ) ) ;
#71635 = CARTESIAN_POINT ( 'NONE',  ( -1.124289693584999972, 1517.184063036290127, 215.6857614941170027 ) ) ;
#71636 = CARTESIAN_POINT ( 'NONE',  ( -6.500000019064997581, 1516.051704408390151, 209.1218459511669892 ) ) ;
#71637 = ORIENTED_EDGE ( 'NONE', *, *, #99379, .T. ) ;
#71638 = CARTESIAN_POINT ( 'NONE',  ( -16.98677577339999800, 1417.365056119239853, 206.8931061268690144 ) ) ;
#71639 = CARTESIAN_POINT ( 'NONE',  ( 43.51386715234850300, 1440.913060384299797, 268.2728856686210293 ) ) ;
#71640 = CARTESIAN_POINT ( 'NONE',  ( -3.609207719799999659, 1448.636783799939849, 185.0007839605979996 ) ) ;
#71641 = B_SPLINE_CURVE_WITH_KNOTS ( 'NONE', 5,
 ( #110156, #102836, #26130, #17158, #103387, #77124 ),
 .UNSPECIFIED., .F., .F.,
 ( 6, 6 ),
 ( -2.000000000000000000, 0.000000000000000000 ),
 .UNSPECIFIED. ) ;
#71642 = PLANE ( 'NONE',  #51986 ) ;
#71643 = CARTESIAN_POINT ( 'NONE',  ( -38.57173337800420398, 1448.259622455230101, 136.4573440376570090 ) ) ;
#71644 = FACE_OUTER_BOUND ( 'NONE', #94972, .T. ) ;
#71645 = CARTESIAN_POINT ( 'NONE',  ( 2.053820611095168669, 1417.320383901196010, 233.1665847537391301 ) ) ;
#71646 = VECTOR ( 'NONE', #105119, 1000.000000000000000 ) ;
#71647 = CARTESIAN_POINT ( 'NONE',  ( -2.387209960284789823, 1464.875116557210049, 184.0699123369479935 ) ) ;
#71648 = CARTESIAN_POINT ( 'NONE',  ( 10.99133036650000150, 1433.251705345969867, 151.7641221038979893 ) ) ;
#71649 = DIRECTION ( 'NONE',  ( -1.000000000000000000, 0.000000000000000000, 0.000000000000000000 ) ) ;
#71650 = B_SPLINE_SURFACE_WITH_KNOTS ( 'NONE', 4, 5, ( 
 ( #61969, #946, #44038, #68160, #53002, #78176, #17128, #95534, #96083, #35071, #69815, #42935, #103359, #102267, #26661, #18807, #42367, #59739, #68699, #94986, #51318 ),
 ( #25547, #103932, #8752, #27231, #87135, #10425, #34520, #60862, #102804, #51890, #26099, #18254, #60289, #94408, #50774, #86026, #61411, #77634, #52450, #78739, #2054 ),
 ( #70370, #76522, #84908, #110672, #4243, #105046, #97185, #64723, #12078, #45159, #36735, #89886, #63086, #2610, #19358, #4774, #30532, #29974, #88247, #81470, #106145 ),
 ( #53559, #3713, #12637, #11540, #80399, #70930, #37843, #98284, #107240, #96650, #38377, #72553, #55771, #55212, #89341, #87705, #63623, #71486, #19918, #73101, #97739 ),
 ( #79299, #28891, #28335, #64166, #38920, #3163, #54119, #62527, #29424, #21561, #72030, #10985, #106683, #13156, #105607, #45715, #21010, #79852, #37295, #20459, #46814 ) ),
 .UNSPECIFIED., .F., .F., .F.,
 ( 5, 5 ),
 ( 6, 3, 3, 3, 3, 3, 6 ),
 ( 1.603979892999999990, 11.76009528039999985 ),
 ( 27.96617286999999763, 34.32222934679999327, 36.67765262920000424, 37.85536427039999552, 39.03307591160000101, 39.85568086760000028, 40.67828582359999956 ),
 .UNSPECIFIED. ) ;
#71651 = CARTESIAN_POINT ( 'NONE',  ( -9.704836608734391135, 1461.007466806910088, 210.6916309006689971 ) ) ;
#71652 = CARTESIAN_POINT ( 'NONE',  ( -25.03616385470000338, 1508.005457897430006, 220.0251884486980032 ) ) ;
#71653 = PLANE ( 'NONE',  #1026 ) ;
#71654 = ORIENTED_EDGE ( 'NONE', *, *, #26981, .F. ) ;
#71655 = AXIS2_PLACEMENT_3D ( 'NONE', #96865, #3371, #44259 ) ;
#71656 = CARTESIAN_POINT ( 'NONE',  ( 22.90620825975110009, 1507.562497965009925, 210.1669428755749891 ) ) ;
#71657 =( GEOMETRIC_REPRESENTATION_CONTEXT ( 3 ) GLOBAL_UNCERTAINTY_ASSIGNED_CONTEXT ( ( #35647 ) ) GLOBAL_UNIT_ASSIGNED_CONTEXT ( ( #229, #36560, #37111 ) ) REPRESENTATION_CONTEXT ( 'NONE', 'WORKASPACE' ) );
#71658 = CARTESIAN_POINT ( 'NONE',  ( 10.95515571501579899, 1480.001721184990174, 209.1067782184190094 ) ) ;
#71659 = CARTESIAN_POINT ( 'NONE',  ( -19.37630605257373873, 1485.608798315509375, 189.8785843432788738 ) ) ;
#71660 = CARTESIAN_POINT ( 'NONE',  ( -1.637338503800000122, 1444.255706267190135, 199.2007328904890073 ) ) ;
#71661 = CARTESIAN_POINT ( 'NONE',  ( 0.5697989934050000649, 1450.893162568020216, 198.0847581318980133 ) ) ;
#71662 = AXIS2_PLACEMENT_3D ( 'NONE', #71022, #27881, #28432 ) ;
#71663 = CARTESIAN_POINT ( 'NONE',  ( -15.95079730031611831, 1420.249988525623849, 209.7644246339181677 ) ) ;
#71664 = DIRECTION ( 'NONE',  ( 0.3527344445857066857, -0.9357193065623196082, -0.002791223628648406563 ) ) ;
#71665 = CARTESIAN_POINT ( 'NONE',  ( -21.05048463384780177, 1383.852467042130229, 221.2200317013300150 ) ) ;
#71666 =( BOUNDED_CURVE ( )  B_SPLINE_CURVE ( 3, ( #28600, #60577, #17971, #3423 ),
 .UNSPECIFIED., .F., .F. ) 
 B_SPLINE_CURVE_WITH_KNOTS ( ( 4, 4 ),
 ( 0.8955272655465470466, 1.005666413988429930 ),
 .UNSPECIFIED. ) 
 CURVE ( )  GEOMETRIC_REPRESENTATION_ITEM ( )  RATIONAL_B_SPLINE_CURVE ( ( 1.000000000000000000, 0.9989893694451776884, 0.9989893694451776884, 1.000000000000000000 ) ) 
 REPRESENTATION_ITEM ( '' )  );
#71667 = DIRECTION ( 'NONE',  ( 0.000000000000000000, 1.000000000000000000, 0.000000000000000000 ) ) ;
#71668 = CARTESIAN_POINT ( 'NONE',  ( 2.499944111023190363, 1419.634096732200078, 130.9499281974879921 ) ) ;
#71669 = DIRECTION ( 'NONE',  ( -0.6736849260863839728, 0.000000000000000000, 0.7390186874254150995 ) ) ;
#71670 = CARTESIAN_POINT ( 'NONE',  ( 1.649680371479999907, 1465.639337990229933, 235.0739432404980107 ) ) ;
#71672 = VERTEX_POINT ( 'NONE', #31585 ) ;
#71671 = CARTESIAN_POINT ( 'NONE',  ( 9.181100887863649973, 1450.964097471789955, 210.1935140534000084 ) ) ;
#71673 = CARTESIAN_POINT ( 'NONE',  ( -1.192591789150000192, 1451.233485826829792, 183.2247612650980102 ) ) ;
#71674 = CARTESIAN_POINT ( 'NONE',  ( -6.004020725660000224, 1380.880730018859822, 216.3710173946490158 ) ) ;
#71675 = ADVANCED_FACE ( 'NONE', ( #49518 ), #110508, .F. ) ;
#71676 = CARTESIAN_POINT ( 'NONE',  ( -5.519891203089999365, 1440.499824919269940, 154.7645185998979969 ) ) ;
#71678 = ORIENTED_EDGE ( 'NONE', *, *, #31765, .F. ) ;
#71677 = DIRECTION ( 'NONE',  ( -0.8090169943749551118, -0.000000000000000000, -0.5877852522924625900 ) ) ;
#71679 = CARTESIAN_POINT ( 'NONE',  ( 18.46111558074320058, 1471.785967886609797, 195.2229703376199836 ) ) ;
#71680 = ORIENTED_EDGE ( 'NONE', *, *, #32333, .F. ) ;
#71681 = CARTESIAN_POINT ( 'NONE',  ( -8.680524314125149132, 1387.563194770179962, 218.1353776963400151 ) ) ;
#71682 = CARTESIAN_POINT ( 'NONE',  ( -0.9541980877279990780, 1483.985701638789806, 201.2944014693789825 ) ) ;
#71683 = CARTESIAN_POINT ( 'NONE',  ( 3.584503077415259753, 1486.500511906220027, 219.3043361390229791 ) ) ;
#71684 = B_SPLINE_CURVE_WITH_KNOTS ( 'NONE', 3,
 ( #3223, #29483, #88304, #3772, #70988, #64222, #46872, #97243, #81000, #20518, #54725, #53625, #46329 ),
 .UNSPECIFIED., .F., .F.,
 ( 4, 3, 3, 3, 4 ),
 ( -167.7240082859999859, -142.7479071452019923, -102.0777101884260105, -65.48876935620850759, -30.58270280209998759 ),
 .UNSPECIFIED. ) ;
#71685 = CARTESIAN_POINT ( 'NONE',  ( 22.70290200285219484, 1409.705865383426271, 208.6626894467611919 ) ) ;
#71686 = CARTESIAN_POINT ( 'NONE',  ( -2.492462743589999974, 1432.101689878689967, 217.3048426501089807 ) ) ;
#71687 = AXIS2_PLACEMENT_3D ( 'NONE', #76734, #25758, #25202 ) ;
#71688 = CARTESIAN_POINT ( 'NONE',  ( 2.620401159549909487, 1523.382868172863937, 242.1631858340802523 ) ) ;
#71689 = CARTESIAN_POINT ( 'NONE',  ( 14.24591603755999891, 1409.410538736599847, 213.5977365385609801 ) ) ;
#71690 = CARTESIAN_POINT ( 'NONE',  ( 5.650554639980001070, 1452.063337922390019, 211.4905752170589892 ) ) ;
#71691 = CARTESIAN_POINT ( 'NONE',  ( -92.68011806984669931, 1385.200888536659932, 294.0055341178320418 ) ) ;
#71692 = CARTESIAN_POINT ( 'NONE',  ( -19.35957638029999828, 1470.693184109529966, 190.9127711249979882 ) ) ;
#71693 = CARTESIAN_POINT ( 'NONE',  ( -68.43569653030000666, 1379.748342192099926, 279.4446506693590209 ) ) ;
#71694 = CARTESIAN_POINT ( 'NONE',  ( 11.43665885888289857, 1491.402434470230219, 208.3916377791149728 ) ) ;
#71695 = EDGE_CURVE ( 'NONE', #70084, #108510, #50117, .T. ) ;
#71696 = ORIENTED_EDGE ( 'NONE', *, *, #95396, .T. ) ;
#71697 = ORIENTED_EDGE ( 'NONE', *, *, #102915, .F. ) ;
#71698 = CARTESIAN_POINT ( 'NONE',  ( -11.44693299037050060, 1415.124054205840139, 195.4737557617620212 ) ) ;
#71699 = DIRECTION ( 'NONE',  ( 1.000000000000000000, 0.000000000000000000, 0.000000000000000000 ) ) ;
#71700 = CIRCLE ( 'NONE', #26893, 7.932410439649999923 ) ;
#71701 = EDGE_CURVE ( 'NONE', #105896, #21322, #65873, .T. ) ;
#71702 = CARTESIAN_POINT ( 'NONE',  ( 29.83339565102073720, 1462.371191219802768, 269.4690383729464429 ) ) ;
#71703 = FACE_OUTER_BOUND ( 'NONE', #54264, .T. ) ;
#71704 = CARTESIAN_POINT ( 'NONE',  ( 3.586107180329999977, 1396.221082240130045, 220.6064224583979865 ) ) ;
#71705 = CARTESIAN_POINT ( 'NONE',  ( 32.21733187661251918, 1523.844789899204898, 201.4553037014809149 ) ) ;
#71706 = CARTESIAN_POINT ( 'NONE',  ( -0.8850937001509999735, 1467.455705555530130, 182.7531797504979920 ) ) ;
#71707 = CARTESIAN_POINT ( 'NONE',  ( -9.934709065799999905, 1365.494406819939968, 207.6218459616989946 ) ) ;
#71708 = LINE ( 'NONE', #88463, #107295 ) ;
#71709 = CARTESIAN_POINT ( 'NONE',  ( -5.788097265284999793, 1517.099836525840146, 206.6397780718770036 ) ) ;
#71710 = CARTESIAN_POINT ( 'NONE',  ( -13.04373921950000081, 1435.024846296409805, 150.0238230700980182 ) ) ;
#71711 = CARTESIAN_POINT ( 'NONE',  ( 30.90487439922549484, 1525.907212628473644, 201.8101144455178257 ) ) ;
#71712 = CARTESIAN_POINT ( 'NONE',  ( 0.7130140550910000208, 1416.844618635429924, 190.3244981512979734 ) ) ;
#71713 = CARTESIAN_POINT ( 'NONE',  ( 0.3681096306540009855, 1496.876227892089901, 197.1249798701990130 ) ) ;
#71714 = CARTESIAN_POINT ( 'NONE',  ( 4.500000000000000000, 1448.210448412289907, 182.3842140122979743 ) ) ;
#71715 = CARTESIAN_POINT ( 'NONE',  ( -107.7596963679999931, 1382.859817520469733, 297.6961126062590210 ) ) ;
#71716 = EDGE_LOOP ( 'NONE', ( #88870, #80562, #6051, #1473 ) ) ;
#71717 = CARTESIAN_POINT ( 'NONE',  ( -113.4000000000000057, 1384.913060387289988, 304.2218459572590064 ) ) ;
#71718 = CARTESIAN_POINT ( 'NONE',  ( -26.28495520110000072, 1469.245429239829946, 207.2831767420279903 ) ) ;
#71720 = CARTESIAN_POINT ( 'NONE',  ( -0.5987183604784179769, 1507.212886163649955, 231.7504617458309895 ) ) ;
#71719 = CARTESIAN_POINT ( 'NONE',  ( -10.92148113222090089, 1426.083150769400163, 93.54269902050201324 ) ) ;
#71721 = EDGE_CURVE ( 'NONE', #98568, #28929, #10783, .T. ) ;
#71722 = CARTESIAN_POINT ( 'NONE',  ( 1.669890710131026967, 1508.956865050931128, 179.7751757192045261 ) ) ;
#71723 = CARTESIAN_POINT ( 'NONE',  ( -10.53938673480000077, 1414.594228658529801, 248.5638781430979805 ) ) ;
#71724 = CARTESIAN_POINT ( 'NONE',  ( 20.51326474582850068, 1509.672687637749959, 230.6559570000279962 ) ) ;
#71725 = CARTESIAN_POINT ( 'NONE',  ( -109.9855944279999989, 1384.926148861439970, 311.4562326602589906 ) ) ;
#71726 = DIRECTION ( 'NONE',  ( 0.5674277338727796716, 0.8234232003241116482, 0.000000000000000000 ) ) ;
#71727 = ORIENTED_EDGE ( 'NONE', *, *, #85099, .T. ) ;
#71728 = CARTESIAN_POINT ( 'NONE',  ( 3.920879176457659820, 1439.701872010520219, 184.6839060028229937 ) ) ;
#71729 = CARTESIAN_POINT ( 'NONE',  ( 14.63129139947360891, 1514.438069594173157, 225.4795426202890383 ) ) ;
#71730 = CARTESIAN_POINT ( 'NONE',  ( 11.57433915100000021, 1509.317245216830088, 236.3676525501980166 ) ) ;
#71731 = VERTEX_POINT ( 'NONE', #58463 ) ;
#71732 = EDGE_LOOP ( 'NONE', ( #30360, #109704, #60253, #16530, #41311, #11557, #16288, #78712 ) ) ;
#71733 = CARTESIAN_POINT ( 'NONE',  ( 10.06014724255809867, 1452.783669392659931, 210.4777447332699865 ) ) ;
#71734 = CARTESIAN_POINT ( 'NONE',  ( 7.495582065179999809, 1424.824266038629958, 194.2083062206990007 ) ) ;
#71735 = VERTEX_POINT ( 'NONE', #92591 ) ;
#71736 = FACE_OUTER_BOUND ( 'NONE', #86950, .T. ) ;
#71737 = CARTESIAN_POINT ( 'NONE',  ( -4.447876660801433069, 1419.909382011105208, 194.3620334553881150 ) ) ;
#71738 = TOROIDAL_SURFACE ( 'NONE', #107406, 1.000000000000000000, 1.000000000000000000 ) ;
#71739 = CARTESIAN_POINT ( 'NONE',  ( -11.86678758501360065, 1432.386623006779928, 149.9823363065619901 ) ) ;
#71740 = CARTESIAN_POINT ( 'NONE',  ( -1.436137458879999995, 1489.063931860629964, 236.3499381435979956 ) ) ;
#71741 = CARTESIAN_POINT ( 'NONE',  ( 16.83198307404049743, 1526.000688113711703, 235.9162354438186071 ) ) ;
#71742 = ORIENTED_EDGE ( 'NONE', *, *, #46715, .T. ) ;
#71743 = CARTESIAN_POINT ( 'NONE',  ( 10.81506866279999990, 1424.921186100929845, 144.1620444789979842 ) ) ;
#71744 = CARTESIAN_POINT ( 'NONE',  ( -12.03795434196880088, 1414.913057855109855, 220.4160453579169996 ) ) ;
#71745 = CARTESIAN_POINT ( 'NONE',  ( 14.78974000539999878, 1496.665265930929991, 226.0583177165980260 ) ) ;
#71746 = ORIENTED_EDGE ( 'NONE', *, *, #8584, .T. ) ;
#71747 = CARTESIAN_POINT ( 'NONE',  ( -1.712644754285000070, 1516.636036526019780, 204.1262224792070015 ) ) ;
#71748 = ORIENTED_EDGE ( 'NONE', *, *, #96917, .T. ) ;
#71749 = CARTESIAN_POINT ( 'NONE',  ( 11.86398041411250048, 1432.187849662659801, 149.9803448969269937 ) ) ;
#71750 = CARTESIAN_POINT ( 'NONE',  ( 5.551188674472009588, 1510.480349264700180, 216.6723492941099778 ) ) ;
#71751 = ORIENTED_EDGE ( 'NONE', *, *, #62384, .T. ) ;
#71752 = EDGE_LOOP ( 'NONE', ( #80476, #9838, #60407 ) ) ;
#71753 = CARTESIAN_POINT ( 'NONE',  ( 0.5770119038902407071, 1525.581535527370761, 174.8524476110296177 ) ) ;
#71754 = FACE_OUTER_BOUND ( 'NONE', #25097, .T. ) ;
#71755 = CARTESIAN_POINT ( 'NONE',  ( 2.045518813257909851, 1498.492502908489996, 197.9893470804480273 ) ) ;
#71756 = VECTOR ( 'NONE', #49584, 1000.000000000000000 ) ;
#71757 = CARTESIAN_POINT ( 'NONE',  ( -7.630521968176440240, 1469.354043036800022, 216.8955778692430272 ) ) ;
#71758 = LINE ( 'NONE', #54925, #15364 ) ;
#71759 = CARTESIAN_POINT ( 'NONE',  ( 0.4843704149012760252, 1408.561147827879950, 270.4290818619680294 ) ) ;
#71760 = CARTESIAN_POINT ( 'NONE',  ( 1.548774059501979883, 1474.902113389930037, 220.4354346946340115 ) ) ;
#71761 = FACE_OUTER_BOUND ( 'NONE', #105739, .T. ) ;
#71762 = CARTESIAN_POINT ( 'NONE',  ( -20.71991831406684170, 1509.684987494643565, 230.4894327893642867 ) ) ;
#71764 = CARTESIAN_POINT ( 'NONE',  ( 14.20204630610000152, 1416.837080254230159, 196.5054416555979913 ) ) ;
#71763 = CARTESIAN_POINT ( 'NONE',  ( -14.15252861969999820, 1503.726965476990017, 208.7499539689279970 ) ) ;
#71765 = CARTESIAN_POINT ( 'NONE',  ( 11.55990587695049854, 1422.181602173609917, 207.1874422316890048 ) ) ;
#71766 = VECTOR ( 'NONE', #91837, 999.9999999999997726 ) ;
#71767 = CARTESIAN_POINT ( 'NONE',  ( 17.96527429238589946, 1422.523928809379868, 225.1465795047810161 ) ) ;
#71768 = CARTESIAN_POINT ( 'NONE',  ( -7.496083208854999569, 1513.333000339830051, 202.7317914838369859 ) ) ;
#71769 = ORIENTED_EDGE ( 'NONE', *, *, #46840, .T. ) ;
#71770 = CARTESIAN_POINT ( 'NONE',  ( 16.86383896219999912, 1416.370072266829993, 262.6648722463980334 ) ) ;
#71771 = LINE ( 'NONE', #38115, #37269 ) ;
#71772 = CARTESIAN_POINT ( 'NONE',  ( -76.63588753610599724, 1385.003182676139886, 301.4206644342669961 ) ) ;
#71773 = DIRECTION ( 'NONE',  ( 0.4090087482554383147, 0.000000000000000000, 0.9125304618753937724 ) ) ;
#71774 = CARTESIAN_POINT ( 'NONE',  ( 3.775314268589999855, 1507.374707634990045, 220.2027404231990033 ) ) ;
#71775 = DIRECTION ( 'NONE',  ( 0.3971731930706579039, 0.04395516701092885142, 0.9166904592058866541 ) ) ;
#71777 = ORIENTED_EDGE ( 'NONE', *, *, #81687, .T. ) ;
#71776 = CARTESIAN_POINT ( 'NONE',  ( -16.16618494246800353, 1419.872609311620181, 210.0412365793670233 ) ) ;
#71778 = CARTESIAN_POINT ( 'NONE',  ( -15.88421513919616146, 1415.958925770876931, 209.7365058685432189 ) ) ;
#71779 = VECTOR ( 'NONE', #76425, 1000.000000000000114 ) ;
#71780 = CARTESIAN_POINT ( 'NONE',  ( 20.02377564230000218, 1475.402829072889972, 206.2263482165890025 ) ) ;
#71781 = DIRECTION ( 'NONE',  ( -0.6736849260863841948, 0.000000000000000000, 0.7390186874254148774 ) ) ;
#71782 = CARTESIAN_POINT ( 'NONE',  ( -0.6427045307039329636, 1430.099853101789904, 199.7385159216829891 ) ) ;
#71783 = CARTESIAN_POINT ( 'NONE',  ( 15.28532361773500092, 1514.287526756679881, 224.2181362973670105 ) ) ;
#71784 = CARTESIAN_POINT ( 'NONE',  ( -3.829620113550000315, 1515.051704408389924, 209.0973262533439936 ) ) ;
#71785 = CARTESIAN_POINT ( 'NONE',  ( 19.19360523492100157, 1509.583315851710040, 231.6001312093189881 ) ) ;
#71786 = CARTESIAN_POINT ( 'NONE',  ( 7.744112962519119847, 1460.365312253459933, 203.2200444182140018 ) ) ;
#71787 = CARTESIAN_POINT ( 'NONE',  ( -15.28420222199999934, 1497.713060387329961, 224.4060481839979957 ) ) ;
#71788 = CARTESIAN_POINT ( 'NONE',  ( 4.426925289939999786, 1417.415159599829849, 231.7246244170979992 ) ) ;
#71789 = FACE_OUTER_BOUND ( 'NONE', #18030, .T. ) ;
#71790 = CARTESIAN_POINT ( 'NONE',  ( 1.356522472024429993, 1410.335674015750101, 232.6399073486850000 ) ) ;
#71791 = CARTESIAN_POINT ( 'NONE',  ( 4.995623452895000760, 1516.636036526019780, 207.4092012159470073 ) ) ;
#71792 = CARTESIAN_POINT ( 'NONE',  ( 45.06536953950000424, 1434.999718682669936, 268.9906915396979912 ) ) ;
#71793 = CARTESIAN_POINT ( 'NONE',  ( -18.33065379749999835, 1410.049607812529985, 223.7945510231980109 ) ) ;
#71794 = CARTESIAN_POINT ( 'NONE',  ( 17.98866383510000233, 1435.941952030790162, 147.2730939229980152 ) ) ;
#71795 = VECTOR ( 'NONE', #22792, 1000.000000000000000 ) ;
#71796 = CARTESIAN_POINT ( 'NONE',  ( 21.20954604569999802, 1488.584398273929992, 192.3846377322979890 ) ) ;
#71797 = CARTESIAN_POINT ( 'NONE',  ( 22.72408229139999847, 1432.100443994239868, 218.1715127473280234 ) ) ;
#71798 = CARTESIAN_POINT ( 'NONE',  ( -3.829620113550000315, 1515.551704408389924, 211.4519800877889963 ) ) ;
#71799 = CARTESIAN_POINT ( 'NONE',  ( -0.7749238296759999312, 1475.832189872029858, 266.9609160975979876 ) ) ;
#71800 = CARTESIAN_POINT ( 'NONE',  ( 12.61325660393820058, 1426.953648319100012, 205.8283967020159935 ) ) ;
#71801 = CARTESIAN_POINT ( 'NONE',  ( -36.93911259867740426, 1436.285475061979923, 135.0345442704649770 ) ) ;
#71802 = CARTESIAN_POINT ( 'NONE',  ( 0.2072761112290929797, 1458.881660194060260, 183.0010636273980253 ) ) ;
#71803 = CARTESIAN_POINT ( 'NONE',  ( -12.34781077223220080, 1407.409374063429823, 203.9011771819639876 ) ) ;
#71804 = CARTESIAN_POINT ( 'NONE',  ( 0.2417153426969999852, 1418.558758520830224, 184.6769579382979884 ) ) ;
#71805 = CARTESIAN_POINT ( 'NONE',  ( -12.45591551270000075, 1442.246608597349905, 187.4685661162980068 ) ) ;
#71806 = CARTESIAN_POINT ( 'NONE',  ( -7.641220756667040703, 1383.796531935709936, 218.9774033050359776 ) ) ;
#71807 = CARTESIAN_POINT ( 'NONE',  ( 13.50147622419999927, 1434.968985796360130, 146.7592199324979845 ) ) ;
#71808 = FACE_OUTER_BOUND ( 'NONE', #22821, .T. ) ;
#71809 = CARTESIAN_POINT ( 'NONE',  ( -1.018585033021226938, 1419.107236328670524, 184.9305476069722545 ) ) ;
#71810 = ORIENTED_EDGE ( 'NONE', *, *, #20778, .T. ) ;
#71811 = CARTESIAN_POINT ( 'NONE',  ( 6.150246115290385340, 1510.808998940108040, 216.5916852012511811 ) ) ;
#71812 = CARTESIAN_POINT ( 'NONE',  ( -5.146882827519980275, 1409.092793496169861, 223.1895541711200224 ) ) ;
#71813 = CARTESIAN_POINT ( 'NONE',  ( -17.22592475670000312, 1443.913060387330006, 162.9227486557980171 ) ) ;
#71814 = CARTESIAN_POINT ( 'NONE',  ( -5.077887651979027694, 1463.916885366726319, 200.2638546281883123 ) ) ;
#71815 = CARTESIAN_POINT ( 'NONE',  ( 0.000000000000000000, 1526.382868172863937, 209.1218459616979999 ) ) ;
#71816 = CARTESIAN_POINT ( 'NONE',  ( -44.93232737969999135, 1451.209032879530014, 267.0122724004980341 ) ) ;
#71817 = CARTESIAN_POINT ( 'NONE',  ( -30.57819355944234019, 1525.253996226949539, 196.6735304476125066 ) ) ;
#71818 = CARTESIAN_POINT ( 'NONE',  ( -19.82130876261663133, 1501.765438912635773, 189.1477900679612958 ) ) ;
#71819 = CARTESIAN_POINT ( 'NONE',  ( -26.93111412509999880, 1509.630721880230112, 216.4445429101480158 ) ) ;
#71820 = CARTESIAN_POINT ( 'NONE',  ( 17.17241001986484505, 1523.382868172864164, 179.6185504016043524 ) ) ;
#71821 = CARTESIAN_POINT ( 'NONE',  ( -39.94094280074159542, 1384.989748394649951, 212.8264697954110147 ) ) ;
#71822 = COLOUR_RGB ( '', 0.72549020, 0.75294118, 0.79215686) ;
#71823 = CARTESIAN_POINT ( 'NONE',  ( 17.33325820480230206, 1423.906894160079901, 228.7549733049369820 ) ) ;
#71824 = CARTESIAN_POINT ( 'NONE',  ( 21.92402930929999982, 1509.678664361430037, 227.7489718475979998 ) ) ;
#71825 = CARTESIAN_POINT ( 'NONE',  ( 15.72497962809999983, 1506.810797447130199, 224.5140330397979938 ) ) ;
#71826 = CARTESIAN_POINT ( 'NONE',  ( -2.620401159549909487, 1523.382868172863937, 176.0805060893157474 ) ) ;
#71827 = EDGE_CURVE ( 'NONE', #16710, #33454, #15862, .T. ) ;
#71829 = ORIENTED_EDGE ( 'NONE', *, *, #4980, .T. ) ;
#71828 = CARTESIAN_POINT ( 'NONE',  ( 19.53786426059039982, 1511.187213306747708, 236.7197124308265188 ) ) ;
#71830 = CARTESIAN_POINT ( 'NONE',  ( -109.4849134029999931, 1384.882923838719989, 311.2840634072589978 ) ) ;
#71831 = B_SPLINE_CURVE_WITH_KNOTS ( 'NONE', 3,
 ( #65228, #74183, #98805, #81994, #22066, #82572, #5301, #58476, #49531, #92064, #4744, #22614, #73069, #99339, #30498, #31598, #100998, #6410, #74730, #108864, #108314, #38888, #14241, #39459, #65777, #41108, #91517, #107210, #6951, #73632, #90392, #56263, #83656, #56817, #48430, #5864, #23743, #40005, #57931, #99894, #66889, #92604, #75285, #23192, #57391, #109431, #24294, #14797, #48983, #32157, #15877, #50080 ),
 .UNSPECIFIED., .F., .F.,
 ( 4, 2, 2, 1, 1, 2, 2, 2, 2, 1, 1, 2, 2, 2, 1, 1, 1, 2, 2, 2, 1, 1, 2, 2, 2, 1, 2, 2, 2, 2, 4 ),
 ( 0.000000000000000000, 0.06249999999934317818, 0.09374999999905359038, 0.1093749999989083177, 0.1171874999988343352, 0.1210937499987959215, 0.1249999999987574939, 0.1874999999981092347, 0.2187499999977872700, 0.2343749999976272314, 0.2421874999975472120, 0.2460937499974766018, 0.2499999999974060194, 0.3124999999966770470, 0.3437499999963145592, 0.3593749999961312058, 0.3671874999960428876, 0.3710937499960308972, 0.3749999999960189623, 0.4374999999965382136, 0.4687499999967978392, 0.4843749999968984254, 0.4921874999969200748, 0.4999999999969416686, 0.5624999999973839815, 0.5937499999976038056, 0.6093749999977137177, 0.6249999999978236298, 0.6874999999981920018, 0.7499999999985602628, 1.000000000000000000 ),
 .UNSPECIFIED. ) ;
#71832 = DIRECTION ( 'NONE',  ( 0.4090087482554447540, 1.419034154957372271E-15, 0.9125304618753908859 ) ) ;
#71833 = CARTESIAN_POINT ( 'NONE',  ( 25.70439233229999942, 1469.175250655529908, 207.3826630381880136 ) ) ;
#71834 = CARTESIAN_POINT ( 'NONE',  ( -12.45642902069999991, 1416.822690122629865, 194.7673859876979918 ) ) ;
#71835 = LINE ( 'NONE', #71278, #47933 ) ;
#71836 = EDGE_CURVE ( 'NONE', #107891, #15749, #34899, .T. ) ;
#71837 = CARTESIAN_POINT ( 'NONE',  ( 23.99977061020000235, 1410.673205389529812, 209.9141634752309926 ) ) ;
#71838 = CARTESIAN_POINT ( 'NONE',  ( -106.4502107925090115, 1391.913060387289988, 304.8668619185630178 ) ) ;
#71839 = CARTESIAN_POINT ( 'NONE',  ( 19.05639497150000139, 1459.894456182490103, 220.3270700572990108 ) ) ;
#71840 = CARTESIAN_POINT ( 'NONE',  ( -5.614653854145000622, 1512.903985260039917, 201.5078774661370176 ) ) ;
#71842 = CARTESIAN_POINT ( 'NONE',  ( -11.61990403848027675, 1426.774261403575565, 135.7993244020507575 ) ) ;
#71841 = CARTESIAN_POINT ( 'NONE',  ( -10.97596787830000054, 1432.730999280179958, 151.7698537100980047 ) ) ;
#71843 = CARTESIAN_POINT ( 'NONE',  ( 0.3042685152679999727, 1411.657205677930051, 233.3132544252979983 ) ) ;
#71844 = CARTESIAN_POINT ( 'NONE',  ( -119.5163997959657820, 1378.528619065190696, 293.9108410952588315 ) ) ;
#71845 = B_SPLINE_CURVE_WITH_KNOTS ( 'NONE', 3,
 ( #110459, #60635, #103713, #9639, #94760, #77415, #42711, #93633, #85804, #43813 ),
 .UNSPECIFIED., .F., .F.,
 ( 4, 2, 2, 2, 4 ),
 ( 0.000000000000000000, 0.0007189769279726051935, 0.001437953855945210387, 0.002156930783917815689, 0.002875907711890420774 ),
 .UNSPECIFIED. ) ;
#71846 = CARTESIAN_POINT ( 'NONE',  ( 2173.981453289206911, -8382.262153571264207, -1556.947849745907888 ) ) ;
#71847 = FACE_OUTER_BOUND ( 'NONE', #78450, .T. ) ;
#71848 = CARTESIAN_POINT ( 'NONE',  ( -0.8190364809989280070, 1418.969067203539907, 184.8287228181580133 ) ) ;
#71849 = AXIS2_PLACEMENT_3D ( 'NONE', #32927, #103290, #35554 ) ;
#71850 = CARTESIAN_POINT ( 'NONE',  ( -5.009478105444999940, 1516.886345593249871, 204.5093386581970094 ) ) ;
#71851 = CARTESIAN_POINT ( 'NONE',  ( 13.40431027868319980, 1508.087536715469696, 233.1606899894430001 ) ) ;
#71852 = CARTESIAN_POINT ( 'NONE',  ( -18.39201604218439812, 1486.027299296950105, 188.9270178829710005 ) ) ;
#71853 = CARTESIAN_POINT ( 'NONE',  ( 8787.386475773348138, -2339.246371527899555, -2767.671033105199513 ) ) ;
#71854 = CARTESIAN_POINT ( 'NONE',  ( -11.17519453696281140, 1422.142527340527977, 210.6369239073095798 ) ) ;
#71856 = VERTEX_POINT ( 'NONE', #87529 ) ;
#71855 = CARTESIAN_POINT ( 'NONE',  ( -68.33529581026429867, 1379.747047273969883, 279.8915150897229864 ) ) ;
#71857 = ORIENTED_EDGE ( 'NONE', *, *, #61177, .T. ) ;
#71858 = CARTESIAN_POINT ( 'NONE',  ( 28.60142811679999753, 1509.872226484729936, 213.7037800932280049 ) ) ;
#71859 = ORIENTED_EDGE ( 'NONE', *, *, #91022, .F. ) ;
#71860 = DIRECTION ( 'NONE',  ( 0.9746209764380640017, 5.558287066451319365E-07, 0.2238614577961240137 ) ) ;
#71861 = LINE ( 'NONE', #89703, #97621 ) ;
#71863 = CARTESIAN_POINT ( 'NONE',  ( 1.129089833999999959, 1507.125633147629969, 181.0548235415979832 ) ) ;
#71862 = CARTESIAN_POINT ( 'NONE',  ( -1.077847364669999991E-15, 1428.043997280830126, 101.8807690336980016 ) ) ;
#71864 = CARTESIAN_POINT ( 'NONE',  ( -5.371346839175000554, 1516.551704408390151, 218.7599618298069970 ) ) ;
#71865 = CIRCLE ( 'NONE', #36017, 3.000000000000002665 ) ;
#71866 = CARTESIAN_POINT ( 'NONE',  ( -24.24285629885429927, 1452.061333677959965, 136.5609822530450117 ) ) ;
#71867 = CARTESIAN_POINT ( 'NONE',  ( -1.636741585329999804, 1469.777368439289830, 219.0527109404189900 ) ) ;
#71868 = CARTESIAN_POINT ( 'NONE',  ( 4.247845347069999278, 1409.061398416330121, 230.4234178570980021 ) ) ;
#71869 = CARTESIAN_POINT ( 'NONE',  ( 12.53490346717240023, 1501.124165648190001, 211.2564677464939962 ) ) ;
#71870 =( NAMED_UNIT ( * ) PLANE_ANGLE_UNIT ( ) SI_UNIT ( $, .RADIAN. ) );
#71871 = CARTESIAN_POINT ( 'NONE',  ( 1.715704490974999885, 1516.757508073510053, 212.3732403323669757 ) ) ;
#71872 = CARTESIAN_POINT ( 'NONE',  ( 41.49772933728709745, 1445.334750750500007, 134.0999999984909721 ) ) ;
#71873 = CARTESIAN_POINT ( 'NONE',  ( -7.110895733399999585, 1481.050959687990144, 207.2709231533789875 ) ) ;
#71874 = ORIENTED_EDGE ( 'NONE', *, *, #9882, .F. ) ;
#71875 = CARTESIAN_POINT ( 'NONE',  ( 14.59287365574109963, 1436.244834338669989, 149.8708846901989773 ) ) ;
#71876 = CARTESIAN_POINT ( 'NONE',  ( -1.219629049478790028, 1431.745899841950177, 200.8064624575089852 ) ) ;
#71877 = VERTEX_POINT ( 'NONE', #77469 ) ;
#71878 = EDGE_LOOP ( 'NONE', ( #99186, #9990, #49068, #65931, #56085 ) ) ;
#71879 = VERTEX_POINT ( 'NONE', #69087 ) ;
#71880 = CARTESIAN_POINT ( 'NONE',  ( -6.557434894264999592, 1513.513616978030086, 216.5800176418070180 ) ) ;
#71881 = DIRECTION ( 'NONE',  ( 1.000000000000000000, 0.000000000000000000, 0.000000000000000000 ) ) ;
#71882 = CARTESIAN_POINT ( 'NONE',  ( 8.737474774033083591, 1451.364372104259473, 152.7144497316307650 ) ) ;
#71883 = CARTESIAN_POINT ( 'NONE',  ( -3.116134553580160560, 1509.034509793703819, 204.6344886145632529 ) ) ;
#71884 = CARTESIAN_POINT ( 'NONE',  ( 9.742642355230000106, 1463.575582522990089, 210.1498719498890182 ) ) ;
#71885 = AXIS2_PLACEMENT_3D ( 'NONE', #67901, #27527, #34269 ) ;
#71886 = CARTESIAN_POINT ( 'NONE',  ( -12.62971280459999868, 1379.172876932190093, 208.6065707151580000 ) ) ;
#71887 = CARTESIAN_POINT ( 'NONE',  ( -63.86443237624047953, 1379.736326793258058, 269.9080968292980742 ) ) ;
#71888 = CARTESIAN_POINT ( 'NONE',  ( 0.1600667122320010294, 1463.646925499989948, 199.3014139421989910 ) ) ;
#71889 = CARTESIAN_POINT ( 'NONE',  ( 5.808539518960000869, 1415.087797054229895, 192.8637157185980016 ) ) ;
#71890 = B_SPLINE_CURVE_WITH_KNOTS ( 'NONE', 3,
 ( #14886, #49077, #47418, #91609, #31145, #13777, #81540, #6501, #99999, #40655, #73166, #107310, #74826 ),
 .UNSPECIFIED., .F., .F.,
 ( 4, 3, 3, 3, 4 ),
 ( -167.9629942519999872, -131.9082348649870085, -95.51900912811341016, -62.09002792079060384, -30.61745639480000136 ),
 .UNSPECIFIED. ) ;
#71891 = CARTESIAN_POINT ( 'NONE',  ( -1.137296688934999800, 1516.908147884120126, 207.4199954749970232 ) ) ;
#71892 = ORIENTED_EDGE ( 'NONE', *, *, #2155, .F. ) ;
#71893 = CARTESIAN_POINT ( 'NONE',  ( 31.96508519263229786, 1440.913060387330006, 255.8875838973339683 ) ) ;
#71894 = CARTESIAN_POINT ( 'NONE',  ( 11.54563913674000020, 1478.900881724800001, 206.9376360146720231 ) ) ;
#71895 = ORIENTED_EDGE ( 'NONE', *, *, #15100, .F. ) ;
#71896 = CARTESIAN_POINT ( 'NONE',  ( -7.012530104786800500, 1508.551704607450120, 203.1375064762430043 ) ) ;
#71897 = CARTESIAN_POINT ( 'NONE',  ( -14.54947616759999995, 1409.923023063329993, 190.7312617873979832 ) ) ;
#71898 = CARTESIAN_POINT ( 'NONE',  ( -17.69340222479375058, 1508.456513906287682, 212.3435705202165025 ) ) ;
#71900 = CARTESIAN_POINT ( 'NONE',  ( 14.95092670185879946, 1512.169469372310004, 196.6644221003890038 ) ) ;
#71899 = CARTESIAN_POINT ( 'NONE',  ( 8.249561420100000930, 1502.931132867190172, 210.0140376356389993 ) ) ;
#71901 = CARTESIAN_POINT ( 'NONE',  ( 22.04426538949190117, 1410.014371781770024, 206.2776455835269758 ) ) ;
#71902 = FACE_OUTER_BOUND ( 'NONE', #47120, .T. ) ;
#71903 = CARTESIAN_POINT ( 'NONE',  ( -12.10808283629549820, 1433.926313951669499, 147.5251541910231765 ) ) ;
#71904 = CARTESIAN_POINT ( 'NONE',  ( -12.91306329870000091, 1434.774359993769849, 148.5639779176980255 ) ) ;
#71905 = CARTESIAN_POINT ( 'NONE',  ( -4.297012669169999910, 1508.497024723489858, 220.4589697836989899 ) ) ;
#71907 = CARTESIAN_POINT ( 'NONE',  ( -0.004106634418278950170, 1498.706732373090063, 200.5431806547190092 ) ) ;
#71906 = CARTESIAN_POINT ( 'NONE',  ( 7.696916953700000619, 1464.574746897430032, 233.3918279888980010 ) ) ;
#71908 = CARTESIAN_POINT ( 'NONE',  ( -3.258474617075000079, 1517.083030555940013, 215.6838419306269827 ) ) ;
#71909 = CARTESIAN_POINT ( 'NONE',  ( -32.85805783624297760, 1523.678648413191695, 217.1983043299907763 ) ) ;
#71910 = CARTESIAN_POINT ( 'NONE',  ( 5.718152469055599596, 1511.533951550999973, 217.5449680129780177 ) ) ;
#71911 = CARTESIAN_POINT ( 'NONE',  ( 16.67654997235155534, 1449.441375609227862, 219.1029392211832771 ) ) ;
#71912 = CARTESIAN_POINT ( 'NONE',  ( 0.7576635334400020350, 1516.855632454399938, 211.9899581013969794 ) ) ;
#71913 = EDGE_CURVE ( 'NONE', #86132, #10824, #46521, .T. ) ;
#71914 = CARTESIAN_POINT ( 'NONE',  ( -11.44339780954279995, 1482.754209377100096, 205.8243739520100064 ) ) ;
#71915 = CARTESIAN_POINT ( 'NONE',  ( 30.15498238788762819, 1525.730671215510711, 221.2486442788145382 ) ) ;
#71917 = ORIENTED_EDGE ( 'NONE', *, *, #93872, .T. ) ;
#71916 = CARTESIAN_POINT ( 'NONE',  ( -113.4000000000000057, 1389.425727822280123, 300.1302024219590407 ) ) ;
#71918 = DIRECTION ( 'NONE',  ( 0.9996573249755574819, -0.02617694830786557875, 0.000000000000000000 ) ) ;
#71919 = CARTESIAN_POINT ( 'NONE',  ( 22.59987829099999956, 1454.496478413630030, 232.0087828362979963 ) ) ;
#71920 = EDGE_CURVE ( 'NONE', #70558, #67122, #41144, .T. ) ;
#71921 = FACE_OUTER_BOUND ( 'NONE', #7267, .T. ) ;
#71922 = CARTESIAN_POINT ( 'NONE',  ( -14.86532350809999947, 1415.677402202029953, 206.7896748190889866 ) ) ;
#71923 = EDGE_CURVE ( 'NONE', #52837, #73912, #39056, .T. ) ;
#71924 = CARTESIAN_POINT ( 'NONE',  ( 2.193589587269999974, 1410.361569429029942, 231.8614317343979963 ) ) ;
#71925 = CARTESIAN_POINT ( 'NONE',  ( -15.46337563405010052, 1415.677402202039957, 209.5778891453549875 ) ) ;
#71926 = AXIS2_PLACEMENT_3D ( 'NONE', #45521, #37639, #104846 ) ;
#71928 = CARTESIAN_POINT ( 'NONE',  ( 5.382707040917719787, 1431.444277130069850, 154.5902336194710074 ) ) ;
#71927 = CARTESIAN_POINT ( 'NONE',  ( -19.29250527829999839, 1444.805202439009918, 225.3992152728980329 ) ) ;
#71929 = CARTESIAN_POINT ( 'NONE',  ( -0.2308247287459999908, 1470.816572150329876, 188.6928027695979893 ) ) ;
#71930 = CARTESIAN_POINT ( 'NONE',  ( -106.1419745320000061, 1379.261221625959934, 307.4042368804589955 ) ) ;
#71931 = ORIENTED_EDGE ( 'NONE', *, *, #65263, .F. ) ;
#71932 = CARTESIAN_POINT ( 'NONE',  ( -3.265407155974999753, 1516.754149861460064, 204.5121726906670006 ) ) ;
#71933 = CARTESIAN_POINT ( 'NONE',  ( 1.777755710779999943, 1405.800407096930030, 268.4824710471980325 ) ) ;
#71934 = CARTESIAN_POINT ( 'NONE',  ( -0.7620301703830010265, 1515.588179473189939, 213.1365024013990137 ) ) ;
#71935 = CARTESIAN_POINT ( 'NONE',  ( 39.04070846521679528, 1456.280716702200152, 270.3387515494820263 ) ) ;
#71936 = CARTESIAN_POINT ( 'NONE',  ( -0.0002122017571388959824, 1432.353341358199941, 123.3907408769529894 ) ) ;
#71937 = CARTESIAN_POINT ( 'NONE',  ( 11.60004869883886869, 1424.049974457302142, 137.1751211143046874 ) ) ;
#71938 = CARTESIAN_POINT ( 'NONE',  ( -10.10200468158650011, 1447.143925580010091, 211.2823309413680022 ) ) ;
#71939 = CARTESIAN_POINT ( 'NONE',  ( 12.53380745427929988, 1442.773887455719887, 186.4115735415020083 ) ) ;
#71940 = CARTESIAN_POINT ( 'NONE',  ( 14.39948538648319776, 1509.538292521139510, 235.4401890623756799 ) ) ;
#71941 = CARTESIAN_POINT ( 'NONE',  ( -22.08327125186963258, 1523.604703353109926, 184.4267662568474009 ) ) ;
#71942 = CARTESIAN_POINT ( 'NONE',  ( 17.38482601099109814, 1410.884446382940041, 192.4603632472940262 ) ) ;
#71943 = EDGE_CURVE ( 'NONE', #92278, #105852, #103188, .T. ) ;
#71944 = VERTEX_POINT ( 'NONE', #25929 ) ;
#71945 = CARTESIAN_POINT ( 'NONE',  ( 6.439293542829999756E-15, 1420.418457356630142, 243.9198229339980060 ) ) ;
#71946 = CARTESIAN_POINT ( 'NONE',  ( 9.501613403289589144, 1467.857654184219882, 205.8614462207000031 ) ) ;
#71947 = CARTESIAN_POINT ( 'NONE',  ( -0.3397164161819999917, 1476.075833985229792, 267.5371225513979994 ) ) ;
#71948 = CARTESIAN_POINT ( 'NONE',  ( 19.38392212389999969, 1495.496321584190127, 199.6762541507190178 ) ) ;
#71949 = CARTESIAN_POINT ( 'NONE',  ( -29.12559713569999786, 1509.873774314229877, 210.4730869765679984 ) ) ;
#71950 = CARTESIAN_POINT ( 'NONE',  ( -3.854452527945675389, 1448.295591906145319, 185.0328819066131700 ) ) ;
#71951 = CARTESIAN_POINT ( 'NONE',  ( -40.62633303070520441, 1384.784726197159898, 243.2388129929060199 ) ) ;
#71952 = CIRCLE ( 'NONE', #75522, 28.41070217520000440 ) ;
#71953 = CARTESIAN_POINT ( 'NONE',  ( 12.32716646574370145, 1492.190914138330072, 209.5898718627249764 ) ) ;
#71954 = CARTESIAN_POINT ( 'NONE',  ( -10.49359245019999953, 1482.960578323189793, 204.4802844074689858 ) ) ;
#71955 = CARTESIAN_POINT ( 'NONE',  ( 26.80802651847389839, 1435.516884147950122, 135.8294075311020208 ) ) ;
#71956 = CARTESIAN_POINT ( 'NONE',  ( -2.313829914396530185, 1395.993861108439887, 219.8905569203290042 ) ) ;
#71957 = CARTESIAN_POINT ( 'NONE',  ( -14.75316392789999931, 1422.315547878330108, 228.7562151032980182 ) ) ;
#71958 = CARTESIAN_POINT ( 'NONE',  ( -20.79738390328697761, 1511.187213306747708, 237.0406858230491025 ) ) ;
#71959 = ORIENTED_EDGE ( 'NONE', *, *, #49598, .T. ) ;
#71960 = EDGE_CURVE ( 'NONE', #39586, #97416, #69790, .T. ) ;
#71961 = CARTESIAN_POINT ( 'NONE',  ( -13.90496247579444322, 1414.913060387329779, 200.7481815758607411 ) ) ;
#71962 = CARTESIAN_POINT ( 'NONE',  ( 1.943617413929999982, 1409.147975478429998, 231.3620511928980079 ) ) ;
#71963 = CARTESIAN_POINT ( 'NONE',  ( -11.86590139589999815, 1432.348266868109931, 151.0567667964980103 ) ) ;
#71965 = CARTESIAN_POINT ( 'NONE',  ( -13.59434826296499921, 1512.526319173689899, 193.1055684605670137 ) ) ;
#71964 = CARTESIAN_POINT ( 'NONE',  ( 11.62168133680000004, 1426.773520508030060, 135.9278380674980156 ) ) ;
#71966 = CARTESIAN_POINT ( 'NONE',  ( -18.39846574424100112, 1508.551704408389924, 210.4158962701780240 ) ) ;
#71967 = CARTESIAN_POINT ( 'NONE',  ( 4.210524679639359391, 1424.023046679440085, 184.1832055361919913 ) ) ;
#71968 = CARTESIAN_POINT ( 'NONE',  ( -109.9864287870510111, 1384.705349330230092, 311.4509910198939906 ) ) ;
#71969 = CARTESIAN_POINT ( 'NONE',  ( 7.278733183479999980, 1426.463158066219876, 212.8449153079989742 ) ) ;
#71970 = CARTESIAN_POINT ( 'NONE',  ( -17.55008888309999904, 1487.029577685089862, 194.9701234138989889 ) ) ;
#71971 = CARTESIAN_POINT ( 'NONE',  ( 1.585275487589999921, 1508.725511249229839, 180.2575163522980120 ) ) ;
#71972 = CARTESIAN_POINT ( 'NONE',  ( 7.105427357599999217E-15, 1423.509254465030153, 167.6739826277979830 ) ) ;
#71973 = CARTESIAN_POINT ( 'NONE',  ( -66.39852830834199438, 1377.354015942380101, 281.9312505627179917 ) ) ;
#71974 = CARTESIAN_POINT ( 'NONE',  ( 3.421935753948512016, 1367.252205776827850, 208.3718459617061285 ) ) ;
#71976 = ORIENTED_EDGE ( 'NONE', *, *, #13146, .F. ) ;
#71975 = CARTESIAN_POINT ( 'NONE',  ( -14.03937168550959846, 1379.585977840610212, 211.7499898191520344 ) ) ;
#71977 = ORIENTED_EDGE ( 'NONE', *, *, #30273, .T. ) ;
#71978 = CARTESIAN_POINT ( 'NONE',  ( -10.57949873459999779, 1396.282504623229897, 204.0310317109180005 ) ) ;
#71979 = CARTESIAN_POINT ( 'NONE',  ( -11.49359948000000031, 1409.314425725430056, 190.5616205332979973 ) ) ;
#71980 = CARTESIAN_POINT ( 'NONE',  ( 8.099819236969999281, 1497.713060387329961, 229.6744222972979799 ) ) ;
#71981 = CARTESIAN_POINT ( 'NONE',  ( -8.072094066334999596, 1511.572472350439739, 212.7333085737770091 ) ) ;
#71983 = DIRECTION ( 'NONE',  ( 0.000000000000000000, -1.000000000000000000, 0.000000000000000000 ) ) ;
#71982 = CARTESIAN_POINT ( 'NONE',  ( -7.946775756959999271, 1383.555175293329967, 218.7288224669989916 ) ) ;
#71984 = CARTESIAN_POINT ( 'NONE',  ( -31.34137657907861652, 1523.481610118011986, 196.3411265156833565 ) ) ;
#71985 = CARTESIAN_POINT ( 'NONE',  ( 19.39983987835422496, 1501.977400791986611, 239.2921289694223219 ) ) ;
#71986 = CARTESIAN_POINT ( 'NONE',  ( -41.48253158878969771, 1444.135608968060069, 136.5500586159059822 ) ) ;
#71987 = CARTESIAN_POINT ( 'NONE',  ( 37.28638872520870251, 1436.958943370610086, 136.2769035375250155 ) ) ;
#71988 = CARTESIAN_POINT ( 'NONE',  ( 22.03465957474552539, 1512.187213306747481, 182.8300405912328301 ) ) ;
#71989 = CARTESIAN_POINT ( 'NONE',  ( 33.92729347383400551, 1436.577116162089851, 136.5096455005439964 ) ) ;
#71990 = CARTESIAN_POINT ( 'NONE',  ( -3.772679660826560255, 1406.882484426249903, 269.6459227122439870 ) ) ;
#71991 = FACE_OUTER_BOUND ( 'NONE', #36459, .T. ) ;
#71992 = ORIENTED_EDGE ( 'NONE', *, *, #110291, .T. ) ;
#71993 = CARTESIAN_POINT ( 'NONE',  ( 4.087259578919999470, 1424.194160912629968, 184.7150810775980005 ) ) ;
#71994 = ORIENTED_EDGE ( 'NONE', *, *, #47610, .F. ) ;
#71995 = ORIENTED_EDGE ( 'NONE', *, *, #34372, .T. ) ;
#71996 = ADVANCED_FACE ( 'NONE', ( #26491 ), #60730, .F. ) ;
#71997 = CARTESIAN_POINT ( 'NONE',  ( 0.000000000000000000, 1511.187213306747708, 179.0139814193315999 ) ) ;
#71998 = CARTESIAN_POINT ( 'NONE',  ( 17.68237282055029880, 1517.151704408390060, 212.5589510568480023 ) ) ;
#71999 = ADVANCED_FACE ( 'NONE', ( #48839 ), #6255, .T. ) ;
#72000 = CARTESIAN_POINT ( 'NONE',  ( 6.557909882634999299, 1516.908489800550115, 214.8995913655070069 ) ) ;
#72001 = CARTESIAN_POINT ( 'NONE',  ( 5.139225450924999272, 1511.037966505499980, 216.8073032440570103 ) ) ;
#72002 = ORIENTED_EDGE ( 'NONE', *, *, #19527, .F. ) ;
#72003 = CARTESIAN_POINT ( 'NONE',  ( -5.985688616083930214, 1509.236238061519771, 179.5306295814190207 ) ) ;
#72004 = CARTESIAN_POINT ( 'NONE',  ( -68.69226509189999774, 1379.746858117560123, 280.5557816734590233 ) ) ;
#72005 =( BOUNDED_CURVE ( )  B_SPLINE_CURVE ( 3, ( #8241, #59783, #85496, #8795 ),
 .UNSPECIFIED., .F., .F. ) 
 B_SPLINE_CURVE_WITH_KNOTS ( ( 4, 4 ),
 ( 4.621677078022849550, 4.871924224616510202 ),
 .UNSPECIFIED. ) 
 CURVE ( )  GEOMETRIC_REPRESENTATION_ITEM ( )  RATIONAL_B_SPLINE_CURVE ( ( 1.000000000000000000, 0.9947881687906164894, 0.9947881687906164894, 1.000000000000000000 ) ) 
 REPRESENTATION_ITEM ( '' )  );
#72006 = CARTESIAN_POINT ( 'NONE',  ( 5.332222640600000396, 1416.518532928330160, 226.4836215587980064 ) ) ;
#72007 = CARTESIAN_POINT ( 'NONE',  ( -2.296124889065000119, 1516.677239312369920, 204.5136991508470032 ) ) ;
#72008 = CARTESIAN_POINT ( 'NONE',  ( -28.54286204732466103, 1526.382868172863937, 219.8009395035764726 ) ) ;
#72009 = CARTESIAN_POINT ( 'NONE',  ( -113.4000000000000057, 1384.913060387289988, 297.2218459572590064 ) ) ;
#72010 = CARTESIAN_POINT ( 'NONE',  ( -3.672183373650000249, 1409.545492258829881, 232.1063284713980011 ) ) ;
#72012 = EDGE_LOOP ( 'NONE', ( #28350, #75101, #61593, #42299 ) ) ;
#72011 = CARTESIAN_POINT ( 'NONE',  ( 13.51610093809999924, 1443.913060387330006, 169.3501091259980171 ) ) ;
#72013 = CARTESIAN_POINT ( 'NONE',  ( 0.000000000000000000, 1523.382868172864164, 209.1218459616979999 ) ) ;
#72014 = DIRECTION ( 'NONE',  ( 0.000000000000000000, -1.000000000000000000, 6.123233995736769734E-17 ) ) ;
#72015 = CARTESIAN_POINT ( 'NONE',  ( -22.68421185029999876, 1384.517311655589992, 222.0365106238589874 ) ) ;
#72016 = CARTESIAN_POINT ( 'NONE',  ( 30.31940284292419818, 1523.382868172864164, 222.4933038710543087 ) ) ;
#72017 = ADVANCED_FACE ( 'NONE', ( #31450 ), #60837, .T. ) ;
#72018 = CARTESIAN_POINT ( 'NONE',  ( 40.92984665081159790, 1427.618493474619981, 270.2459107829799905 ) ) ;
#72019 = CARTESIAN_POINT ( 'NONE',  ( 3.460101851884999746, 1516.812923327049930, 213.1504765548870068 ) ) ;
#72020 = CIRCLE ( 'NONE', #9174, 3.999999999999997335 ) ;
#72021 = CARTESIAN_POINT ( 'NONE',  ( -67.97548607400000265, 1379.747377450629983, 278.4939589122589609 ) ) ;
#72022 = CARTESIAN_POINT ( 'NONE',  ( 23.67748127589999996, 1410.709634711930221, 207.9970578281480016 ) ) ;
#72023 = CARTESIAN_POINT ( 'NONE',  ( 0.01564820846407900465, 1507.754288909950901, 237.4874347475621619 ) ) ;
#72024 = CARTESIAN_POINT ( 'NONE',  ( 14.76737052841249920, 1427.310067236570148, 198.6611131540680049 ) ) ;
#72026 = EDGE_CURVE ( 'NONE', #69447, #106884, #97782, .T. ) ;
#72025 = CARTESIAN_POINT ( 'NONE',  ( -0.03314418650357400103, 1502.038643116309913, 233.2541165707570201 ) ) ;
#72027 = CARTESIAN_POINT ( 'NONE',  ( 3.460866170685000132, 1517.020847257979995, 209.8575449048190080 ) ) ;
#72028 = ORIENTED_EDGE ( 'NONE', *, *, #31527, .F. ) ;
#72029 = CARTESIAN_POINT ( 'NONE',  ( 4.291363136070279083, 1421.924736920739861, 184.1044750076529795 ) ) ;
#72030 = CARTESIAN_POINT ( 'NONE',  ( -3.615035349779999851, 1420.447245347430226, 232.7901725780979802 ) ) ;
#72031 = CARTESIAN_POINT ( 'NONE',  ( -102.7367842069999995, 1384.710423195750082, 311.2303077692589568 ) ) ;
#72032 = EDGE_CURVE ( 'NONE', #78921, #328, #24386, .T. ) ;
#72033 = EDGE_LOOP ( 'NONE', ( #69333, #105773, #28439, #51780 ) ) ;
#72034 = CARTESIAN_POINT ( 'NONE',  ( -22.02211068124400128, 1385.268219036880055, 221.8684547256000030 ) ) ;
#72035 = CARTESIAN_POINT ( 'NONE',  ( -2.940135782350000060, 1428.954742266889980, 200.2247184200489869 ) ) ;
#72036 = CARTESIAN_POINT ( 'NONE',  ( -21.87101081987050222, 1509.710974767680000, 229.2198085769670115 ) ) ;
#72037 = CARTESIAN_POINT ( 'NONE',  ( -0.6157698266020030786, 1500.133018751690088, 230.4529138410990186 ) ) ;
#72038 = CARTESIAN_POINT ( 'NONE',  ( 0.2565248355029999816, 1409.415731479529995, 232.9897570089979979 ) ) ;
#72039 = CARTESIAN_POINT ( 'NONE',  ( 0.07335717183216540482, 1420.449307609759899, 182.6843235195379975 ) ) ;
#72040 = EDGE_CURVE ( 'NONE', #105370, #10196, #73801, .T. ) ;
#72042 = CARTESIAN_POINT ( 'NONE',  ( 4.329791490734999471, 1515.051704408389924, 212.4519801359869859 ) ) ;
#72041 = CARTESIAN_POINT ( 'NONE',  ( 1.131796810615000037, 1516.659138130710289, 214.8948242487770131 ) ) ;
#72043 = CARTESIAN_POINT ( 'NONE',  ( 19.26470018019999841, 1508.010672954829943, 188.6340786004979861 ) ) ;
#72044 = CARTESIAN_POINT ( 'NONE',  ( 10.08381526586729926, 1469.545492192299889, 207.5775108819740069 ) ) ;
#72045 = EDGE_LOOP ( 'NONE', ( #98909, #36433 ) ) ;
#72046 = CARTESIAN_POINT ( 'NONE',  ( 2.484577657225000014, 1517.170512887980067, 201.7834339727070017 ) ) ;
#72047 = DIRECTION ( 'NONE',  ( 1.755985294532464991E-16, -1.000000000000000000, 1.338183447452830017E-16 ) ) ;
#72048 = ORIENTED_EDGE ( 'NONE', *, *, #80775, .T. ) ;
#72049 = CARTESIAN_POINT ( 'NONE',  ( -0.1702787592430000108, 1497.005873238030063, 230.8763743371980013 ) ) ;
#72050 = EDGE_CURVE ( 'NONE', #88934, #26765, #1848, .T. ) ;
#72051 = CARTESIAN_POINT ( 'NONE',  ( -13.74310390781900004, 1517.051704408389924, 201.1531303618569950 ) ) ;
#72052 = CARTESIAN_POINT ( 'NONE',  ( 9.044573916982399098, 1425.064980843364992, 195.6694192215943815 ) ) ;
#72053 = EDGE_CURVE ( 'NONE', #89980, #71879, #32194, .T. ) ;
#72054 = CARTESIAN_POINT ( 'NONE',  ( -0.4938125538340010778, 1443.407940923189926, 218.3972833972489980 ) ) ;
#72055 = CARTESIAN_POINT ( 'NONE',  ( -26.38747615144840353, 1508.287016310790023, 201.5298666568500039 ) ) ;
#72056 = CARTESIAN_POINT ( 'NONE',  ( 4.401092417150000102, 1420.174153566729956, 185.7217845719979721 ) ) ;
#72057 = CARTESIAN_POINT ( 'NONE',  ( -13.80537871780000003, 1434.979603129589805, 148.5370412790979913 ) ) ;
#72058 = CARTESIAN_POINT ( 'NONE',  ( -19.75056259240000145, 1465.177823603190063, 209.1218459616989946 ) ) ;
#72059 = CARTESIAN_POINT ( 'NONE',  ( 18.11157302770000044, 1509.545530454130130, 186.5307135953979980 ) ) ;
#72061 = CARTESIAN_POINT ( 'NONE',  ( 28.25086641300000068, 1508.135711190629991, 209.3856964555159834 ) ) ;
#72060 = CARTESIAN_POINT ( 'NONE',  ( 1.270728227940000066, 1414.996442546130083, 191.7853923321980005 ) ) ;
#72062 = EDGE_CURVE ( 'NONE', #53799, #57779, #42912, .T. ) ;
#72063 = CARTESIAN_POINT ( 'NONE',  ( 0.4681535437661719090, 1524.397344074316607, 244.4282029790948627 ) ) ;
#72064 = ORIENTED_EDGE ( 'NONE', *, *, #3058, .F. ) ;
#72065 = CARTESIAN_POINT ( 'NONE',  ( -103.6168536339999946, 1379.900079317219934, 303.2097866628589600 ) ) ;
#72066 = CARTESIAN_POINT ( 'NONE',  ( -16.52648624529999921, 1508.522148411690068, 213.6168893376890026 ) ) ;
#72067 = CARTESIAN_POINT ( 'NONE',  ( -45.09884245687089788, 1435.519538208483709, 268.9899558901107071 ) ) ;
#72068 = EDGE_CURVE ( 'NONE', #1550, #36754, #32007, .T. ) ;
#72069 = CARTESIAN_POINT ( 'NONE',  ( -23.93221639060000072, 1436.995215223070090, 212.4007312564980055 ) ) ;
#72070 = LINE ( 'NONE', #46855, #45355 ) ;
#72071 = DIRECTION ( 'NONE',  ( -0.9455185755993178454, 0.000000000000000000, 0.3255681544571539798 ) ) ;
#72072 = CARTESIAN_POINT ( 'NONE',  ( 12.63891593913163014, 1435.851297268093504, 150.8990495699463565 ) ) ;
#72073 = CARTESIAN_POINT ( 'NONE',  ( -17.10420012025889847, 1414.913526845469960, 207.6224735737659728 ) ) ;
#72074 = CARTESIAN_POINT ( 'NONE',  ( 5.755594507168209084, 1494.343245214239914, 219.1208262999909948 ) ) ;
#72075 = ADVANCED_FACE ( 'NONE', ( #66196 ), #100844, .F. ) ;
#72076 = CARTESIAN_POINT ( 'NONE',  ( -8.494709194219998594, 1488.072329416189859, 217.7903042847989923 ) ) ;
#72077 = CARTESIAN_POINT ( 'NONE',  ( -18.47517498779149747, 1466.235640218240178, 200.8822797504410005 ) ) ;
#72078 = CARTESIAN_POINT ( 'NONE',  ( -81.02254885351089797, 1383.776253998839820, 304.3069785600009709 ) ) ;
#72079 = CARTESIAN_POINT ( 'NONE',  ( -109.2306744385840034, 1383.829459731100087, 311.1332719636980073 ) ) ;
#72080 = CARTESIAN_POINT ( 'NONE',  ( 5.773132394310000137, 1428.572103629089952, 215.3275095299590021 ) ) ;
#72082 = ORIENTED_EDGE ( 'NONE', *, *, #93906, .F. ) ;
#72081 = CARTESIAN_POINT ( 'NONE',  ( -8.799999999999998934, 1412.913060387329779, 209.1218459616989946 ) ) ;
#72083 = CARTESIAN_POINT ( 'NONE',  ( -102.9989294650000033, 1380.111416001630232, 307.4955441714590165 ) ) ;
#72084 = CARTESIAN_POINT ( 'NONE',  ( 13.58541694415399981, 1512.759354980459875, 224.4342445094760023 ) ) ;
#72085 = ORIENTED_EDGE ( 'NONE', *, *, #27349, .F. ) ;
#72086 = ORIENTED_EDGE ( 'NONE', *, *, #52584, .T. ) ;
#72087 = CARTESIAN_POINT ( 'NONE',  ( 17.15013451049770055, 1414.913057819779851, 210.5788933209909715 ) ) ;
#72088 = CARTESIAN_POINT ( 'NONE',  ( 2.475018581880529922, 1497.111080376900190, 196.9667223532030107 ) ) ;
#72089 = CARTESIAN_POINT ( 'NONE',  ( 13.42574451573709915, 1443.464390912571616, 169.3656144573682241 ) ) ;
#72091 = CARTESIAN_POINT ( 'NONE',  ( -29.87496815560000130, 1440.913060384770006, 238.0574314952980046 ) ) ;
#72090 = CARTESIAN_POINT ( 'NONE',  ( 40.69310009642936166, 1433.220003743809912, 269.6228712187607357 ) ) ;
#72092 = CARTESIAN_POINT ( 'NONE',  ( -19.59580092090000036, 1494.488138752529949, 189.3579594609980177 ) ) ;
#72093 = CARTESIAN_POINT ( 'NONE',  ( -11.81944340819999972, 1433.674010844490113, 150.7526810563979893 ) ) ;
#72094 = CARTESIAN_POINT ( 'NONE',  ( -5.100957845159999948, 1482.122785942490054, 228.9672709512990139 ) ) ;
#72095 = CARTESIAN_POINT ( 'NONE',  ( -19.82947209420000334, 1486.245552723730043, 190.1506153878980001 ) ) ;
#72096 = CARTESIAN_POINT ( 'NONE',  ( 6.413454494903159997, 1466.819085582309981, 216.7143828116000179 ) ) ;
#72097 = CARTESIAN_POINT ( 'NONE',  ( 6.328983188139999605, 1409.301000327829797, 187.4842807998980163 ) ) ;
#72098 = CARTESIAN_POINT ( 'NONE',  ( 5.461421721539999830, 1423.173959525930059, 185.7905159978980123 ) ) ;
#72099 = CARTESIAN_POINT ( 'NONE',  ( -24.49316664000000188, 1440.648604759869841, 210.9862992980479817 ) ) ;
#72100 = CARTESIAN_POINT ( 'NONE',  ( 7.036086740800000072, 1439.758761535590111, 154.1890769228979821 ) ) ;
#72101 = CARTESIAN_POINT ( 'NONE',  ( -7.281830411814069315, 1478.108126808140014, 218.1541311745150153 ) ) ;
#72102 = FACE_OUTER_BOUND ( 'NONE', #87553, .T. ) ;
#72103 = EDGE_CURVE ( 'NONE', #59489, #67300, #85888, .T. ) ;
#72105 = EDGE_LOOP ( 'NONE', ( #44501, #14326, #62209, #86413 ) ) ;
#72104 = CARTESIAN_POINT ( 'NONE',  ( 2.485998036212079895E-11, 1411.655689664790089, 254.4737176916400188 ) ) ;
#72106 = ORIENTED_EDGE ( 'NONE', *, *, #51036, .F. ) ;
#72107 = CARTESIAN_POINT ( 'NONE',  ( -11.85761565696060060, 1431.744374585950027, 149.9502556072889945 ) ) ;
#72108 = EDGE_CURVE ( 'NONE', #28853, #24977, #88464, .T. ) ;
#72109 = CARTESIAN_POINT ( 'NONE',  ( -11.69896337610000181, 1483.759246082390064, 228.3345905838990291 ) ) ;
#72110 = CARTESIAN_POINT ( 'NONE',  ( -25.30728195769999900, 1466.918094299930090, 270.3546022141979961 ) ) ;
#72111 = CARTESIAN_POINT ( 'NONE',  ( 37.65047687761219919, 1442.773887286080026, 137.1096749932030150 ) ) ;
#72112 = CARTESIAN_POINT ( 'NONE',  ( -102.6425412143391469, 1375.179104070689618, 310.0986724762475433 ) ) ;
#72113 = CARTESIAN_POINT ( 'NONE',  ( -14.94781368989999848, 1495.930802959929906, 224.6074030012979961 ) ) ;
#72114 = CARTESIAN_POINT ( 'NONE',  ( 0.3084180738009330014, 1451.032819945409983, 181.9791184512139921 ) ) ;
#72115 = CARTESIAN_POINT ( 'NONE',  ( 3.495214741176849937, 1484.713663407669856, 220.4421414041750040 ) ) ;
#72116 = CARTESIAN_POINT ( 'NONE',  ( -29.85692247043837710, 1525.159196711359755, 222.1259805706810084 ) ) ;
#72117 = CARTESIAN_POINT ( 'NONE',  ( -1.404759085750468373, 1484.431622893082249, 182.4191754957871296 ) ) ;
#72118 = CARTESIAN_POINT ( 'NONE',  ( 9.559785582989375641, 1361.831719013449856, 210.6218459617030021 ) ) ;
#72119 = CARTESIAN_POINT ( 'NONE',  ( -44.73938210465490073, 1432.137784287730028, 267.0202877731520061 ) ) ;
#72120 = ORIENTED_EDGE ( 'NONE', *, *, #11972, .T. ) ;
#72121 = CARTESIAN_POINT ( 'NONE',  ( -7.800000000000001599, 1392.213060387289943, 209.1218459616989946 ) ) ;
#72122 = ORIENTED_EDGE ( 'NONE', *, *, #1915, .F. ) ;
#72123 = EDGE_LOOP ( 'NONE', ( #55598, #15443, #81732, #15631 ) ) ;
#72124 = CARTESIAN_POINT ( 'NONE',  ( -7.708745685915000756, 1516.523379810429788, 210.8299382363969983 ) ) ;
#72125 = ADVANCED_FACE ( 'NONE', ( #11766 ), #62200, .F. ) ;
#72126 = APPLICATION_CONTEXT ( 'automotive_design' ) ;
#72127 = CARTESIAN_POINT ( 'NONE',  ( 16.89684008137831484, 1409.672990159872597, 224.8086551987313726 ) ) ;
#72128 = CARTESIAN_POINT ( 'NONE',  ( -15.33845266750000036, 1425.420605040230157, 190.2292057122979827 ) ) ;
#72129 = CARTESIAN_POINT ( 'NONE',  ( -3.289314091018219699, 1497.168725298330173, 221.0708042131589934 ) ) ;
#72130 = EDGE_LOOP ( 'NONE', ( #71874, #97023, #48719, #50363 ) ) ;
#72131 = CARTESIAN_POINT ( 'NONE',  ( 6.554151426245000245, 1516.906641539930206, 201.7900338461269882 ) ) ;
#72132 = ADVANCED_FACE ( 'NONE', ( #72248 ), #17729, .T. ) ;
#72133 = CARTESIAN_POINT ( 'NONE',  ( 6.024188629869999367, 1473.161425684690130, 217.8957855105489898 ) ) ;
#72134 = CARTESIAN_POINT ( 'NONE',  ( 0.4649367091635221994, 1508.983694905193943, 238.8636469665097763 ) ) ;
#72135 = VERTEX_POINT ( 'NONE', #108579 ) ;
#72136 = CARTESIAN_POINT ( 'NONE',  ( -13.38634297238620086, 1410.004322308419887, 270.4097950069890430 ) ) ;
#72137 = CARTESIAN_POINT ( 'NONE',  ( 4.017110540329999856E-16, 1428.413060387330006, 91.31218443469779800 ) ) ;
#72138 = FACE_OUTER_BOUND ( 'NONE', #68537, .T. ) ;
#72139 = EDGE_CURVE ( 'NONE', #98647, #101745, #24967, .T. ) ;
#72141 = ORIENTED_EDGE ( 'NONE', *, *, #97442, .T. ) ;
#72140 = CARTESIAN_POINT ( 'NONE',  ( -9.934709065808439377, 1365.494406819946107, 210.6218459616987957 ) ) ;
#72142 = VERTEX_POINT ( 'NONE', #107467 ) ;
#72143 = CARTESIAN_POINT ( 'NONE',  ( 45.63156121253045683, 1441.449654500054976, 268.9749044632669666 ) ) ;
#72144 = CARTESIAN_POINT ( 'NONE',  ( 11.34298750825909963, 1471.339403186539812, 210.4402065159420090 ) ) ;
#72145 = CARTESIAN_POINT ( 'NONE',  ( -23.10442739037580040, 1411.095127590459924, 210.9251608898400150 ) ) ;
#72146 = DIRECTION ( 'NONE',  ( -0.6736849260863839728, 0.000000000000000000, 0.7390186874254150995 ) ) ;
#72147 = CARTESIAN_POINT ( 'NONE',  ( 2.500000195207620290, 1448.894380947069976, 182.3534016008459844 ) ) ;
#72148 = CARTESIAN_POINT ( 'NONE',  ( 5.395424494550000283, 1433.568245638130065, 154.6346167951979851 ) ) ;
#72149 = CARTESIAN_POINT ( 'NONE',  ( -14.45805363400000054, 1420.164084007830070, 221.6834749228980002 ) ) ;
#72150 = CARTESIAN_POINT ( 'NONE',  ( 11.24049419410000006, 1414.988017874730076, 222.4824403021980004 ) ) ;
#72151 = EDGE_CURVE ( 'NONE', #35341, #56358, #60520, .T. ) ;
#72152 = CARTESIAN_POINT ( 'NONE',  ( -7.005862043813290743E-15, 1521.551704408389924, 209.1218459616989946 ) ) ;
#72153 = CARTESIAN_POINT ( 'NONE',  ( 2.476733476015000157, 1516.858326417339867, 206.6281461634669938 ) ) ;
#72154 = VERTEX_POINT ( 'NONE', #75551 ) ;
#72155 = CARTESIAN_POINT ( 'NONE',  ( -38.81202640297369300, 1436.797832147450208, 135.6928027013960047 ) ) ;
#72156 = CARTESIAN_POINT ( 'NONE',  ( -21.11429705600878393, 1454.601516258118863, 222.9879907867546649 ) ) ;
#72157 = ORIENTED_EDGE ( 'NONE', *, *, #9743, .F. ) ;
#72158 = LINE ( 'NONE', #99505, #15881 ) ;
#72159 = EDGE_CURVE ( 'NONE', #14138, #71450, #19020, .T. ) ;
#72160 = CARTESIAN_POINT ( 'NONE',  ( 25.41125599211969899, 1450.806039855719973, 137.2920521431910004 ) ) ;
#72161 = FACE_OUTER_BOUND ( 'NONE', #41545, .T. ) ;
#72162 = CARTESIAN_POINT ( 'NONE',  ( -9.104488409295518281, 1384.623999641839873, 199.9569213373260084 ) ) ;
#72163 = CARTESIAN_POINT ( 'NONE',  ( 18.81460391099999896, 1409.734757761829997, 196.1127275027980090 ) ) ;
#72164 = CARTESIAN_POINT ( 'NONE',  ( 22.92333831959999557, 1411.083494111930122, 207.1379507454479949 ) ) ;
#72165 = CARTESIAN_POINT ( 'NONE',  ( -24.89775082669573081, 1442.835544666243777, 210.5176539913697980 ) ) ;
#72166 = CARTESIAN_POINT ( 'NONE',  ( -14.08142637225379978, 1379.709117121690042, 211.5303641152310092 ) ) ;
#72167 = CARTESIAN_POINT ( 'NONE',  ( 0.5369751114729359731, 1452.020381932720056, 183.1429488159060099 ) ) ;
#72168 = EDGE_CURVE ( 'NONE', #7001, #75598, #49800, .T. ) ;
#72169 = CARTESIAN_POINT ( 'NONE',  ( 32.02808312589922224, 1501.977400791986611, 219.9649204700462235 ) ) ;
#72170 = CARTESIAN_POINT ( 'NONE',  ( -2.482067898354999969, 1517.099836525840146, 214.9099431973869798 ) ) ;
#72171 = ORIENTED_EDGE ( 'NONE', *, *, #41765, .F. ) ;
#72172 = CARTESIAN_POINT ( 'NONE',  ( 7.709937712299099744, 1516.568902917619880, 207.6216162931799829 ) ) ;
#72173 = B_SPLINE_SURFACE_WITH_KNOTS ( 'NONE', 5, 5, ( 
 ( #40023, #74744, #108333, #65793, #99915, #91535 ),
 ( #14813, #17551, #15898, #33822, #76950, #50640 ),
 ( #69117, #77501, #102124, #42238, #25403, #109992 ),
 ( #102659, #94275, #101559, #801, #51189, #24313 ),
 ( #60154, #85318, #41683, #34386, #76386, #259 ),
 ( #49548, #25959, #92621, #34930, #103218, #59596 ),
 ( #51753, #58495, #101014, #109447, #85889, #67458 ),
 ( #24850, #68560, #7525, #9191, #110535, #43353 ),
 ( #75843, #26526, #68014, #33269, #59053, #16444 ),
 ( #66907, #93174, #60723, #15355, #16989, #83673 ),
 ( #84770, #6970, #8068, #41124, #75304, #93712 ),
 ( #8613, #42790, #32727, #50098, #84225, #80258 ) ),
 .UNSPECIFIED., .F., .F., .F.,
 ( 6, 3, 3, 6 ),
 ( 6, 6 ),
 ( 256.2762652140000341, 274.6371078000000239, 288.1827336739999623, 303.9584180850000052 ),
 ( 0.000000000000000000, 2.000000000000000000 ),
 .UNSPECIFIED. ) ;
#72174 = CARTESIAN_POINT ( 'NONE',  ( -0.4918994192140000443, 1474.175172928430129, 270.1377426665980011 ) ) ;
#72175 = CARTESIAN_POINT ( 'NONE',  ( -3.467940602053699806, 1495.562067921990092, 197.2905559617530002 ) ) ;
#72176 = ADVANCED_FACE ( 'NONE', ( #14505 ), #6111, .T. ) ;
#72177 = CARTESIAN_POINT ( 'NONE',  ( -13.54981492583890024, 1508.446256337960222, 216.7328168714189758 ) ) ;
#72178 = CARTESIAN_POINT ( 'NONE',  ( -36.68740469744260224, 1449.713037953679986, 136.2729166271199972 ) ) ;
#72179 = CARTESIAN_POINT ( 'NONE',  ( 10.93432276284407578, 1424.900206430952039, 138.2785255352749800 ) ) ;
#72180 = CARTESIAN_POINT ( 'NONE',  ( 2.151158825738029190, 1417.448177126915425, 233.3079752067678783 ) ) ;
#72181 = CARTESIAN_POINT ( 'NONE',  ( -1.724584671162449956, 1484.237036739869836, 182.7452427733539935 ) ) ;
#72182 = CARTESIAN_POINT ( 'NONE',  ( 11.68464665229999966, 1433.115614787020149, 150.9197101507980108 ) ) ;
#72183 = CARTESIAN_POINT ( 'NONE',  ( -0.9073772589629539587, 1475.052622579760055, 269.6443551920880282 ) ) ;
#72184 = CARTESIAN_POINT ( 'NONE',  ( 25.38699096459989946, 1440.913060399439928, 218.4286271017939782 ) ) ;
#72185 = CARTESIAN_POINT ( 'NONE',  ( -109.1643725169999897, 1385.128571951890081, 297.1381730982590170 ) ) ;
#72186 = CARTESIAN_POINT ( 'NONE',  ( 10.47998729271419904, 1499.735940323320165, 203.4895150079940151 ) ) ;
#72187 = ORIENTED_EDGE ( 'NONE', *, *, #91306, .T. ) ;
#72188 = EDGE_CURVE ( 'NONE', #33248, #78937, #4388, .T. ) ;
#72189 = CARTESIAN_POINT ( 'NONE',  ( 12.45478753333600430, 1442.762691980110276, 206.9140754477638779 ) ) ;
#72190 = DIRECTION ( 'NONE',  ( 0.9786619618251632957, 0.000000000000000000, -0.2054769195713296581 ) ) ;
#72191 = FACE_OUTER_BOUND ( 'NONE', #49819, .T. ) ;
#72192 = CARTESIAN_POINT ( 'NONE',  ( 12.01579051976940171, 1501.533415298749787, 211.5805978092899977 ) ) ;
#72193 = EDGE_CURVE ( 'NONE', #31705, #42338, #67945, .T. ) ;
#72194 = CARTESIAN_POINT ( 'NONE',  ( -16.33084092821613709, 1420.150255326767819, 208.9983406252053726 ) ) ;
#72195 = CARTESIAN_POINT ( 'NONE',  ( -12.20547381490000127, 1508.837368717929849, 234.0475190257980103 ) ) ;
#72196 = CARTESIAN_POINT ( 'NONE',  ( -26.26504494448730043, 1383.846605286560134, 224.4265172497430001 ) ) ;
#72197 = DIRECTION ( 'NONE',  ( 1.000000000000000000, 0.000000000000000000, 0.000000000000000000 ) ) ;
#72198 = CARTESIAN_POINT ( 'NONE',  ( 2.499944954983469803, 1419.437547127799917, 141.5609276200659963 ) ) ;
#72199 = FACE_OUTER_BOUND ( 'NONE', #73778, .T. ) ;
#72201 = ORIENTED_EDGE ( 'NONE', *, *, #42824, .T. ) ;
#72200 = CARTESIAN_POINT ( 'NONE',  ( -8.776010960647441905, 1437.272641178195499, 153.2877079375153073 ) ) ;
#72202 = CARTESIAN_POINT ( 'NONE',  ( -1.126185392460000045, 1452.246737684529990, 183.5926816214980022 ) ) ;
#72203 = CARTESIAN_POINT ( 'NONE',  ( -36.40844407859999876, 1381.507950937409987, 211.1775457167789796 ) ) ;
#72204 = CARTESIAN_POINT ( 'NONE',  ( -3.265595362850000072, 1475.097840200290193, 198.5785976524989849 ) ) ;
#72206 = ORIENTED_EDGE ( 'NONE', *, *, #89185, .F. ) ;
#72205 = CARTESIAN_POINT ( 'NONE',  ( -17.36569701797450094, 1415.089948427370018, 208.2953144318539671 ) ) ;
#72207 = CARTESIAN_POINT ( 'NONE',  ( -3.005266857462870256, 1450.300088869250203, 188.5532293206870236 ) ) ;
#72208 = ORIENTED_EDGE ( 'NONE', *, *, #39971, .F. ) ;
#72209 = CARTESIAN_POINT ( 'NONE',  ( -9.849592119879998720, 1390.061260120649877, 216.6447051224889719 ) ) ;
#72210 = CARTESIAN_POINT ( 'NONE',  ( -17.83292639989999984, 1416.519106787530063, 211.9794219605880130 ) ) ;
#72211 = LINE ( 'NONE', #63803, #65516 ) ;
#72212 = VECTOR ( 'NONE', #109688, 1000.000000000000000 ) ;
#72213 = CARTESIAN_POINT ( 'NONE',  ( -3.915803421951532748, 1515.051704408389924, 213.4516362061156656 ) ) ;
#72214 = CARTESIAN_POINT ( 'NONE',  ( -15.03789156734744381, 1420.076630009843029, 212.7487531976570097 ) ) ;
#72215 = CARTESIAN_POINT ( 'NONE',  ( 21.02561364274377453, 1509.697797271616992, 188.0382605465152892 ) ) ;
#72216 = CARTESIAN_POINT ( 'NONE',  ( 14.81250144069860042, 1409.430324335749901, 207.2165134956449890 ) ) ;
#72217 = DIRECTION ( 'NONE',  ( 0.3363363969981225110, -0.6659120918163835556, 0.6659120918162170222 ) ) ;
#72218 = CARTESIAN_POINT ( 'NONE',  ( -97.56006093131890111, 1385.214537156219876, 295.7380020258559625 ) ) ;
#72219 = CARTESIAN_POINT ( 'NONE',  ( -18.52991418089999698, 1440.813075470910007, 192.5628466259980200 ) ) ;
#72220 = CARTESIAN_POINT ( 'NONE',  ( -68.70865610920000677, 1379.748126065489942, 280.0489821606589658 ) ) ;
#72221 = CARTESIAN_POINT ( 'NONE',  ( 11.15330175375659927, 1491.129753307649935, 208.9113124793660177 ) ) ;
#72222 = ORIENTED_EDGE ( 'NONE', *, *, #57754, .F. ) ;
#72223 = VERTEX_POINT ( 'NONE', #24548 ) ;
#72224 = CARTESIAN_POINT ( 'NONE',  ( -7.444963660044519926, 1508.731180391400130, 214.6350537475119893 ) ) ;
#72225 = CARTESIAN_POINT ( 'NONE',  ( -12.11709951228450066, 1416.029511585980117, 194.8129639842090057 ) ) ;
#72226 = CARTESIAN_POINT ( 'NONE',  ( -11.14668889100000193, 1434.019367915380144, 151.6529889640980002 ) ) ;
#72227 = CARTESIAN_POINT ( 'NONE',  ( -8.373252022487429826E-10, 1467.972697941590013, 248.1685000166579869 ) ) ;
#72228 = CARTESIAN_POINT ( 'NONE',  ( -20.13950479349729861, 1492.949028624929952, 190.8218133787059969 ) ) ;
#72229 = CARTESIAN_POINT ( 'NONE',  ( -0.08248982457600000096, 1397.911842041330146, 222.1215842558980000 ) ) ;
#72230 = CARTESIAN_POINT ( 'NONE',  ( 30.95751052620454402, 1525.821544997590308, 201.4531494772885196 ) ) ;
#72231 = CARTESIAN_POINT ( 'NONE',  ( -19.25953065130653030, 1486.268686617437652, 189.5640820582841855 ) ) ;
#72232 = CARTESIAN_POINT ( 'NONE',  ( -10.93574897646141153, 1366.250303372820781, 210.6218459617030021 ) ) ;
#72233 = CARTESIAN_POINT ( 'NONE',  ( -26.79413167943010166, 1436.761919080860025, 136.7821860765010058 ) ) ;
#72234 = CARTESIAN_POINT ( 'NONE',  ( 3.300164695495766853, 1524.538768545233779, 176.3797544596794182 ) ) ;
#72235 = CARTESIAN_POINT ( 'NONE',  ( 3.251394362135000105, 1516.757508073510053, 207.4061414411269766 ) ) ;
#72236 = CARTESIAN_POINT ( 'NONE',  ( -13.82697551398640101, 1435.577831593989913, 150.0135038830870258 ) ) ;
#72237 = CARTESIAN_POINT ( 'NONE',  ( -8.305981014989999522, 1385.249635131719970, 218.6869742267090260 ) ) ;
#72238 = CARTESIAN_POINT ( 'NONE',  ( 16.49791572389999672, 1409.489180299430018, 193.7307885960979945 ) ) ;
#72239 = PLANE ( 'NONE',  #51875 ) ;
#72240 = FACE_OUTER_BOUND ( 'NONE', #39185, .T. ) ;
#72241 = ORIENTED_EDGE ( 'NONE', *, *, #15349, .F. ) ;
#72242 = CARTESIAN_POINT ( 'NONE',  ( 5.038677013330000065, 1414.987262866129868, 244.5742075695980020 ) ) ;
#72243 = CARTESIAN_POINT ( 'NONE',  ( -26.22657672300000087, 1469.244931008629919, 207.0149935993579788 ) ) ;
#72245 = CARTESIAN_POINT ( 'NONE',  ( -17.83435983690000270, 1410.458698071030085, 195.0679307497979948 ) ) ;
#72244 = CARTESIAN_POINT ( 'NONE',  ( -3.546950034939999608, 1504.656051162229915, 181.0822442398979888 ) ) ;
#72246 = CARTESIAN_POINT ( 'NONE',  ( -5.513435588854999736, 1508.551704408389924, 216.1347675159770176 ) ) ;
#72247 = CARTESIAN_POINT ( 'NONE',  ( -10.01186952819999831, 1415.800370259029933, 244.5548898303979968 ) ) ;
#72248 = FACE_OUTER_BOUND ( 'NONE', #86543, .T. ) ;
#72249 = CARTESIAN_POINT ( 'NONE',  ( 1.259881505249289102, 1415.704932012589325, 232.9709734747342225 ) ) ;
#72250 = CARTESIAN_POINT ( 'NONE',  ( 33.53414239590000534, 1451.742177158130062, 135.1601382658980128 ) ) ;
#72251 = ORIENTED_EDGE ( 'NONE', *, *, #56340, .F. ) ;
#72252 = CARTESIAN_POINT ( 'NONE',  ( -2.500000000000000000, 1428.057245272730142, 156.8186834866980064 ) ) ;
#72253 = CARTESIAN_POINT ( 'NONE',  ( 15.20279842864010078, 1514.921193439799936, 225.0317510863630162 ) ) ;
#72254 = DIRECTION ( 'NONE',  ( -0.9455185755993178454, 0.000000000000000000, 0.3255681544571537578 ) ) ;
#72255 = ORIENTED_EDGE ( 'NONE', *, *, #97988, .F. ) ;
#72256 = ORIENTED_EDGE ( 'NONE', *, *, #40299, .F. ) ;
#72257 = CARTESIAN_POINT ( 'NONE',  ( 10.11443659974309917, 1452.508654505240202, 209.7494611922460024 ) ) ;
#72258 = CARTESIAN_POINT ( 'NONE',  ( -23.31956537140380092, 1409.842592781089934, 208.8535798542440034 ) ) ;
#72259 = ORIENTED_EDGE ( 'NONE', *, *, #85910, .F. ) ;
#72260 = CARTESIAN_POINT ( 'NONE',  ( 0.3621993321110000275, 1416.825784017230035, 227.1772709138980133 ) ) ;
#72261 = CYLINDRICAL_SURFACE ( 'NONE', #101016, 2.000000000000003553 ) ;
#72262 = CARTESIAN_POINT ( 'NONE',  ( -2.529530985780000130, 1479.773065607530043, 235.7142106943980195 ) ) ;
#72263 = ORIENTED_EDGE ( 'NONE', *, *, #43723, .F. ) ;
#72264 = CARTESIAN_POINT ( 'NONE',  ( 11.63666214179999869, 1425.864857562230100, 144.1663263553980130 ) ) ;
#72265 = CARTESIAN_POINT ( 'NONE',  ( -12.45618235598599988, 1416.218047878440075, 222.0802500694620107 ) ) ;
#72266 = CARTESIAN_POINT ( 'NONE',  ( 0.09323026570510001276, 1419.758325144530090, 184.3752198323979883 ) ) ;
#72267 = ORIENTED_EDGE ( 'NONE', *, *, #39849, .T. ) ;
#72268 = CARTESIAN_POINT ( 'NONE',  ( 3.255967386345000047, 1516.989560013210166, 204.1101670940770134 ) ) ;
#72269 = EDGE_LOOP ( 'NONE', ( #13663, #54773, #2743, #91234, #72171 ) ) ;
#72270 = CARTESIAN_POINT ( 'NONE',  ( 5.436197771951739810, 1483.947504832600089, 219.6404701149249945 ) ) ;
#72271 = EDGE_CURVE ( 'NONE', #86829, #46077, #91019, .T. ) ;
#72272 = CARTESIAN_POINT ( 'NONE',  ( 12.91283110541483481, 1442.898483852980235, 187.0493004153197774 ) ) ;
#72273 = ORIENTED_EDGE ( 'NONE', *, *, #19568, .T. ) ;
#72274 = ORIENTED_EDGE ( 'NONE', *, *, #110707, .T. ) ;
#72275 = CARTESIAN_POINT ( 'NONE',  ( 2.682480990172567470, 1524.330813522192102, 176.3761848884416281 ) ) ;
#72276 = EDGE_CURVE ( 'NONE', #60533, #110334, #20584, .T. ) ;
#72277 = CARTESIAN_POINT ( 'NONE',  ( 17.04521562810657187, 1526.211523310372513, 235.5955797450462796 ) ) ;
#72278 = CARTESIAN_POINT ( 'NONE',  ( 13.08557583159999993, 1509.198239579430037, 234.3544144791979988 ) ) ;
#72279 = CARTESIAN_POINT ( 'NONE',  ( -8.451373773768418474, 1470.993491901630023, 214.7957158758800063 ) ) ;
#72280 = CARTESIAN_POINT ( 'NONE',  ( -4.269482153190000240, 1423.951865566630204, 184.8620142645980025 ) ) ;
#72281 = CARTESIAN_POINT ( 'NONE',  ( 8.743785848119999926, 1420.947065512389827, 196.4302455952989703 ) ) ;
#72282 = CARTESIAN_POINT ( 'NONE',  ( 6.252266454184999489, 1511.741868877540128, 217.9101624594169948 ) ) ;
#72283 = CARTESIAN_POINT ( 'NONE',  ( -4.633397090840619903, 1377.913060387289988, 204.3568503472270095 ) ) ;
#72284 = VECTOR ( 'NONE', #104061, 1000.000000000000114 ) ;
#72285 = CARTESIAN_POINT ( 'NONE',  ( 0.03361787647180682764, 1409.314441787272244, 232.7761456571624024 ) ) ;
#72287 = CARTESIAN_POINT ( 'NONE',  ( -105.9720658651419996, 1391.644115899230201, 306.2957621946390532 ) ) ;
#72286 = CARTESIAN_POINT ( 'NONE',  ( -16.32500455070000100, 1504.098762924189941, 208.8919858110830035 ) ) ;
#72288 = CARTESIAN_POINT ( 'NONE',  ( -60.26586262694746665, 1379.746226297675776, 265.9249327382016190 ) ) ;
#72289 = CARTESIAN_POINT ( 'NONE',  ( -9.526128307108560733, 1440.436522615020067, 205.9995050262249947 ) ) ;
#72290 = CARTESIAN_POINT ( 'NONE',  ( -6.843878254575000319, 1512.371933174370042, 200.6190499138870109 ) ) ;
#72291 = ORIENTED_EDGE ( 'NONE', *, *, #33553, .T. ) ;
#72292 = CARTESIAN_POINT ( 'NONE',  ( 5.757839680740000077, 1413.763055107629953, 262.6648722463980334 ) ) ;
#72293 = AXIS2_PLACEMENT_3D ( 'NONE', #65031, #32525, #50443 ) ;
#72294 = CARTESIAN_POINT ( 'NONE',  ( 40.71506177431396623, 1443.618738248601403, 137.1015905690878185 ) ) ;
#72295 = CARTESIAN_POINT ( 'NONE',  ( -78.30924043174148608, 1384.998499083409797, 302.6966419283749588 ) ) ;
#72296 = ADVANCED_FACE ( 'NONE', ( #36706 ), #50820, .T. ) ;
#72297 = B_SPLINE_SURFACE_WITH_KNOTS ( 'NONE', 5, 1, ( 
 ( #11056, #54732 ),
 ( #79365, #79917 ),
 ( #105677, #55280 ),
 ( #54184, #2679 ),
 ( #96155, #10496 ),
 ( #36249, #88860 ),
 ( #70995, #87775 ),
 ( #36804, #28404 ),
 ( #81007, #72094 ) ),
 .UNSPECIFIED., .F., .F., .F.,
 ( 6, 3, 6 ),
 ( 2, 2 ),
 ( 0.000000000000000000, 3.871851108280000009, 7.729255844190000779 ),
 ( 0.000000000000000000, 14.00000000000000000 ),
 .UNSPECIFIED. ) ;
#72298 = CARTESIAN_POINT ( 'NONE',  ( 5.423172162180000200, 1506.748560102689908, 219.4673452336990067 ) ) ;
#72299 = SHAPE_REPRESENTATION ( 'Grinding Plate', ( #21632 ), #61094 ) ;
#72300 = CARTESIAN_POINT ( 'NONE',  ( -15.28618265780000129, 1416.164270469039820, 211.6194353647389903 ) ) ;
#72302 = ORIENTED_EDGE ( 'NONE', *, *, #37770, .T. ) ;
#72301 = CARTESIAN_POINT ( 'NONE',  ( -17.84478100760759745, 1419.380458095060021, 206.8875292346940000 ) ) ;
#72303 = CARTESIAN_POINT ( 'NONE',  ( 3.355048246850000471, 1428.659755942190031, 216.6919371868989970 ) ) ;
#72304 = CARTESIAN_POINT ( 'NONE',  ( -2.493947715939999643, 1442.756953654919926, 150.6345094620980092 ) ) ;
#72305 = CARTESIAN_POINT ( 'NONE',  ( -16.48345269260000023, 1416.839564662629982, 208.3476362942829780 ) ) ;
#72306 = CARTESIAN_POINT ( 'NONE',  ( 1.419401350206249912, 1430.917749770590035, 199.7704084515799821 ) ) ;
#72307 = CARTESIAN_POINT ( 'NONE',  ( 13.32051254013499886, 1512.868709057579963, 225.8700958719669813 ) ) ;
#72308 = CARTESIAN_POINT ( 'NONE',  ( 4.472031081881574721, 1370.472125110218485, 209.2051454052445081 ) ) ;
#72309 = CARTESIAN_POINT ( 'NONE',  ( 13.17829454071469897, 1509.452805009219901, 181.0409878138019906 ) ) ;
#72310 = CARTESIAN_POINT ( 'NONE',  ( 30.44526109729614305, 1526.211528530236592, 217.1519773718490569 ) ) ;
#72311 = CARTESIAN_POINT ( 'NONE',  ( 11.96010483130011615, 1433.559153112955300, 149.8793145819948620 ) ) ;
#72312 = CARTESIAN_POINT ( 'NONE',  ( 16.13570061800000133, 1417.429050015530038, 227.1491849133979883 ) ) ;
#72313 = CARTESIAN_POINT ( 'NONE',  ( 0.2876204004905856815, 1410.303643508743107, 233.2107274150785656 ) ) ;
#72314 = CARTESIAN_POINT ( 'NONE',  ( -3.462948834675000143, 1516.956048353049937, 206.8373194734570006 ) ) ;
#72315 = CARTESIAN_POINT ( 'NONE',  ( 45.85459148159999643, 1440.913082154319909, 268.7562765770979922 ) ) ;
#72316 = CARTESIAN_POINT ( 'NONE',  ( -18.52609349599999788, 1410.056276687730133, 223.4391609856979812 ) ) ;
#72317 = EDGE_CURVE ( 'NONE', #86947, #89851, #71576, .T. ) ;
#72318 = CARTESIAN_POINT ( 'NONE',  ( 16.85424017000000063, 1435.512808430289851, 147.9204353908980352 ) ) ;
#72319 = CARTESIAN_POINT ( 'NONE',  ( 21.16806657020000060, 1508.013423686629949, 190.7674652822980192 ) ) ;
#72320 = CARTESIAN_POINT ( 'NONE',  ( 23.06896861730000126, 1432.937351989309946, 217.3496264744780149 ) ) ;
#72321 = CARTESIAN_POINT ( 'NONE',  ( -17.51833969970000027, 1423.339066635030122, 226.5264271338980109 ) ) ;
#72322 = CARTESIAN_POINT ( 'NONE',  ( 12.46349861749770049, 1427.083103380439752, 206.6193291359699913 ) ) ;
#72323 = CARTESIAN_POINT ( 'NONE',  ( -39.55169151563139707, 1438.906647882520019, 136.4243423413529968 ) ) ;
#72324 = ADVANCED_FACE ( 'NONE', ( #17241 ), #62501, .F. ) ;
#72325 = CARTESIAN_POINT ( 'NONE',  ( 0.2082676714215480063, 1458.322912406209980, 183.0250375897019808 ) ) ;
#72326 = CARTESIAN_POINT ( 'NONE',  ( -9.544533345749998787, 1409.066719050529855, 198.6089048286980017 ) ) ;
#72327 = CARTESIAN_POINT ( 'NONE',  ( -13.00742463789999981, 1414.913060387329779, 199.6866883146780083 ) ) ;
#72328 = CARTESIAN_POINT ( 'NONE',  ( 17.07724394728954209, 1524.330813522192102, 181.0533268958136830 ) ) ;
#72329 = CARTESIAN_POINT ( 'NONE',  ( -27.78906332080140018, 1508.131006276290009, 210.4760188063899875 ) ) ;
#72330 = CARTESIAN_POINT ( 'NONE',  ( 13.19913408340000061, 1434.900406177449895, 146.4345303725980045 ) ) ;
#72331 = CARTESIAN_POINT ( 'NONE',  ( -37.83686684702099967, 1436.862236044670226, 134.0999999968879877 ) ) ;
#72332 = CARTESIAN_POINT ( 'NONE',  ( 5.960845302450000105, 1441.842620914080044, 183.2877535976979857 ) ) ;
#72333 = ORIENTED_EDGE ( 'NONE', *, *, #39103, .T. ) ;
#72334 = CARTESIAN_POINT ( 'NONE',  ( 2.961801441480000019, 1478.312073041489839, 199.0497942763989840 ) ) ;
#72335 = CARTESIAN_POINT ( 'NONE',  ( 28.11559569350000132, 1443.570698335169936, 137.5389433186979886 ) ) ;
#72336 = CARTESIAN_POINT ( 'NONE',  ( -11.16049073669999991, 1491.416285126389994, 208.9675611111450166 ) ) ;
#72337 = ORIENTED_EDGE ( 'NONE', *, *, #25305, .F. ) ;
#72338 = CARTESIAN_POINT ( 'NONE',  ( -8.590093507847479160, 1437.218756716850066, 210.0971559123210000 ) ) ;
#72339 = CARTESIAN_POINT ( 'NONE',  ( 17.68492033649999939, 1509.541129174830075, 232.7807741972980011 ) ) ;
#72340 = CARTESIAN_POINT ( 'NONE',  ( -30.12632811909999830, 1467.434565237230117, 266.8625626170980354 ) ) ;
#72341 = CARTESIAN_POINT ( 'NONE',  ( -11.60954088560589881, 1481.114764782069869, 211.3792897891370046 ) ) ;
#72342 = CARTESIAN_POINT ( 'NONE',  ( -19.40402912745183173, 1488.299841789603761, 189.5360758023356027 ) ) ;
#72343 = DIRECTION ( 'NONE',  ( -0.7566862579294338920, 0.02642405976598289144, 0.6532439637120530662 ) ) ;
#72344 = CARTESIAN_POINT ( 'NONE',  ( -90.41991271562498866, 1384.618437443740049, 308.8387648450170104 ) ) ;
#72345 = CARTESIAN_POINT ( 'NONE',  ( -46.00916994163010543, 1385.006067563419947, 219.5881877202340036 ) ) ;
#72346 = CARTESIAN_POINT ( 'NONE',  ( -8.770356860863364190, 1423.116964779634145, 210.6628905271092265 ) ) ;
#72347 = CARTESIAN_POINT ( 'NONE',  ( 22.52609269779999934, 1509.699688877929930, 227.6602567939980020 ) ) ;
#72348 = CARTESIAN_POINT ( 'NONE',  ( -32.97913964219446115, 1511.187213306747708, 197.9697544589750464 ) ) ;
#72349 = CARTESIAN_POINT ( 'NONE',  ( -2.470168522032202940, 1523.481610118012441, 175.3649660273468101 ) ) ;
#72351 = EDGE_LOOP ( 'NONE', ( #28581, #55594, #32984, #63314 ) ) ;
#72350 = CARTESIAN_POINT ( 'NONE',  ( 0.4863421998530879642, 1418.702335047680208, 184.7127968358159933 ) ) ;
#72352 = CARTESIAN_POINT ( 'NONE',  ( -9.442895466421070694, 1461.069229439506216, 206.8582801283209847 ) ) ;
#72353 = CARTESIAN_POINT ( 'NONE',  ( 3.803126312677917120, 1420.824521573977336, 137.2929579002170328 ) ) ;
#72354 = CARTESIAN_POINT ( 'NONE',  ( 3.375977092230000309, 1446.395221922789915, 199.5681764357789802 ) ) ;
#72355 = CARTESIAN_POINT ( 'NONE',  ( -12.54660221610000193, 1415.996778984329922, 195.2080008646979934 ) ) ;
#72356 = CARTESIAN_POINT ( 'NONE',  ( 33.42844755917195698, 1522.382868172863937, 222.1271778627166213 ) ) ;
#72357 = CARTESIAN_POINT ( 'NONE',  ( 23.06615049169999665, 1409.718548108430014, 209.6838289468859955 ) ) ;
#72358 = PLANE ( 'NONE',  #57073 ) ;
#72359 = CARTESIAN_POINT ( 'NONE',  ( -19.58883600250999635, 1465.811282985779826, 204.1485273088549945 ) ) ;
#72360 = CARTESIAN_POINT ( 'NONE',  ( -5.381128819750470527, 1430.992662387599921, 154.5043601312420094 ) ) ;
#72362 = CARTESIAN_POINT ( 'NONE',  ( -12.04010205419999835, 1379.345554316609878, 205.4175452398490052 ) ) ;
#72361 = CYLINDRICAL_SURFACE ( 'NONE', #26448, 0.9999999999999865663 ) ;
#72364 = B_SPLINE_CURVE_WITH_KNOTS ( 'NONE', 3,
 ( #56858, #82607, #57966, #5897, #32196, #40042 ),
 .UNSPECIFIED., .F., .F.,
 ( 4, 2, 4 ),
 ( 0.000000000000000000, 0.5000000000000000000, 1.000000000000000000 ),
 .UNSPECIFIED. ) ;
#72363 = CARTESIAN_POINT ( 'NONE',  ( 26.85785241404909840, 1488.762402825080017, 207.6809295873910060 ) ) ;
#72365 = CARTESIAN_POINT ( 'NONE',  ( -113.4000000000000057, 1376.302340817389904, 292.3950450905590515 ) ) ;
#72366 = CARTESIAN_POINT ( 'NONE',  ( 203.9558787908000284, -8382.262153571269664, -1760.903728536709878 ) ) ;
#72367 = CARTESIAN_POINT ( 'NONE',  ( -0.4731238061870000067, 1415.788375264130082, 233.4112679483980060 ) ) ;
#72368 = VECTOR ( 'NONE', #12222, 1000.000000000000227 ) ;
#72369 = CARTESIAN_POINT ( 'NONE',  ( -8.082564370840001899, 1362.241991287399969, 210.6218459616991936 ) ) ;
#72370 = CARTESIAN_POINT ( 'NONE',  ( 2.478306819944999795, 1516.938330505699923, 205.6592251139969960 ) ) ;
#72371 = CARTESIAN_POINT ( 'NONE',  ( -18.43681367705789853, 1485.257906025299917, 189.1833959593609791 ) ) ;
#72372 = ORIENTED_EDGE ( 'NONE', *, *, #69826, .F. ) ;
#72373 = CARTESIAN_POINT ( 'NONE',  ( 11.41987517966060039, 1502.185978170540011, 211.2996822900650216 ) ) ;
#72374 = CARTESIAN_POINT ( 'NONE',  ( -12.46225008516609556, 1421.619546445686638, 210.6462345555370916 ) ) ;
#72376 = ORIENTED_EDGE ( 'NONE', *, *, #47629, .T. ) ;
#72375 = CARTESIAN_POINT ( 'NONE',  ( -68.07056945215670396, 1379.746976000390077, 279.5289119377829934 ) ) ;
#72377 = B_SPLINE_CURVE_WITH_KNOTS ( 'NONE', 3,
 ( #57818, #15217, #75709, #15752, #85189, #34793, #24167, #58357, #34242, #58908, #59469, #75166, #102528, #94139, #8475, #23636, #24709, #109315, #25267, #68426, #77361, #49953, #7933, #83534, #100348, #25820, #92481, #101419 ),
 .UNSPECIFIED., .F., .F.,
 ( 4, 3, 3, 3, 3, 3, 3, 3, 3, 4 ),
 ( -1.114100600540000041, -0.9686789198448820803, -0.7108214831117060095, -0.4506324998962669692, -0.1893315385652869498, 0.07294047128922009904, 0.3351094554373470480, 0.5965822039599320004, 0.8568144055465909403, 1.114100600540000041 ),
 .UNSPECIFIED. ) ;
#72378 = ORIENTED_EDGE ( 'NONE', *, *, #53610, .F. ) ;
#72379 = CARTESIAN_POINT ( 'NONE',  ( 28.40019573429999866, 1509.157491143330162, 209.8143715515469978 ) ) ;
#72380 = ORIENTED_EDGE ( 'NONE', *, *, #65887, .T. ) ;
#72381 = CARTESIAN_POINT ( 'NONE',  ( 0.9962946536900849637, 1485.568703864239978, 220.9525874579420019 ) ) ;
#72382 = CARTESIAN_POINT ( 'NONE',  ( -109.8255548870000098, 1384.923179268330159, 311.3807808352589745 ) ) ;
#72384 = CARTESIAN_POINT ( 'NONE',  ( 0.4857469785310000177, 1507.117126404930104, 180.9629171623980142 ) ) ;
#72383 = CARTESIAN_POINT ( 'NONE',  ( -15.73408764137255034, 1409.498451079286042, 225.6596250670369272 ) ) ;
#72385 = CARTESIAN_POINT ( 'NONE',  ( 5.013429356055000063, 1517.123342927159911, 210.2437967141769946 ) ) ;
#72386 = CARTESIAN_POINT ( 'NONE',  ( -24.71204467725759812, 1451.893171190130033, 136.8663216757400107 ) ) ;
#72387 = DIRECTION ( 'NONE',  ( 1.000000000000000000, 0.000000000000000000, 0.000000000000000000 ) ) ;
#72388 = CARTESIAN_POINT ( 'NONE',  ( 8.918237991669998976, 1409.224492122430092, 229.1880316136980014 ) ) ;
#72389 = CARTESIAN_POINT ( 'NONE',  ( 7.628187097038660269, 1483.025225563630102, 218.3251324470150223 ) ) ;
#72390 = SHAPE_DEFINITION_REPRESENTATION ( #88434, #14372 ) ;
#72391 = PRODUCT_DEFINITION_SHAPE ( 'NONE', 'NONE',  #82922 ) ;
#72392 = CARTESIAN_POINT ( 'NONE',  ( 40.80783872799189993, 1447.308166564819885, 134.0999999984899773 ) ) ;
#72393 = CARTESIAN_POINT ( 'NONE',  ( 4.554071316310000839, 1435.609063005990038, 205.7950640489989951 ) ) ;
#72394 = CARTESIAN_POINT ( 'NONE',  ( 11.21032122953132770, 1519.551704408389924, 188.3716648695481695 ) ) ;
#72395 = CARTESIAN_POINT ( 'NONE',  ( -11.15738487964140013, 1390.939238811560017, 203.8452351040699853 ) ) ;
#72396 = ORIENTED_EDGE ( 'NONE', *, *, #7783, .F. ) ;
#72397 = ORIENTED_EDGE ( 'NONE', *, *, #95886, .T. ) ;
#72398 = VERTEX_POINT ( 'NONE', #80373 ) ;
#72399 = CARTESIAN_POINT ( 'NONE',  ( 9.965445173606990892, 1410.635768303481655, 229.8293632461459879 ) ) ;
#72400 = CARTESIAN_POINT ( 'NONE',  ( 16.35769667426164986, 1514.438069564495208, 194.4905545724909075 ) ) ;
#72401 = CARTESIAN_POINT ( 'NONE',  ( -5.623474965688048840E-07, 1451.660737107639989, 154.0815186765750013 ) ) ;
#72402 = CARTESIAN_POINT ( 'NONE',  ( -8.298029079490001791, 1384.907497196539907, 218.7036230386890168 ) ) ;
#72403 = CARTESIAN_POINT ( 'NONE',  ( -18.55485652327908142, 1445.548742844001254, 214.3589705322614805 ) ) ;
#72404 = CARTESIAN_POINT ( 'NONE',  ( -68.56305339912407248, 1379.747553719651478, 279.6255597516078524 ) ) ;
#72405 = DIRECTION ( 'NONE',  ( 0.7616194158028416483, 1.190401854521374756E-16, 0.6480245870892076265 ) ) ;
#72406 = CIRCLE ( 'NONE', #47366, 1.999999999999915623 ) ;
#72407 = CARTESIAN_POINT ( 'NONE',  ( -9828.720208194639781, 54.28084076250829781, -1083.674256066600037 ) ) ;
#72408 = CARTESIAN_POINT ( 'NONE',  ( 3.923553339340000168, 1416.217772597929979, 190.9999006073979899 ) ) ;
#72410 = CIRCLE ( 'NONE', #24075, 5.301724629749982043 ) ;
#72409 = CARTESIAN_POINT ( 'NONE',  ( -58.01177053069230283, 1384.661045340669943, 239.8217497119959773 ) ) ;
#72411 = ORIENTED_EDGE ( 'NONE', *, *, #86512, .T. ) ;
#72412 = CARTESIAN_POINT ( 'NONE',  ( -6.563595907815000352, 1517.154223579619838, 206.8322214998769937 ) ) ;
#72413 = EDGE_LOOP ( 'NONE', ( #92919, #79318, #18615, #22306 ) ) ;
#72414 = CARTESIAN_POINT ( 'NONE',  ( 28.19745448794409981, 1440.913060387330006, 248.0707952811780217 ) ) ;
#72415 = CARTESIAN_POINT ( 'NONE',  ( -18.88961621640000033, 1507.836736047129989, 187.8591162544979909 ) ) ;
#72416 = ORIENTED_EDGE ( 'NONE', *, *, #53835, .F. ) ;
#72417 = CARTESIAN_POINT ( 'NONE',  ( -17.43549085681739541, 1525.211473355384896, 181.0323682579330580 ) ) ;
#72418 = CARTESIAN_POINT ( 'NONE',  ( -3.034707026709789979, 1440.440247136690004, 157.2489849372729793 ) ) ;
#72419 = CARTESIAN_POINT ( 'NONE',  ( -18.14127185173783019, 1508.457047458428633, 211.6720055858629337 ) ) ;
#72420 = CARTESIAN_POINT ( 'NONE',  ( -24.49648242109999785, 1440.984241468170012, 210.9954442990479890 ) ) ;
#72421 = CARTESIAN_POINT ( 'NONE',  ( -6.806372913706649541, 1435.357145811779901, 216.0422613199140187 ) ) ;
#72422 = CARTESIAN_POINT ( 'NONE',  ( 13.74454213900000177, 1436.216140752829915, 150.3798544741980265 ) ) ;
#72423 = CARTESIAN_POINT ( 'NONE',  ( 39.21111056970000419, 1422.625647128129913, 266.3742241808980111 ) ) ;
#72424 = DIRECTION ( 'NONE',  ( -0.6736849260863839728, 0.000000000000000000, 0.7390186874254150995 ) ) ;
#72425 = CARTESIAN_POINT ( 'NONE',  ( 25.82427654007650020, 1484.679466883040050, 206.2250770722999960 ) ) ;
#72427 = CARTESIAN_POINT ( 'NONE',  ( -11.60004869885203682, 1423.462184080716270, 135.7647354703441351 ) ) ;
#72426 = CARTESIAN_POINT ( 'NONE',  ( 7.744760412899999835, 1463.664893275730037, 234.4935621930980005 ) ) ;
#72428 = B_SPLINE_SURFACE_WITH_KNOTS ( 'NONE', 4, 5, ( 
 ( #38572, #97384, #11734, #62163, #97926, #55951 ),
 ( #20655, #30169, #45903, #90073, #53772, #108543 ),
 ( #48097, #5538, #82237, #13912, #109652, #48662 ),
 ( #82788, #101218, #100142, #15558, #58158, #73857 ),
 ( #22299, #65465, #32394, #6082, #57064, #39117 ),
 ( #73297, #15011, #41351, #40234, #107984, #13355 ),
 ( #56501, #74964, #99572, #90630, #39689, #91189 ),
 ( #47547, #57621, #22858, #49759, #81667, #6633 ),
 ( #23428, #32928, #83888, #14470, #74417, #31281 ) ),
 .UNSPECIFIED., .F., .F., .F.,
 ( 5, 4, 5 ),
 ( 6, 6 ),
 ( 36.89059838979999739, 37.78706028239999881, 37.79602490132599968 ),
 ( 0.000000000000000000, 2.000000000000000000 ),
 .UNSPECIFIED. ) ;
#72429 = CARTESIAN_POINT ( 'NONE',  ( 0.01126491619350150110, 1516.939530130779985, 216.0663127125970107 ) ) ;
#72430 = LINE ( 'NONE', #55084, #87374 ) ;
#72431 = CARTESIAN_POINT ( 'NONE',  ( -0.1594943249209899994, 1507.184524987769919, 180.8985575764880025 ) ) ;
#72432 = EDGE_CURVE ( 'NONE', #75633, #22619, #30430, .T. ) ;
#72433 = CARTESIAN_POINT ( 'NONE',  ( 16.81138730642775769, 1449.242716094900288, 218.8724950056246712 ) ) ;
#72434 = CARTESIAN_POINT ( 'NONE',  ( -3.253462098795000035, 1516.874084700499907, 212.5832060635069922 ) ) ;
#72435 = CARTESIAN_POINT ( 'NONE',  ( -22.03740498310000007, 1506.809279317530127, 209.2115705851809935 ) ) ;
#72436 = DIRECTION ( 'NONE',  ( 0.9455185755993167351, 0.000000000000000000, -0.3255681544571568109 ) ) ;
#72438 = ORIENTED_EDGE ( 'NONE', *, *, #83607, .F. ) ;
#72437 = CARTESIAN_POINT ( 'NONE',  ( -12.94448954231350868, 1519.913060387329779, 185.4271167906579478 ) ) ;
#72439 = CARTESIAN_POINT ( 'NONE',  ( -8.604462330509999646, 1384.894731729009891, 199.8686916664790090 ) ) ;
#72440 = CARTESIAN_POINT ( 'NONE',  ( 3.814136268639999994, 1460.517119005329960, 217.3476460196580149 ) ) ;
#72441 = ADVANCED_FACE ( 'NONE', ( #13677 ), #97409, .T. ) ;
#72442 = CARTESIAN_POINT ( 'NONE',  ( -4.238023215140263034, 1486.921097696548031, 220.3845390032697367 ) ) ;
#72443 = CARTESIAN_POINT ( 'NONE',  ( -14.68843015960000109, 1416.151303865629870, 204.4183550279689712 ) ) ;
#72444 = CARTESIAN_POINT ( 'NONE',  ( 2.923531254659999856, 1410.372839466330106, 231.6299449191980102 ) ) ;
#72445 = CARTESIAN_POINT ( 'NONE',  ( 11.78588353789999843, 1420.143588805510035, 199.1665921514089916 ) ) ;
#72446 = AXIS2_PLACEMENT_3D ( 'NONE', #90680, #73347, #89582 ) ;
#72447 = CARTESIAN_POINT ( 'NONE',  ( 11.75111247159999905, 1446.815402699049855, 187.7955951978979954 ) ) ;
#72449 = CARTESIAN_POINT ( 'NONE',  ( 19.74393297489999810, 1455.407987973630043, 226.2017192373979810 ) ) ;
#72448 = CARTESIAN_POINT ( 'NONE',  ( -19.47133434590000078, 1457.447441929329898, 226.1258623160980221 ) ) ;
#72450 = CARTESIAN_POINT ( 'NONE',  ( -2.897715842900000283, 1486.012679015429967, 182.1056253353979741 ) ) ;
#72451 = EDGE_LOOP ( 'NONE', ( #54220, #64777, #42768 ) ) ;
#72452 = CARTESIAN_POINT ( 'NONE',  ( -4.621897862544999569, 1516.858533673840157, 204.5099662467769974 ) ) ;
#72453 = CARTESIAN_POINT ( 'NONE',  ( 2.778298004749999883, 1405.778071318030015, 267.8507722644980049 ) ) ;
#72454 = CIRCLE ( 'NONE', #86732, 2.000015581134258369 ) ;
#72455 = CARTESIAN_POINT ( 'NONE',  ( 1.842963900900000063, 1515.551704191689851, 212.9514661349190021 ) ) ;
#72456 = CARTESIAN_POINT ( 'NONE',  ( 6.422733791020810656, 1471.791680861769919, 269.8654503459380294 ) ) ;
#72457 = CARTESIAN_POINT ( 'NONE',  ( 1.150023946295242183, 1463.916996383109336, 199.3782771554538442 ) ) ;
#72458 = CARTESIAN_POINT ( 'NONE',  ( 13.72029690906714805, 1499.818747152161222, 226.3681697707128251 ) ) ;
#72459 = FACE_OUTER_BOUND ( 'NONE', #78440, .T. ) ;
#72460 = PLANE ( 'NONE',  #84192 ) ;
#72461 = CARTESIAN_POINT ( 'NONE',  ( -7.604289863101939773, 1426.735970264149955, 206.0920986175900111 ) ) ;
#72462 = CARTESIAN_POINT ( 'NONE',  ( 0.5699886612280750109, 1450.893155944679847, 155.0620510323830104 ) ) ;
#72463 = CARTESIAN_POINT ( 'NONE',  ( -14.22819488934809939, 1415.834070662929889, 221.1563499966289896 ) ) ;
#72464 = CARTESIAN_POINT ( 'NONE',  ( -4.138543415650000057, 1515.492058123790002, 210.9648098330690118 ) ) ;
#72465 = ORIENTED_EDGE ( 'NONE', *, *, #54269, .F. ) ;
#72466 = CARTESIAN_POINT ( 'NONE',  ( -20.41675352909999930, 1440.913060387330006, 219.6133834379979817 ) ) ;
#72467 = CARTESIAN_POINT ( 'NONE',  ( 2.704956093210000301, 1440.760885240010111, 170.5389561584980243 ) ) ;
#72468 = CARTESIAN_POINT ( 'NONE',  ( -0.5566428566430000613, 1475.834717975330022, 266.9610393015980208 ) ) ;
#72469 = CARTESIAN_POINT ( 'NONE',  ( -29.80701629120000007, 1451.872188912029969, 134.8363203424979986 ) ) ;
#72470 = CARTESIAN_POINT ( 'NONE',  ( -9.814778378175621043, 1424.216271979959856, 144.1582897904220033 ) ) ;
#72471 = CARTESIAN_POINT ( 'NONE',  ( -3.558031533707346927, 1448.289799212619300, 184.9044431245979183 ) ) ;
#72472 = CARTESIAN_POINT ( 'NONE',  ( -30.22200536124639925, 1384.827631819069893, 228.2875610643100117 ) ) ;
#72473 = CARTESIAN_POINT ( 'NONE',  ( -105.7666966480000070, 1378.955190987910100, 302.3809606587589656 ) ) ;
#72474 = CARTESIAN_POINT ( 'NONE',  ( 31.87600794503219603, 1525.042337199240137, 216.1377579384306671 ) ) ;
#72475 = CARTESIAN_POINT ( 'NONE',  ( 8.394745799167832701, 1511.398924905634203, 204.5081796389210638 ) ) ;
#72476 = AXIS2_PLACEMENT_3D ( 'NONE', #6827, #119, #49954 ) ;
#72477 = CARTESIAN_POINT ( 'NONE',  ( -10.66105778724350017, 1396.285352728870066, 212.1046978785340116 ) ) ;
#72478 = CARTESIAN_POINT ( 'NONE',  ( -2.487934962309999776, 1508.551704408389924, 204.1347675205190058 ) ) ;
#72479 = CARTESIAN_POINT ( 'NONE',  ( -44.92200289279999481, 1440.533167347589824, 269.6914162027979955 ) ) ;
#72480 = ORIENTED_EDGE ( 'NONE', *, *, #80775, .F. ) ;
#72481 = CARTESIAN_POINT ( 'NONE',  ( -11.33349574978999819, 1502.222612973462901, 207.2846957396286598 ) ) ;
#72482 = CARTESIAN_POINT ( 'NONE',  ( -13.58135394501369930, 1508.550209656430070, 210.2785163480139943 ) ) ;
#72483 = VECTOR ( 'NONE', #84618, 1000.000000000000114 ) ;
#72484 = CARTESIAN_POINT ( 'NONE',  ( -6.509625120830000000, 1510.892449458290002, 215.5197494809989962 ) ) ;
#72486 = CARTESIAN_POINT ( 'NONE',  ( -14.32514194706499921, 1513.248517198770060, 192.8985536356669854 ) ) ;
#72485 = CARTESIAN_POINT ( 'NONE',  ( 11.34308291480000008, 1426.877116246929972, 115.7237209403979961 ) ) ;
#72487 = LINE ( 'NONE', #37775, #51978 ) ;
#72488 = CARTESIAN_POINT ( 'NONE',  ( -9.066559479250001274, 1450.410201457089897, 206.4479026976190141 ) ) ;
#72489 = CARTESIAN_POINT ( 'NONE',  ( 4.035536225084999984, 1517.086065052259983, 201.3983658527070020 ) ) ;
#72490 = CARTESIAN_POINT ( 'NONE',  ( 7.958039864590000789, 1426.668732447519915, 211.8424160901890048 ) ) ;
#72491 = CARTESIAN_POINT ( 'NONE',  ( -11.84242369139999873, 1431.324257919750153, 147.6543138610979895 ) ) ;
#72492 = CARTESIAN_POINT ( 'NONE',  ( 2.491448480239999874, 1508.759613064230052, 180.3874124875980272 ) ) ;
#72493 = CARTESIAN_POINT ( 'NONE',  ( 7.683494238625000250, 1512.058324472099912, 206.4100757371070074 ) ) ;
#72494 = CARTESIAN_POINT ( 'NONE',  ( -94.35249819378030622, 1379.531630662760108, 302.8770685251070631 ) ) ;
#72495 = CARTESIAN_POINT ( 'NONE',  ( 7.162147128334975577, 1365.790004795873074, 209.6218459617148824 ) ) ;
#72497 = ORIENTED_EDGE ( 'NONE', *, *, #55500, .F. ) ;
#72496 = CARTESIAN_POINT ( 'NONE',  ( 8.572313988419999475, 1452.460948930489849, 212.8151060300189954 ) ) ;
#72498 = VERTEX_POINT ( 'NONE', #12610 ) ;
#72499 = FACE_OUTER_BOUND ( 'NONE', #38433, .T. ) ;
#72500 = CARTESIAN_POINT ( 'NONE',  ( 2.892830563952609957, 1409.416455242979964, 231.1906418284260099 ) ) ;
#72501 = CARTESIAN_POINT ( 'NONE',  ( -3.454119954913678292, 1516.594591940487589, 201.4112355775968126 ) ) ;
#72502 = CARTESIAN_POINT ( 'NONE',  ( -9.251110758310000293, 1409.236116293629948, 189.6234339899980057 ) ) ;
#72503 = DIRECTION ( 'NONE',  ( 0.9272802558616994872, -0.03238135539626126047, 0.3729648440694676714 ) ) ;
#72504 = CARTESIAN_POINT ( 'NONE',  ( -7.549016801754999229, 1510.423579818969984, 213.5498276941069946 ) ) ;
#72506 = CARTESIAN_POINT ( 'NONE',  ( 17.38002308720000144, 1413.529868483829887, 226.0648461332980332 ) ) ;
#72505 = CARTESIAN_POINT ( 'NONE',  ( -8.445660594239999597, 1383.900183497409898, 218.5659211283389993 ) ) ;
#72507 = CARTESIAN_POINT ( 'NONE',  ( 1.721725048689999760, 1429.772963309329953, 184.5251936066979965 ) ) ;
#72508 = CARTESIAN_POINT ( 'NONE',  ( -38.13298815378909978, 1448.843107352490051, 136.3720512951870205 ) ) ;
#72509 = B_SPLINE_CURVE_WITH_KNOTS ( 'NONE', 5,
 ( #39328, #100861, #83519, #21938, #82981, #82439, #24151, #58341, #23620, #84076, #56132, #31467 ),
 .UNSPECIFIED., .F., .F.,
 ( 6, 3, 3, 6 ),
 ( 0.000000000000000000, 0.3812068090311336310, 0.7624136180702053567, 1.000000000000000000 ),
 .UNSPECIFIED. ) ;
#72510 = CARTESIAN_POINT ( 'NONE',  ( 40.69210606679339293, 1440.912522207950133, 136.6173652597990156 ) ) ;
#72511 = CARTESIAN_POINT ( 'NONE',  ( 27.05712719250106701, 1435.442241411316218, 135.2793719061239130 ) ) ;
#72512 = CARTESIAN_POINT ( 'NONE',  ( 33.93536013789529449, 1436.159636157269915, 136.2998715483510068 ) ) ;
#72513 = CARTESIAN_POINT ( 'NONE',  ( 10.94632149490000117, 1430.668062723530056, 151.5807326048979746 ) ) ;
#72514 = CARTESIAN_POINT ( 'NONE',  ( 41.65668456659999919, 1444.003990099839712, 136.1262293497980238 ) ) ;
#72515 = ORIENTED_EDGE ( 'NONE', *, *, #95034, .F. ) ;
#72516 = LINE ( 'NONE', #46777, #82230 ) ;
#72517 = CARTESIAN_POINT ( 'NONE',  ( 20.53760542139780298, 1525.821544997590536, 233.5223198772804665 ) ) ;
#72518 = ORIENTED_EDGE ( 'NONE', *, *, #20517, .T. ) ;
#72519 = EDGE_LOOP ( 'NONE', ( #56664, #20 ) ) ;
#72520 = CARTESIAN_POINT ( 'NONE',  ( -14.74939910209999994, 1460.058428731729919, 231.1927315459980150 ) ) ;
#72521 = FACE_OUTER_BOUND ( 'NONE', #58192, .T. ) ;
#72522 = CARTESIAN_POINT ( 'NONE',  ( 30.29630067237317803, 1526.329757971585195, 196.4535985240150637 ) ) ;
#72523 = CARTESIAN_POINT ( 'NONE',  ( 0.01244693565920149993, 1516.939646076049939, 214.9034317483770167 ) ) ;
#72524 = CARTESIAN_POINT ( 'NONE',  ( -12.31497494632570167, 1378.366662294749858, 209.7019801924109856 ) ) ;
#72525 = ORIENTED_EDGE ( 'NONE', *, *, #42564, .T. ) ;
#72526 = CARTESIAN_POINT ( 'NONE',  ( -18.72256362461450152, 1508.551704408389924, 209.8107881426000176 ) ) ;
#72527 = CARTESIAN_POINT ( 'NONE',  ( 2.500000000000000000, 1448.763411304559895, 157.1038816470399979 ) ) ;
#72528 = CARTESIAN_POINT ( 'NONE',  ( -29.63091391959999754, 1375.535769174380221, 213.7170380704389743 ) ) ;
#72529 = CIRCLE ( 'NONE', #8078, 4.250000000000000000 ) ;
#72530 = CARTESIAN_POINT ( 'NONE',  ( 0.2210648319480000012, 1414.913060387329779, 225.4904991280980084 ) ) ;
#72531 = CARTESIAN_POINT ( 'NONE',  ( -5.784638357945000031, 1516.939574742129935, 204.5080835752170003 ) ) ;
#72532 = EDGE_LOOP ( 'NONE', ( #67991, #68197, #67563, #31821, #37393 ) ) ;
#72533 = CARTESIAN_POINT ( 'NONE',  ( -12.20950249781779995, 1490.126853475539974, 210.0346353896779874 ) ) ;
#72534 = B_SPLINE_SURFACE_WITH_KNOTS ( 'NONE', 5, 1, ( 
 ( #99502, #16579 ),
 ( #82165, #23357 ),
 ( #15493, #84375 ),
 ( #31214, #83820 ),
 ( #22785, #40168 ),
 ( #74351, #49140 ) ),
 .UNSPECIFIED., .F., .F., .F.,
 ( 6, 6 ),
 ( 2, 2 ),
 ( 0.000000000000000000, 52.98959944900320096 ),
 ( -1.500000000000000000, 1.500000000000000000 ),
 .UNSPECIFIED. ) ;
#72535 = CARTESIAN_POINT ( 'NONE',  ( -30.18855271174454558, 1419.717913747435205, 269.4728395028291743 ) ) ;
#72536 = CARTESIAN_POINT ( 'NONE',  ( -5.505226529499999799, 1409.105307133929955, 230.1454130303979753 ) ) ;
#72538 = ORIENTED_EDGE ( 'NONE', *, *, #72632, .F. ) ;
#72537 = DIRECTION ( 'NONE',  ( 0.000000000000000000, 0.000000000000000000, -1.000000000000000000 ) ) ;
#72539 = CARTESIAN_POINT ( 'NONE',  ( -3.677613769069999778E-16, 1378.399971913189802, 209.1218459616989946 ) ) ;
#72540 = CARTESIAN_POINT ( 'NONE',  ( -31.87892841237279740, 1440.913060389169914, 243.7976297880429684 ) ) ;
#72541 = CARTESIAN_POINT ( 'NONE',  ( 20.28287979410820085, 1497.593060318700054, 226.9821815841060300 ) ) ;
#72542 = CARTESIAN_POINT ( 'NONE',  ( 10.95098205620359977, 1471.837422849929908, 212.3987392730099657 ) ) ;
#72543 = CARTESIAN_POINT ( 'NONE',  ( 20.37632423397029768, 1412.699084889349933, 270.3601818045660252 ) ) ;
#72544 = CARTESIAN_POINT ( 'NONE',  ( 2.492130623175000448, 1516.778761582560037, 212.5675310476169955 ) ) ;
#72545 = CARTESIAN_POINT ( 'NONE',  ( -68.16069380650000653, 1379.746470013149974, 278.7868268744589955 ) ) ;
#72546 = CARTESIAN_POINT ( 'NONE',  ( 23.72051015330000112, 1411.111939740129856, 207.9527775095279765 ) ) ;
#72547 = CARTESIAN_POINT ( 'NONE',  ( 0.01365740389280096709, 1507.932904300896780, 237.5666955293443436 ) ) ;
#72548 = CARTESIAN_POINT ( 'NONE',  ( 5.440512190109999757, 1424.738065781850082, 191.9794586101990319 ) ) ;
#72550 = CARTESIAN_POINT ( 'NONE',  ( -7.709003326667110301, 1516.533218713809902, 211.0246589237959824 ) ) ;
#72549 = AXIS2_PLACEMENT_3D ( 'NONE', #102172, #84813, #34976 ) ;
#72551 = CARTESIAN_POINT ( 'NONE',  ( 3.455495833855000143, 1516.939877939420057, 209.1085718841020196 ) ) ;
#72552 = CARTESIAN_POINT ( 'NONE',  ( 4.176954718270289746, 1421.290050260260159, 185.1746166876249902 ) ) ;
#72553 = CARTESIAN_POINT ( 'NONE',  ( -3.077130052889999856, 1417.912031963829804, 232.8375555567980086 ) ) ;
#72554 = CARTESIAN_POINT ( 'NONE',  ( -113.4000000000000057, 1384.913060387289988, 311.2218459572590064 ) ) ;
#72555 = ORIENTED_EDGE ( 'NONE', *, *, #72168, .F. ) ;
#72556 = CARTESIAN_POINT ( 'NONE',  ( -29.95569946650590154, 1385.233789043189745, 227.9819273993630020 ) ) ;
#72557 = FACE_OUTER_BOUND ( 'NONE', #65780, .T. ) ;
#72558 = EDGE_CURVE ( 'NONE', #36324, #2313, #107099, .T. ) ;
#72559 = CARTESIAN_POINT ( 'NONE',  ( -0.009082284558410000028, 1417.355061569330019, 235.2087945027979856 ) ) ;
#72560 = CIRCLE ( 'NONE', #4620, 2.000000000000000000 ) ;
#72561 = B_SPLINE_CURVE_WITH_KNOTS ( 'NONE', 3,
 ( #99640, #64977, #89604, #29158, #54928, #106416 ),
 .UNSPECIFIED., .F., .F.,
 ( 4, 2, 4 ),
 ( 0.000000000000000000, 0.5000000000000000000, 1.000000000000000000 ),
 .UNSPECIFIED. ) ;
#72562 = CARTESIAN_POINT ( 'NONE',  ( 11.52804851922353890, 1414.677402202029953, 211.3132271615170623 ) ) ;
#72563 = CARTESIAN_POINT ( 'NONE',  ( -19.39983987835443457, 1522.382868172863937, 178.9515629539737631 ) ) ;
#72564 = CARTESIAN_POINT ( 'NONE',  ( 11.34922769319999958, 1426.257359350699971, 206.1386472418390099 ) ) ;
#72565 = CARTESIAN_POINT ( 'NONE',  ( -2.240533496870801944, 1497.807162272345067, 198.0577364717022419 ) ) ;
#72567 = CARTESIAN_POINT ( 'NONE',  ( -16.18244964864798163, 1416.494914503025257, 208.5996723762598037 ) ) ;
#72566 = CARTESIAN_POINT ( 'NONE',  ( 1.130002494264999990, 1516.621991115350056, 216.0576472317669925 ) ) ;
#72568 = CARTESIAN_POINT ( 'NONE',  ( 9.529616025180215999, 1459.343410991622932, 203.7689766306496040 ) ) ;
#72569 = CARTESIAN_POINT ( 'NONE',  ( 11.41166285218010046, 1470.995102172900033, 209.2012249493139961 ) ) ;
#72570 = ORIENTED_EDGE ( 'NONE', *, *, #2794, .F. ) ;
#72571 = CARTESIAN_POINT ( 'NONE',  ( -7.718134667564999774, 1516.881930554049859, 201.7919159189069944 ) ) ;
#72572 = CARTESIAN_POINT ( 'NONE',  ( -16.23061969806499860, 1512.609537213029853, 220.4047961632670081 ) ) ;
#72573 = ORIENTED_EDGE ( 'NONE', *, *, #15031, .T. ) ;
#72574 = DIRECTION ( 'NONE',  ( -1.224646799147353207E-16, -1.836970198721029688E-16, -1.000000000000000000 ) ) ;
#72575 = B_SPLINE_CURVE_WITH_KNOTS ( 'NONE', 5,
 ( #100681, #107433, #6083, #73858, #22859, #22300 ),
 .UNSPECIFIED., .F., .F.,
 ( 6, 6 ),
 ( 0.000000000000000000, 1.000000000000000000 ),
 .UNSPECIFIED. ) ;
#72576 = DIRECTION ( 'NONE',  ( -0.9455185755993178454, 0.000000000000000000, 0.3255681544571537578 ) ) ;
#72577 = CARTESIAN_POINT ( 'NONE',  ( 9.651063919191019025, 1425.440657924460083, 195.4941620015079877 ) ) ;
#72578 = CARTESIAN_POINT ( 'NONE',  ( 1.042629999269999885, 1442.250188905790083, 219.0243665098589929 ) ) ;
#72579 = CARTESIAN_POINT ( 'NONE',  ( -27.00783404025900225, 1509.422393139779842, 201.2804958749899811 ) ) ;
#72580 = CARTESIAN_POINT ( 'NONE',  ( -2.500000000000000000, 1448.229591734839914, 165.9681906964980271 ) ) ;
#72581 = CARTESIAN_POINT ( 'NONE',  ( -19.91120744939999909, 1427.184642357730127, 223.3904735300980064 ) ) ;
#72582 = CARTESIAN_POINT ( 'NONE',  ( 9.947665014826124974, 1488.618077319816621, 204.6704152026359793 ) ) ;
#72583 = CARTESIAN_POINT ( 'NONE',  ( -104.4930758389999994, 1390.118383696849833, 304.1821339162590334 ) ) ;
#72584 = CARTESIAN_POINT ( 'NONE',  ( 18.78950644500000067, 1478.520229345230064, 189.7031885923980212 ) ) ;
#72586 = CARTESIAN_POINT ( 'NONE',  ( 29.77420891850000118, 1509.998730826829842, 209.4122126407480096 ) ) ;
#72585 = CARTESIAN_POINT ( 'NONE',  ( 0.08580183426129689428, 1408.916056653429905, 231.7748806593529878 ) ) ;
#72587 = CARTESIAN_POINT ( 'NONE',  ( 2.372478608334043670, 1522.644714754858114, 243.3440112565160973 ) ) ;
#72588 = ORIENTED_EDGE ( 'NONE', *, *, #52115, .T. ) ;
#72589 = CARTESIAN_POINT ( 'NONE',  ( -9.549500093889998098, 1508.435385506690182, 218.9685490284190053 ) ) ;
#72590 = DIRECTION ( 'NONE',  ( -9.152776640618289361E-47, 1.000000000000000000, -1.836970198721029688E-16 ) ) ;
#72591 = EDGE_CURVE ( 'NONE', #42283, #94550, #7510, .T. ) ;
#72592 = CARTESIAN_POINT ( 'NONE',  ( 10.62769165429999951, 1422.391598617170075, 210.1052261204159777 ) ) ;
#72593 = CARTESIAN_POINT ( 'NONE',  ( -2.936010229900000379, 1484.512606866390115, 198.6791449311989766 ) ) ;
#72594 = CARTESIAN_POINT ( 'NONE',  ( -18.49117141179999990, 1508.844092022629866, 229.9893364338979893 ) ) ;
#72595 = CARTESIAN_POINT ( 'NONE',  ( -3.302346719094112260, 1524.524650307243519, 241.8695341946817337 ) ) ;
#72596 = CARTESIAN_POINT ( 'NONE',  ( -13.29514579968463295, 1443.228841607992308, 186.9064473022689867 ) ) ;
#72597 = CARTESIAN_POINT ( 'NONE',  ( -17.39559655639999747, 1414.988015881329829, 207.6227086602179952 ) ) ;
#72598 = CARTESIAN_POINT ( 'NONE',  ( 4.028444003397729567, 1493.864063547320029, 219.5261911965480124 ) ) ;
#72599 = CARTESIAN_POINT ( 'NONE',  ( -4.705750868621540128, 1479.984690096089935, 230.9466464819849989 ) ) ;
#72600 = AXIS2_PLACEMENT_3D ( 'NONE', #72013, #27218, #36720 ) ;
#72601 = CARTESIAN_POINT ( 'NONE',  ( -15.44962914106915441, 1415.677402202029953, 209.5155034275957746 ) ) ;
#72602 = DIRECTION ( 'NONE',  ( -9.138167445698339565E-47, 1.000000000000000000, -1.836970198721029688E-16 ) ) ;
#72603 = CARTESIAN_POINT ( 'NONE',  ( 5.311406560260000020, 1429.286496272289924, 216.0669640761489916 ) ) ;
#72605 = ORIENTED_EDGE ( 'NONE', *, *, #55698, .T. ) ;
#72604 = CARTESIAN_POINT ( 'NONE',  ( 4.900006679340000559, 1499.255191946190052, 229.7873568473989963 ) ) ;
#72606 = CARTESIAN_POINT ( 'NONE',  ( 32.30068554584606488, 1526.382868172863937, 198.0073124585814242 ) ) ;
#72607 = CARTESIAN_POINT ( 'NONE',  ( 13.31081193891139947, 1512.571279492530039, 224.4121312145439902 ) ) ;
#72608 = ORIENTED_EDGE ( 'NONE', *, *, #76582, .T. ) ;
#72609 = ORIENTED_EDGE ( 'NONE', *, *, #93847, .T. ) ;
#72610 = CYLINDRICAL_SURFACE ( 'NONE', #65001, 2.000000000000000888 ) ;
#72611 = CARTESIAN_POINT ( 'NONE',  ( -109.5347599920000050, 1384.912562451920166, 297.1230869496590117 ) ) ;
#72612 = CARTESIAN_POINT ( 'NONE',  ( -8.431440857724776805, 1382.698224402347705, 199.9722048618648955 ) ) ;
#72614 = CARTESIAN_POINT ( 'NONE',  ( -22.71362857400000124, 1462.471423925029967, 250.3594883113980245 ) ) ;
#72613 = CARTESIAN_POINT ( 'NONE',  ( 34.22334808525543082, 1423.233184880918998, 269.5210271296780888 ) ) ;
#72615 = CARTESIAN_POINT ( 'NONE',  ( -20.08751159799999897, 1491.264926706829783, 190.5547343358980186 ) ) ;
#72616 = CARTESIAN_POINT ( 'NONE',  ( -11.20119892960000030, 1433.868452093230189, 151.6098175551980205 ) ) ;
#72617 = CARTESIAN_POINT ( 'NONE',  ( -7.082960536665612317, 1445.824516962028611, 183.6528070193931796 ) ) ;
#72618 = CARTESIAN_POINT ( 'NONE',  ( -19.69623350909999715, 1485.259879109029953, 190.3329780841980323 ) ) ;
#72619 = CARTESIAN_POINT ( 'NONE',  ( -14.31466601544043904, 1507.539053601158457, 232.2266900997976222 ) ) ;
#72620 = DIRECTION ( 'NONE',  ( 1.988619772330852129E-13, 0.03085824620771311644, -0.9995237709234254808 ) ) ;
#72621 = CARTESIAN_POINT ( 'NONE',  ( 0.1783569641990820354, 1515.156623775960043, 213.4488900611540032 ) ) ;
#72622 = CARTESIAN_POINT ( 'NONE',  ( 7.492226197380000841, 1440.568647855370045, 154.1013268154979983 ) ) ;
#72623 = CARTESIAN_POINT ( 'NONE',  ( 13.14097700228099974, 1428.660233805160033, 223.2339875276319958 ) ) ;
#72624 = CARTESIAN_POINT ( 'NONE',  ( 0.05823133897714560109, 1360.390585217530088, 210.6218459616987957 ) ) ;
#72625 = CARTESIAN_POINT ( 'NONE',  ( 32.36284091028937127, 1525.878013734321257, 199.2622049721660176 ) ) ;
#72626 = AXIS2_PLACEMENT_3D ( 'NONE', #55233, #3734, #28914 ) ;
#72628 = ORIENTED_EDGE ( 'NONE', *, *, #47971, .T. ) ;
#72627 = CARTESIAN_POINT ( 'NONE',  ( 3.013314585799149801E-09, 1410.335667381920075, 257.7916050914839730 ) ) ;
#72629 = ORIENTED_EDGE ( 'NONE', *, *, #50933, .F. ) ;
#72630 = FACE_OUTER_BOUND ( 'NONE', #51056, .T. ) ;
#72631 = EDGE_CURVE ( 'NONE', #30342, #86629, #94773, .T. ) ;
#72632 = EDGE_CURVE ( 'NONE', #89343, #73491, #51867, .T. ) ;
#72633 = CARTESIAN_POINT ( 'NONE',  ( 9.636843969170000079, 1494.191090576590113, 188.1746674836989826 ) ) ;
#72634 = CARTESIAN_POINT ( 'NONE',  ( -20.94370973279999859, 1470.568016209030020, 270.0430967339979702 ) ) ;
#72635 = CARTESIAN_POINT ( 'NONE',  ( 7.439417113980000273, 1422.547532122410075, 195.6475770543989938 ) ) ;
#72636 =( BOUNDED_CURVE ( )  B_SPLINE_CURVE ( 3, ( #96510, #95955, #3579, #62385 ),
 .UNSPECIFIED., .F., .T. ) 
 B_SPLINE_CURVE_WITH_KNOTS ( ( 4, 4 ),
 ( 5.908974974280949866, 6.104714675071489793 ),
 .UNSPECIFIED. ) 
 CURVE ( )  GEOMETRIC_REPRESENTATION_ITEM ( )  RATIONAL_B_SPLINE_CURVE ( ( 1.000000000000000000, 0.9968097118645246058, 0.9968097118645246058, 1.000000000000000000 ) ) 
 REPRESENTATION_ITEM ( '' )  );
#72637 = DIRECTION ( 'NONE',  ( 0.9942586961433758086, 0.000000000000000000, 0.1070030146457303932 ) ) ;
#72638 = EDGE_CURVE ( 'NONE', #107075, #29531, #50625, .T. ) ;
#72639 = DIRECTION ( 'NONE',  ( 0.9786619618251657382, 0.000000000000000000, 0.2054769195713184449 ) ) ;
#72640 = B_SPLINE_CURVE_WITH_KNOTS ( 'NONE', 3,
 ( #83945, #33521, #25123, #100729, #58756, #24014, #58211, #67722, #49815, #7245, #92337, #15609, #41406, #101830, #93438, #24565, #32980, #75573, #101269, #16168, #84497, #11126, #104057, #69943, #86157, #78308, #43062, #96218, #19495, #26800, #25677, #36858, #17816, #53697, #77222, #2737, #102394, #8881, #78883, #45285, #44733, #60987, #87265, #44170, #95113, #36302 ),
 .UNSPECIFIED., .F., .F.,
 ( 4, 3, 3, 3, 3, 3, 3, 3, 3, 3, 3, 3, 3, 3, 3, 4 ),
 ( 0.000000000000000000, 0.8425732785457979990, 1.714272507910759913, 2.605598717659390218, 3.529198674031960081, 3.734573540650000023, 4.706518334241139634, 5.735038120595219446, 6.516940428549999886, 7.557162126475709840, 8.512610629112849381, 9.373333392597750446, 9.468059131749999580, 10.28051844247830005, 11.05372975085490062, 11.47905148820000143 ),
 .UNSPECIFIED. ) ;
#72642 = ADVANCED_FACE ( 'NONE', ( #6958 ), #3614, .T. ) ;
#72641 = CARTESIAN_POINT ( 'NONE',  ( 4.327495487223619541, 1515.139385973049912, 209.7044482359050050 ) ) ;
#72643 = LINE ( 'NONE', #3803, #87295 ) ;
#72644 = CARTESIAN_POINT ( 'NONE',  ( 0.5257072283710009231, 1456.163790123490116, 198.9387035231989955 ) ) ;
#72645 = FACE_OUTER_BOUND ( 'NONE', #15459, .T. ) ;
#72646 = CARTESIAN_POINT ( 'NONE',  ( 9.176918871551549728, 1361.548833878397545, 210.6218459617030021 ) ) ;
#72647 = CARTESIAN_POINT ( 'NONE',  ( -39.33011038453689423, 1423.172057499710036, 269.1477809332180300 ) ) ;
#72648 = ORIENTED_EDGE ( 'NONE', *, *, #41059, .T. ) ;
#72649 = CARTESIAN_POINT ( 'NONE',  ( -3.547294053305450223, 1505.009196866179991, 181.0671712231609831 ) ) ;
#72650 = VERTEX_POINT ( 'NONE', #84214 ) ;
#72651 = ORIENTED_EDGE ( 'NONE', *, *, #86358, .F. ) ;
#72652 = CARTESIAN_POINT ( 'NONE',  ( 0.01319650876840149957, 1516.941178807709775, 211.4140629809269853 ) ) ;
#72653 = CARTESIAN_POINT ( 'NONE',  ( -8.728534304065659555, 1447.922708812389828, 212.1734976818020186 ) ) ;
#72654 = CARTESIAN_POINT ( 'NONE',  ( -22.52594231189999974, 1509.699683626429987, 190.3521444180979927 ) ) ;
#72655 = CARTESIAN_POINT ( 'NONE',  ( -5.956347180529999896, 1440.426868644620072, 185.7687637636979900 ) ) ;
#72656 = CARTESIAN_POINT ( 'NONE',  ( -15.67479435197149940, 1461.186449370369928, 228.5358082348789992 ) ) ;
#72657 = ORIENTED_EDGE ( 'NONE', *, *, #49792, .F. ) ;
#72658 = CARTESIAN_POINT ( 'NONE',  ( -26.43469822969999683, 1435.724577353250197, 136.2325690242980158 ) ) ;
#72659 = EDGE_CURVE ( 'NONE', #37652, #68294, #82745, .T. ) ;
#72660 = CARTESIAN_POINT ( 'NONE',  ( 3.260357128764999946, 1517.133889586189980, 201.3971135232069969 ) ) ;
#72661 = DIRECTION ( 'NONE',  ( -0.8090169943749507819, -0.000000000000000000, -0.5877852522924685852 ) ) ;
#72662 = EDGE_CURVE ( 'NONE', #77151, #18150, #17851, .T. ) ;
#72663 = CARTESIAN_POINT ( 'NONE',  ( -16.77637052012299890, 1384.526196172110076, 200.9536932091479855 ) ) ;
#72664 = EDGE_LOOP ( 'NONE', ( #58834, #46080, #16061, #40074, #15174, #27691, #30066 ) ) ;
#72665 = CARTESIAN_POINT ( 'NONE',  ( -18.91874693594079915, 1412.285123103680007, 270.3614442910130151 ) ) ;
#72666 = CARTESIAN_POINT ( 'NONE',  ( -2.244413413239999766, 1428.081157166129969, 101.8807690336980016 ) ) ;
#72667 = CARTESIAN_POINT ( 'NONE',  ( 9.744580062524020647, 1435.065973224739992, 208.0102391462599769 ) ) ;
#72669 = ORIENTED_EDGE ( 'NONE', *, *, #6343, .T. ) ;
#72668 = CARTESIAN_POINT ( 'NONE',  ( -9.690020260125340457, 1366.026910387859971, 210.6218459616987957 ) ) ;
#72670 = ORIENTED_EDGE ( 'NONE', *, *, #62426, .T. ) ;
#72671 = EDGE_CURVE ( 'NONE', #16982, #35617, #30940, .T. ) ;
#72672 = CARTESIAN_POINT ( 'NONE',  ( 39.42853080850703407, 1458.278269001917351, 269.1443194363598082 ) ) ;
#72673 = CARTESIAN_POINT ( 'NONE',  ( 10.99606214793050007, 1471.801637878359998, 212.2474561802740141 ) ) ;
#72674 = CARTESIAN_POINT ( 'NONE',  ( -14.42367087132340053, 1436.254602620129845, 149.9796175991139933 ) ) ;
#72675 = CARTESIAN_POINT ( 'NONE',  ( -0.03669057782753510494, 1409.908510651789811, 185.0915849681089753 ) ) ;
#72676 = CARTESIAN_POINT ( 'NONE',  ( -4.028611259245000298, 1516.744381837270112, 210.2562039408269925 ) ) ;
#72677 = EDGE_CURVE ( 'NONE', #105138, #15491, #55466, .T. ) ;
#72678 = CARTESIAN_POINT ( 'NONE',  ( -18.72196294886500212, 1507.117986375961891, 221.9823435811830734 ) ) ;
#72679 = CARTESIAN_POINT ( 'NONE',  ( -33.28034951413921760, 1522.382868172863937, 217.4407153818824838 ) ) ;
#72680 =( GEOMETRIC_REPRESENTATION_CONTEXT ( 3 ) GLOBAL_UNCERTAINTY_ASSIGNED_CONTEXT ( ( #70393 ) ) GLOBAL_UNIT_ASSIGNED_CONTEXT ( ( #14654, #90254, #31452 ) ) REPRESENTATION_CONTEXT ( 'NONE', 'WORKASPACE' ) );
#72681 = CARTESIAN_POINT ( 'NONE',  ( -13.79590940549999978, 1416.844618645930041, 221.9094009210980118 ) ) ;
#72682 = CARTESIAN_POINT ( 'NONE',  ( 12.26151716610000086, 1416.568813549730066, 223.5713197806979906 ) ) ;
#72683 = CARTESIAN_POINT ( 'NONE',  ( 7.685457273825000435, 1511.037966505489976, 203.9826204811770083 ) ) ;
#72684 = ORIENTED_EDGE ( 'NONE', *, *, #97074, .T. ) ;
#72685 = CARTESIAN_POINT ( 'NONE',  ( 4.027051405805000428, 1516.733363207009916, 206.6306575737070261 ) ) ;
#72686 = ORIENTED_EDGE ( 'NONE', *, *, #89323, .F. ) ;
#72687 = CARTESIAN_POINT ( 'NONE',  ( -33.91369107984309750, 1435.681798568270096, 135.3761632788110205 ) ) ;
#72688 = CARTESIAN_POINT ( 'NONE',  ( -23.85399841774137286, 1446.449082436806748, 213.6949048731282801 ) ) ;
#72689 = ORIENTED_EDGE ( 'NONE', *, *, #6290, .T. ) ;
#72690 = CARTESIAN_POINT ( 'NONE',  ( 3.840665656060542776, 1457.471497273520299, 228.5188823049041957 ) ) ;
#72691 = CARTESIAN_POINT ( 'NONE',  ( -27.68516857330043734, 1508.595246550359661, 210.6013668309819593 ) ) ;
#72692 = CARTESIAN_POINT ( 'NONE',  ( 13.43950372030000118, 1415.041103191630100, 197.6576099831980002 ) ) ;
#72693 = CARTESIAN_POINT ( 'NONE',  ( -11.80614671260000037, 1416.487503907969767, 205.3428939757990008 ) ) ;
#72694 = CARTESIAN_POINT ( 'NONE',  ( 18.14423173670000367, 1409.546670921429950, 196.7317315907980060 ) ) ;
#72695 = CARTESIAN_POINT ( 'NONE',  ( -3.503071675944339880, 1446.464826362650228, 170.5350607194175154 ) ) ;
#72696 = CARTESIAN_POINT ( 'NONE',  ( -26.53940720459999980, 1435.424242704579910, 135.2833523932980029 ) ) ;
#72697 = CARTESIAN_POINT ( 'NONE',  ( 32.86470156657956920, 1523.580204110583963, 201.0415738463115360 ) ) ;
#72698 = CARTESIAN_POINT ( 'NONE',  ( 0.1909392970979732207, 1506.691119431691050, 186.9237900612206147 ) ) ;
#72699 = CARTESIAN_POINT ( 'NONE',  ( 4.250709873168109887, 1441.341571527049837, 160.9975569674199960 ) ) ;
#72700 = CARTESIAN_POINT ( 'NONE',  ( 2.500000000000349942, 1439.188131747740272, 158.6514102456989974 ) ) ;
#72701 = CARTESIAN_POINT ( 'NONE',  ( 2.488360629304999794, 1516.616791731099966, 214.8929950451170043 ) ) ;
#72702 = ORIENTED_EDGE ( 'NONE', *, *, #9660, .T. ) ;
#72703 = CARTESIAN_POINT ( 'NONE',  ( 7.709266964192710070, 1516.543288080860066, 207.3768922116219926 ) ) ;
#72704 = DIRECTION ( 'NONE',  ( -0.03173147633638096626, -0.9969860201949397593, 0.07079540200725449595 ) ) ;
#72705 = CARTESIAN_POINT ( 'NONE',  ( -15.74021840509336556, 1519.551704408389924, 221.9061614126840425 ) ) ;
#72706 = PRESENTATION_LAYER_ASSIGNMENT (  '', '', ( #44087 ) ) ;
#72707 = DIRECTION ( 'NONE',  ( -0.1070030146457249254, 0.000000000000000000, 0.9942586961433763637 ) ) ;
#72708 = EDGE_CURVE ( 'NONE', #63161, #67085, #45651, .T. ) ;
#72709 = CARTESIAN_POINT ( 'NONE',  ( -36.20521733875069970, 1449.935881827250114, 136.2514865721049659 ) ) ;
#72710 = CARTESIAN_POINT ( 'NONE',  ( 11.60004869885203682, 1425.182052903856402, 137.9775777671608523 ) ) ;
#72711 = CARTESIAN_POINT ( 'NONE',  ( -1.430539248151910137, 1444.328264662749916, 199.1703804428329931 ) ) ;
#72712 = CARTESIAN_POINT ( 'NONE',  ( -2.500000000000000000, 1424.573971167730178, 154.8453096575980226 ) ) ;
#72713 = CARTESIAN_POINT ( 'NONE',  ( -105.1761031979999927, 1379.258906148879987, 302.7941945437589766 ) ) ;
#72714 = CARTESIAN_POINT ( 'NONE',  ( -33.03302978810000212, 1464.710710526430148, 269.2927538329980166 ) ) ;
#72715 = CARTESIAN_POINT ( 'NONE',  ( 29.11563328215180135, 1440.913060387169935, 235.3779001622630176 ) ) ;
#72716 = CARTESIAN_POINT ( 'NONE',  ( -21.83283345040000256, 1508.011745662929798, 226.4479051240980141 ) ) ;
#72717 = AXIS2_PLACEMENT_3D ( 'NONE', #24421, #101124, #18640 ) ;
#72718 = CARTESIAN_POINT ( 'NONE',  ( 10.92768932611909882, 1501.618341437669869, 205.6861941585989939 ) ) ;
#72719 = ORIENTED_EDGE ( 'NONE', *, *, #102706, .F. ) ;
#72720 = CARTESIAN_POINT ( 'NONE',  ( 11.33311166264400072, 1479.605569753980035, 208.8962439930940036 ) ) ;
#72721 = EDGE_CURVE ( 'NONE', #66491, #82014, #81686, .T. ) ;
#72722 = DIRECTION ( 'NONE',  ( 0.000000000000000000, -1.000000000000000000, -0.000000000000000000 ) ) ;
#72723 = CARTESIAN_POINT ( 'NONE',  ( -3.648559762950000174, 1443.531551953690041, 199.7293442341890000 ) ) ;
#72724 = CARTESIAN_POINT ( 'NONE',  ( -5.639308305133534205, 1426.925666188799596, 144.1938086916980524 ) ) ;
#72725 = FACE_OUTER_BOUND ( 'NONE', #54788, .T. ) ;
#72726 = CARTESIAN_POINT ( 'NONE',  ( -10.37122021030000063, 1508.772071339130207, 234.9411915187980071 ) ) ;
#72727 = CARTESIAN_POINT ( 'NONE',  ( -42.48766164769039477, 1383.824249582309903, 246.2945377681980119 ) ) ;
#72728 = CARTESIAN_POINT ( 'NONE',  ( -4.544862314595019548, 1508.551704408290107, 205.1599765735010124 ) ) ;
#72729 = CARTESIAN_POINT ( 'NONE',  ( 6.224176841629999402, 1407.473636846729960, 220.5349837110979934 ) ) ;
#72730 = CARTESIAN_POINT ( 'NONE',  ( 0.000000000000000000, 1395.913060387330006, 209.1218459616979999 ) ) ;
#72731 = CARTESIAN_POINT ( 'NONE',  ( 2.500838501690000548, 1464.655874327429956, 236.6367800689979788 ) ) ;
#72733 = EDGE_LOOP ( 'NONE', ( #62171, #96059, #30717, #2074 ) ) ;
#72732 = CARTESIAN_POINT ( 'NONE',  ( -4.678155188338201320, 1508.611350403811230, 212.6094318194185746 ) ) ;
#72734 = CARTESIAN_POINT ( 'NONE',  ( -1.298841827429999984, 1450.798617704459957, 182.5802580294979691 ) ) ;
#72735 = EDGE_CURVE ( 'NONE', #110691, #56739, #21939, .T. ) ;
#72736 = CARTESIAN_POINT ( 'NONE',  ( -14.94466045259999909, 1378.908932901829985, 209.1574112226180091 ) ) ;
#72737 = CARTESIAN_POINT ( 'NONE',  ( -3.152270363119999974, 1474.954422145789977, 198.1306181043989909 ) ) ;
#72739 = EDGE_LOOP ( 'NONE', ( #105374, #18292, #2558, #86164 ) ) ;
#72738 = CARTESIAN_POINT ( 'NONE',  ( -16.93365818059630001, 1414.971717244350202, 208.3952357857560003 ) ) ;
#72740 = CARTESIAN_POINT ( 'NONE',  ( -19.34950756859469934, 1446.106588470199995, 200.0047979462570140 ) ) ;
#72741 = ORIENTED_EDGE ( 'NONE', *, *, #59405, .T. ) ;
#72742 = CARTESIAN_POINT ( 'NONE',  ( -10.18804078449999828, 1389.424862935219835, 216.4200518291889921 ) ) ;
#72743 = CARTESIAN_POINT ( 'NONE',  ( -9.809994025999090539, 1391.913060387289988, 214.8154631801960193 ) ) ;
#72744 = CARTESIAN_POINT ( 'NONE',  ( 3.487584963630629087, 1508.551704408609794, 213.9544627601069351 ) ) ;
#72745 = DIRECTION ( 'NONE',  ( 1.755985294532464991E-16, -1.000000000000000000, 1.338183447452830017E-16 ) ) ;
#72746 = CARTESIAN_POINT ( 'NONE',  ( 3.554051323329999956, 1466.352086058089981, 219.5854740514990056 ) ) ;
#72747 = CARTESIAN_POINT ( 'NONE',  ( -10.06682062296219904, 1472.945273473310181, 207.3391469858899825 ) ) ;
#72748 = DIRECTION ( 'NONE',  ( -6.123233995736769734E-17, -1.000000000000000000, 7.888609052210119587E-33 ) ) ;
#72749 = FACE_OUTER_BOUND ( 'NONE', #71462, .T. ) ;
#72750 = DIRECTION ( 'NONE',  ( 0.000000000000000000, 0.000000000000000000, -1.000000000000000000 ) ) ;
#72751 = FACE_OUTER_BOUND ( 'NONE', #83307, .T. ) ;
#72752 = CARTESIAN_POINT ( 'NONE',  ( -68.77278092737650184, 1379.747928288920093, 280.3133413970129482 ) ) ;
#72753 = AXIS2_PLACEMENT_3D ( 'NONE', #21312, #28650, #106994 ) ;
#72754 = DIRECTION ( 'NONE',  ( 0.000000000000000000, 0.000000000000000000, 1.000000000000000000 ) ) ;
#72755 = VERTEX_POINT ( 'NONE', #71331 ) ;
#72756 = ORIENTED_EDGE ( 'NONE', *, *, #5777, .F. ) ;
#72757 = B_SPLINE_CURVE_WITH_KNOTS ( 'NONE', 5,
 ( #73803, #21142, #29036, #4391, #57001, #63753 ),
 .UNSPECIFIED., .F., .F.,
 ( 6, 6 ),
 ( -68.29823909129999038, -30.60719516609999857 ),
 .UNSPECIFIED. ) ;
#72758 = ADVANCED_FACE ( 'NONE', ( #75697 ), #76754, .F. ) ;
#72759 = CARTESIAN_POINT ( 'NONE',  ( 17.61183580542362037, 1523.982201850120191, 237.6741279912554035 ) ) ;
#72760 = CARTESIAN_POINT ( 'NONE',  ( -11.39648213456350057, 1415.089996094060098, 195.5240353112880030 ) ) ;
#72761 = CARTESIAN_POINT ( 'NONE',  ( -12.68300523669999968, 1434.599391714779813, 149.8266026369979897 ) ) ;
#72762 = EDGE_CURVE ( 'NONE', #43673, #7200, #89289, .T. ) ;
#72763 = CARTESIAN_POINT ( 'NONE',  ( -6.811018194030011041E-10, 1468.607607974030088, 250.1015337166009829 ) ) ;
#72764 = CARTESIAN_POINT ( 'NONE',  ( -20.44043492644280136, 1502.696401150339852, 190.5393524559290199 ) ) ;
#72765 = CARTESIAN_POINT ( 'NONE',  ( -15.58093640500000099, 1419.947093784519893, 211.3491018407289914 ) ) ;
#72766 = CARTESIAN_POINT ( 'NONE',  ( -109.8365661610000075, 1385.307778176620104, 311.3803512332590344 ) ) ;
#72767 = CARTESIAN_POINT ( 'NONE',  ( -8.641402442529509287, 1511.681013979509999, 215.1708878290160101 ) ) ;
#72768 = CARTESIAN_POINT ( 'NONE',  ( -10.93963839782591663, 1363.584717398963221, 210.6218459617030021 ) ) ;
#72769 = CARTESIAN_POINT ( 'NONE',  ( -3.448830483803564828, 1512.187213306747481, 243.0842028158767789 ) ) ;
#72770 = CARTESIAN_POINT ( 'NONE',  ( -3.448830483803564828, 1511.187213306747708, 243.0842028158767789 ) ) ;
#72771 = EDGE_CURVE ( 'NONE', #97433, #53857, #96394, .T. ) ;
#72772 = CARTESIAN_POINT ( 'NONE',  ( -3.463767296015000330, 1517.014196759610059, 207.4190915607570105 ) ) ;
#72773 = CARTESIAN_POINT ( 'NONE',  ( -2.664535259099999805E-15, 1424.786834349990158, 209.1218459616989946 ) ) ;
#72774 = CARTESIAN_POINT ( 'NONE',  ( 11.96005369018680042, 1433.558984481940115, 149.8785667304369724 ) ) ;
#72775 = CARTESIAN_POINT ( 'NONE',  ( -14.07841550641330031, 1435.880379415640164, 150.0502609686649862 ) ) ;
#72776 = CIRCLE ( 'NONE', #67443, 1.000000000000001554 ) ;
#72777 = CARTESIAN_POINT ( 'NONE',  ( -7.780674843099999904, 1385.361898457490042, 218.8940646902889853 ) ) ;
#72778 = CARTESIAN_POINT ( 'NONE',  ( 20.63995199495029809, 1409.633823393240164, 203.6085389666449998 ) ) ;
#72779 = CARTESIAN_POINT ( 'NONE',  ( 1.502806645429999977, 1497.907953363189790, 197.7820368093990169 ) ) ;
#72780 = CARTESIAN_POINT ( 'NONE',  ( -15.46700379407589843, 1461.188231737419756, 228.6959062608830209 ) ) ;
#72781 = EDGE_CURVE ( 'NONE', #87520, #85181, #50980, .T. ) ;
#72782 = ORIENTED_EDGE ( 'NONE', *, *, #77567, .F. ) ;
#72783 = CARTESIAN_POINT ( 'NONE',  ( 29.43658765630000218, 1426.244274388930080, 250.1802633497980253 ) ) ;
#72784 = CARTESIAN_POINT ( 'NONE',  ( -12.99775963039999915, 1420.302662752830201, 196.1023006302990268 ) ) ;
#72786 = CARTESIAN_POINT ( 'NONE',  ( -17.98939636220000082, 1410.465183404129903, 195.2754017030979981 ) ) ;
#72785 = CARTESIAN_POINT ( 'NONE',  ( -3.505536969380000034, 1469.883756972129959, 182.5602054222979973 ) ) ;
#72787 = CARTESIAN_POINT ( 'NONE',  ( 21.40977039944027283, 1506.404057884778922, 204.2043969544953086 ) ) ;
#72788 = CARTESIAN_POINT ( 'NONE',  ( -23.03273353839999871, 1432.943670924359822, 216.3812418159480160 ) ) ;
#72789 = CARTESIAN_POINT ( 'NONE',  ( -0.6032294603500010233, 1487.495129746489965, 219.9704429636989857 ) ) ;
#72790 = CARTESIAN_POINT ( 'NONE',  ( 2.563011323989787815, 1448.466148586485360, 154.6738348880471960 ) ) ;
#72791 = CARTESIAN_POINT ( 'NONE',  ( 27.84004021000000151, 1451.940495779430194, 134.8938502556979984 ) ) ;
#72792 = ORIENTED_EDGE ( 'NONE', *, *, #98337, .T. ) ;
#72793 = CARTESIAN_POINT ( 'NONE',  ( -5.386608739887719821, 1432.386065917429960, 154.6079987177780026 ) ) ;
#72794 = CARTESIAN_POINT ( 'NONE',  ( -19.75056259240000145, 1465.177823603190063, 209.1218459616989946 ) ) ;
#72795 = DIRECTION ( 'NONE',  ( -0.7067700396628828763, 0.03085822887489574409, -0.7067700338480908950 ) ) ;
#72796 = EDGE_LOOP ( 'NONE', ( #26861, #81172, #70217, #68549 ) ) ;
#72797 = ORIENTED_EDGE ( 'NONE', *, *, #10580, .F. ) ;
#72798 = EDGE_CURVE ( 'NONE', #43776, #34771, #44764, .T. ) ;
#72799 = CARTESIAN_POINT ( 'NONE',  ( -3.078458355069999985, 1384.494027187519805, 199.6978503428690033 ) ) ;
#72800 = CARTESIAN_POINT ( 'NONE',  ( -23.74108481809569682, 1410.154262403590110, 208.8447893202840078 ) ) ;
#72801 = VERTEX_POINT ( 'NONE', #104 ) ;
#72802 = CARTESIAN_POINT ( 'NONE',  ( 4.833437623558549667, 1508.551704408389924, 205.2117058254140147 ) ) ;
#72803 = AXIS2_PLACEMENT_3D ( 'NONE', #98551, #22370, #4515 ) ;
#72804 = CARTESIAN_POINT ( 'NONE',  ( 7.666452193948486205, 1446.704586381792069, 154.1277914733520618 ) ) ;
#72805 = EDGE_CURVE ( 'NONE', #16677, #10257, #85904, .T. ) ;
#72806 = CARTESIAN_POINT ( 'NONE',  ( -3.866472413419999921, 1470.481908910429866, 234.9634525317979978 ) ) ;
#72807 = CARTESIAN_POINT ( 'NONE',  ( 16.50400130224763018, 1525.907212628473644, 236.2546788475580968 ) ) ;
#72808 = ORIENTED_EDGE ( 'NONE', *, *, #58984, .T. ) ;
#72809 = CARTESIAN_POINT ( 'NONE',  ( -12.50239138351000001, 1416.520646088589956, 222.1348975693170189 ) ) ;
#72810 = CARTESIAN_POINT ( 'NONE',  ( -0.1660195018879999929, 1419.189969043630072, 184.6475926504979839 ) ) ;
#72811 = CARTESIAN_POINT ( 'NONE',  ( -2.875850132345000087, 1516.647618671360078, 203.3500485059169876 ) ) ;
#72812 = VERTEX_POINT ( 'NONE', #87400 ) ;
#72813 = CARTESIAN_POINT ( 'NONE',  ( -3.430374836980000008, 1431.708658569990121, 216.7924588047190184 ) ) ;
#72814 = CARTESIAN_POINT ( 'NONE',  ( 10.02421119480000122, 1480.534221758890226, 205.8829018067289951 ) ) ;
#72815 = VERTEX_POINT ( 'NONE', #9024 ) ;
#72816 = VERTEX_POINT ( 'NONE', #34227 ) ;
#72817 = CARTESIAN_POINT ( 'NONE',  ( 2.792392588003332232, 1526.382868172863937, 176.8996806668727118 ) ) ;
#72818 = FACE_OUTER_BOUND ( 'NONE', #59557, .T. ) ;
#72819 = CARTESIAN_POINT ( 'NONE',  ( -16.87240959569610155, 1409.502257913620042, 196.1298155364530089 ) ) ;
#72820 = CARTESIAN_POINT ( 'NONE',  ( -4.285317720289061327, 1423.936271504486967, 184.7606816147036000 ) ) ;
#72821 = CARTESIAN_POINT ( 'NONE',  ( 12.35308117012139917, 1452.481681287280026, 149.4845737701170094 ) ) ;
#72822 = CARTESIAN_POINT ( 'NONE',  ( 12.57118999910000134, 1420.461935673439939, 200.4069075869790026 ) ) ;
#72823 = CARTESIAN_POINT ( 'NONE',  ( -1.360835085989610116, 1475.742324412110065, 220.4819849918339969 ) ) ;
#72824 = DIRECTION ( 'NONE',  ( 0.000000000000000000, 1.000000000000000000, 0.000000000000000000 ) ) ;
#72825 = CARTESIAN_POINT ( 'NONE',  ( -11.77874533540000002, 1433.007533761370041, 150.8097953740980017 ) ) ;
#72826 = CARTESIAN_POINT ( 'NONE',  ( 0.03674529885730881684, 1409.783607822271051, 233.1033682352890253 ) ) ;
#72828 = DIRECTION ( 'NONE',  ( -1.755985294532469921E-16, 1.000000000000000000, -1.338183447452831989E-16 ) ) ;
#72827 = CARTESIAN_POINT ( 'NONE',  ( 29.67375955053568148, 1525.697946996616565, 196.9718785854857401 ) ) ;
#72829 = CIRCLE ( 'NONE', #24510, 1.999999999999998668 ) ;
#72830 = CARTESIAN_POINT ( 'NONE',  ( -40.81304585798746842, 1379.731884792838628, 229.1715070870794762 ) ) ;
#72831 = CARTESIAN_POINT ( 'NONE',  ( -9.860305081645158509, 1439.899766047359890, 207.4024662252320184 ) ) ;
#72832 = CARTESIAN_POINT ( 'NONE',  ( -6.681558948264999742, 1511.816633140270142, 201.8377905138470112 ) ) ;
#72833 = EDGE_LOOP ( 'NONE', ( #21246, #79264, #50168, #65730 ) ) ;
#72834 = CARTESIAN_POINT ( 'NONE',  ( 10.78869837091210115, 1414.913060387399810, 222.2791104508980027 ) ) ;
#72835 = CARTESIAN_POINT ( 'NONE',  ( -2.652938167623882126, 1396.005703029557480, 201.4552012694761629 ) ) ;
#72836 = AXIS2_PLACEMENT_3D ( 'NONE', #6074, #84439, #74956 ) ;
#72837 = CARTESIAN_POINT ( 'NONE',  ( -90.81899498049169495, 1384.967630141919926, 308.9748035079580291 ) ) ;
#72838 = CARTESIAN_POINT ( 'NONE',  ( -8.480130668890000223, 1385.259995920419897, 199.8152338849189675 ) ) ;
#72839 = CARTESIAN_POINT ( 'NONE',  ( -5.864566082395439750, 1517.051704408389924, 192.0899093523580063 ) ) ;
#72841 = ORIENTED_EDGE ( 'NONE', *, *, #56365, .F. ) ;
#72840 = CARTESIAN_POINT ( 'NONE',  ( -17.11352124978379763, 1419.945169622900039, 207.4943747003180192 ) ) ;
#72842 = FACE_OUTER_BOUND ( 'NONE', #62717, .T. ) ;
#72843 = CARTESIAN_POINT ( 'NONE',  ( 21.01415622463856891, 1519.551704408389924, 200.8719909741391803 ) ) ;
#72844 = CARTESIAN_POINT ( 'NONE',  ( -14.45783246989999959, 1416.839692131129823, 221.3920770846980020 ) ) ;
#72845 = FACE_OUTER_BOUND ( 'NONE', #28986, .T. ) ;
#72846 = CARTESIAN_POINT ( 'NONE',  ( 13.56546623563500020, 1512.571022561229938, 224.6914189826670167 ) ) ;
#72847 = CARTESIAN_POINT ( 'NONE',  ( -15.90990259576500065, 1516.814170398969964, 224.3246417466669982 ) ) ;
#72848 = CARTESIAN_POINT ( 'NONE',  ( 5.062170296090039656, 1457.731097799089866, 200.0536533579299885 ) ) ;
#72849 = CARTESIAN_POINT ( 'NONE',  ( 0.07204350251990000731, 1420.438792470029966, 183.3235075831980225 ) ) ;
#72850 = CARTESIAN_POINT ( 'NONE',  ( 16.75937749040000213, 1417.431709849029858, 226.7626019668980177 ) ) ;
#72851 = ADVANCED_FACE ( 'NONE', ( #2317 ), #78608, .F. ) ;
#72852 = FACE_OUTER_BOUND ( 'NONE', #26102, .T. ) ;
#72853 = CARTESIAN_POINT ( 'NONE',  ( 3.445407533985000104, 1516.764084769670262, 206.8237970085970119 ) ) ;
#72854 = CARTESIAN_POINT ( 'NONE',  ( 2.281064403174069888, 1474.722235171090006, 220.3124694468160101 ) ) ;
#72855 = CARTESIAN_POINT ( 'NONE',  ( -17.33214102919999888, 1409.518312089029905, 223.0780283743980306 ) ) ;
#72856 = CARTESIAN_POINT ( 'NONE',  ( 14.84366460950000111, 1435.005722275260041, 148.3982965428979810 ) ) ;
#72857 = CARTESIAN_POINT ( 'NONE',  ( -0.9046944608469998927, 1420.511302084529916, 228.1910018231980075 ) ) ;
#72858 = CARTESIAN_POINT ( 'NONE',  ( 20.84791299872678394, 1428.606219089622300, 221.9193619309947962 ) ) ;
#72859 = CARTESIAN_POINT ( 'NONE',  ( 12.73024473090000086, 1416.833018185029914, 223.1308346796979833 ) ) ;
#72860 = CARTESIAN_POINT ( 'NONE',  ( -31.32995031131182628, 1523.678648413191695, 221.9013357025048947 ) ) ;
#72861 = CARTESIAN_POINT ( 'NONE',  ( -38.08542200536700051, 1437.973992156650183, 136.5281536927070078 ) ) ;
#72862 = CARTESIAN_POINT ( 'NONE',  ( 0.2106922363277919930, 1456.959421693720060, 183.0835369170150102 ) ) ;
#72863 = CARTESIAN_POINT ( 'NONE',  ( -10.35371055715830124, 1408.750016124369949, 200.1903725439599953 ) ) ;
#72864 = CARTESIAN_POINT ( 'NONE',  ( -17.05693858869999957, 1415.931669658029932, 202.9275732158079961 ) ) ;
#72865 = CARTESIAN_POINT ( 'NONE',  ( 18.37487226820733355, 1526.382868172863937, 182.5038319547554693 ) ) ;
#72866 = EDGE_CURVE ( 'NONE', #50703, #60010, #87068, .T. ) ;
#72867 = CARTESIAN_POINT ( 'NONE',  ( -28.14748610570159926, 1509.264785235030104, 210.8191992312090122 ) ) ;
#72868 = CARTESIAN_POINT ( 'NONE',  ( 13.19895467340000117, 1434.900408194780084, 147.2732437339979867 ) ) ;
#72869 = CARTESIAN_POINT ( 'NONE',  ( -39.33777288045889975, 1438.052711712020027, 134.0999999977100003 ) ) ;
#72870 = FACE_OUTER_BOUND ( 'NONE', #54915, .T. ) ;
#72871 = VERTEX_POINT ( 'NONE', #40282 ) ;
#72872 = CARTESIAN_POINT ( 'NONE',  ( 1.270728227940000066, 1414.996442546130083, 191.7853923321980005 ) ) ;
#72873 = CARTESIAN_POINT ( 'NONE',  ( -9.407086540023099630, 1428.119775475241568, 137.0999999980979567 ) ) ;
#72874 = CARTESIAN_POINT ( 'NONE',  ( -7.883119093557859891, 1409.188344972089908, 221.8444256219010242 ) ) ;
#72875 = CARTESIAN_POINT ( 'NONE',  ( -11.02929229669999955, 1491.798645198889972, 209.3597145180599739 ) ) ;
#72876 = CARTESIAN_POINT ( 'NONE',  ( 0.000000000000000000, 1523.382868172864164, 209.1218459616979999 ) ) ;
#72877 = CARTESIAN_POINT ( 'NONE',  ( -5.000000000000000000, 1374.913060387289988, 209.1218459572589836 ) ) ;
#72878 = CARTESIAN_POINT ( 'NONE',  ( -45.63712929009999897, 1440.913040511230065, 268.9747524132980061 ) ) ;
#72879 = CARTESIAN_POINT ( 'NONE',  ( 19.59664182059999860, 1435.002040243510237, 209.8413840370809851 ) ) ;
#72880 = CARTESIAN_POINT ( 'NONE',  ( -12.29056600139999844, 1378.273160383739878, 210.0576833531530099 ) ) ;
#72881 = CARTESIAN_POINT ( 'NONE',  ( -92.43963088858200194, 1384.614736519750068, 309.4282936136820013 ) ) ;
#72882 = CARTESIAN_POINT ( 'NONE',  ( -37.45666113624130134, 1384.983989573890085, 210.6155393482590057 ) ) ;
#72883 = CARTESIAN_POINT ( 'NONE',  ( -12.02742519731079973, 1491.141813116759977, 206.6978330293360102 ) ) ;
#72884 = CARTESIAN_POINT ( 'NONE',  ( -4.626713179916450258, 1508.551704408389924, 205.3420549087489917 ) ) ;
#72885 = CARTESIAN_POINT ( 'NONE',  ( -28.35149942255360145, 1508.694958915340067, 208.8230497516570381 ) ) ;
#72886 = CARTESIAN_POINT ( 'NONE',  ( 2.581714097353351889, 1419.606499247553529, 137.0999999980980135 ) ) ;
#72888 = EDGE_LOOP ( 'NONE', ( #106627, #75921, #78682 ) ) ;
#72887 = CARTESIAN_POINT ( 'NONE',  ( 0.4891117522232159565, 1417.821273825019944, 184.7505294229070216 ) ) ;
#72889 = CARTESIAN_POINT ( 'NONE',  ( -11.87970252420000072, 1508.569810688830103, 183.0303274090979926 ) ) ;
#72890 = CARTESIAN_POINT ( 'NONE',  ( 4.897299265963440007, 1421.905024103366259, 138.0290641785962009 ) ) ;
#72891 = CARTESIAN_POINT ( 'NONE',  ( -11.25082884059999877, 1500.153667613989910, 210.9046300046090039 ) ) ;
#72892 = CARTESIAN_POINT ( 'NONE',  ( -0.07306891522338199163, 1420.163695034950024, 183.7345046574349965 ) ) ;
#72893 = DIRECTION ( 'NONE',  ( 0.000000000000000000, 1.000000000000000000, 0.000000000000000000 ) ) ;
#72894 = EDGE_CURVE ( 'NONE', #80364, #19422, #62687, .T. ) ;
#72895 = CARTESIAN_POINT ( 'NONE',  ( 22.02607710719999901, 1409.682227949630033, 213.2973235375779950 ) ) ;
#72896 = FACE_OUTER_BOUND ( 'NONE', #58602, .T. ) ;
#72897 = CARTESIAN_POINT ( 'NONE',  ( -20.42726709853700129, 1466.741775361090049, 211.1910253039249881 ) ) ;
#72898 = CARTESIAN_POINT ( 'NONE',  ( -18.00891941800000140, 1424.550924635830143, 228.0706972725979824 ) ) ;
#72900 = CARTESIAN_POINT ( 'NONE',  ( -11.66434316710000019, 1426.744466202629837, 138.9734773543980282 ) ) ;
#72899 = CARTESIAN_POINT ( 'NONE',  ( -3.699374228837535306, 1511.553914496345442, 201.0215753219823114 ) ) ;
#72901 = CARTESIAN_POINT ( 'NONE',  ( -31.23437356469425907, 1523.382868172864164, 222.8968241038848248 ) ) ;
#72902 = CARTESIAN_POINT ( 'NONE',  ( -8.359890808884999913, 1517.051704408389924, 205.8920033474969955 ) ) ;
#72903 = CARTESIAN_POINT ( 'NONE',  ( -2173.981453289206911, -8382.262153571264207, 1975.191541669308435 ) ) ;
#72904 = CARTESIAN_POINT ( 'NONE',  ( -1.879696342130000142, 1417.130803178230053, 233.8217075207979860 ) ) ;
#72905 = CONICAL_SURFACE ( 'NONE', #78329, 6.911399307709998219, 0.04363323129990067523 ) ;
#72906 = CARTESIAN_POINT ( 'NONE',  ( -2.380813228429999651, 1360.502616939890004, 210.6218459616991936 ) ) ;
#72907 = EDGE_CURVE ( 'NONE', #66206, #23409, #101712, .T. ) ;
#72908 = CARTESIAN_POINT ( 'NONE',  ( 2.284526458645000258, 1516.956048353049937, 205.6588971355569981 ) ) ;
#72909 = CARTESIAN_POINT ( 'NONE',  ( -8.525248407514739668, 1485.814754067230069, 183.6819159046639811 ) ) ;
#72910 = ORIENTED_EDGE ( 'NONE', *, *, #37278, .F. ) ;
#72911 = CARTESIAN_POINT ( 'NONE',  ( -4.378216884482949212, 1453.707746088449994, 199.6107954155660025 ) ) ;
#72912 = CARTESIAN_POINT ( 'NONE',  ( -10.44405160111380759, 1422.438935318351241, 210.6442778920145429 ) ) ;
#72915 = EDGE_LOOP ( 'NONE', ( #20304, #85863 ) ) ;
#72914 = CARTESIAN_POINT ( 'NONE',  ( -67.59948389071639951, 1379.746398059029843, 278.8592533132159588 ) ) ;
#72913 = CIRCLE ( 'NONE', #1451, 13.01015689117599194 ) ;
#72916 = EDGE_CURVE ( 'NONE', #22669, #92171, #47023, .T. ) ;
#72917 = ORIENTED_EDGE ( 'NONE', *, *, #40063, .T. ) ;
#72918 = CARTESIAN_POINT ( 'NONE',  ( 28.65017561800000223, 1509.591492509430054, 210.6114885952979989 ) ) ;
#72919 = EDGE_LOOP ( 'NONE', ( #103060, #3134 ) ) ;
#72920 = CARTESIAN_POINT ( 'NONE',  ( -1.888943442820300023, 1486.364918105139850, 220.8936722016070178 ) ) ;
#72921 = CARTESIAN_POINT ( 'NONE',  ( 12.34024189100000157, 1499.852123274089990, 206.2429094169490043 ) ) ;
#72923 = CARTESIAN_POINT ( 'NONE',  ( 15.72580792003489947, 1409.716081128220139, 192.1010822671919982 ) ) ;
#72922 = CARTESIAN_POINT ( 'NONE',  ( 15.72893663209239890, 1412.349048870499928, 191.4707002167729968 ) ) ;
#72924 = CARTESIAN_POINT ( 'NONE',  ( -6.550870182235000172, 1516.727502608469877, 209.8762341530540141 ) ) ;
#72925 = CARTESIAN_POINT ( 'NONE',  ( -25.06305140060980108, 1451.591299545579886, 137.0985386837109843 ) ) ;
#72926 = CARTESIAN_POINT ( 'NONE',  ( -11.73707087880000088, 1426.695959143629807, 144.1731741466979884 ) ) ;
#72927 = CARTESIAN_POINT ( 'NONE',  ( 11.55483592659999914, 1410.690417346330150, 229.2024983323979939 ) ) ;
#72928 = CARTESIAN_POINT ( 'NONE',  ( 156.6846457583361882, 1526.382868172863937, 340.9912860285725174 ) ) ;
#72929 = CARTESIAN_POINT ( 'NONE',  ( 0.000000000000000000, 0.000000000000000000, 0.000000000000000000 ) ) ;
#72930 = CARTESIAN_POINT ( 'NONE',  ( 41.65423399716409847, 1444.110307755000122, 134.0999999982789745 ) ) ;
#72931 = CARTESIAN_POINT ( 'NONE',  ( -39.90911398472610472, 1441.456692148860157, 136.8748725833579840 ) ) ;
#72932 = CARTESIAN_POINT ( 'NONE',  ( -17.66147422859999949, 1440.150478811289986, 218.7822781203190061 ) ) ;
#72933 = CARTESIAN_POINT ( 'NONE',  ( 3.746090737668994031, 1425.475261178803976, 185.1844613459034576 ) ) ;
#72934 = ORIENTED_EDGE ( 'NONE', *, *, #34393, .F. ) ;
#72935 = ORIENTED_EDGE ( 'NONE', *, *, #16095, .T. ) ;
#72936 = CARTESIAN_POINT ( 'NONE',  ( -5.818574493064999409, 1514.487275757750012, 216.8147464187570108 ) ) ;
#72937 = FACE_OUTER_BOUND ( 'NONE', #64902, .T. ) ;
#72938 = CARTESIAN_POINT ( 'NONE',  ( 0.2178194638410000106, 1452.982787315429960, 183.2541300742979899 ) ) ;
#72939 = CIRCLE ( 'NONE', #46180, 23.05825808840000946 ) ;
#72940 = CARTESIAN_POINT ( 'NONE',  ( -2.981888917330000055, 1484.262615835429870, 183.3265128428980120 ) ) ;
#72941 = EDGE_CURVE ( 'NONE', #85887, #59575, #8036, .T. ) ;
#72942 = CARTESIAN_POINT ( 'NONE',  ( -12.31949146110000015, 1378.253793539069875, 209.5105131724709793 ) ) ;
#72943 = CARTESIAN_POINT ( 'NONE',  ( -68.76678092981147472, 1379.747948897872448, 280.1164399018334166 ) ) ;
#72944 = CARTESIAN_POINT ( 'NONE',  ( -3.061914603009583402, 1369.391151255473005, 210.6218459616997336 ) ) ;
#72945 = CARTESIAN_POINT ( 'NONE',  ( 28.04656794799999986, 1508.051246012029878, 208.1255033510109911 ) ) ;
#72946 =( BOUNDED_CURVE ( )  B_SPLINE_CURVE ( 3, ( #101901, #49881, #33057, #67245 ),
 .UNSPECIFIED., .F., .F. ) 
 B_SPLINE_CURVE_WITH_KNOTS ( ( 4, 4 ),
 ( 4.712545043314881887, 6.283338161952983114 ),
 .UNSPECIFIED. ) 
 CURVE ( )  GEOMETRIC_REPRESENTATION_ITEM ( )  RATIONAL_B_SPLINE_CURVE ( ( 1.000000000000000000, 0.8047386102935668584, 0.8047386102935668584, 1.000000000000000000 ) ) 
 REPRESENTATION_ITEM ( '' )  );
#72947 = EDGE_CURVE ( 'NONE', #33227, #28182, #76275, .T. ) ;
#72948 = CARTESIAN_POINT ( 'NONE',  ( 7.646911088080000418, 1414.913060387329779, 194.5277328420979757 ) ) ;
#72949 = CARTESIAN_POINT ( 'NONE',  ( -52.54124001031040336, 1384.631524148350081, 229.4357186639910253 ) ) ;
#72950 = EDGE_LOOP ( 'NONE', ( #63986, #101764, #13765, #22200 ) ) ;
#72951 = CARTESIAN_POINT ( 'NONE',  ( 9.688817234588901428, 1462.677202180080030, 207.9888309564389886 ) ) ;
#72952 = CARTESIAN_POINT ( 'NONE',  ( -5.788097265284999793, 1517.099836525840146, 206.6397780718770036 ) ) ;
#72953 = ORIENTED_EDGE ( 'NONE', *, *, #61441, .T. ) ;
#72954 = CARTESIAN_POINT ( 'NONE',  ( 35.98947194835299968, 1440.913060387330006, 262.2736039185940058 ) ) ;
#72955 = CARTESIAN_POINT ( 'NONE',  ( 18.74558053519999845, 1457.022375937530114, 227.2948936758980096 ) ) ;
#72956 = VERTEX_POINT ( 'NONE', #2184 ) ;
#72957 = CARTESIAN_POINT ( 'NONE',  ( -111.2060435952740676, 1379.013060387289897, 303.0232821107484824 ) ) ;
#72958 = CARTESIAN_POINT ( 'NONE',  ( 8.303833566477019090, 1428.472849154070218, 213.7034505198590182 ) ) ;
#72959 = CARTESIAN_POINT ( 'NONE',  ( -17.40244824282851255, 1508.456020371283103, 212.7521859866272678 ) ) ;
#72960 = CARTESIAN_POINT ( 'NONE',  ( 21.08771820830000010, 1497.249269049990062, 211.1908499358290214 ) ) ;
#72961 = CARTESIAN_POINT ( 'NONE',  ( -7.845903147674250455, 1436.115355770489941, 214.9328208583779940 ) ) ;
#72962 = CARTESIAN_POINT ( 'NONE',  ( -5.469699274806250067, 1510.954290761809943, 201.4579565197620070 ) ) ;
#72963 = CARTESIAN_POINT ( 'NONE',  ( -3.540693246070000022, 1508.270058569329876, 180.7688421415979860 ) ) ;
#72964 = CARTESIAN_POINT ( 'NONE',  ( -11.87952668650000021, 1433.311289539269865, 147.8551187025980198 ) ) ;
#72965 = CARTESIAN_POINT ( 'NONE',  ( 26.80046753784469971, 1506.622207043549906, 206.2312287904520076 ) ) ;
#72967 = DIRECTION ( 'NONE',  ( 0.9455185755993178454, 0.000000000000000000, -0.3255681544571537578 ) ) ;
#72966 = CARTESIAN_POINT ( 'NONE',  ( 6.084791432159999403, 1464.440196481730027, 234.2785017269980017 ) ) ;
#72968 = AXIS2_PLACEMENT_3D ( 'NONE', #64509, #81269, #80189 ) ;
#72969 = CARTESIAN_POINT ( 'NONE',  ( -2.483949978725000118, 1517.156142772249950, 216.0726795003369887 ) ) ;
#72970 = CARTESIAN_POINT ( 'NONE',  ( -22.59789932822333114, 1409.702173780693784, 209.4225277437891179 ) ) ;
#72971 = CARTESIAN_POINT ( 'NONE',  ( -10.23881579017958643, 1480.796270772398884, 206.5571936345679376 ) ) ;
#72972 = CARTESIAN_POINT ( 'NONE',  ( 6.232532001850000114, 1407.162969929529936, 220.5304192662980256 ) ) ;
#72974 = B_SPLINE_CURVE_WITH_KNOTS ( 'NONE', 5,
 ( #79967, #3284, #20580, #80524, #37967, #72148, #103223, #26532, #92761, #83266, #100064, #40160, #60728, #91664, #74343, #84367, #110121, #99494, #41813, #22777, #14390 ),
 .UNSPECIFIED., .F., .F.,
 ( 6, 3, 3, 3, 3, 3, 6 ),
 ( 37.33063420879999939, 38.00991709350000036, 40.59642292560000243, 43.18292875779999918, 44.87875381330000124, 46.52360639289999966, 48.64583233200000478 ),
 .UNSPECIFIED. ) ;
#72973 = CARTESIAN_POINT ( 'NONE',  ( 7.335900995594999863, 1517.068717944079935, 213.1567545299469657 ) ) ;
#72975 = CARTESIAN_POINT ( 'NONE',  ( 18.63433765150000099, 1508.246382733229893, 188.5113568914979965 ) ) ;
#72976 = CARTESIAN_POINT ( 'NONE',  ( -4.501970322318059381, 1483.174855501109960, 199.4671179167419837 ) ) ;
#72978 = EDGE_LOOP ( 'NONE', ( #67674, #92822, #33496, #88765, #49975 ) ) ;
#72977 = CARTESIAN_POINT ( 'NONE',  ( -106.5907474589999993, 1390.522254817180055, 304.4566592667590044 ) ) ;
#72979 = CARTESIAN_POINT ( 'NONE',  ( -1.775988990187477246, 1526.208281990535852, 177.6737791622278451 ) ) ;
#72980 = CARTESIAN_POINT ( 'NONE',  ( 7.601478266899999170, 1459.957272486130023, 217.3594088466479946 ) ) ;
#72981 = CARTESIAN_POINT ( 'NONE',  ( -11.85693426559999963, 1431.696772119709976, 149.9476199621979902 ) ) ;
#72982 = CARTESIAN_POINT ( 'NONE',  ( -20.69918688649430294, 1486.905067481629885, 208.2779964567390039 ) ) ;
#72983 = CARTESIAN_POINT ( 'NONE',  ( -6.985287221996019369, 1440.244100505809911, 203.7176696286690287 ) ) ;
#72984 = FACE_OUTER_BOUND ( 'NONE', #107780, .T. ) ;
#72985 = CARTESIAN_POINT ( 'NONE',  ( -19.79581205538870137, 1456.560075471280015, 209.4938375809250033 ) ) ;
#72986 = CIRCLE ( 'NONE', #10384, 95.87905590040163872 ) ;
#72987 = CARTESIAN_POINT ( 'NONE',  ( 12.53380496490000162, 1445.052233482669862, 186.0874927582979979 ) ) ;
#72989 = CARTESIAN_POINT ( 'NONE',  ( 19.08704549389999627, 1456.215544484829934, 225.8584252592980022 ) ) ;
#72988 = CARTESIAN_POINT ( 'NONE',  ( -20.98155299119999739, 1444.799239553469988, 222.3056163179979876 ) ) ;
#72990 = CARTESIAN_POINT ( 'NONE',  ( 19.09822630769999918, 1458.162647406989890, 212.8926528854489959 ) ) ;
#72991 = VERTEX_POINT ( 'NONE', #20046 ) ;
#72993 = CIRCLE ( 'NONE', #10389, 15.40132948099999943 ) ;
#72992 = CARTESIAN_POINT ( 'NONE',  ( 2.285487581364999965, 1517.001127920769704, 205.0775242521070254 ) ) ;
#72994 = CARTESIAN_POINT ( 'NONE',  ( 1.774875596600000049, 1405.867537697030002, 267.2336946155980399 ) ) ;
#72995 = CARTESIAN_POINT ( 'NONE',  ( 0.7331377668379990276, 1515.470556211590065, 213.3402424911989783 ) ) ;
#72996 = VECTOR ( 'NONE', #84003, 1000.000000000000000 ) ;
#72998 = B_SPLINE_CURVE_WITH_KNOTS ( 'NONE', 3,
 ( #36764, #87165, #9900, #70398, #78207, #3741 ),
 .UNSPECIFIED., .F., .F.,
 ( 4, 2, 4 ),
 ( -1.131363979616252987E-05, 0.001067788114096044532, 0.002146889867988251502 ),
 .UNSPECIFIED. ) ;
#72997 = DIRECTION ( 'NONE',  ( 0.000000000000000000, 1.000000000000000000, 0.000000000000000000 ) ) ;
#72999 = CIRCLE ( 'NONE', #24665, 2.000000000000003553 ) ;
#73000 = CARTESIAN_POINT ( 'NONE',  ( 24.65284846709989708, 1440.998862877870124, 212.5088464049670165 ) ) ;
#73001 = CARTESIAN_POINT ( 'NONE',  ( -23.91828057749999914, 1452.077818060030040, 136.8096204223980124 ) ) ;
#73002 = DIRECTION ( 'NONE',  ( -1.000000000000000000, 0.000000000000000000, 0.000000000000000000 ) ) ;
#73003 = CARTESIAN_POINT ( 'NONE',  ( -1.466050900909950050, 1450.686205460179963, 155.3356496213909850 ) ) ;
#73004 = CARTESIAN_POINT ( 'NONE',  ( -1.556377437525894969, 1451.184650619072954, 183.7355129867053734 ) ) ;
#73005 = CARTESIAN_POINT ( 'NONE',  ( 2.498115803822699821, 1449.212599866119945, 155.3362470018159911 ) ) ;
#73006 = CARTESIAN_POINT ( 'NONE',  ( -105.5460821599999974, 1391.484866075830041, 304.2071864700581614 ) ) ;
#73007 = CARTESIAN_POINT ( 'NONE',  ( 12.78776258890000150, 1416.851343894929869, 222.4918226423980059 ) ) ;
#73008 = CARTESIAN_POINT ( 'NONE',  ( -20.41675369440000054, 1438.655740950709969, 219.6133835466979747 ) ) ;
#73009 = DIRECTION ( 'NONE',  ( -0.000000000000000000, -1.000000000000000000, -0.000000000000000000 ) ) ;
#73010 = CARTESIAN_POINT ( 'NONE',  ( 2.500000000000000000, 1439.072300154540017, 157.1879318970979966 ) ) ;
#73011 = CARTESIAN_POINT ( 'NONE',  ( -2.094747537599999987, 1475.526797592629919, 269.2930943650979998 ) ) ;
#73012 = CARTESIAN_POINT ( 'NONE',  ( -4.232601323828700579, 1446.314705677049915, 164.3433706556850211 ) ) ;
#73013 = CARTESIAN_POINT ( 'NONE',  ( 8.784743044050069116, 1452.237884045540113, 212.1741271052380000 ) ) ;
#73014 = CARTESIAN_POINT ( 'NONE',  ( -21.12212911286992068, 1512.187213306747481, 235.8226600804187285 ) ) ;
#73015 = CARTESIAN_POINT ( 'NONE',  ( -37.93199094438229935, 1384.796719469609798, 238.6434350429059918 ) ) ;
#73016 = CARTESIAN_POINT ( 'NONE',  ( 3.827327205999999649, 1432.413060387330006, 146.1721969590979882 ) ) ;
#73017 = CARTESIAN_POINT ( 'NONE',  ( 3.744429477602492895, 1509.032014137963188, 213.3627840903013180 ) ) ;
#73018 = CARTESIAN_POINT ( 'NONE',  ( 12.32485495299399858, 1492.010170158399887, 208.9028815630869929 ) ) ;
#73019 = CARTESIAN_POINT ( 'NONE',  ( 32.13446200735371860, 1525.163457223744444, 217.0282479337336383 ) ) ;
#73020 = CARTESIAN_POINT ( 'NONE',  ( 8.147597079235938011, 1511.509056589849934, 205.2719880346207901 ) ) ;
#73021 = CARTESIAN_POINT ( 'NONE',  ( -2.832629554588100174, 1396.011977991119920, 219.7725838655079826 ) ) ;
#73022 = B_SPLINE_CURVE_WITH_KNOTS ( 'NONE', 5,
 ( #6355, #5818, #40503, #107159, #13625, #29890 ),
 .UNSPECIFIED., .F., .F.,
 ( 6, 6 ),
 ( 0.000000000000000000, 1.000000000000000000 ),
 .UNSPECIFIED. ) ;
#73023 = CARTESIAN_POINT ( 'NONE',  ( -14.65117625699999948, 1422.174524681930279, 228.3982350620979958 ) ) ;
#73024 = CARTESIAN_POINT ( 'NONE',  ( -44.92382433299999889, 1440.913060387330006, 269.6913831256979961 ) ) ;
#73025 = EDGE_CURVE ( 'NONE', #21931, #48402, #36299, .T. ) ;
#73026 = ORIENTED_EDGE ( 'NONE', *, *, #50103, .F. ) ;
#73027 = DIRECTION ( 'NONE',  ( 0.000000000000000000, 1.000000000000000000, -6.123233995736769734E-17 ) ) ;
#73028 = CARTESIAN_POINT ( 'NONE',  ( -7.509820346537817493, 1510.675349056949244, 215.1027603218261106 ) ) ;
#73029 = DIRECTION ( 'NONE',  ( -8.555280247707230573E-26, -1.000000000000000000, 1.836970198721029688E-16 ) ) ;
#73031 = CARTESIAN_POINT ( 'NONE',  ( -12.85600966886500096, 1512.300546902530186, 193.9285717199670103 ) ) ;
#73030 = CARTESIAN_POINT ( 'NONE',  ( 11.41401861810000007, 1426.451055098430061, 121.0026485950980089 ) ) ;
#73032 = CARTESIAN_POINT ( 'NONE',  ( 9794.298952142280541, 2837.541834147234567, -1088.485031629833202 ) ) ;
#73033 = CARTESIAN_POINT ( 'NONE',  ( -4.378216172770000192, 1453.707746473490033, 199.6107950798590025 ) ) ;
#73034 = CARTESIAN_POINT ( 'NONE',  ( -3.454748846324999789, 1516.609912606490070, 201.7988116581369979 ) ) ;
#73035 = CARTESIAN_POINT ( 'NONE',  ( 12.24365541422369930, 1500.600794001439908, 208.6479367469619888 ) ) ;
#73036 = CARTESIAN_POINT ( 'NONE',  ( -5.586162938070000195, 1491.245995699590139, 185.8699225748990216 ) ) ;
#73037 = CARTESIAN_POINT ( 'NONE',  ( 3.214223997639999997, 1507.157966923930189, 181.4588691503979874 ) ) ;
#73038 = FACE_BOUND ( 'NONE', #15460, .T. ) ;
#73039 = CARTESIAN_POINT ( 'NONE',  ( -57.85321423391380335, 1379.895658627149942, 259.2190435032479741 ) ) ;
#73040 = CARTESIAN_POINT ( 'NONE',  ( 4.501691961677919629, 1368.956319095248091, 210.6218459616987957 ) ) ;
#73042 = EDGE_LOOP ( 'NONE', ( #23188, #84834, #25109, #11538 ) ) ;
#73041 = CARTESIAN_POINT ( 'NONE',  ( -14.01382144633140037, 1379.590371145329982, 211.9185990975750258 ) ) ;
#73043 = VERTEX_POINT ( 'NONE', #72147 ) ;
#73044 = ADVANCED_FACE ( 'NONE', ( #79966 ), #16174, .T. ) ;
#73045 = CARTESIAN_POINT ( 'NONE',  ( 11.60004869885203682, 0.000000000000000000, 137.0999999980979851 ) ) ;
#73046 = CARTESIAN_POINT ( 'NONE',  ( -7.105427357599999217E-15, 1423.509254465030153, 167.6739826277979830 ) ) ;
#73047 = CARTESIAN_POINT ( 'NONE',  ( 1.440662989070000011, 1507.675818290129882, 236.8848933730980093 ) ) ;
#73048 = CARTESIAN_POINT ( 'NONE',  ( -13.44029829071352289, 1444.325445693611982, 169.3641228205755169 ) ) ;
#73049 = CARTESIAN_POINT ( 'NONE',  ( 3.487133837120000024, 1431.113060387329824, 227.6029907049980068 ) ) ;
#73050 = CARTESIAN_POINT ( 'NONE',  ( 2.372478608332514671, 1512.187213306747481, 174.8996806668726549 ) ) ;
#73052 = CARTESIAN_POINT ( 'NONE',  ( 17.58529957360000040, 1413.534267924229880, 225.6949097933979829 ) ) ;
#73051 = CARTESIAN_POINT ( 'NONE',  ( -7.724153670609999800, 1383.436097328069991, 218.9006927288590134 ) ) ;
#73053 = CARTESIAN_POINT ( 'NONE',  ( 10.37662516520000011, 1410.292580643930023, 188.8195959794979899 ) ) ;
#73054 = CARTESIAN_POINT ( 'NONE',  ( -5.302730571406519822, 1464.205385412599981, 199.9536530435450175 ) ) ;
#73055 = EDGE_CURVE ( 'NONE', #64407, #104566, #21125, .T. ) ;
#73056 = CARTESIAN_POINT ( 'NONE',  ( -39.04566459149999957, 1447.730051266930104, 136.5320742054979917 ) ) ;
#73057 = CARTESIAN_POINT ( 'NONE',  ( 11.03661645814000103, 1396.298467526650029, 208.2457624720319984 ) ) ;
#73058 = CARTESIAN_POINT ( 'NONE',  ( 1.547118986179999878, 1416.568813549730066, 190.2343231038979923 ) ) ;
#73059 = CARTESIAN_POINT ( 'NONE',  ( 11.73653109249999993, 1426.280329148629789, 144.1709412064980143 ) ) ;
#73060 = CARTESIAN_POINT ( 'NONE',  ( 3.415238410854999795, 1511.775527460079957, 212.5370843810869985 ) ) ;
#73061 = EDGE_LOOP ( 'NONE', ( #99890, #14114, #29655, #5065, #9800, #95064 ) ) ;
#73062 = CARTESIAN_POINT ( 'NONE',  ( 4.218115660059999605, 1425.254488096429895, 185.4299414137979909 ) ) ;
#73063 = DIRECTION ( 'NONE',  ( -0.000000000000000000, -1.000000000000000000, -0.000000000000000000 ) ) ;
#73064 = ORIENTED_EDGE ( 'NONE', *, *, #42085, .T. ) ;
#73065 = VERTEX_POINT ( 'NONE', #44730 ) ;
#73066 = CARTESIAN_POINT ( 'NONE',  ( -19.86657363567449863, 1497.939529676289794, 228.5868823338410039 ) ) ;
#73067 = CARTESIAN_POINT ( 'NONE',  ( 20.69709747799999988, 1495.539518117790067, 213.2340985757189742 ) ) ;
#73068 = CIRCLE ( 'NONE', #31959, 0.9999999999999998890 ) ;
#73069 = CARTESIAN_POINT ( 'NONE',  ( -109.7582210444096802, 1386.278646697699969, 311.3050739296813845 ) ) ;
#73070 = CARTESIAN_POINT ( 'NONE',  ( -29.61692403811275298, 1526.104292489132376, 197.4873780791112949 ) ) ;
#73071 = CARTESIAN_POINT ( 'NONE',  ( -3.451033427095000050, 1517.025653221279981, 214.9083735325669977 ) ) ;
#73072 = CARTESIAN_POINT ( 'NONE',  ( -14.43834517638610038, 1380.180499307529999, 209.0320278544499786 ) ) ;
#73073 = AXIS2_PLACEMENT_3D ( 'NONE', #63815, #99028, #108549 ) ;
#73074 = ORIENTED_EDGE ( 'NONE', *, *, #74106, .T. ) ;
#73075 = CARTESIAN_POINT ( 'NONE',  ( -18.67382096187029816, 1508.542127769639819, 210.2892683469680151 ) ) ;
#73076 = CARTESIAN_POINT ( 'NONE',  ( 0.04954745150389999742, 1508.966889293630175, 179.3740839253979971 ) ) ;
#73077 = CARTESIAN_POINT ( 'NONE',  ( -52.12027059500000092, 1379.080878082759909, 241.5351867017590166 ) ) ;
#73078 = EDGE_CURVE ( 'NONE', #52143, #77481, #20579, .T. ) ;
#73079 = CARTESIAN_POINT ( 'NONE',  ( 18.69410140469999959, 1415.934222461130048, 210.6093379841479987 ) ) ;
#73080 = CARTESIAN_POINT ( 'NONE',  ( -3.460101890015000237, 1516.812923327049930, 205.0932153474469715 ) ) ;
#73081 = VERTEX_POINT ( 'NONE', #107910 ) ;
#73082 = CARTESIAN_POINT ( 'NONE',  ( -8.099792069101098946, 1452.596710452009802, 204.5152729218939669 ) ) ;
#73083 = CARTESIAN_POINT ( 'NONE',  ( -35.05411225082677618, 1424.110335121155231, 269.5322562813408922 ) ) ;
#73084 = CARTESIAN_POINT ( 'NONE',  ( -1.953612668519999707, 1408.981282045029957, 231.3328323811979885 ) ) ;
#73086 = EDGE_LOOP ( 'NONE', ( #96785, #108034, #27933, #28951 ) ) ;
#73085 = CARTESIAN_POINT ( 'NONE',  ( -2.442490654179999457E-15, 1519.913060387329779, 186.5374469562979698 ) ) ;
#73087 = CARTESIAN_POINT ( 'NONE',  ( -0.01304300961527469875, 1452.999749643619907, 183.2385070609109903 ) ) ;
#73088 = CARTESIAN_POINT ( 'NONE',  ( -31.74795755313090240, 1440.913060389009843, 243.4509895537200066 ) ) ;
#73089 = CARTESIAN_POINT ( 'NONE',  ( -81.22608496769998965, 1384.058471608169839, 304.8846490667589819 ) ) ;
#73090 = CARTESIAN_POINT ( 'NONE',  ( -0.3644052467364989889, 1465.020711461070050, 237.7552395868789858 ) ) ;
#73091 = AXIS2_PLACEMENT_3D ( 'NONE', #38450, #89957, #64795 ) ;
#73092 = CARTESIAN_POINT ( 'NONE',  ( 25.30727743885159953, 1414.908034988650115, 270.3546021691070109 ) ) ;
#73093 = CARTESIAN_POINT ( 'NONE',  ( -7.710610441124999603, 1516.594591938570147, 212.5759658869370128 ) ) ;
#73094 = CARTESIAN_POINT ( 'NONE',  ( -60.11231289889999374, 1379.722095685149952, 261.7638568618589829 ) ) ;
#73095 = CARTESIAN_POINT ( 'NONE',  ( 23.53385057170000039, 1410.392363598830116, 208.0208997170380201 ) ) ;
#73096 = CARTESIAN_POINT ( 'NONE',  ( 28.27139721233031722, 1526.382868172864164, 198.6830693683572235 ) ) ;
#73097 = CARTESIAN_POINT ( 'NONE',  ( 14.05303364027069968, 1427.055417490390028, 197.7369918085530003 ) ) ;
#73098 = CARTESIAN_POINT ( 'NONE',  ( -7.709376407373089712, 1516.547466091170008, 210.8176141999059894 ) ) ;
#73099 = CARTESIAN_POINT ( 'NONE',  ( -6.935801299664999142, 1516.621991115350056, 210.2518484644969874 ) ) ;
#73100 = CARTESIAN_POINT ( 'NONE',  ( 4.180280406913070124, 1421.234997433459966, 185.2258708144169930 ) ) ;
#73101 = CARTESIAN_POINT ( 'NONE',  ( -0.6154731172430000230, 1417.919335479829897, 233.4687737631979871 ) ) ;
#73102 = CARTESIAN_POINT ( 'NONE',  ( 9.482715713316885342, 1424.109889425399160, 139.1406707392753219 ) ) ;
#73103 = ORIENTED_EDGE ( 'NONE', *, *, #103453, .T. ) ;
#73104 = CARTESIAN_POINT ( 'NONE',  ( -28.14421679356709660, 1385.242063718970030, 226.2112307642150029 ) ) ;
#73105 = CARTESIAN_POINT ( 'NONE',  ( -15.36551281277120040, 1420.352422733189769, 229.0210882522540032 ) ) ;
#73106 = CARTESIAN_POINT ( 'NONE',  ( 0.4612165794449999967, 1416.141396914929828, 233.4958257179979739 ) ) ;
#73107 = DIRECTION ( 'NONE',  ( -1.755985294532469921E-16, 1.000000000000000000, -1.338183447452831989E-16 ) ) ;
#73108 = CARTESIAN_POINT ( 'NONE',  ( 7.548380872364999661, 1510.399296111369949, 204.3167683741870064 ) ) ;
#73109 = CARTESIAN_POINT ( 'NONE',  ( 12.11317892429999965, 1426.372560516109843, 203.9710410313989826 ) ) ;
#73110 = CARTESIAN_POINT ( 'NONE',  ( 2.134964941497458302, 1389.913060387289988, 207.8211059036665063 ) ) ;
#73112 = CARTESIAN_POINT ( 'NONE',  ( 9.788554748827010599, 1435.243870499410150, 208.4607419128279844 ) ) ;
#73111 = CARTESIAN_POINT ( 'NONE',  ( 4.036748838804999906, 1516.667393516340098, 216.0582443258770127 ) ) ;
#73113 = CARTESIAN_POINT ( 'NONE',  ( -26.60987491003508865, 1450.724930346239034, 136.4551442334351350 ) ) ;
#73114 = CARTESIAN_POINT ( 'NONE',  ( 10.06361417826360061, 1469.502718807920019, 207.4652888198990013 ) ) ;
#73115 = ORIENTED_EDGE ( 'NONE', *, *, #54917, .F. ) ;
#73116 = CARTESIAN_POINT ( 'NONE',  ( 6.553524377605000062, 1516.882690742909972, 202.1776141839370098 ) ) ;
#73117 = DIRECTION ( 'NONE',  ( 0.9455185755993178454, 0.000000000000000000, -0.3255681544571537578 ) ) ;
#73118 = ORIENTED_EDGE ( 'NONE', *, *, #22303, .F. ) ;
#73119 = CARTESIAN_POINT ( 'NONE',  ( 11.60004869885204570, 1426.273943615695998, 138.2686089212693332 ) ) ;
#73120 = CARTESIAN_POINT ( 'NONE',  ( 23.21630602169999946, 1448.997447280589995, 218.4239157672980127 ) ) ;
#73121 = CARTESIAN_POINT ( 'NONE',  ( 7.905726602093638533, 1438.201532849469913, 153.7305789053409057 ) ) ;
#73122 = CARTESIAN_POINT ( 'NONE',  ( 7.558249307053370281, 1510.689985724130111, 203.4323075703590007 ) ) ;
#73123 = CARTESIAN_POINT ( 'NONE',  ( 1.569168191259999956, 1442.549728379589851, 218.2360776051089886 ) ) ;
#73124 = DIRECTION ( 'NONE',  ( -1.836970198721029688E-16, -1.000000000000000000, 0.000000000000000000 ) ) ;
#73125 = CARTESIAN_POINT ( 'NONE',  ( -3.123967365489999981, 1446.720974256299996, 162.7331173440980194 ) ) ;
#73126 = CARTESIAN_POINT ( 'NONE',  ( -19.61843130789999989, 1426.543110900729744, 225.3457329349979830 ) ) ;
#73127 = CARTESIAN_POINT ( 'NONE',  ( 4.431405375871572794, 1485.802552508792360, 199.2752504294042524 ) ) ;
#73128 = CARTESIAN_POINT ( 'NONE',  ( -103.5631853459999974, 1389.967198823729859, 302.9633942972590148 ) ) ;
#73129 = CARTESIAN_POINT ( 'NONE',  ( 15.40324653509999919, 1508.176740489129998, 186.7739816122980017 ) ) ;
#73131 = CARTESIAN_POINT ( 'NONE',  ( -17.34555439375539976, 1433.759845372730069, 216.6575063138343182 ) ) ;
#73130 = CARTESIAN_POINT ( 'NONE',  ( -106.4806709740000059, 1391.913060444069970, 302.1193611446589671 ) ) ;
#73132 = CARTESIAN_POINT ( 'NONE',  ( -9.699660872752350116, 1472.030908259890111, 212.1562907213800031 ) ) ;
#73133 = ORIENTED_EDGE ( 'NONE', *, *, #27478, .F. ) ;
#73134 = FACE_OUTER_BOUND ( 'NONE', #98363, .T. ) ;
#73135 = CARTESIAN_POINT ( 'NONE',  ( -15.59348407829999950, 1508.491154456789900, 214.8963640716490033 ) ) ;
#73136 = CARTESIAN_POINT ( 'NONE',  ( 3.348648543330357885, 1523.530935881284904, 242.0864759303845801 ) ) ;
#73137 = CARTESIAN_POINT ( 'NONE',  ( -5.292247061280000331, 1391.613060387290034, 209.1218459616989946 ) ) ;
#73138 = DIRECTION ( 'NONE',  ( 6.360620485575798415E-17, 1.000000000000000000, -8.754643039332639448E-17 ) ) ;
#73139 = CARTESIAN_POINT ( 'NONE',  ( 1.450275408081650008, 1505.525276553959884, 181.1825906324010020 ) ) ;
#73140 = CARTESIAN_POINT ( 'NONE',  ( -2.708195641334396608, 1524.374578187333100, 241.9868732463102958 ) ) ;
#73141 = CARTESIAN_POINT ( 'NONE',  ( -12.82065136370706959, 1442.853462007010876, 186.3191038284279841 ) ) ;
#73142 = CARTESIAN_POINT ( 'NONE',  ( 8.999538239140179030, 1407.274461440940058, 198.9439808189530083 ) ) ;
#73143 = DIRECTION ( 'NONE',  ( 0.000000000000000000, -6.123233995736759873E-17, -1.000000000000000000 ) ) ;
#73144 = AXIS2_PLACEMENT_3D ( 'NONE', #27782, #68163, #33968 ) ;
#73145 = CARTESIAN_POINT ( 'NONE',  ( 30.31940284292420174, 1518.913060387330006, 222.4933038710543087 ) ) ;
#73146 = CARTESIAN_POINT ( 'NONE',  ( 17.60611259787588523, 1410.890515051577950, 223.7447835159890985 ) ) ;
#73147 = AXIS2_PLACEMENT_3D ( 'NONE', #71639, #78907, #28489 ) ;
#73148 = CARTESIAN_POINT ( 'NONE',  ( 23.77649893510000112, 1435.334014145809988, 137.3596790345980025 ) ) ;
#73149 = CARTESIAN_POINT ( 'NONE',  ( 5.009886284249999377, 1430.069699660889910, 217.1776678749689893 ) ) ;
#73151 = ORIENTED_EDGE ( 'NONE', *, *, #56832, .F. ) ;
#73150 = CARTESIAN_POINT ( 'NONE',  ( 7.359652241210000057, 1491.427741320190080, 211.7193137660989919 ) ) ;
#73152 = CARTESIAN_POINT ( 'NONE',  ( -32.28466283162143213, 1512.187213306747481, 219.1752493337717738 ) ) ;
#73153 = CARTESIAN_POINT ( 'NONE',  ( 14.28356506509309831, 1513.356256558030054, 224.3145391780770126 ) ) ;
#73154 = EDGE_LOOP ( 'NONE', ( #25288, #58141, #67011, #88147 ) ) ;
#73155 = ORIENTED_EDGE ( 'NONE', *, *, #50118, .T. ) ;
#73156 = DIRECTION ( 'NONE',  ( 0.000000000000000000, 1.000000000000000000, 0.000000000000000000 ) ) ;
#73157 = CARTESIAN_POINT ( 'NONE',  ( -109.1646038599999997, 1384.934474657399960, 297.1326231125589743 ) ) ;
#73158 = CARTESIAN_POINT ( 'NONE',  ( -11.66675062582269895, 1378.331411511049055, 205.1377757328165785 ) ) ;
#73160 = CARTESIAN_POINT ( 'NONE',  ( -24.64758684859999960, 1455.655050827730065, 240.2509105628980137 ) ) ;
#73159 = CARTESIAN_POINT ( 'NONE',  ( 35.00577369931135507, 1424.057531348699285, 269.5315920939452781 ) ) ;
#73161 = CARTESIAN_POINT ( 'NONE',  ( -20.26716426260000148, 1499.099646743829908, 190.0126279463979984 ) ) ;
#73162 = CARTESIAN_POINT ( 'NONE',  ( -11.90126260809999970, 1433.308376196790050, 149.9471563285979983 ) ) ;
#73163 = CARTESIAN_POINT ( 'NONE',  ( 3.250000000000000444, 1524.551704408390151, 209.1218459616989946 ) ) ;
#73164 = CARTESIAN_POINT ( 'NONE',  ( -19.34584564980000110, 1485.639564621229965, 189.8374633502980089 ) ) ;
#73165 = AXIS2_PLACEMENT_3D ( 'NONE', #38612, #10680, #62203 ) ;
#73166 = CARTESIAN_POINT ( 'NONE',  ( 24.71878886508709883, 1425.936351871569968, 209.5854886089860258 ) ) ;
#73167 = CARTESIAN_POINT ( 'NONE',  ( -2.372478608332517336, 1522.382868172863937, 243.3440112565233449 ) ) ;
#73168 = CARTESIAN_POINT ( 'NONE',  ( -24.67000132220000097, 1440.968503961899842, 210.6876455942679911 ) ) ;
#73169 = CARTESIAN_POINT ( 'NONE',  ( 6.907297471969998881, 1441.639242655719954, 154.4648439803980011 ) ) ;
#73170 = CARTESIAN_POINT ( 'NONE',  ( -8.143105617842628874, 1478.527044422649851, 217.4342497289609923 ) ) ;
#73171 = CARTESIAN_POINT ( 'NONE',  ( -2.380813228419999650, 1360.502616939890004, 207.6218459616989946 ) ) ;
#73172 = CARTESIAN_POINT ( 'NONE',  ( 31.50799703744293367, 1524.382868172863937, 201.8203724569132191 ) ) ;
#73174 = VERTEX_POINT ( 'NONE', #101147 ) ;
#73173 = CARTESIAN_POINT ( 'NONE',  ( 1.314629143778269967E-08, 1407.049767188329952, 264.9246803212090526 ) ) ;
#73175 = VERTEX_POINT ( 'NONE', #5456 ) ;
#73176 = CARTESIAN_POINT ( 'NONE',  ( -12.81343579419999834, 1504.349109748190131, 208.8281390619199840 ) ) ;
#73177 = CARTESIAN_POINT ( 'NONE',  ( 24.05733473906539999, 1495.051195187770190, 207.1050250271510151 ) ) ;
#73178 = CARTESIAN_POINT ( 'NONE',  ( -15.30542548040000028, 1471.644218537830056, 270.3573229403979781 ) ) ;
#73179 = CARTESIAN_POINT ( 'NONE',  ( 13.19514936480000067, 1509.316610144029937, 234.6191713803979724 ) ) ;
#73180 = DIRECTION ( 'NONE',  ( 0.000000000000000000, 0.000000000000000000, -1.000000000000000000 ) ) ;
#73181 = CYLINDRICAL_SURFACE ( 'NONE', #107333, 1.000000000000003109 ) ;
#73182 = CARTESIAN_POINT ( 'NONE',  ( 0.2118832605204210018, 1452.815003554979967, 183.2547493383920028 ) ) ;
#73183 = CARTESIAN_POINT ( 'NONE',  ( 5.170554601400000116, 1484.055082523290139, 219.7711189574989703 ) ) ;
#73184 = LINE ( 'NONE', #69204, #89583 ) ;
#73185 = CARTESIAN_POINT ( 'NONE',  ( -5.208772481359999595, 1458.757019672090109, 218.5248626948989852 ) ) ;
#73186 = CARTESIAN_POINT ( 'NONE',  ( 11.23464237080011863, 1364.859423985571993, 210.6218459617030021 ) ) ;
#73187 = CARTESIAN_POINT ( 'NONE',  ( -28.78832826715930082, 1414.041031752499975, 269.2046387276820383 ) ) ;
#73188 = B_SPLINE_CURVE_WITH_KNOTS ( 'NONE', 3,
 ( #26167, #60353, #94476, #17749, #77697, #36245, #103425, #95050, #18318, #52509, #44104, #13221, #55276, #22162, #12694, #81003, #45778, #56362, #97793, #98895, #28398, #46875, #4310, #96715, #89406, #21070, #79913, #107304, #63145, #105673, #30031, #105107, #80462, #106744, #88856, #38437, #37908, #63682, #98348, #64225, #3226, #72613, #64785, #13769, #47411, #70991, #20521, #73159, #88307, #28956, #36799, #62598, #90494, #37353, #21621, #81533, #55826, #46332, #89946, #4835, #38982, #30597, #29486, #3775, #47953, #2674, #19985, #97246, #54179, #54728, #72090, #12140, #106204, #11599, #71552, #15974, #22712, #101086, #91604, #14331, #92697, #16516 ),
 .UNSPECIFIED., .F., .F.,
 ( 4, 2, 2, 2, 1, 1, 1, 1, 1, 2, 2, 2, 2, 2, 1, 1, 1, 1, 1, 1, 1, 2, 2, 2, 2, 2, 2, 2, 1, 1, 1, 1, 1, 2, 2, 2, 2, 2, 1, 1, 1, 1, 1, 2, 2, 2, 2, 1, 1, 1, 1, 2, 2, 4 ),
 ( 0.000000000000000000, 0.1250000000125275623, 0.1875000000187913851, 0.2187500000219232965, 0.2343750000234892383, 0.2421875000242721954, 0.2460937500246623000, 0.2480468750248588650, 0.2490234375249570642, 0.2495117187750076626, 0.2500000000250582888, 0.3750000000379676290, 0.4375000000444223547, 0.4687500000476496620, 0.4843750000492632046, 0.4921875000500729458, 0.4960937500504778441, 0.4980468750506802933, 0.4990234375507814901, 0.4995117188008350584, 0.4997558594258618703, 0.4998779297383753595, 0.5000000000508888487, 0.5312500000477524686, 0.5625000000446159776, 0.5937500000414795975, 0.6093750000399111855, 0.6171875000391271460, 0.6210937500387376797, 0.6230468750385455001, 0.6240234375384495769, 0.6245117187884015042, 0.6247558594133776344, 0.6248779297258629795, 0.6250000000383483245, 0.6875000000317065263, 0.7187500000283806312, 0.7343750000267115219, 0.7421875000258768562, 0.7460937500254666288, 0.7480468750252686760, 0.7490234375251770826, 0.7495117187751239030, 0.7497558594000971466, 0.7500000000250703902, 0.8125000000181976656, 0.8437500000147613033, 0.8593750000130431221, 0.8671875000121839205, 0.8710937500117614807, 0.8730468750115574217, 0.8740234375114624976, 0.8750000000113676846, 1.000000000000000000 ),
 .UNSPECIFIED. ) ;
#73189 = ORIENTED_EDGE ( 'NONE', *, *, #61343, .F. ) ;
#73190 = CARTESIAN_POINT ( 'NONE',  ( -11.73107767829999837, 1391.121393030069839, 205.1223722441990276 ) ) ;
#73191 = ORIENTED_EDGE ( 'NONE', *, *, #49364, .F. ) ;
#73192 = ORIENTED_EDGE ( 'NONE', *, *, #66450, .T. ) ;
#73193 = CARTESIAN_POINT ( 'NONE',  ( -4.026614517785000125, 1516.699825673279975, 210.8361802174170236 ) ) ;
#73194 = CARTESIAN_POINT ( 'NONE',  ( -8.673948557444399299, 1448.059622049680002, 212.1973933741120106 ) ) ;
#73196 = LINE ( 'NONE', #49659, #88366 ) ;
#73195 = CARTESIAN_POINT ( 'NONE',  ( 2.298369469825000344, 1516.779243033999819, 212.3734572960470075 ) ) ;
#73197 = CARTESIAN_POINT ( 'NONE',  ( -16.37744738580000003, 1440.438196244339906, 190.1083942918979801 ) ) ;
#73198 = B_SPLINE_CURVE_WITH_KNOTS ( 'NONE', 3,
 ( #8388, #22, #33583, #40345, #25733, #109226 ),
 .UNSPECIFIED., .F., .F.,
 ( 4, 2, 4 ),
 ( 0.000000000000000000, 0.5000000000000000000, 1.000000000000000000 ),
 .UNSPECIFIED. ) ;
#73199 = DIRECTION ( 'NONE',  ( 0.000000000000000000, 0.000000000000000000, -1.000000000000000000 ) ) ;
#73200 = B_SPLINE_SURFACE_WITH_KNOTS ( 'NONE', 5, 5, ( 
 ( #12108, #19953, #46301, #97765, #21037, #72583, #21593, #22131, #38948 ),
 ( #90462, #22684, #4803, #13188, #49591, #89914, #56883, #82632, #73128 ),
 ( #64192, #74791, #13739, #98314, #57992, #92126, #49044, #39524, #56330 ),
 ( #15402, #47923, #30565, #40620, #66403, #55798, #108934, #6470, #47376 ),
 ( #32222, #14303, #23801, #57453, #40070, #82059, #107270, #91014, #91580 ),
 ( #30001, #106711, #48493, #81501, #5924, #74249, #64755, #100522, #98866 ),
 ( #5364, #83723, #73699, #107825, #31113, #14853, #65293, #99406, #108380 ),
 ( #31662, #83180, #7018, #65842, #41175, #99961, #23254, #101058, #299 ),
 ( #58542, #84810, #68056, #50146, #24356, #101605, #7568, #15945, #59097 ),
 ( #84273, #92668, #18163, #41723, #25448, #51227, #75883, #33865, #32766 ),
 ( #93221, #66949, #26567, #60763, #17593, #8109, #24890, #110031, #94886 ),
 ( #9235, #34971, #33306, #77542, #85932, #67501, #42276, #846, #93752 ) ),
 .UNSPECIFIED., .F., .F., .F.,
 ( 6, 3, 3, 6 ),
 ( 6, 3, 6 ),
 ( 29.56117038800000074, 40.55923757500000448, 46.18177991610000532, 51.15186658319999680 ),
 ( 0.000000000000000000, 1.000000000000000000, 2.000000000000000000 ),
 .UNSPECIFIED. ) ;
#73201 = ORIENTED_EDGE ( 'NONE', *, *, #41183, .F. ) ;
#73202 = CARTESIAN_POINT ( 'NONE',  ( -26.03017368029999901, 1436.520442997449891, 136.8941006876979998 ) ) ;
#73203 = CARTESIAN_POINT ( 'NONE',  ( -1.708092304294999808, 1516.523379810429788, 201.4131002843170108 ) ) ;
#73204 = AXIS2_PLACEMENT_3D ( 'NONE', #87630, #37771, #38850 ) ;
#73205 = CARTESIAN_POINT ( 'NONE',  ( 1.546867617820790075, 1416.839692126689897, 190.2222510973109877 ) ) ;
#73206 = CARTESIAN_POINT ( 'NONE',  ( -18.50881575315199967, 1384.530072707220143, 201.3187559258710166 ) ) ;
#73207 = CARTESIAN_POINT ( 'NONE',  ( -27.82281737747349837, 1416.493833913160188, 270.3515857537420288 ) ) ;
#73208 = CARTESIAN_POINT ( 'NONE',  ( -5.889293977349999487, 1482.137417484389971, 204.3352348937889928 ) ) ;
#73209 = CARTESIAN_POINT ( 'NONE',  ( -2.551337388519999916, 1397.989667269630218, 196.2720235379979954 ) ) ;
#73211 = ORIENTED_EDGE ( 'NONE', *, *, #103630, .F. ) ;
#73210 = CARTESIAN_POINT ( 'NONE',  ( -8.123413751219246137, 1364.885445916480421, 208.3718459617061285 ) ) ;
#73212 = ORIENTED_EDGE ( 'NONE', *, *, #51936, .F. ) ;
#73213 = CARTESIAN_POINT ( 'NONE',  ( 32.91700288581939304, 1464.589777195947590, 269.2964102291147697 ) ) ;
#73214 = CARTESIAN_POINT ( 'NONE',  ( -6.790918657024139549, 1522.051704408389924, 184.0243675267330161 ) ) ;
#73215 = CARTESIAN_POINT ( 'NONE',  ( -14.59020679048630065, 1436.244981818430006, 149.8726110424499893 ) ) ;
#73216 = CARTESIAN_POINT ( 'NONE',  ( -0.03728987521009100026, 1409.697654410689893, 185.1798867859249924 ) ) ;
#73218 = CARTESIAN_POINT ( 'NONE',  ( 6.564578685215000320, 1517.199196846569976, 210.8299485595169926 ) ) ;
#73217 = VECTOR ( 'NONE', #86469, 1000.000000000000114 ) ;
#73219 = DIRECTION ( 'NONE',  ( -9.341989762165448955E-47, 1.000000000000000000, -1.836970198721029688E-16 ) ) ;
#73220 = CARTESIAN_POINT ( 'NONE',  ( 3.034663161748390348, 1440.440203176670138, 157.2490260270419924 ) ) ;
#73221 = CIRCLE ( 'NONE', #35643, 1.749999999999996891 ) ;
#73222 = CARTESIAN_POINT ( 'NONE',  ( 6.844748814533139658, 1439.290426551219753, 215.8329238270310100 ) ) ;
#73223 = CARTESIAN_POINT ( 'NONE',  ( 12.22173834910000068, 1416.311719782429918, 223.5326879811980234 ) ) ;
#73224 = CARTESIAN_POINT ( 'NONE',  ( 12.37688904839999893, 1445.074465566569870, 186.3522953654979801 ) ) ;
#73225 = CARTESIAN_POINT ( 'NONE',  ( -3.463767296015000330, 1517.014196759610059, 207.4190915607570105 ) ) ;
#73226 = ORIENTED_EDGE ( 'NONE', *, *, #27140, .F. ) ;
#73227 = DIRECTION ( 'NONE',  ( -0.4035202328300252494, 0.000000000000000000, 0.9149707217702663931 ) ) ;
#73228 = CARTESIAN_POINT ( 'NONE',  ( -23.83739627443888409, 1446.557502124605435, 213.8096630186308573 ) ) ;
#73229 = ORIENTED_EDGE ( 'NONE', *, *, #14108, .F. ) ;
#73231 = B_SPLINE_CURVE_WITH_KNOTS ( 'NONE', 5,
 ( #38265, #39376, #108227, #55653, #20903, #13045 ),
 .UNSPECIFIED., .F., .F.,
 ( 6, 6 ),
 ( -1.999999915403020134, 0.000000000000000000 ),
 .UNSPECIFIED. ) ;
#73230 = LINE ( 'NONE', #106813, #21306 ) ;
#73232 = CARTESIAN_POINT ( 'NONE',  ( 24.18662061371099981, 1452.052842388240151, 136.8071046221860172 ) ) ;
#73233 = CARTESIAN_POINT ( 'NONE',  ( -4.122298849506555563, 1439.983387333591963, 185.4581667231335302 ) ) ;
#73234 = CARTESIAN_POINT ( 'NONE',  ( 2.431412526649999961, 1428.647745098929818, 149.4227846719979880 ) ) ;
#73235 = CARTESIAN_POINT ( 'NONE',  ( 22.51990846810000235, 1410.619212186030154, 206.2037071705079825 ) ) ;
#73236 = B_SPLINE_CURVE_WITH_KNOTS ( 'NONE', 5,
 ( #58282, #100804, #15142, #15679, #49883, #101342 ),
 .UNSPECIFIED., .F., .F.,
 ( 6, 6 ),
 ( 0.000000000000000000, 1.000000000000000000 ),
 .UNSPECIFIED. ) ;
#73237 = CARTESIAN_POINT ( 'NONE',  ( -24.89775108082510968, 1442.835550636541257, 210.5176539979092638 ) ) ;
#73238 = CARTESIAN_POINT ( 'NONE',  ( -14.06292235172921679, 1379.592324727026835, 211.7786485450617135 ) ) ;
#73239 = CYLINDRICAL_SURFACE ( 'NONE', #102162, 3.999999999999991118 ) ;
#73240 = DIRECTION ( 'NONE',  ( 0.000000000000000000, 0.000000000000000000, 1.000000000000000000 ) ) ;
#73241 = CIRCLE ( 'NONE', #108970, 1.999999999999999556 ) ;
#73242 = DIRECTION ( 'NONE',  ( 1.000000000000000000, 0.000000000000000000, 0.000000000000000000 ) ) ;
#73243 = CARTESIAN_POINT ( 'NONE',  ( 3.263521904354999670, 1516.676340709600026, 214.8942497445370066 ) ) ;
#73244 = ORIENTED_EDGE ( 'NONE', *, *, #76661, .F. ) ;
#73245 = CARTESIAN_POINT ( 'NONE',  ( 7.709178328070479758, 1516.539903203899939, 206.5651024190640044 ) ) ;
#73246 = CARTESIAN_POINT ( 'NONE',  ( -4.161605046760000093, 1448.983014852180077, 185.0801900870980035 ) ) ;
#73247 = EDGE_CURVE ( 'NONE', #29545, #26775, #109589, .T. ) ;
#73248 = CARTESIAN_POINT ( 'NONE',  ( 0.3220030984499608340, 1452.978637988592709, 183.2674086474032720 ) ) ;
#73249 = EDGE_CURVE ( 'NONE', #64698, #2577, #6007, .T. ) ;
#73250 = FACE_OUTER_BOUND ( 'NONE', #37384, .T. ) ;
#73251 = CARTESIAN_POINT ( 'NONE',  ( 11.60004869885203682, 1426.339115466829298, 138.4394687558738042 ) ) ;
#73252 = CARTESIAN_POINT ( 'NONE',  ( -16.06428795287819966, 1416.913060341709979, 209.3174441336760196 ) ) ;
#73253 = CARTESIAN_POINT ( 'NONE',  ( -2.500000000000000000, 1430.722531270429954, 157.4400244878979720 ) ) ;
#73254 = ADVANCED_FACE ( 'NONE', ( #100063 ), #86619, .F. ) ;
#73255 = CARTESIAN_POINT ( 'NONE',  ( -3.047096304819949975, 1454.406456363820098, 199.0892365841679919 ) ) ;
#73256 = CARTESIAN_POINT ( 'NONE',  ( -5.461771172978369628E-06, 1406.917628766249891, 222.1218527342900018 ) ) ;
#73258 = EDGE_CURVE ( 'NONE', #96281, #53641, #107392, .T. ) ;
#73257 = CARTESIAN_POINT ( 'NONE',  ( 34.44461235088070339, 1440.913060385129938, 249.8013572737719983 ) ) ;
#73259 = DIRECTION ( 'NONE',  ( 1.000000000000000000, 0.000000000000000000, 0.000000000000000000 ) ) ;
#73260 = FACE_OUTER_BOUND ( 'NONE', #25759, .T. ) ;
#73261 = ORIENTED_EDGE ( 'NONE', *, *, #48911, .T. ) ;
#73262 = VERTEX_POINT ( 'NONE', #95266 ) ;
#73263 = CARTESIAN_POINT ( 'NONE',  ( 11.33998819790270041, 1479.686981350909946, 209.1734062345460075 ) ) ;
#73264 = PLANE ( 'NONE',  #101475 ) ;
#73265 = CARTESIAN_POINT ( 'NONE',  ( -2.349897617149999896, 1443.007235233090114, 200.3879200387590060 ) ) ;
#73266 = CYLINDRICAL_SURFACE ( 'NONE', #99181, 0.9999999999999982236 ) ;
#73267 = DIRECTION ( 'NONE',  ( -3.697785493223495027E-32, -1.000000000000000000, 1.836970198721029688E-16 ) ) ;
#73268 = CARTESIAN_POINT ( 'NONE',  ( -10.96015512746500065, 1514.690994518219895, 193.2119433744669834 ) ) ;
#73269 = CARTESIAN_POINT ( 'NONE',  ( -52.39341264816799537, 1383.808018661449978, 266.2425820643259726 ) ) ;
#73270 = CARTESIAN_POINT ( 'NONE',  ( -3.558864061465000006, 1511.483345606789953, 201.2317265620570197 ) ) ;
#73271 = CARTESIAN_POINT ( 'NONE',  ( -13.29290641609999923, 1434.997135647470031, 194.5463675775980334 ) ) ;
#73272 = ADVANCED_FACE ( 'NONE', ( #64437 ), #96926, .F. ) ;
#73274 =( BOUNDED_SURFACE ( )  B_SPLINE_SURFACE ( 3, 2, ( 
 ( #55545, #12954, #29764 ),
 ( #96993, #30313, #80732 ),
 ( #47135, #7190, #72349 ),
 ( #106478, #71826, #20256 ) ),
 .UNSPECIFIED., .F., .F., .T. ) 
 B_SPLINE_SURFACE_WITH_KNOTS ( ( 4, 4 ),
 ( 3, 3 ),
 ( 0.000000000000000000, 0.0002960034161023844057 ),
 ( 0.000000000000000000, 1.000000000000000000 ),
 .UNSPECIFIED. ) 
 GEOMETRIC_REPRESENTATION_ITEM ( )  RATIONAL_B_SPLINE_SURFACE ( (
 ( 1.000000000000000000, 0.8070209408749940971, 1.000000000000000000),
 ( 1.000000000000000000, 0.8071723757218307593, 1.000000000000000000),
 ( 1.000000000000000000, 0.8072480346917725313, 1.000000000000000000),
 ( 1.000000000000000000, 0.8072480644198083422, 1.000000000000000000) ) ) 
 REPRESENTATION_ITEM ( '' )  SURFACE ( )  );
#73273 = CARTESIAN_POINT ( 'NONE',  ( -11.43788434358669903, 1501.179491375600037, 208.6405304903099989 ) ) ;
#73275 = CARTESIAN_POINT ( 'NONE',  ( 1.783238944200000065, 1465.101364307329732, 235.5168545023980187 ) ) ;
#73277 = VERTEX_POINT ( 'NONE', #21270 ) ;
#73276 = FACE_OUTER_BOUND ( 'NONE', #90055, .T. ) ;
#73278 = CARTESIAN_POINT ( 'NONE',  ( -0.3197736170449999582, 1452.655606759629791, 183.2748911062979857 ) ) ;
#73279 = AXIS2_PLACEMENT_3D ( 'NONE', #22474, #32567, #93006 ) ;
#73280 = CARTESIAN_POINT ( 'NONE',  ( -14.07327828060000030, 1379.838870826219818, 214.5512279352489884 ) ) ;
#73281 = CARTESIAN_POINT ( 'NONE',  ( -3.046862472289999513, 1475.471993788190048, 198.8673669194990339 ) ) ;
#73283 = ORIENTED_EDGE ( 'NONE', *, *, #108925, .F. ) ;
#73282 = CARTESIAN_POINT ( 'NONE',  ( -18.15372975567069957, 1416.529254608160045, 209.0703203373900010 ) ) ;
#73284 = CARTESIAN_POINT ( 'NONE',  ( -20.43379687057499794, 1466.940231432759902, 211.2182850803170027 ) ) ;
#73285 = EDGE_LOOP ( 'NONE', ( #46599, #39627, #44098 ) ) ;
#73286 = PRODUCT_DEFINITION_SHAPE ( 'NONE', 'NONE',  #41841 ) ;
#73287 = EDGE_CURVE ( 'NONE', #105413, #76827, #25472, .T. ) ;
#73288 = CARTESIAN_POINT ( 'NONE',  ( -11.63740560221349973, 1390.801072237219842, 213.8478914447200054 ) ) ;
#73289 = CARTESIAN_POINT ( 'NONE',  ( -3.912777227685780179, 1515.493283046529996, 205.6567642959410023 ) ) ;
#73290 = DIRECTION ( 'NONE',  ( 0.000000000000000000, 6.123233995736769734E-17, 1.000000000000000000 ) ) ;
#73291 = CIRCLE ( 'NONE', #50039, 0.5000000000000000000 ) ;
#73292 = ADVANCED_FACE ( 'NONE', ( #89057 ), #39386, .T. ) ;
#73293 = CARTESIAN_POINT ( 'NONE',  ( -5.534112078819999780, 1464.371868428389917, 199.5915707823590139 ) ) ;
#73294 = CARTESIAN_POINT ( 'NONE',  ( 1.909779004914692990, 1526.107876515966382, 177.3667160767706150 ) ) ;
#73295 = CARTESIAN_POINT ( 'NONE',  ( 20.97480781879999867, 1494.611541218489947, 207.0969001841590114 ) ) ;
#73296 = CARTESIAN_POINT ( 'NONE',  ( 9.328875054663598121, 1409.238831882729755, 197.4315850328979707 ) ) ;
#73297 = CARTESIAN_POINT ( 'NONE',  ( 18.02092397397800028, 1424.326467398671866, 225.2005593169499775 ) ) ;
#73298 = CYLINDRICAL_SURFACE ( 'NONE', #91146, 2.000000000000003109 ) ;
#73299 = CARTESIAN_POINT ( 'NONE',  ( -9.786977751178733698, 1517.051704408389924, 191.2793932888540951 ) ) ;
#73300 = CARTESIAN_POINT ( 'NONE',  ( 26.45259648960871601, 1507.993349550278708, 202.6659236194934124 ) ) ;
#73301 = VECTOR ( 'NONE', #18995, 1000.000000000000114 ) ;
#73302 = CARTESIAN_POINT ( 'NONE',  ( -2.642710937080679834, 1449.302916809479939, 183.9132731832050069 ) ) ;
#73303 = VERTEX_POINT ( 'NONE', #55480 ) ;
#73304 = ORIENTED_EDGE ( 'NONE', *, *, #50153, .T. ) ;
#73305 = CARTESIAN_POINT ( 'NONE',  ( 18.00465857451067819, 1523.390106123591067, 238.0296012445054998 ) ) ;
#73306 = CARTESIAN_POINT ( 'NONE',  ( 17.74781233178610051, 1458.373075302629786, 228.4006037624550061 ) ) ;
#73307 = CARTESIAN_POINT ( 'NONE',  ( -11.57148588749999973, 1434.949327167670162, 151.3949104721980063 ) ) ;
#73308 = CARTESIAN_POINT ( 'NONE',  ( -2.205916257146450025E-10, 1466.549663538289906, 243.4496450869259832 ) ) ;
#73309 = CARTESIAN_POINT ( 'NONE',  ( -20.59250019004760190, 1507.621919103199843, 190.3962728046239761 ) ) ;
#73310 = CARTESIAN_POINT ( 'NONE',  ( -14.57096372540000040, 1420.584117712579882, 213.1076017662689992 ) ) ;
#73311 = CARTESIAN_POINT ( 'NONE',  ( -109.1427469879999990, 1386.396569596549853, 311.0572058512590274 ) ) ;
#73312 = CARTESIAN_POINT ( 'NONE',  ( -7.536818064318620003, 1511.326458810320219, 215.2928205442640035 ) ) ;
#73313 = CARTESIAN_POINT ( 'NONE',  ( -9.690020260109999839, 1366.026910387849966, 207.6218459616989946 ) ) ;
#73314 = CARTESIAN_POINT ( 'NONE',  ( 9.374720191569998917, 1498.531797635389921, 228.6938383677990316 ) ) ;
#73315 = CARTESIAN_POINT ( 'NONE',  ( -20.59684415639999955, 1507.762623717429960, 190.9355247909979880 ) ) ;
#73316 = CARTESIAN_POINT ( 'NONE',  ( 4.610079833424999940, 1516.713079096360161, 207.9883289669969884 ) ) ;
#73317 = CARTESIAN_POINT ( 'NONE',  ( -9.983087554349619808, 1446.969730184950095, 211.7543459487629889 ) ) ;
#73318 = AXIS2_PLACEMENT_3D ( 'NONE', #32659, #102590, #85815 ) ;
#73319 = CARTESIAN_POINT ( 'NONE',  ( -13.89810820305640071, 1435.230276586210039, 149.5229838337619981 ) ) ;
#73320 = CARTESIAN_POINT ( 'NONE',  ( -8.579394357329999110, 1384.984320043210118, 218.6689291461190123 ) ) ;
#73321 = B_SPLINE_SURFACE_WITH_KNOTS ( 'NONE', 5, 4, ( 
 ( #39533, #6478, #48502, #31121, #13200 ),
 ( #47390, #99970, #49600, #58001, #66413 ),
 ( #92135, #5932, #74258, #81511, #108390 ),
 ( #89925, #22142, #56342, #83733, #5374 ),
 ( #90474, #4814, #32774, #13749, #57461 ),
 ( #47935, #23263, #31671, #65852, #98324 ) ),
 .UNSPECIFIED., .F., .F., .F.,
 ( 6, 6 ),
 ( 5, 5 ),
 ( 0.000000000000000000, 111.1101480259999903 ),
 ( 25.81581217359999769, 39.03307591160000101 ),
 .UNSPECIFIED. ) ;
#73322 = CARTESIAN_POINT ( 'NONE',  ( 10.87683910581177216, 1427.022019987679414, 224.8651914639115432 ) ) ;
#73323 = CARTESIAN_POINT ( 'NONE',  ( 7.366488175266259653, 1425.086169979620081, 212.5226571148190260 ) ) ;
#73324 = PRODUCT_RELATED_PRODUCT_CATEGORY ( 'part', '', ( #22290 ) ) ;
#73325 = EDGE_LOOP ( 'NONE', ( #62799, #76635, #22458, #39728, #92655 ) ) ;
#73326 = CARTESIAN_POINT ( 'NONE',  ( 33.60183515729999471, 1438.777037861339977, 248.0844435631979650 ) ) ;
#73327 = FACE_OUTER_BOUND ( 'NONE', #39886, .T. ) ;
#73329 = CARTESIAN_POINT ( 'NONE',  ( -15.25688968024340042, 1512.464953430870082, 222.2583362424209952 ) ) ;
#73328 = CARTESIAN_POINT ( 'NONE',  ( 1.491332443579999945, 1469.880992466429916, 182.7373208613979898 ) ) ;
#73330 = CARTESIAN_POINT ( 'NONE',  ( -23.40570496174960269, 1412.384583249233174, 270.0161671065278028 ) ) ;
#73331 = VECTOR ( 'NONE', #87534, 1000.000000000000227 ) ;
#73332 = CARTESIAN_POINT ( 'NONE',  ( -25.42953928600000069, 1428.064052528830189, 238.1443913133980175 ) ) ;
#73333 = DIRECTION ( 'NONE',  ( -0.6396908461234346310, -0.7404633132259050843, 0.2061788135391205146 ) ) ;
#73334 = CARTESIAN_POINT ( 'NONE',  ( -1.247677516857949989E-10, 1452.913060387320002, 152.5211338456990120 ) ) ;
#73335 = CARTESIAN_POINT ( 'NONE',  ( 30.24884739909999709, 1451.401555985529967, 136.0545012092980244 ) ) ;
#73336 = ORIENTED_EDGE ( 'NONE', *, *, #61669, .F. ) ;
#73337 = CARTESIAN_POINT ( 'NONE',  ( -3.286480964850000408, 1456.341185808290220, 218.0120306903490075 ) ) ;
#73338 = DIRECTION ( 'NONE',  ( 0.000000000000000000, 0.000000000000000000, 1.000000000000000000 ) ) ;
#73339 = CARTESIAN_POINT ( 'NONE',  ( 8.956493609840000758, 1509.358276789029787, 238.0100333225980194 ) ) ;
#73340 = ORIENTED_EDGE ( 'NONE', *, *, #51036, .T. ) ;
#73341 = ORIENTED_EDGE ( 'NONE', *, *, #3657, .T. ) ;
#73342 = CARTESIAN_POINT ( 'NONE',  ( -23.00221949109999997, 1384.956020836430071, 202.3857052141389943 ) ) ;
#73343 = CARTESIAN_POINT ( 'NONE',  ( -22.91552897997099691, 1409.723198887639910, 208.8960376927099958 ) ) ;
#73344 = EDGE_CURVE ( 'NONE', #25549, #102491, #84193, .T. ) ;
#73345 = VERTEX_POINT ( 'NONE', #63346 ) ;
#73346 = CARTESIAN_POINT ( 'NONE',  ( 4.119399112420410347, 1508.879003890470131, 204.7521254745670092 ) ) ;
#73347 = DIRECTION ( 'NONE',  ( 0.000000000000000000, 1.000000000000000000, -1.836970198721029688E-16 ) ) ;
#73348 = EDGE_CURVE ( 'NONE', #51048, #14195, #97465, .T. ) ;
#73349 = CARTESIAN_POINT ( 'NONE',  ( -3.198241401019999763, 1489.061078771829898, 235.9665387607980165 ) ) ;
#73350 = DIRECTION ( 'NONE',  ( 1.000000000000000000, 0.000000000000000000, 0.000000000000000000 ) ) ;
#73351 = ORIENTED_EDGE ( 'NONE', *, *, #3139, .F. ) ;
#73352 = CARTESIAN_POINT ( 'NONE',  ( 11.73652925620000076, 1426.280330920429833, 144.1708004945979837 ) ) ;
#73353 = CARTESIAN_POINT ( 'NONE',  ( -12.74111629470790064, 1416.830086716310007, 221.9830696278120001 ) ) ;
#73354 = CARTESIAN_POINT ( 'NONE',  ( -7.096551626949999303, 1426.600319239269993, 204.6398483329990086 ) ) ;
#73355 = CARTESIAN_POINT ( 'NONE',  ( 7.712490952985000980, 1516.666407245520077, 204.5049844236870058 ) ) ;
#73356 = EDGE_LOOP ( 'NONE', ( #76602, #36719, #78290, #78016 ) ) ;
#73357 = CARTESIAN_POINT ( 'NONE',  ( 9.855039225750559240, 1481.788109175460022, 215.6330005400349705 ) ) ;
#73358 = AXIS2_PLACEMENT_3D ( 'NONE', #76418, #60755, #94879 ) ;
#73359 = ADVANCED_FACE ( 'NONE', ( #79580 ), #19718, .T. ) ;
#73360 = DIRECTION ( 'NONE',  ( 0.9750097311986455351, 0.1381407795329493426, -0.1739918075599369285 ) ) ;
#73361 = ORIENTED_EDGE ( 'NONE', *, *, #51331, .T. ) ;
#73362 = VERTEX_POINT ( 'NONE', #72283 ) ;
#73363 = CARTESIAN_POINT ( 'NONE',  ( -11.00403485397939995, 1481.586315828709985, 208.5475605672099846 ) ) ;
#73364 = CARTESIAN_POINT ( 'NONE',  ( 4.987078422726499483, 1508.551704408389924, 205.6342535031670025 ) ) ;
#73365 = CARTESIAN_POINT ( 'NONE',  ( -22.64306613040000116, 1409.703773680230142, 208.6811978374589955 ) ) ;
#73366 = CARTESIAN_POINT ( 'NONE',  ( -4.567580137773889604, 1425.583738731856783, 186.2099746554915782 ) ) ;
#73367 = CARTESIAN_POINT ( 'NONE',  ( 11.32581438617719982, 1502.327464439309779, 214.9380970868279803 ) ) ;
#73368 = CIRCLE ( 'NONE', #80493, 1.999999999999999556 ) ;
#73369 = CARTESIAN_POINT ( 'NONE',  ( 8.768419210700001187, 1421.106171289960002, 196.5082349784990186 ) ) ;
#73370 = CARTESIAN_POINT ( 'NONE',  ( 0.6402605648741300781, 1475.143224049549872, 220.5254527812860204 ) ) ;
#73371 = CARTESIAN_POINT ( 'NONE',  ( 19.02704169900689735, 1456.915441405320053, 225.6706379604710264 ) ) ;
#73372 = CARTESIAN_POINT ( 'NONE',  ( -10.98084453577630093, 1433.016921785290151, 151.7694248368179899 ) ) ;
#73373 = CARTESIAN_POINT ( 'NONE',  ( 0.005542294731646350836, 1408.915806758429653, 231.8992816016082941 ) ) ;
#73375 = CARTESIAN_POINT ( 'NONE',  ( -106.0930553259309903, 1391.335640847810055, 307.0497040399930029 ) ) ;
#73374 = CARTESIAN_POINT ( 'NONE',  ( 30.11859361092137632, 1525.055402519434438, 196.5532433872490969 ) ) ;
#73376 = CARTESIAN_POINT ( 'NONE',  ( 11.07919842396059984, 1425.821831854960010, 206.4952777197320017 ) ) ;
#73377 = CARTESIAN_POINT ( 'NONE',  ( -25.58488017426969918, 1509.794763074989987, 223.0410912172320081 ) ) ;
#73378 = ADVANCED_FACE ( 'NONE', ( #20193 ), #28610, .F. ) ;
#73379 = CARTESIAN_POINT ( 'NONE',  ( 4.897375497219999652, 1432.353341358199941, 150.0655110971979980 ) ) ;
#73380 = ORIENTED_EDGE ( 'NONE', *, *, #73348, .F. ) ;
#73381 = DIRECTION ( 'NONE',  ( 0.000000000000000000, 0.000000000000000000, 1.000000000000000000 ) ) ;
#73382 = CIRCLE ( 'NONE', #80567, 1.000000000000000000 ) ;
#73383 = CARTESIAN_POINT ( 'NONE',  ( -17.00293377828755581, 1417.375270068509735, 206.8726622690845431 ) ) ;
#73384 = CARTESIAN_POINT ( 'NONE',  ( -81.83538110834038548, 1384.989206256060015, 305.0088236927869616 ) ) ;
#73385 = EDGE_CURVE ( 'NONE', #25549, #74855, #29450, .T. ) ;
#73386 = CARTESIAN_POINT ( 'NONE',  ( -10.77443953700000101, 1387.520226337789836, 201.1700256806890081 ) ) ;
#73387 = CARTESIAN_POINT ( 'NONE',  ( -3.527569048119670203, 1486.518325592330029, 181.8541486797999767 ) ) ;
#73389 = ORIENTED_EDGE ( 'NONE', *, *, #8584, .F. ) ;
#73388 = CARTESIAN_POINT ( 'NONE',  ( -15.57735599724670017, 1420.358456224219935, 210.5575541888260034 ) ) ;
#73390 = EDGE_CURVE ( 'NONE', #78921, #67457, #50888, .T. ) ;
#73391 = CARTESIAN_POINT ( 'NONE',  ( 3.075808390909999801, 1430.545926202089959, 217.6856249740289968 ) ) ;
#73392 = CARTESIAN_POINT ( 'NONE',  ( -0.8288084222790000899, 1440.444625599219989, 150.6821045058979962 ) ) ;
#73393 = CARTESIAN_POINT ( 'NONE',  ( -13.79577745739999983, 1416.837309312929847, 221.9091491129979943 ) ) ;
#73394 = CARTESIAN_POINT ( 'NONE',  ( 11.92878151090000038, 1433.442688111030066, 149.9099994665980091 ) ) ;
#73395 = CARTESIAN_POINT ( 'NONE',  ( 28.52406123160000107, 1451.758636106830181, 255.3819207682979595 ) ) ;
#73396 = CARTESIAN_POINT ( 'NONE',  ( 12.31551432482880060, 1414.913060387399810, 198.2593941373620225 ) ) ;
#73397 = CARTESIAN_POINT ( 'NONE',  ( 1.145281290628310078, 1458.110497838100173, 199.6352755006269888 ) ) ;
#73398 = CARTESIAN_POINT ( 'NONE',  ( 8.539235273727440401, 1425.244712013389972, 194.2347455539940029 ) ) ;
#73399 = CARTESIAN_POINT ( 'NONE',  ( 13.47673469449999928, 1422.102502196930118, 228.8541257092979890 ) ) ;
#73400 = EDGE_CURVE ( 'NONE', #56950, #63442, #58773, .T. ) ;
#73401 = DIRECTION ( 'NONE',  ( -5.980589973904019347E-17, 1.000000000000000000, -1.736889445713099699E-16 ) ) ;
#73402 = AXIS2_PLACEMENT_3D ( 'NONE', #18589, #19712, #9649 ) ;
#73403 = CARTESIAN_POINT ( 'NONE',  ( 12.17073567488309926, 1499.730396444349708, 205.6506566649260321 ) ) ;
#73404 = CARTESIAN_POINT ( 'NONE',  ( -18.39618391109999607, 1410.051843682230128, 223.6762995290979745 ) ) ;
#73405 = CARTESIAN_POINT ( 'NONE',  ( 1.548232229107720181, 1416.321686226080146, 190.3132320445130006 ) ) ;
#73406 = CARTESIAN_POINT ( 'NONE',  ( 20.93328349789999976, 1508.014070803829782, 190.4233152825979971 ) ) ;
#73407 = ADVANCED_FACE ( 'NONE', ( #15084 ), #16805, .T. ) ;
#73408 = B_SPLINE_CURVE_WITH_KNOTS ( 'NONE', 5,
 ( #16487, #8108, #24889, #59096, #109488, #51226 ),
 .UNSPECIFIED., .F., .F.,
 ( 6, 6 ),
 ( 0.000000000000000000, 1.000000000000000000 ),
 .UNSPECIFIED. ) ;
#73409 = FACE_OUTER_BOUND ( 'NONE', #108603, .T. ) ;
#73410 = CARTESIAN_POINT ( 'NONE',  ( -17.60627488151730091, 1410.895757528699960, 193.4350316887010024 ) ) ;
#73411 = CARTESIAN_POINT ( 'NONE',  ( 1.125259334100000119, 1515.531689041389882, 205.0307428966389978 ) ) ;
#73412 = CARTESIAN_POINT ( 'NONE',  ( -31.34137657934000387, 1523.481610426287716, 221.9025654077414345 ) ) ;
#73413 = CARTESIAN_POINT ( 'NONE',  ( -9.771923697420890065, 1448.872169750079820, 190.8346798121849872 ) ) ;
#73414 = CARTESIAN_POINT ( 'NONE',  ( -9.790177377270000036, 1414.971287085229960, 222.6285949133980182 ) ) ;
#73415 = CARTESIAN_POINT ( 'NONE',  ( 0.2093852927156230059, 1457.693901257390280, 183.0520252844249853 ) ) ;
#73416 = CARTESIAN_POINT ( 'NONE',  ( -11.43679079880000060, 1409.312441922530070, 199.2442402772080072 ) ) ;
#73417 = CARTESIAN_POINT ( 'NONE',  ( -14.63039435740000016, 1416.519106787730152, 198.5326739117980139 ) ) ;
#73418 = AXIS2_PLACEMENT_3D ( 'NONE', #12521, #56732, #106576 ) ;
#73419 = CARTESIAN_POINT ( 'NONE',  ( -28.18627406427190252, 1509.319237329340012, 210.8542828833879810 ) ) ;
#73420 = CARTESIAN_POINT ( 'NONE',  ( 11.94148329819999965, 1433.615059856560038, 147.6243649254979857 ) ) ;
#73421 = CARTESIAN_POINT ( 'NONE',  ( -33.91369120210140409, 1435.681798817159915, 134.0999999980979851 ) ) ;
#73422 = CARTESIAN_POINT ( 'NONE',  ( 11.73542121899999913, 1441.459447619979983, 188.0641116183980159 ) ) ;
#73423 = EDGE_LOOP ( 'NONE', ( #17430, #60674, #12027 ) ) ;
#73425 = EDGE_CURVE ( 'NONE', #53764, #50471, #102950, .T. ) ;
#73424 = CARTESIAN_POINT ( 'NONE',  ( -17.78112617923709138, 1523.954924407802537, 180.4163696555889658 ) ) ;
#73426 = CARTESIAN_POINT ( 'NONE',  ( 2.008229241910000074, 1477.194275679390103, 198.7982270564990017 ) ) ;
#73427 = CARTESIAN_POINT ( 'NONE',  ( -104.5246723904855770, 1380.568180134393060, 307.6284135004361247 ) ) ;
#73428 = CARTESIAN_POINT ( 'NONE',  ( -10.99857149249999999, 1492.065342166190021, 207.0970266674490006 ) ) ;
#73429 = ADVANCED_FACE ( 'NONE', ( #59887 ), #40564, .T. ) ;
#73430 = CARTESIAN_POINT ( 'NONE',  ( 4.967684365510000255, 1469.890599266690060, 189.7939106698990201 ) ) ;
#73431 = CARTESIAN_POINT ( 'NONE',  ( -15.57748978299999898, 1507.212883763329955, 192.6976421578980023 ) ) ;
#73432 = CARTESIAN_POINT ( 'NONE',  ( 45.47494684930080666, 1437.303802531743713, 268.9792534891967648 ) ) ;
#73433 = B_SPLINE_CURVE_WITH_KNOTS ( 'NONE', 3,
 ( #79083, #11319, #34843, #104263, #61735, #53900, #69034, #95859, #53327, #105371, #62291, #44936, #2390, #88035, #79631, #2935, #71248, #55528, #97515, #39251, #80717, #71811, #11859, #12397, #29210, #37609, #4026, #12940, #105931 ),
 .UNSPECIFIED., .F., .F.,
 ( 4, 2, 2, 1, 1, 2, 2, 2, 2, 2, 2, 2, 1, 2, 2, 4 ),
 ( 0.000000000000000000, 0.1250000000000399958, 0.1875000000000586753, 0.2187500000000699718, 0.2343749999999852340, 0.2421874999998512579, 0.2499999999997172817, 0.3750000000002788880, 0.4375000000005585532, 0.5000000000008382184, 0.6250000000009311441, 0.6875000000011701751, 0.7187500000011074475, 0.7343750000010753620, 0.7500000000010433876, 1.000000000000000000 ),
 .UNSPECIFIED. ) ;
#73434 = CARTESIAN_POINT ( 'NONE',  ( 20.50343491230000126, 1453.154616238729886, 210.0312230869269854 ) ) ;
#73435 = CARTESIAN_POINT ( 'NONE',  ( -86.83071232126310690, 1384.625104402849956, 307.5136755095109606 ) ) ;
#73436 = CARTESIAN_POINT ( 'NONE',  ( -60.12142991202459541, 1385.061945964109782, 244.2500411141640200 ) ) ;
#73437 = CARTESIAN_POINT ( 'NONE',  ( -12.10212147083699996, 1491.001746246500034, 207.1149663066109952 ) ) ;
#73438 = CARTESIAN_POINT ( 'NONE',  ( -4.105525334182019925, 1508.551704408389924, 204.7297663225739939 ) ) ;
#73439 = EDGE_CURVE ( 'NONE', #77078, #62097, #28071, .T. ) ;
#73440 = CARTESIAN_POINT ( 'NONE',  ( -27.52167012439999993, 1450.663735262239925, 136.4333507960980114 ) ) ;
#73441 = PLANE ( 'NONE',  #76737 ) ;
#73442 = CARTESIAN_POINT ( 'NONE',  ( -16.98264939016419817, 1410.452980272770219, 226.1748295909769695 ) ) ;
#73444 = EDGE_LOOP ( 'NONE', ( #97986, #23241, #19779, #40279 ) ) ;
#73443 = CARTESIAN_POINT ( 'NONE',  ( -0.03690140138640260470, 1502.066352419989926, 230.5451525067989849 ) ) ;
#73445 = CARTESIAN_POINT ( 'NONE',  ( -9.642223397419670050, 1460.679120766980077, 208.4218084076549928 ) ) ;
#73446 = CARTESIAN_POINT ( 'NONE',  ( 10.24713651180139884, 1471.272112719760116, 211.7185712946420040 ) ) ;
#73447 = B_SPLINE_CURVE_WITH_KNOTS ( 'NONE', 3,
 ( #83646, #92054, #14788, #67433 ),
 .UNSPECIFIED., .F., .F.,
 ( 4, 4 ),
 ( 0.000000000000000000, 1.000000000000000000 ),
 .UNSPECIFIED. ) ;
#73448 = CARTESIAN_POINT ( 'NONE',  ( 3.069076556224334063, 1369.654997644983041, 210.5785052009047433 ) ) ;
#73449 = CARTESIAN_POINT ( 'NONE',  ( -109.8265548189999947, 1384.687384907379965, 311.3749632952589650 ) ) ;
#73450 = CARTESIAN_POINT ( 'NONE',  ( -0.1314651167789250008, 1419.667472256169958, 184.2940143127850092 ) ) ;
#73451 = AXIS2_PLACEMENT_3D ( 'NONE', #96724, #94487, #69329 ) ;
#73452 = CARTESIAN_POINT ( 'NONE',  ( 0.0006788796961669999862, 1465.026769819230140, 237.7732385775979935 ) ) ;
#73453 = CARTESIAN_POINT ( 'NONE',  ( 21.29410851689999973, 1409.656667046429902, 215.2264874598780011 ) ) ;
#73454 = B_SPLINE_SURFACE_WITH_KNOTS ( 'NONE', 5, 5, ( 
 ( #76744, #67811, #94082, #103597, #58851, #26897 ),
 ( #16257, #61086, #95201, #8419, #17352, #51547 ),
 ( #8981, #18462, #84036, #7334, #33076, #67267 ),
 ( #101359, #43153, #50460, #34187, #77309, #68927 ),
 ( #101925, #25211, #59416, #53218, #53788, #44822 ),
 ( #11746, #45915, #78975, #2819, #104150, #1715 ) ),
 .UNSPECIFIED., .F., .F., .F.,
 ( 6, 6 ),
 ( 6, 6 ),
 ( 111.4340720229999988, 112.5451345809999992 ),
 ( 0.000000000000000000, 2.000000000000000000 ),
 .UNSPECIFIED. ) ;
#73455 = CARTESIAN_POINT ( 'NONE',  ( -2.670080947820280048, 1412.658061024129893, 186.4741318146120079 ) ) ;
#73456 = CARTESIAN_POINT ( 'NONE',  ( -18.27900023279999786, 1466.853294321590283, 217.8669514379789973 ) ) ;
#73457 = CARTESIAN_POINT ( 'NONE',  ( -17.59443979970000171, 1423.391293522529850, 226.3973360769979877 ) ) ;
#73459 = CARTESIAN_POINT ( 'NONE',  ( 17.06591927879999915, 1409.674274255629825, 223.8482220529980111 ) ) ;
#73458 = CARTESIAN_POINT ( 'NONE',  ( -4.613769899311276568, 1511.398921086024302, 200.7270633290623607 ) ) ;
#73460 = CARTESIAN_POINT ( 'NONE',  ( 20.02429320899999965, 1475.403248319589693, 206.2289784283690040 ) ) ;
#73461 = CARTESIAN_POINT ( 'NONE',  ( -107.1941519259529798, 1348.229899472569514, 298.0159978832118099 ) ) ;
#73462 = CARTESIAN_POINT ( 'NONE',  ( 17.83486663330506872, 1523.678648413191695, 237.8759530894958800 ) ) ;
#73463 = CARTESIAN_POINT ( 'NONE',  ( -16.36753375360000007, 1504.434416204990157, 208.8870069452450196 ) ) ;
#73464 = CARTESIAN_POINT ( 'NONE',  ( 18.89959486413309975, 1416.839692127159879, 210.6687135792209915 ) ) ;
#73465 = CARTESIAN_POINT ( 'NONE',  ( -4.042417815834999928, 1516.904492006980036, 205.6736390534169914 ) ) ;
#73466 = CARTESIAN_POINT ( 'NONE',  ( -6.384986843198960038, 1485.140801668499989, 183.7378743282880009 ) ) ;
#73467 = CARTESIAN_POINT ( 'NONE',  ( 9578.491711904032854, -2339.246371527899555, -432.3565737843579768 ) ) ;
#73468 = CARTESIAN_POINT ( 'NONE',  ( -4.230746000628669456, 1441.524192597599949, 164.6884930711709956 ) ) ;
#73470 = EDGE_LOOP ( 'NONE', ( #65357, #58883, #29915, #23063 ) ) ;
#73469 = CARTESIAN_POINT ( 'NONE',  ( -67.66759637757709811, 1379.745741269309974, 278.9788985089999755 ) ) ;
#73471 = ORIENTED_EDGE ( 'NONE', *, *, #103731, .F. ) ;
#73472 = EDGE_CURVE ( 'NONE', #81438, #53391, #46607, .T. ) ;
#73473 = CARTESIAN_POINT ( 'NONE',  ( 28.26971619830000293, 1508.651289825929780, 209.4063489423409976 ) ) ;
#73474 = EDGE_LOOP ( 'NONE', ( #76009, #68102, #88771, #4604 ) ) ;
#73475 = CARTESIAN_POINT ( 'NONE',  ( -0.7745270672630399922, 1486.078395409020004, 220.9964989435360110 ) ) ;
#73476 = CYLINDRICAL_SURFACE ( 'NONE', #104715, 1.000000000000000888 ) ;
#73478 = CARTESIAN_POINT ( 'NONE',  ( 21.39322610469999830, 1453.000988217330132, 223.2795384177979940 ) ) ;
#73477 = CARTESIAN_POINT ( 'NONE',  ( -8.178500771994089646, 1441.152429774469965, 153.9860759686779943 ) ) ;
#73479 = CARTESIAN_POINT ( 'NONE',  ( -0.7352271553329990939, 1516.963431999339946, 210.8369554172870153 ) ) ;
#73480 = CARTESIAN_POINT ( 'NONE',  ( -24.17245393478090065, 1452.068978953060196, 136.5158210362200180 ) ) ;
#73481 = CARTESIAN_POINT ( 'NONE',  ( -107.3025753749169979, 1378.913060387289988, 307.5931263302900334 ) ) ;
#73482 = CARTESIAN_POINT ( 'NONE',  ( 2.923521116649999918, 1410.394928919730091, 231.6309306915980244 ) ) ;
#73483 = CARTESIAN_POINT ( 'NONE',  ( 10.33351940753939857, 1481.839770964269974, 211.5429078627209947 ) ) ;
#73484 = PRODUCT_CONTEXT ( 'NONE', #83513, 'mechanical' ) ;
#73485 = CARTESIAN_POINT ( 'NONE',  ( 35.74845714555229392, 1451.452973098439998, 134.0999999985519935 ) ) ;
#73486 = CIRCLE ( 'NONE', #101316, 27.00880975787848470 ) ;
#73487 = CARTESIAN_POINT ( 'NONE',  ( 0.000000000000000000, 1523.382868172864164, 209.1218459616979999 ) ) ;
#73488 = ORIENTED_EDGE ( 'NONE', *, *, #1758, .T. ) ;
#73489 = CARTESIAN_POINT ( 'NONE',  ( 11.27339694790000024, 1433.557990534789951, 225.8166789514989716 ) ) ;
#73490 = DIRECTION ( 'NONE',  ( -0.6736849260863841948, 0.000000000000000000, 0.7390186874254148774 ) ) ;
#73491 = VERTEX_POINT ( 'NONE', #20595 ) ;
#73492 = ORIENTED_EDGE ( 'NONE', *, *, #96617, .F. ) ;
#73493 = CARTESIAN_POINT ( 'NONE',  ( 13.46271771603947087, 1410.756095866311398, 228.3121742440291655 ) ) ;
#73494 = CARTESIAN_POINT ( 'NONE',  ( 16.25286368722670716, 1514.564622118244188, 194.3294294352374436 ) ) ;
#73495 = EDGE_CURVE ( 'NONE', #32890, #81031, #50198, .T. ) ;
#73496 = CIRCLE ( 'NONE', #53854, 1.999999999999999556 ) ;
#73497 = CARTESIAN_POINT ( 'NONE',  ( 12.66527585539470024, 1500.313660553920045, 208.2538028397970038 ) ) ;
#73498 = CARTESIAN_POINT ( 'NONE',  ( -19.39187281942849950, 1508.251301914079932, 209.6313561747230096 ) ) ;
#73499 = B_SPLINE_CURVE_WITH_KNOTS ( 'NONE', 5,
 ( #99282, #22558, #21468, #47805, #72470, #12548 ),
 .UNSPECIFIED., .F., .F.,
 ( 6, 6 ),
 ( -0.9266590516050000614, 5.517428931161120431 ),
 .UNSPECIFIED. ) ;
#73500 = CARTESIAN_POINT ( 'NONE',  ( -2.500000000000000000, 1439.624617065190023, 168.6282375182209989 ) ) ;
#73501 = CARTESIAN_POINT ( 'NONE',  ( -13.15516956290000117, 1379.513185268939878, 208.2695793243090066 ) ) ;
#73502 = DIRECTION ( 'NONE',  ( 0.02616798426433289068, 0.9993150019884036173, 0.02616798426433289068 ) ) ;
#73503 = CARTESIAN_POINT ( 'NONE',  ( -1.255931481480000000, 1464.641271298989977, 198.9598639639989983 ) ) ;
#73504 = CARTESIAN_POINT ( 'NONE',  ( 30.31052258194597115, 1523.604703353109699, 222.4930856806589929 ) ) ;
#73505 = CARTESIAN_POINT ( 'NONE',  ( 11.41806921110000062, 1414.913060387329779, 197.3911438671979965 ) ) ;
#73506 = CARTESIAN_POINT ( 'NONE',  ( -68.27866047183589160, 1384.726245259990037, 262.2716603733960028 ) ) ;
#73507 = ORIENTED_EDGE ( 'NONE', *, *, #109924, .T. ) ;
#73508 = CARTESIAN_POINT ( 'NONE',  ( 3.487592428934999766, 1509.038615934169911, 204.6345961781970004 ) ) ;
#73509 = CARTESIAN_POINT ( 'NONE',  ( 7.710966977635000497, 1516.608208975040043, 207.9930883710269711 ) ) ;
#73510 = ORIENTED_EDGE ( 'NONE', *, *, #54271, .F. ) ;
#73511 = CARTESIAN_POINT ( 'NONE',  ( 11.00355868729999997, 1414.913528139930122, 222.3255397388979873 ) ) ;
#73512 = AXIS2_PLACEMENT_3D ( 'NONE', #10190, #60624, #36500 ) ;
#73513 = ADVANCED_FACE ( 'NONE', ( #105187 ), #87572, .T. ) ;
#73514 = CARTESIAN_POINT ( 'NONE',  ( -0.0002319074763942019469, 1452.464470640482432, 153.6345273712305186 ) ) ;
#73515 = VERTEX_POINT ( 'NONE', #2568 ) ;
#73516 = CARTESIAN_POINT ( 'NONE',  ( -33.91369114349999592, 1451.728768196330066, 134.7155300131979914 ) ) ;
#73517 = FACE_OUTER_BOUND ( 'NONE', #77229, .T. ) ;
#73518 = CARTESIAN_POINT ( 'NONE',  ( -18.51436573157338117, 1511.187213306747708, 237.1421867457408723 ) ) ;
#73519 = CARTESIAN_POINT ( 'NONE',  ( -1.925297170580940076, 1519.551704408389924, 187.5582988486569889 ) ) ;
#73520 = CARTESIAN_POINT ( 'NONE',  ( -6.988050048983349249, 1435.480056246220101, 215.8758039753799949 ) ) ;
#73521 = EDGE_CURVE ( 'NONE', #71877, #67084, #10870, .T. ) ;
#73522 = CARTESIAN_POINT ( 'NONE',  ( 32.86802468386284914, 1523.382868172864164, 201.0396662540042030 ) ) ;
#73523 = CARTESIAN_POINT ( 'NONE',  ( 4.970023385829999363, 1406.187660922729947, 266.9514890597980070 ) ) ;
#73524 = CARTESIAN_POINT ( 'NONE',  ( -6.187521092793239141, 1510.844697583444713, 201.6626558324045391 ) ) ;
#73525 = DIRECTION ( 'NONE',  ( 0.4090087482554383147, -0.000000000000000000, 0.9125304618753937724 ) ) ;
#73527 = CARTESIAN_POINT ( 'NONE',  ( -10.63901352068986483, 1424.089911397193191, 137.5855889613041256 ) ) ;
#73526 = CARTESIAN_POINT ( 'NONE',  ( 16.35084419920000087, 1459.109911444630143, 230.6444591943979958 ) ) ;
#73528 = CARTESIAN_POINT ( 'NONE',  ( -4.733473252797362640, 1422.203616401994850, 184.7151843475826922 ) ) ;
#73529 = CARTESIAN_POINT ( 'NONE',  ( -0.7403206051589980019, 1517.139320148880188, 216.8467205834170102 ) ) ;
#73530 = CARTESIAN_POINT ( 'NONE',  ( -0.2728668963706926687, 1486.429877400285932, 181.7829858203650986 ) ) ;
#73531 = CARTESIAN_POINT ( 'NONE',  ( -10.38518064779726657, 1480.556690206445182, 207.3434171914812225 ) ) ;
#73532 = CARTESIAN_POINT ( 'NONE',  ( 3.401541474470889614, 1468.225229937070026, 218.5224292273400124 ) ) ;
#73533 = CARTESIAN_POINT ( 'NONE',  ( -3.254401441735000233, 1516.919782530640077, 213.1645757730269963 ) ) ;
#73534 = CARTESIAN_POINT ( 'NONE',  ( 18.62446811629999743, 1507.629699719829887, 188.5309061728979998 ) ) ;
#73535 = CARTESIAN_POINT ( 'NONE',  ( -11.60004869885203682, 1426.459394169735333, 139.0224411922850436 ) ) ;
#73537 = ORIENTED_EDGE ( 'NONE', *, *, #64472, .F. ) ;
#73536 = CARTESIAN_POINT ( 'NONE',  ( -1.078902958008049989E-15, 1372.293237941190000, 209.1218459616989946 ) ) ;
#73538 = CARTESIAN_POINT ( 'NONE',  ( -8.604696469749999466, 1384.902331291159953, 199.8686668561790043 ) ) ;
#73539 = CARTESIAN_POINT ( 'NONE',  ( 15.63397015710000026, 1455.915410822730109, 213.2303957300479738 ) ) ;
#73540 = ADVANCED_FACE ( 'NONE', ( #77047 ), #45116, .T. ) ;
#73541 = CARTESIAN_POINT ( 'NONE',  ( -11.75482189299999902, 1431.209516603920065, 150.7135045689980188 ) ) ;
#73542 = DIRECTION ( 'NONE',  ( 0.000000000000000000, 0.000000000000000000, 1.000000000000000000 ) ) ;
#73543 = CARTESIAN_POINT ( 'NONE',  ( -7.195143960150679696, 1440.674916713600169, 203.7359215401640142 ) ) ;
#73544 = CARTESIAN_POINT ( 'NONE',  ( 4.401092417150000102, 1420.174153566729956, 185.7217845719979721 ) ) ;
#73545 = EDGE_CURVE ( 'NONE', #89306, #29708, #9282, .T. ) ;
#73546 = CARTESIAN_POINT ( 'NONE',  ( 7.524255332260000095, 1421.856213011689988, 195.6731416337989913 ) ) ;
#73547 = CARTESIAN_POINT ( 'NONE',  ( -2.823233910641499644, 1474.899251128670130, 216.0777834340740071 ) ) ;
#73548 = EDGE_CURVE ( 'NONE', #83547, #100304, #61615, .T. ) ;
#73550 = CARTESIAN_POINT ( 'NONE',  ( -6.736199635445266232, 1420.681931525483833, 137.0999999980981272 ) ) ;
#73549 = CARTESIAN_POINT ( 'NONE',  ( -20.73607666650000070, 1470.086132943030179, 225.0942381079979953 ) ) ;
#73551 = CARTESIAN_POINT ( 'NONE',  ( 25.98102620618460179, 1446.564900598649956, 138.2990622187049894 ) ) ;
#73552 = ORIENTED_EDGE ( 'NONE', *, *, #17108, .F. ) ;
#73553 = CARTESIAN_POINT ( 'NONE',  ( -7.334957394705000411, 1517.030858226499959, 204.5055736355369902 ) ) ;
#73554 = CARTESIAN_POINT ( 'NONE',  ( 7.030088544379999860, 1406.659535857730134, 269.2761678244980317 ) ) ;
#73555 = PRESENTATION_LAYER_ASSIGNMENT (  '', '', ( #10959 ) ) ;
#73556 = CARTESIAN_POINT ( 'NONE',  ( 0.3610052795299999451, 1409.865909187230045, 185.0540742924980009 ) ) ;
#73557 = CARTESIAN_POINT ( 'NONE',  ( 18.67620478639999959, 1410.876507162430016, 194.6621290597979907 ) ) ;
#73558 = EDGE_CURVE ( 'NONE', #80324, #81409, #69561, .T. ) ;
#73559 = CARTESIAN_POINT ( 'NONE',  ( 24.59474210122779425, 1439.616678441558406, 212.4961791304409076 ) ) ;
#73560 = CARTESIAN_POINT ( 'NONE',  ( 0.5244545025614146816, 1463.744894996491666, 199.3254876305578307 ) ) ;
#73561 = DIRECTION ( 'NONE',  ( 0.000000000000000000, -1.000000000000000000, 6.123233995736769734E-17 ) ) ;
#73562 = AXIS2_PLACEMENT_3D ( 'NONE', #63609, #36175, #63074 ) ;
#73563 = CARTESIAN_POINT ( 'NONE',  ( -7.228518429932707434, 1439.534556209132461, 204.1938366727016501 ) ) ;
#73564 = CARTESIAN_POINT ( 'NONE',  ( -2.500000001420000117, 1449.201558854039831, 155.6080925163979884 ) ) ;
#73565 = CARTESIAN_POINT ( 'NONE',  ( -12.32298830910000120, 1445.672643151689954, 187.1727947595979913 ) ) ;
#73566 = CARTESIAN_POINT ( 'NONE',  ( -19.88442509963795857, 1485.192351728225049, 190.7964254835079885 ) ) ;
#73567 = CARTESIAN_POINT ( 'NONE',  ( -2.469737515570000319, 1507.227429580189892, 221.7265305201989918 ) ) ;
#73568 = CARTESIAN_POINT ( 'NONE',  ( -4.325231544520000249, 1515.225845272990000, 210.2100514189989724 ) ) ;
#73569 = CARTESIAN_POINT ( 'NONE',  ( -3.444929440920000197, 1424.916853926129988, 224.8635561966979708 ) ) ;
#73570 = EDGE_CURVE ( 'NONE', #17762, #100644, #89496, .T. ) ;
#73571 = CARTESIAN_POINT ( 'NONE',  ( -11.75869035456349998, 1517.051704408389924, 190.9442076542370046 ) ) ;
#73572 = CARTESIAN_POINT ( 'NONE',  ( 2.500000000000000000, 1439.577074560470010, 165.1593652681980018 ) ) ;
#73573 = VECTOR ( 'NONE', #26279, 1000.000000000000114 ) ;
#73574 = CARTESIAN_POINT ( 'NONE',  ( -2.102271589710000388, 1475.801440029330024, 266.9594147012980443 ) ) ;
#73575 = CARTESIAN_POINT ( 'NONE',  ( -4.221728487123090012, 1446.223285440960126, 169.8967716716199732 ) ) ;
#73576 = CARTESIAN_POINT ( 'NONE',  ( -18.15573260460000071, 1428.693028929629918, 192.9183044383979961 ) ) ;
#73577 = ADVANCED_FACE ( 'NONE', ( #96603 ), #33829, .T. ) ;
#73578 = CARTESIAN_POINT ( 'NONE',  ( -10.32949511124177633, 1486.513216322853395, 183.6385995678631389 ) ) ;
#73579 = CARTESIAN_POINT ( 'NONE',  ( -30.81915246055419999, 1384.825406036370168, 228.9375977134340019 ) ) ;
#73580 = CARTESIAN_POINT ( 'NONE',  ( -30.87201549882227525, 1524.816548299036867, 221.7489384518832196 ) ) ;
#73581 = CARTESIAN_POINT ( 'NONE',  ( 12.25049518300349938, 1416.576002137149999, 223.5606104245470078 ) ) ;
#73582 = CARTESIAN_POINT ( 'NONE',  ( 12.10692502261549919, 1491.460737533769816, 207.0028281992289863 ) ) ;
#73583 = CARTESIAN_POINT ( 'NONE',  ( 32.06267705388252409, 1524.739563915922645, 216.1098277237242655 ) ) ;
#73584 = CARTESIAN_POINT ( 'NONE',  ( 8.517158571662550415, 1511.399506464603064, 204.1391972876773480 ) ) ;
#73585 = CARTESIAN_POINT ( 'NONE',  ( -19.99185821690000253, 1409.775774462230174, 199.2575659085879920 ) ) ;
#73586 = AXIS2_PLACEMENT_3D ( 'NONE', #99843, #105099, #92009 ) ;
#73587 = CARTESIAN_POINT ( 'NONE',  ( 12.77583168044349904, 1421.377537522909961, 206.0195167871399917 ) ) ;
#73588 = CARTESIAN_POINT ( 'NONE',  ( -44.34342732500000039, 1432.315964142800112, 269.0104413644979786 ) ) ;
#73589 = VERTEX_POINT ( 'NONE', #71444 ) ;
#73590 = CARTESIAN_POINT ( 'NONE',  ( -5.511118846543562100, 1410.480444842805809, 231.6789814916551506 ) ) ;
#73591 = CARTESIAN_POINT ( 'NONE',  ( -7.540791941105130292, 1510.557600718731237, 214.8905100802431036 ) ) ;
#73592 = CARTESIAN_POINT ( 'NONE',  ( -19.73708035071419786, 1467.795414648790029, 204.3773339574159991 ) ) ;
#73593 = AXIS2_PLACEMENT_3D ( 'NONE', #39784, #48196, #98020 ) ;
#73595 = CARTESIAN_POINT ( 'NONE',  ( -13.86270804226499997, 1513.875858217480072, 192.3565727231670053 ) ) ;
#73594 = CARTESIAN_POINT ( 'NONE',  ( 10.81507089449999981, 1424.921187596630034, 144.1620444886980010 ) ) ;
#73596 = CARTESIAN_POINT ( 'NONE',  ( 17.42134197181193045, 1525.253996226949084, 237.1661559799196652 ) ) ;
#73597 = CARTESIAN_POINT ( 'NONE',  ( 27.28327538803539909, 1449.032212788670222, 136.7238666261060018 ) ) ;
#73598 = CARTESIAN_POINT ( 'NONE',  ( -0.7533001734329990429, 1516.714320817460020, 201.7957737879569891 ) ) ;
#73599 = CARTESIAN_POINT ( 'NONE',  ( 7.527441479340000186, 1427.147074679829984, 212.6188437181790221 ) ) ;
#73600 = CARTESIAN_POINT ( 'NONE',  ( -17.84103545810000213, 1489.004099770289940, 195.1797354288989936 ) ) ;
#73601 = CARTESIAN_POINT ( 'NONE',  ( 15.31485518243500010, 1513.484013041540038, 194.5539220954669872 ) ) ;
#73602 = CARTESIAN_POINT ( 'NONE',  ( -21.33855393657290023, 1418.051173837530087, 208.5953683876979881 ) ) ;
#73603 = CARTESIAN_POINT ( 'NONE',  ( -18.52790950258529890, 1380.296293541789964, 211.3290533409030161 ) ) ;
#73604 = AXIS2_PLACEMENT_3D ( 'NONE', #55119, #45066, #71390 ) ;
#73605 = CARTESIAN_POINT ( 'NONE',  ( 6.904968631809683011, 1366.095340045324292, 208.3718459617061285 ) ) ;
#73607 = ORIENTED_EDGE ( 'NONE', *, *, #19926, .F. ) ;
#73606 = CARTESIAN_POINT ( 'NONE',  ( 4.987078429774149946, 1508.551704408389924, 205.1632116869930087 ) ) ;
#73608 = VERTEX_POINT ( 'NONE', #105560 ) ;
#73609 = CARTESIAN_POINT ( 'NONE',  ( -12.25627298530000076, 1396.517938870329999, 207.5036536129880176 ) ) ;
#73610 = CARTESIAN_POINT ( 'NONE',  ( -20.28244347700000105, 1409.621338920729841, 216.0116594248979993 ) ) ;
#73611 = CARTESIAN_POINT ( 'NONE',  ( 0.000000000000000000, 1512.187213306747481, 209.1218459616979999 ) ) ;
#73612 = CARTESIAN_POINT ( 'NONE',  ( -13.50678276547792578, 1444.060212379681616, 169.3531415429766867 ) ) ;
#73613 = CARTESIAN_POINT ( 'NONE',  ( -25.84053268629999778, 1509.815431673230023, 196.9032967497980167 ) ) ;
#73614 = CARTESIAN_POINT ( 'NONE',  ( -7.588802720235000798, 1511.942942747529969, 211.3806715220270007 ) ) ;
#73615 =( BOUNDED_SURFACE ( )  B_SPLINE_SURFACE ( 3, 2, ( 
 ( #10058, #103563, #105233 ),
 ( #44231, #35823, #10624 ),
 ( #44791, #36363, #78943 ),
 ( #78375, #2251, #70555 ),
 ( #104673, #68897, #62151 ),
 ( #62721, #19555, #53761 ),
 ( #17323, #51517, #94606 ),
 ( #8950, #34706, #102999 ),
 ( #26296, #86212, #9505 ),
 ( #69446, #63261, #4961 ),
 ( #22286, #21738, #55940 ),
 ( #106328, #99009, #37473 ),
 ( #13898, #11720, #45892 ),
 ( #3349, #30716, #48085 ) ),
 .UNSPECIFIED., .F., .F., .F. ) 
 B_SPLINE_SURFACE_WITH_KNOTS ( ( 4, 2, 2, 2, 2, 2, 4 ),
 ( 3, 3 ),
 ( 0.000000000000000000, 0.0009440840677144979451, 0.001416126101571746863, 0.001888168135428995890, 0.002360210169286244917, 0.002832252203143493727, 0.003776336270857991780 ),
 ( 0.000000000000000000, 1.000000000000000000 ),
 .UNSPECIFIED. ) 
 GEOMETRIC_REPRESENTATION_ITEM ( )  RATIONAL_B_SPLINE_SURFACE ( (
 ( 1.000000000000000000, 0.8070209408750077529, 1.000000000000000000),
 ( 1.000000000000000000, 0.8215603905271136043, 1.000000000000000000),
 ( 1.000000000000000000, 0.8340988699078115687, 1.000000000000000000),
 ( 1.000000000000000000, 0.8516751610450099541, 1.000000000000000000),
 ( 1.000000000000000000, 0.8573697395149780798, 1.000000000000000000),
 ( 1.000000000000000000, 0.8683586635666556974, 1.000000000000000000),
 ( 1.000000000000000000, 0.8736518481708377415, 1.000000000000000000),
 ( 1.000000000000000000, 0.8840377753030403962, 1.000000000000000000),
 ( 1.000000000000000000, 0.8891294171309215288, 1.000000000000000000),
 ( 1.000000000000000000, 0.8992456600571828718, 1.000000000000000000),
 ( 1.000000000000000000, 0.9042785869255108855, 1.000000000000000000),
 ( 1.000000000000000000, 0.9189749222834227016, 1.000000000000000000),
 ( 1.000000000000000000, 0.9283978182351991792, 1.000000000000000000),
 ( 1.000000000000000000, 0.9376006582765968878, 1.000000000000000000) ) ) 
 REPRESENTATION_ITEM ( '' )  SURFACE ( )  );
#73617 = CARTESIAN_POINT ( 'NONE',  ( -1.362051879945949784, 1414.539935085650086, 185.4257519797239979 ) ) ;
#73616 = CARTESIAN_POINT ( 'NONE',  ( 1.668731198869999988, 1443.775019653990057, 200.3211300381289846 ) ) ;
#73618 = CARTESIAN_POINT ( 'NONE',  ( 13.45197010939999949, 1429.761463759329899, 189.7509718724980132 ) ) ;
#73619 = CARTESIAN_POINT ( 'NONE',  ( -11.60080416610000142, 1414.971439108430104, 195.8791986486979795 ) ) ;
#73620 = CARTESIAN_POINT ( 'NONE',  ( -41.63813770664379632, 1444.512218055099993, 135.5979372019099856 ) ) ;
#73621 = CARTESIAN_POINT ( 'NONE',  ( 6.227580691487869302, 1396.130532339959927, 200.0029583712910153 ) ) ;
#73622 = CARTESIAN_POINT ( 'NONE',  ( 0.9297777941500000587, 1416.254459046630018, 190.2947620677979899 ) ) ;
#73623 = CARTESIAN_POINT ( 'NONE',  ( 11.75224816899999958, 1426.683125471030053, 145.2383014675980064 ) ) ;
#73624 = CARTESIAN_POINT ( 'NONE',  ( 41.49257106529999817, 1443.690927668370023, 136.5669627357980005 ) ) ;
#73625 = ORIENTED_EDGE ( 'NONE', *, *, #76848, .T. ) ;
#73626 = CARTESIAN_POINT ( 'NONE',  ( 3.964339422799999735, 1425.349073522829940, 185.3440290947980031 ) ) ;
#73627 = CARTESIAN_POINT ( 'NONE',  ( 1.514738106409309948, 1507.606285602550088, 186.2052147526660235 ) ) ;
#73628 = ORIENTED_EDGE ( 'NONE', *, *, #27754, .F. ) ;
#73629 = ORIENTED_EDGE ( 'NONE', *, *, #832, .T. ) ;
#73630 = LINE ( 'NONE', #74181, #84150 ) ;
#73631 = CARTESIAN_POINT ( 'NONE',  ( -15.33872957789999880, 1460.931222701129855, 228.7803497734979885 ) ) ;
#73632 = CARTESIAN_POINT ( 'NONE',  ( -108.9682439114556729, 1387.781254760463980, 310.7917411045218046 ) ) ;
#73633 = CARTESIAN_POINT ( 'NONE',  ( -6.940473372275000052, 1516.833525648419936, 215.6778681647369922 ) ) ;
#73634 = CARTESIAN_POINT ( 'NONE',  ( -14.51820269904870031, 1379.827956527899914, 208.4132882441429899 ) ) ;
#73635 = AXIS2_PLACEMENT_3D ( 'NONE', #30353, #66198, #64544 ) ;
#73636 = ORIENTED_EDGE ( 'NONE', *, *, #104265, .F. ) ;
#73637 = CARTESIAN_POINT ( 'NONE',  ( -11.42155100230000109, 1501.800602108690100, 208.0855181463290080 ) ) ;
#73638 = DIRECTION ( 'NONE',  ( 1.755985294532464991E-16, -1.000000000000000000, 1.338183447452830017E-16 ) ) ;
#73639 = CARTESIAN_POINT ( 'NONE',  ( -57.14396137519999286, 1379.007173132990147, 252.3469708262589961 ) ) ;
#73640 = CARTESIAN_POINT ( 'NONE',  ( 17.84625751240000113, 1415.088275290029969, 210.3637142236279942 ) ) ;
#73641 = CARTESIAN_POINT ( 'NONE',  ( 7.710285837685000310, 1516.582197289609894, 205.8614676770269796 ) ) ;
#73642 = VERTEX_POINT ( 'NONE', #63042 ) ;
#73643 = CARTESIAN_POINT ( 'NONE',  ( -4.037051035714999792, 1516.939819969850078, 209.1350663277499962 ) ) ;
#73644 = CARTESIAN_POINT ( 'NONE',  ( -19.94909556640000048, 1508.591193276130070, 229.3655219236979974 ) ) ;
#73645 = CARTESIAN_POINT ( 'NONE',  ( -30.76343349190171139, 1420.155678438769428, 269.4791553875487011 ) ) ;
#73646 = CARTESIAN_POINT ( 'NONE',  ( -2.942223483390000283, 1409.952541811230049, 232.5239949635980281 ) ) ;
#73648 = EDGE_LOOP ( 'NONE', ( #6105, #35466, #5773, #42117 ) ) ;
#73647 = CARTESIAN_POINT ( 'NONE',  ( -4.314829847434394239, 1413.913060387330006, 201.2236029046909209 ) ) ;
#73649 = CARTESIAN_POINT ( 'NONE',  ( -0.003590212486869529679, 1450.985003860830147, 181.7900261978950027 ) ) ;
#73650 = CARTESIAN_POINT ( 'NONE',  ( -28.62889416593939984, 1440.913060387320002, 233.6045261250210103 ) ) ;
#73651 = CARTESIAN_POINT ( 'NONE',  ( -47.53302541269999892, 1383.816002435690052, 256.2046081452590442 ) ) ;
#73652 = CARTESIAN_POINT ( 'NONE',  ( -14.25094185831662230, 1415.731847238539103, 214.3326356602875649 ) ) ;
#73653 = AXIS2_PLACEMENT_3D ( 'NONE', #42573, #110324, #59950 ) ;
#73654 = B_SPLINE_CURVE_WITH_KNOTS ( 'NONE', 5,
 ( #22407, #56609, #82354, #90744, #6187, #39802 ),
 .UNSPECIFIED., .F., .F.,
 ( 6, 6 ),
 ( -1.020974158415999922, 5.536280491647819879 ),
 .UNSPECIFIED. ) ;
#73655 = CARTESIAN_POINT ( 'NONE',  ( 12.98193753819199792, 1411.684960533729964, 269.6330119701129888 ) ) ;
#73656 = CARTESIAN_POINT ( 'NONE',  ( 0.01328393942530149870, 1516.939580991450157, 212.3834982571270018 ) ) ;
#73657 = CARTESIAN_POINT ( 'NONE',  ( -47.71314244639999913, 1379.676121073949844, 235.3060314611589945 ) ) ;
#73658 = CARTESIAN_POINT ( 'NONE',  ( 24.12183011420000156, 1410.980265346130182, 208.8601329017200214 ) ) ;
#73659 = CARTESIAN_POINT ( 'NONE',  ( -20.65862871410000423, 1509.573541660129877, 188.2595635174980089 ) ) ;
#73660 = CARTESIAN_POINT ( 'NONE',  ( 12.27064591350710110, 1492.413804220679822, 210.4788641801989684 ) ) ;
#73661 = CARTESIAN_POINT ( 'NONE',  ( -7.709060745858529629, 1516.535411464270055, 210.9785344462470107 ) ) ;
#73662 = CARTESIAN_POINT ( 'NONE',  ( -2.865636847234999784, 1516.815173273089840, 210.2578502442970318 ) ) ;
#73663 = CARTESIAN_POINT ( 'NONE',  ( 4.188808935644120268, 1421.671353483030089, 184.7101618531249869 ) ) ;
#73664 = CARTESIAN_POINT ( 'NONE',  ( 0.1469469801610000237, 1420.465541450629871, 183.3355677249980147 ) ) ;
#73665 = CARTESIAN_POINT ( 'NONE',  ( -5.513435705061030312, 1509.038615938849944, 201.6090957135359929 ) ) ;
#73666 = B_SPLINE_CURVE_WITH_KNOTS ( 'NONE', 3,
 ( #21081, #37920, #30607, #39562, #54189, #80471 ),
 .UNSPECIFIED., .F., .F.,
 ( 4, 2, 4 ),
 ( 0.000000000000000000, 0.5000000000000000000, 1.000000000000000000 ),
 .UNSPECIFIED. ) ;
#73668 = ORIENTED_EDGE ( 'NONE', *, *, #59118, .T. ) ;
#73667 = CARTESIAN_POINT ( 'NONE',  ( -22.78935994269999910, 1386.920570514349947, 221.8588691826589923 ) ) ;
#73670 = AXIS2_PLACEMENT_3D ( 'NONE', #93730, #1365, #69701 ) ;
#73669 = CARTESIAN_POINT ( 'NONE',  ( -42.71391872090229924, 1385.166217023060199, 247.0682200317750130 ) ) ;
#73671 = ADVANCED_FACE ( 'NONE', ( #63578 ), #78, .T. ) ;
#73672 = CARTESIAN_POINT ( 'NONE',  ( 18.79707643829999952, 1416.837309283529976, 209.8349447685179996 ) ) ;
#73673 = ADVANCED_FACE ( 'NONE', ( #97694 ), #20501, .T. ) ;
#73674 = CARTESIAN_POINT ( 'NONE',  ( 0.1425930925969999818, 1416.432970197429995, 233.7167792884980031 ) ) ;
#73675 = CARTESIAN_POINT ( 'NONE',  ( 4.987078442593329441, 1508.551704408389924, 206.6339108768089829 ) ) ;
#73676 = CARTESIAN_POINT ( 'NONE',  ( -2.673720665360000304, 1500.461465227589997, 230.2728548803989952 ) ) ;
#73677 = CARTESIAN_POINT ( 'NONE',  ( 12.07937513949999975, 1426.251990374380057, 203.1934598926790159 ) ) ;
#73678 = DIRECTION ( 'NONE',  ( -1.000000000000000000, 0.000000000000000000, 0.000000000000000000 ) ) ;
#73680 = LINE ( 'NONE', #73112, #81913 ) ;
#73679 = CARTESIAN_POINT ( 'NONE',  ( -2.483949978725000118, 1517.156142772249950, 216.0726795003369887 ) ) ;
#73681 = CARTESIAN_POINT ( 'NONE',  ( 4.617353517619999792, 1460.098150474590057, 228.0971968620989969 ) ) ;
#73682 = CARTESIAN_POINT ( 'NONE',  ( 31.97743984922262683, 1525.878013734321485, 220.1676294520832755 ) ) ;
#73683 = VERTEX_POINT ( 'NONE', #3363 ) ;
#73684 = CARTESIAN_POINT ( 'NONE',  ( -2.291047527245000381, 1516.524310051880093, 201.4130759250869858 ) ) ;
#73685 = CARTESIAN_POINT ( 'NONE',  ( 21.03123203779729877, 1507.789098030329797, 226.0655639048319756 ) ) ;
#73686 = EDGE_LOOP ( 'NONE', ( #75977, #11680, #65814, #101820 ) ) ;
#73687 = AXIS2_PLACEMENT_3D ( 'NONE', #294, #27133, #18702 ) ;
#73688 = CARTESIAN_POINT ( 'NONE',  ( -0.04790324752389999580, 1506.806593731130079, 231.2201824205980074 ) ) ;
#73689 = ADVANCED_FACE ( 'NONE', ( #87911 ), #77837, .F. ) ;
#73690 = CARTESIAN_POINT ( 'NONE',  ( 22.30619483830000149, 1451.363309493629913, 221.4011829164979872 ) ) ;
#73691 = CARTESIAN_POINT ( 'NONE',  ( 10.85236227365940032, 1461.719670514279869, 210.7330291806389937 ) ) ;
#73692 = CARTESIAN_POINT ( 'NONE',  ( 8.436619542363665403, 1424.469057821296929, 195.8194399936322725 ) ) ;
#73693 = VECTOR ( 'NONE', #102600, 1000.000000000000227 ) ;
#73694 = CARTESIAN_POINT ( 'NONE',  ( 2.942575405789999987, 1443.229435617889749, 217.5275331713689866 ) ) ;
#73695 = CARTESIAN_POINT ( 'NONE',  ( 17.02668221408760019, 1422.112876149069962, 226.8213126862850118 ) ) ;
#73696 = CARTESIAN_POINT ( 'NONE',  ( -2.499999995540000075, 1447.977244151060177, 159.5594115894979836 ) ) ;
#73697 = CARTESIAN_POINT ( 'NONE',  ( -19.25146917829999893, 1426.258557004829754, 225.2352025288980144 ) ) ;
#73698 = CARTESIAN_POINT ( 'NONE',  ( -25.78987273775174671, 1469.122194850858023, 269.4331841604852116 ) ) ;
#73699 = CARTESIAN_POINT ( 'NONE',  ( -108.1293204100000054, 1388.564942467859964, 298.2680007914589737 ) ) ;
#73700 = CARTESIAN_POINT ( 'NONE',  ( 18.60936348979999977, 1461.935155496729976, 190.4888835971979972 ) ) ;
#73701 = FACE_OUTER_BOUND ( 'NONE', #891, .T. ) ;
#73702 = CARTESIAN_POINT ( 'NONE',  ( -20.75102955870752908, 1467.505718010989767, 269.3935093439889101 ) ) ;
#73703 = ORIENTED_EDGE ( 'NONE', *, *, #7769, .F. ) ;
#73704 = CARTESIAN_POINT ( 'NONE',  ( -104.2332084890000061, 1379.842145981129988, 303.2776814956590101 ) ) ;
#73705 = CARTESIAN_POINT ( 'NONE',  ( -14.30687469689999958, 1508.551704411289847, 215.7932974708489837 ) ) ;
#73706 = CARTESIAN_POINT ( 'NONE',  ( -121.7571430937320827, 1378.913060387289988, 299.6563178771723415 ) ) ;
#73707 = DIRECTION ( 'NONE',  ( 1.224646799147350002E-16, -1.836970198721029688E-16, -1.000000000000000000 ) ) ;
#73708 = FACE_OUTER_BOUND ( 'NONE', #80918, .T. ) ;
#73709 = CARTESIAN_POINT ( 'NONE',  ( -0.02598383688650000162, 1416.108377156529968, 233.5481721888980076 ) ) ;
#73710 = CARTESIAN_POINT ( 'NONE',  ( -12.96403976842712069, 1442.927061488039499, 186.4958570142325698 ) ) ;
#73711 = EDGE_CURVE ( 'NONE', #24288, #26097, #29117, .T. ) ;
#73712 = CARTESIAN_POINT ( 'NONE',  ( -8.628345599877569327, 1437.012300105949862, 209.5206063237490071 ) ) ;
#73713 = SPHERICAL_SURFACE ( 'NONE', #15015, 2.000000000000000000 ) ;
#73714 = FACE_OUTER_BOUND ( 'NONE', #54233, .T. ) ;
#73715 = CARTESIAN_POINT ( 'NONE',  ( -108.6616353267809956, 1383.758284946439971, 311.0749865448200353 ) ) ;
#73716 = CARTESIAN_POINT ( 'NONE',  ( -9.642223397419670050, 1460.679120766980077, 208.4218084076549928 ) ) ;
#73718 = EDGE_CURVE ( 'NONE', #35166, #49199, #21507, .T. ) ;
#73717 = CARTESIAN_POINT ( 'NONE',  ( -15.15772398740000071, 1439.441663529990137, 221.0618115286989962 ) ) ;
#73720 = ORIENTED_EDGE ( 'NONE', *, *, #110273, .F. ) ;
#73719 = CARTESIAN_POINT ( 'NONE',  ( 17.93635821316399870, 1424.337455629530041, 225.8600358504349970 ) ) ;
#73721 = CARTESIAN_POINT ( 'NONE',  ( -90.90849950880000563, 1380.088580609059818, 305.1544273986589815 ) ) ;
#73722 = CARTESIAN_POINT ( 'NONE',  ( 12.45742383169469925, 1512.169469372300000, 224.0727726720780026 ) ) ;
#73723 = ORIENTED_EDGE ( 'NONE', *, *, #52876, .T. ) ;
#73724 = EDGE_LOOP ( 'NONE', ( #81066, #64819, #5928, #99139 ) ) ;
#73725 = CARTESIAN_POINT ( 'NONE',  ( -11.38916142969999967, 1500.505134835889976, 209.9622123134469973 ) ) ;
#73726 = CARTESIAN_POINT ( 'NONE',  ( 6.238899643214079305, 1516.716532632738563, 204.9585377404597466 ) ) ;
#73728 = CARTESIAN_POINT ( 'NONE',  ( -4.804950789190000293, 1465.695272584430086, 240.4142139981979938 ) ) ;
#73727 = CARTESIAN_POINT ( 'NONE',  ( 1.423785136650000060, 1455.243703889889957, 218.4445183310089931 ) ) ;
#73729 = CARTESIAN_POINT ( 'NONE',  ( 9.309724285312150016, 1436.355445090830017, 210.5148441957229863 ) ) ;
#73730 = CARTESIAN_POINT ( 'NONE',  ( -11.63477288290000011, 1433.176682644480024, 151.0246002562979868 ) ) ;
#73731 = CARTESIAN_POINT ( 'NONE',  ( -31.23437356469455040, 1512.187213306747481, 195.3468678195118287 ) ) ;
#73732 = CARTESIAN_POINT ( 'NONE',  ( 8.778595366665010502, 1422.758389621050128, 213.4479264546969830 ) ) ;
#73733 = CARTESIAN_POINT ( 'NONE',  ( 17.59268578599999699, 1410.455475235630047, 224.1775087684979724 ) ) ;
#73734 = CARTESIAN_POINT ( 'NONE',  ( -26.87493968100000075, 1439.491391334960099, 137.1013534362979840 ) ) ;
#73735 = CARTESIAN_POINT ( 'NONE',  ( 1.107569330185070200, 1515.100382602269974, 213.4503627880180261 ) ) ;
#73736 = CARTESIAN_POINT ( 'NONE',  ( 16.80709188200000170, 1415.354938809929763, 226.6316513545979774 ) ) ;
#73737 = CARTESIAN_POINT ( 'NONE',  ( 0.5620975284970839425, 1416.851343896850040, 190.4751211475700075 ) ) ;
#73738 = CARTESIAN_POINT ( 'NONE',  ( 6.892224678239939450, 1361.632554499738035, 210.6218459616987957 ) ) ;
#73739 = CARTESIAN_POINT ( 'NONE',  ( 32.40058737600722338, 1524.130440953581001, 201.3079925683071849 ) ) ;
#73741 = VERTEX_POINT ( 'NONE', #36928 ) ;
#73740 = CARTESIAN_POINT ( 'NONE',  ( 5.068991372531999845E-09, 1406.036819823360247, 266.8717186750929500 ) ) ;
#73742 = ORIENTED_EDGE ( 'NONE', *, *, #14410, .T. ) ;
#73743 = CARTESIAN_POINT ( 'NONE',  ( -11.86205860565950054, 1432.053659880270061, 149.9751002826119759 ) ) ;
#73744 = CARTESIAN_POINT ( 'NONE',  ( 19.23094364312690274, 1497.625611886179968, 221.9534124282759819 ) ) ;
#73745 = CARTESIAN_POINT ( 'NONE',  ( -8.194407608160000578, 1472.709661065629916, 270.4215667392979867 ) ) ;
#73746 = CARTESIAN_POINT ( 'NONE',  ( 12.70677192039999959, 1507.773872374229995, 233.3565881929980037 ) ) ;
#73747 = CARTESIAN_POINT ( 'NONE',  ( -123.7789942035663557, 1376.302340817389450, 298.5517755817776333 ) ) ;
#73748 = CYLINDRICAL_SURFACE ( 'NONE', #3621, 0.9999999999999976685 ) ;
#73749 = CIRCLE ( 'NONE', #2219, 0.9999999999999953371 ) ;
#73750 = CARTESIAN_POINT ( 'NONE',  ( 4.327725855061919980, 1515.130588580249878, 209.8370891087949985 ) ) ;
#73751 = CARTESIAN_POINT ( 'NONE',  ( -8.846465147500001791, 1384.759259630609904, 199.9281972367089963 ) ) ;
#73752 = CARTESIAN_POINT ( 'NONE',  ( 10.03054928460160156, 1469.026556028670029, 208.9478250291980146 ) ) ;
#73753 = CARTESIAN_POINT ( 'NONE',  ( -4.665462402540000220, 1457.845415160889843, 217.6027515947390327 ) ) ;
#73754 = CARTESIAN_POINT ( 'NONE',  ( 9.971295257834839276, 1364.502667329742053, 210.6218459616991936 ) ) ;
#73755 = CARTESIAN_POINT ( 'NONE',  ( -42.19526865402289673, 1426.222309814289929, 267.1071618434610286 ) ) ;
#73756 = VERTEX_POINT ( 'NONE', #10638 ) ;
#73757 = FACE_OUTER_BOUND ( 'NONE', #62083, .T. ) ;
#73758 = ORIENTED_EDGE ( 'NONE', *, *, #245, .T. ) ;
#73759 = ORIENTED_EDGE ( 'NONE', *, *, #81678, .T. ) ;
#73760 = CARTESIAN_POINT ( 'NONE',  ( -1.118104767724999782, 1516.965971551240045, 211.4215139361070044 ) ) ;
#73761 = CARTESIAN_POINT ( 'NONE',  ( -8.570364584155420573, 1448.478232341050216, 212.2952113106709930 ) ) ;
#73762 = CARTESIAN_POINT ( 'NONE',  ( 41.49081953422589919, 1444.098784150369738, 136.3336049811159967 ) ) ;
#73764 = CARTESIAN_POINT ( 'NONE',  ( -17.64794458902535723, 1419.546587406255867, 207.1439701417919252 ) ) ;
#73763 = CARTESIAN_POINT ( 'NONE',  ( 4.623787969365000805, 1516.947419719950176, 212.5709951659769956 ) ) ;
#73765 = CARTESIAN_POINT ( 'NONE',  ( -17.62598095200000259, 1440.442471470339797, 190.9074128188979955 ) ) ;
#73766 = AXIS2_PLACEMENT_3D ( 'NONE', #84920, #102279, #41287 ) ;
#73767 = CARTESIAN_POINT ( 'NONE',  ( -17.54299231450000107, 1415.063410489729904, 207.9622084005079898 ) ) ;
#73768 = VERTEX_POINT ( 'NONE', #104687 ) ;
#73769 = DIRECTION ( 'NONE',  ( 0.000000000000000000, -1.000000000000000000, 0.000000000000000000 ) ) ;
#73770 = CARTESIAN_POINT ( 'NONE',  ( 4.615017327834999961, 1516.987478262539980, 202.5620478758069964 ) ) ;
#73771 = CARTESIAN_POINT ( 'NONE',  ( -36.40679624375492551, 1451.403536190284058, 134.6865211625845973 ) ) ;
#73772 = CARTESIAN_POINT ( 'NONE',  ( -14.32917876877730023, 1384.520675589830034, 200.5334063978870063 ) ) ;
#73773 = CARTESIAN_POINT ( 'NONE',  ( -38.85064735957119808, 1426.481882780939941, 270.1670862944069995 ) ) ;
#73774 = CARTESIAN_POINT ( 'NONE',  ( -3.392503662839999823, 1483.205550810290106, 202.1035814847290055 ) ) ;
#73775 = CARTESIAN_POINT ( 'NONE',  ( -5.639077242409999968, 1396.170382959830022, 198.9228296104979847 ) ) ;
#73777 = ORIENTED_EDGE ( 'NONE', *, *, #42327, .T. ) ;
#73776 = CARTESIAN_POINT ( 'NONE',  ( -7.999724627149254808, 1364.917771588045298, 209.6218459617148824 ) ) ;
#73778 = EDGE_LOOP ( 'NONE', ( #31457, #19168, #72465, #15683 ) ) ;
#73779 = CARTESIAN_POINT ( 'NONE',  ( -11.86816883041749904, 1432.490446933490148, 149.9820829498439991 ) ) ;
#73780 = CARTESIAN_POINT ( 'NONE',  ( 8.133565924525001378, 1515.203649598490074, 214.8418076220970079 ) ) ;
#73781 = CARTESIAN_POINT ( 'NONE',  ( -13.53579909870000009, 1380.123783341879971, 205.1599962651189912 ) ) ;
#73782 = CARTESIAN_POINT ( 'NONE',  ( 2.742048936850008722, 1367.348608298013232, 208.3718459617061569 ) ) ;
#73783 = CARTESIAN_POINT ( 'NONE',  ( -8.840620885073990465, 1512.187213306747481, 223.8289249455316394 ) ) ;
#73784 = CARTESIAN_POINT ( 'NONE',  ( -5.772978316675000166, 1516.659138130710289, 210.2536427808470023 ) ) ;
#73785 = CARTESIAN_POINT ( 'NONE',  ( -68.78265774330000681, 1379.747948328889834, 280.2440287133589436 ) ) ;
#73786 = CARTESIAN_POINT ( 'NONE',  ( -2.754695366840110182, 1484.262296928430032, 183.2948712447399657 ) ) ;
#73787 = DIRECTION ( 'NONE',  ( 0.000000000000000000, 0.000000000000000000, 1.000000000000000000 ) ) ;
#73788 = CARTESIAN_POINT ( 'NONE',  ( 11.30241272710000011, 1414.983773852929744, 222.3815203350980028 ) ) ;
#73789 = CARTESIAN_POINT ( 'NONE',  ( 12.22832204270000034, 1445.155618030669984, 186.6170962671980078 ) ) ;
#73790 = CARTESIAN_POINT ( 'NONE',  ( 4.997718238375000510, 1516.693851263360102, 207.9888968556769839 ) ) ;
#73791 = ORIENTED_EDGE ( 'NONE', *, *, #29516, .F. ) ;
#73792 = CARTESIAN_POINT ( 'NONE',  ( -42.60628463550339973, 1443.705283444799761, 134.7398504477979770 ) ) ;
#73793 = CARTESIAN_POINT ( 'NONE',  ( -10.17628962590000086, 1472.218688241290238, 207.3995869476289897 ) ) ;
#73794 = CARTESIAN_POINT ( 'NONE',  ( -23.79010043309475364, 1446.860041990635182, 214.1309382182860475 ) ) ;
#73795 = ORIENTED_EDGE ( 'NONE', *, *, #12307, .F. ) ;
#73796 = CARTESIAN_POINT ( 'NONE',  ( 18.07871887829625379, 1459.074710307333362, 227.9662036257006434 ) ) ;
#73797 = CARTESIAN_POINT ( 'NONE',  ( -29.02628104977890189, 1509.926680457060002, 211.9910930732060024 ) ) ;
#73798 = CARTESIAN_POINT ( 'NONE',  ( 13.68684928399999912, 1415.245980412430072, 197.2862492497980043 ) ) ;
#73799 = DIRECTION ( 'NONE',  ( -0.06124624279912479347, -0.4472592145003609354, -0.8923049326253389424 ) ) ;
#73800 = CARTESIAN_POINT ( 'NONE',  ( -15.69795926999090163, 1519.551704408389924, 195.4758181584410011 ) ) ;
#73801 = B_SPLINE_CURVE_WITH_KNOTS ( 'NONE', 3,
 ( #58325, #50483, #24676, #23039, #58874, #49923, #75135, #6796, #41522, #82963, #75679, #108716, #23601 ),
 .UNSPECIFIED., .F., .F.,
 ( 4, 3, 3, 3, 4 ),
 ( -14.83961564490000029, -13.59114161543520005, -10.15622042185490059, -6.776369974453789524, -3.432288051224929859 ),
 .UNSPECIFIED. ) ;
#73802 = CARTESIAN_POINT ( 'NONE',  ( 17.13422049400000446, 1410.007864041130006, 225.8552460202980114 ) ) ;
#73803 = CARTESIAN_POINT ( 'NONE',  ( -24.68077630836099701, 1437.736159206269804, 210.5119845322900005 ) ) ;
#73804 = CARTESIAN_POINT ( 'NONE',  ( -4.240726796310859470, 1476.401387198489829, 199.6760741912259789 ) ) ;
#73805 = CARTESIAN_POINT ( 'NONE',  ( 22.89696446689377041, 1450.775607349197571, 218.3304116664471906 ) ) ;
#73806 = CARTESIAN_POINT ( 'NONE',  ( 2.500000000000000000, 1439.579545565689841, 165.8618548744180146 ) ) ;
#73807 = DIRECTION ( 'NONE',  ( -0.4874171250595387694, 0.8731692540388111823, 0.000000000000000000 ) ) ;
#73808 = CARTESIAN_POINT ( 'NONE',  ( 1.129386202275000084, 1516.613712827999962, 216.4452363774470030 ) ) ;
#73809 = ORIENTED_EDGE ( 'NONE', *, *, #101923, .T. ) ;
#73810 = CARTESIAN_POINT ( 'NONE',  ( 7.709283117220651071, 1516.543904940109996, 207.3844237024999870 ) ) ;
#73811 = CARTESIAN_POINT ( 'NONE',  ( -7.343342699544049739E-05, 1510.912287627390015, 179.8420056942519807 ) ) ;
#73812 = CARTESIAN_POINT ( 'NONE',  ( -2.696218734819999963, 1448.944770110710124, 184.2305108069980122 ) ) ;
#73813 = ADVANCED_FACE ( 'NONE', ( #62738 ), #68913, .F. ) ;
#73814 = CARTESIAN_POINT ( 'NONE',  ( -11.15268736319570131, 1425.700851422820051, 101.7515742452400076 ) ) ;
#73815 = CARTESIAN_POINT ( 'NONE',  ( -2.279616087740000019, 1474.769975645390105, 219.1638168117989949 ) ) ;
#73816 = CARTESIAN_POINT ( 'NONE',  ( 11.43192506429821087, 1425.760849248890963, 138.9701389427312961 ) ) ;
#73817 = CARTESIAN_POINT ( 'NONE',  ( 2.616097128857913123, 1417.751789119419755, 233.8775321444583710 ) ) ;
#73818 = CARTESIAN_POINT ( 'NONE',  ( -2.383222864668309793, 1471.336174120430087, 183.7826184400119871 ) ) ;
#73819 = CARTESIAN_POINT ( 'NONE',  ( -109.1507334230530120, 1385.214303402609858, 297.1444598211750190 ) ) ;
#73820 = EDGE_CURVE ( 'NONE', #59489, #82014, #58813, .T. ) ;
#73821 = DIRECTION ( 'NONE',  ( 0.6038592750913979179, 0.7071067811868638753, -0.3679048462383226470 ) ) ;
#73822 = CARTESIAN_POINT ( 'NONE',  ( 30.16636262817999992, 1440.913060385679955, 238.8788807354779919 ) ) ;
#73824 = CARTESIAN_POINT ( 'NONE',  ( -2.919081270098979441, 1368.383855509380055, 210.4211783971049954 ) ) ;
#73823 = CARTESIAN_POINT ( 'NONE',  ( 3.211105652400000121, 1415.841839642130026, 233.8555032973979735 ) ) ;
#73825 = DIRECTION ( 'NONE',  ( 0.1454373636825659899, -0.4507558898458529084, 0.8807196494993957403 ) ) ;
#73826 = ORIENTED_EDGE ( 'NONE', *, *, #77582, .T. ) ;
#73827 = ORIENTED_EDGE ( 'NONE', *, *, #20671, .F. ) ;
#73828 = CARTESIAN_POINT ( 'NONE',  ( 13.51610093808350577, 1445.063428794548372, 206.7785865123599365 ) ) ;
#73829 = PLANE ( 'NONE',  #58673 ) ;
#73830 = CARTESIAN_POINT ( 'NONE',  ( 15.75336812958949828, 1414.913060387329779, 205.2106275740719639 ) ) ;
#73831 = CARTESIAN_POINT ( 'NONE',  ( 11.43088729239800116, 1502.411350489410097, 211.2362053281570127 ) ) ;
#73832 = CARTESIAN_POINT ( 'NONE',  ( 18.28985832975333281, 1519.551704408389924, 219.7143006364888436 ) ) ;
#73833 = CARTESIAN_POINT ( 'NONE',  ( -17.59428824464819741, 1418.369366143110028, 226.0269679427519804 ) ) ;
#73834 = CARTESIAN_POINT ( 'NONE',  ( -5.409864544089550087, 1440.893826657579893, 154.8143284515260234 ) ) ;
#73835 = CARTESIAN_POINT ( 'NONE',  ( -41.78068117807720228, 1383.825374438059953, 244.9784035970620266 ) ) ;
#73836 = CARTESIAN_POINT ( 'NONE',  ( -16.26078157602950114, 1501.999196264480133, 224.5383738374800089 ) ) ;
#73837 = CARTESIAN_POINT ( 'NONE',  ( -15.59061307530000029, 1507.637957906029897, 192.6843184329979977 ) ) ;
#73838 = CARTESIAN_POINT ( 'NONE',  ( -11.41402561306639996, 1500.969831351809944, 208.5831151434670119 ) ) ;
#73839 = CARTESIAN_POINT ( 'NONE',  ( 2.095292362720000412, 1464.774291476929875, 236.0651601893980001 ) ) ;
#73841 = EDGE_LOOP ( 'NONE', ( #42685, #72397, #50699, #46240 ) ) ;
#73840 = CARTESIAN_POINT ( 'NONE',  ( 0.7098482576299989244, 1456.796867040289953, 219.7430208676990162 ) ) ;
#73842 = CARTESIAN_POINT ( 'NONE',  ( -0.7457676837669999781, 1451.082419665830002, 182.3677269424979954 ) ) ;
#73843 = CARTESIAN_POINT ( 'NONE',  ( -31.25669922000000156, 1381.487600021890103, 207.4386042761090039 ) ) ;
#73844 = CARTESIAN_POINT ( 'NONE',  ( 3.545811734658929737, 1508.551704408389924, 204.3700499762609866 ) ) ;
#73846 = VERTEX_POINT ( 'NONE', #80597 ) ;
#73845 = CARTESIAN_POINT ( 'NONE',  ( -18.20034151899999841, 1415.948532224930204, 208.7150056808090142 ) ) ;
#73847 = CARTESIAN_POINT ( 'NONE',  ( 19.03958733774129897, 1453.804075884379927, 200.7927936193499932 ) ) ;
#73848 = ORIENTED_EDGE ( 'NONE', *, *, #59607, .F. ) ;
#73849 = CARTESIAN_POINT ( 'NONE',  ( -7.798852395605240240, 1385.469439152710038, 218.8921415146500067 ) ) ;
#73850 = CARTESIAN_POINT ( 'NONE',  ( -2.936817763033160222, 1515.374151778960140, 204.8620682627120004 ) ) ;
#73851 = CARTESIAN_POINT ( 'NONE',  ( -17.83486663330526767, 1523.678648413191695, 180.3677388339002334 ) ) ;
#73852 = CARTESIAN_POINT ( 'NONE',  ( -11.60004869885203505, 1426.637431940826900, 134.7518097448552794 ) ) ;
#73853 = CARTESIAN_POINT ( 'NONE',  ( -105.1998544249999981, 1380.198630363649954, 300.9198567136589872 ) ) ;
#73854 = CARTESIAN_POINT ( 'NONE',  ( 31.23437356469446868, 1512.187213306747481, 222.8968241038843701 ) ) ;
#73855 = CARTESIAN_POINT ( 'NONE',  ( 19.76910848268742882, 1509.626936452628797, 187.0485031433751999 ) ) ;
#73856 = CARTESIAN_POINT ( 'NONE',  ( 12.48631014972050046, 1409.349091945879991, 200.9084573645220075 ) ) ;
#73857 = CARTESIAN_POINT ( 'NONE',  ( 18.80431613299999682, 1425.839299934830024, 225.4579059055980110 ) ) ;
#73858 = CARTESIAN_POINT ( 'NONE',  ( 12.55979069370000012, 1458.679714032590027, 224.9161459441990019 ) ) ;
#73859 = CARTESIAN_POINT ( 'NONE',  ( 15.95461386393500369, 1514.857962383129916, 193.9637614619669819 ) ) ;
#73860 = CARTESIAN_POINT ( 'NONE',  ( 26.86204993032690069, 1508.007394616730153, 206.2315948942269870 ) ) ;
#73861 = CARTESIAN_POINT ( 'NONE',  ( -2.289270335424059777, 1449.884603672450112, 183.2456841540659980 ) ) ;
#73862 = ORIENTED_EDGE ( 'NONE', *, *, #56227, .F. ) ;
#73863 = DIRECTION ( 'NONE',  ( 1.755985294532464991E-16, -1.000000000000000000, 1.338183447452830017E-16 ) ) ;
#73864 = DIRECTION ( 'NONE',  ( 0.000000000000000000, 1.000000000000000000, 0.000000000000000000 ) ) ;
#73865 = CARTESIAN_POINT ( 'NONE',  ( -2.500000000000000000, 1439.615672362210034, 183.5288080682979910 ) ) ;
#73866 = CARTESIAN_POINT ( 'NONE',  ( 12.68557844200520002, 1420.747169022329899, 201.7075646973950143 ) ) ;
#73867 = CARTESIAN_POINT ( 'NONE',  ( -20.41179666374959822, 1501.768784456520052, 190.5662750394010061 ) ) ;
#73868 = CARTESIAN_POINT ( 'NONE',  ( -14.86383190760000161, 1420.231781918219895, 213.2204302019290196 ) ) ;
#73869 = CARTESIAN_POINT ( 'NONE',  ( -108.8231103770000061, 1386.831205869259975, 310.8600928752589425 ) ) ;
#73870 = CARTESIAN_POINT ( 'NONE',  ( -7.708815826551380646, 1516.526058373149908, 211.4663580544020078 ) ) ;
#73871 = CARTESIAN_POINT ( 'NONE',  ( -9.505471540885778836, 1363.500209798504102, 210.6218459616991936 ) ) ;
#73872 = CARTESIAN_POINT ( 'NONE',  ( -46.27886737059069588, 1440.913065768309934, 267.5894398601490138 ) ) ;
#73873 = DIRECTION ( 'NONE',  ( -0.000000000000000000, -1.000000000000000000, -0.000000000000000000 ) ) ;
#73874 = CARTESIAN_POINT ( 'NONE',  ( -20.42459865780000072, 1488.376572794829826, 192.7920252002980135 ) ) ;
#73875 = CARTESIAN_POINT ( 'NONE',  ( -6.563915562015000482, 1517.184063036290127, 207.9975562766469750 ) ) ;
#73876 = CARTESIAN_POINT ( 'NONE',  ( -8.894458315472089538, 1449.037666247089874, 211.3340079007809891 ) ) ;
#73877 = CARTESIAN_POINT ( 'NONE',  ( 1.284229296498709871, 1407.590765714829786, 222.1854359568369830 ) ) ;
#73878 = CARTESIAN_POINT ( 'NONE',  ( -13.36099673570619828, 1435.014160632789981, 149.5726766897830089 ) ) ;
#73879 = SURFACE_STYLE_USAGE ( .BOTH. , #39715 ) ;
#73880 = CARTESIAN_POINT ( 'NONE',  ( 5.850881932830000132, 1422.777642752129850, 112.2633461691979875 ) ) ;
#73881 = CARTESIAN_POINT ( 'NONE',  ( 7.417280415950580519, 1425.156060753129850, 212.4179085937329887 ) ) ;
#73882 = ORIENTED_EDGE ( 'NONE', *, *, #92452, .T. ) ;
#73883 = CARTESIAN_POINT ( 'NONE',  ( 39.71667994350000441, 1440.913060391249928, 259.0958843719980109 ) ) ;
#73884 = CARTESIAN_POINT ( 'NONE',  ( -19.63722818156799832, 1519.551704408389924, 200.0074286628000095 ) ) ;
#73886 = DIRECTION ( 'NONE',  ( 0.9786619618251657382, 0.000000000000000000, -0.2054769195713184449 ) ) ;
#73885 = CARTESIAN_POINT ( 'NONE',  ( -0.5171656703849999426, 1486.441294966730084, 181.7112151590980034 ) ) ;
#73887 = EDGE_CURVE ( 'NONE', #56546, #50244, #76967, .T. ) ;
#73888 = CARTESIAN_POINT ( 'NONE',  ( 20.59848286226652903, 1506.575640307617050, 201.1096833366487147 ) ) ;
#73889 = CARTESIAN_POINT ( 'NONE',  ( -27.78131445089999829, 1437.273604214180068, 231.6915032127979828 ) ) ;
#73890 = CARTESIAN_POINT ( 'NONE',  ( -29.50368436323640609, 1509.962337460696517, 206.4587159585742597 ) ) ;
#73891 = EDGE_CURVE ( 'NONE', #10257, #54321, #17640, .T. ) ;
#73892 = CARTESIAN_POINT ( 'NONE',  ( -8.399306680986638796, 1452.619750134839933, 151.1947243576269955 ) ) ;
#73893 = CARTESIAN_POINT ( 'NONE',  ( 27.44752899740000274, 1451.502705272029971, 136.1440125272980026 ) ) ;
#73894 = ORIENTED_EDGE ( 'NONE', *, *, #26859, .F. ) ;
#73895 = CARTESIAN_POINT ( 'NONE',  ( -107.7635570413719961, 1378.913060387369796, 300.2373514716429668 ) ) ;
#73896 = DIRECTION ( 'NONE',  ( -0.000000000000000000, -1.000000000000000000, -0.000000000000000000 ) ) ;
#73897 = CARTESIAN_POINT ( 'NONE',  ( -112.5224174381096276, 1308.913060387289988, 304.7012714958631818 ) ) ;
#73898 = CARTESIAN_POINT ( 'NONE',  ( 16.81223453394349932, 1414.913060391199906, 210.6693087035600058 ) ) ;
#73899 = ORIENTED_EDGE ( 'NONE', *, *, #78055, .T. ) ;
#73900 = ORIENTED_EDGE ( 'NONE', *, *, #41147, .T. ) ;
#73901 = CARTESIAN_POINT ( 'NONE',  ( -6.354804813069999447, 1384.643210436399841, 199.7268052247689809 ) ) ;
#73902 = CARTESIAN_POINT ( 'NONE',  ( -22.91026015634600199, 1409.742958369740109, 209.5388009460739909 ) ) ;
#73903 = ORIENTED_EDGE ( 'NONE', *, *, #96141, .F. ) ;
#73904 = CARTESIAN_POINT ( 'NONE',  ( 4.556910988561660325, 1508.729442836390035, 205.2988677068620120 ) ) ;
#73905 = FACE_OUTER_BOUND ( 'NONE', #17613, .T. ) ;
#73906 = CARTESIAN_POINT ( 'NONE',  ( -3.905916658650000262, 1507.638362680030014, 236.6212078316980012 ) ) ;
#73907 = CARTESIAN_POINT ( 'NONE',  ( 2.487923051973920163, 1508.611354625609920, 213.7999901942370116 ) ) ;
#73908 = CARTESIAN_POINT ( 'NONE',  ( 43.50346336978830664, 1452.801732798669946, 268.2946146135880099 ) ) ;
#73909 = CARTESIAN_POINT ( 'NONE',  ( -12.98785519611649875, 1415.943166310999914, 221.7006290623930056 ) ) ;
#73910 = CARTESIAN_POINT ( 'NONE',  ( 0.07377261094400000552, 1419.750880451330204, 184.3782704745979686 ) ) ;
#73911 = CARTESIAN_POINT ( 'NONE',  ( -7.334957394705000411, 1517.030858226499959, 204.5055736355369902 ) ) ;
#73912 = VERTEX_POINT ( 'NONE', #90633 ) ;
#73913 = CARTESIAN_POINT ( 'NONE',  ( 11.44787351428849931, 1480.383220438659919, 211.9499576844269768 ) ) ;
#73914 = CARTESIAN_POINT ( 'NONE',  ( 14.72576938353500076, 1512.123542805230272, 196.9321265835669976 ) ) ;
#73915 = CARTESIAN_POINT ( 'NONE',  ( 13.20732832327373885, 1443.125461821982526, 187.5576213471996994 ) ) ;
#73916 = ORIENTED_EDGE ( 'NONE', *, *, #91840, .T. ) ;
#73917 = ORIENTED_EDGE ( 'NONE', *, *, #4420, .T. ) ;
#73918 = CARTESIAN_POINT ( 'NONE',  ( 2.686147501205802701, 1526.329757971589515, 176.3936480404081237 ) ) ;
#73919 = CARTESIAN_POINT ( 'NONE',  ( 8.062587302181759341, 1436.235894220949831, 206.1282943059349861 ) ) ;
#73920 = CARTESIAN_POINT ( 'NONE',  ( -4.315706650834171931, 1423.871734710937062, 184.5076872321269263 ) ) ;
#73921 = CARTESIAN_POINT ( 'NONE',  ( 6.713174362274499707, 1504.508803738159941, 219.9706393884620184 ) ) ;
#73922 = CARTESIAN_POINT ( 'NONE',  ( 12.10433974340000063, 1420.521815624170131, 199.8646142222890205 ) ) ;
#73923 = CARTESIAN_POINT ( 'NONE',  ( 19.17520749770000066, 1455.940066015489947, 211.9422318690290012 ) ) ;
#73924 = CARTESIAN_POINT ( 'NONE',  ( -109.0753561177834285, 1382.030600553431668, 297.5814012535014967 ) ) ;
#73925 = CARTESIAN_POINT ( 'NONE',  ( 10.55201363404730230, 1479.182026721460034, 205.9886858934539760 ) ) ;
#73926 = PLANE ( 'NONE',  #28507 ) ;
#73928 = CARTESIAN_POINT ( 'NONE',  ( -106.4049054108890004, 1391.248032509690120, 307.7491839806990015 ) ) ;
#73927 = CARTESIAN_POINT ( 'NONE',  ( 30.15498091547360460, 1525.730671948510917, 196.9950492442363270 ) ) ;
#73929 = CARTESIAN_POINT ( 'NONE',  ( 10.93408409447810037, 1423.050204788569999, 206.8916427814799874 ) ) ;
#73930 = CARTESIAN_POINT ( 'NONE',  ( -24.10874530002790195, 1508.417687901419868, 222.3557339921229925 ) ) ;
#73931 = CARTESIAN_POINT ( 'NONE',  ( 2.409586283469999923, 1426.663880916129983, 144.1938086916980239 ) ) ;
#73932 = ORIENTED_EDGE ( 'NONE', *, *, #2511, .F. ) ;
#73933 = CARTESIAN_POINT ( 'NONE',  ( 11.09668834239110069, 1414.913057819769847, 222.2791104406980196 ) ) ;
#73934 = FACE_OUTER_BOUND ( 'NONE', #9706, .T. ) ;
#73935 = CARTESIAN_POINT ( 'NONE',  ( -94.05214484065579938, 1384.960168895200013, 309.8416638810129484 ) ) ;
#73936 = CARTESIAN_POINT ( 'NONE',  ( -9.216856378879999312, 1385.697103985929971, 200.0334226857090130 ) ) ;
#73937 = CARTESIAN_POINT ( 'NONE',  ( 10.82744550939999861, 1427.328225570349787, 209.3701112376719777 ) ) ;
#73938 =( BOUNDED_SURFACE ( )  B_SPLINE_SURFACE ( 3, 2, ( 
 ( #5783, #99808, #98721 ),
 ( #21981, #91435, #14711 ),
 ( #13590, #4138, #56173 ),
 ( #80283, #64048, #97631 ),
 ( #55099, #89225, #46698 ),
 ( #29862, #21438, #32070 ) ),
 .UNSPECIFIED., .F., .F., .F. ) 
 B_SPLINE_SURFACE_WITH_KNOTS ( ( 4, 2, 4 ),
 ( 3, 3 ),
 ( -4.293440603042597559E-17, 0.001312027981647320837, 0.002624055963294684608 ),
 ( 0.000000000000000000, 1.000000000000000000 ),
 .UNSPECIFIED. ) 
 GEOMETRIC_REPRESENTATION_ITEM ( )  RATIONAL_B_SPLINE_SURFACE ( (
 ( 1.000000000000000000, 0.9376006582765885611, 1.000000000000000000),
 ( 1.000000000000000000, 0.9569320108022199012, 1.000000000000000000),
 ( 1.000000000000000000, 0.9725743441619376650, 1.000000000000000000),
 ( 1.000000000000000000, 0.9942095667135113501, 1.000000000000000000),
 ( 1.000000000000000000, 1.000043666450747493, 1.000000000000000000),
 ( 1.000000000000000000, 1.000000000000000000, 1.000000000000000000) ) ) 
 REPRESENTATION_ITEM ( '' )  SURFACE ( )  );
#73940 = VERTEX_POINT ( 'NONE', #21196 ) ;
#73939 = CARTESIAN_POINT ( 'NONE',  ( 11.13844977941739778, 1424.861034171799929, 203.0515873249630090 ) ) ;
#73941 = CARTESIAN_POINT ( 'NONE',  ( 2.191891361270000171, 1430.523720098889953, 217.5805868065489790 ) ) ;
#73942 = CARTESIAN_POINT ( 'NONE',  ( 22.91663120903140083, 1507.606285602550088, 210.6365840681099826 ) ) ;
#73943 = CARTESIAN_POINT ( 'NONE',  ( -3.657993755839999750, 1474.872004365689918, 218.7367895275489786 ) ) ;
#73944 = CARTESIAN_POINT ( 'NONE',  ( 11.88150807299999911, 1433.590365853900039, 150.5399244709980167 ) ) ;
#73945 = ADVANCED_FACE ( 'NONE', ( #99576 ), #13915, .F. ) ;
#73946 = CARTESIAN_POINT ( 'NONE',  ( 8.562340737000068813, 1433.778957528687442, 204.3790743423090248 ) ) ;
#73947 = FACE_OUTER_BOUND ( 'NONE', #23747, .T. ) ;
#73948 = CARTESIAN_POINT ( 'NONE',  ( 3.974701152529080073, 1457.344300949599983, 199.5572480904559995 ) ) ;
#73949 = CARTESIAN_POINT ( 'NONE',  ( -107.0452211441419621, 1390.407136375272330, 299.6009371605423439 ) ) ;
#73950 = CIRCLE ( 'NONE', #36372, 1.999999999999999556 ) ;
#73951 = CARTESIAN_POINT ( 'NONE',  ( 15.81588731469999942, 1422.108138393630043, 227.5712429109979951 ) ) ;
#73952 = CARTESIAN_POINT ( 'NONE',  ( 0.9862806562982793235, 1410.322815818307618, 232.9487999948802610 ) ) ;
#73953 = CARTESIAN_POINT ( 'NONE',  ( -22.08327125186962192, 1523.604703353109699, 184.4267662568474009 ) ) ;
#73954 = SPHERICAL_SURFACE ( 'NONE', #3449, 2.000000000000000000 ) ;
#73955 = CARTESIAN_POINT ( 'NONE',  ( 5.511665417999469900E-05, 1508.970066526555001, 238.8757070596369942 ) ) ;
#73957 = B_SPLINE_CURVE_WITH_KNOTS ( 'NONE', 3,
 ( #70762, #61799, #52286, #53385 ),
 .UNSPECIFIED., .F., .F.,
 ( 4, 4 ),
 ( -19.44060205079999903, -0.6888856060759991351 ),
 .UNSPECIFIED. ) ;
#73956 = CARTESIAN_POINT ( 'NONE',  ( -20.30852359509999872, 1486.101457756589753, 213.0654537167889657 ) ) ;
#73958 = CARTESIAN_POINT ( 'NONE',  ( 4.781276783620000081, 1452.020048942890071, 190.5513815401990030 ) ) ;
#73959 = DIRECTION ( 'NONE',  ( 0.000000000000000000, 0.000000000000000000, -1.000000000000000000 ) ) ;
#73960 = CARTESIAN_POINT ( 'NONE',  ( 1.454938208119999965, 1515.064792882589927, 204.7923971856590128 ) ) ;
#73961 = CARTESIAN_POINT ( 'NONE',  ( -0.5770119038902318254, 1525.581535527370534, 174.8524476110295325 ) ) ;
#73962 = CARTESIAN_POINT ( 'NONE',  ( 9.373950541344202136, 1512.187213306747481, 228.8708405320806492 ) ) ;
#73963 = CARTESIAN_POINT ( 'NONE',  ( -10.58917179050000001, 1416.519106787530063, 223.7522405382979684 ) ) ;
#73964 = CARTESIAN_POINT ( 'NONE',  ( 0.2176556265100970111, 1453.071422968439947, 183.2503276199190339 ) ) ;
#73965 = CARTESIAN_POINT ( 'NONE',  ( -10.09629858792809820, 1408.224493087130213, 200.4271526767499836 ) ) ;
#73966 = CARTESIAN_POINT ( 'NONE',  ( -17.23902921200000193, 1416.518938591829965, 202.8396764550879823 ) ) ;
#73967 = CARTESIAN_POINT ( 'NONE',  ( -28.85025895338739588, 1509.857219934619934, 211.4429886291059972 ) ) ;
#73968 = CARTESIAN_POINT ( 'NONE',  ( 12.06109101570000064, 1433.903535342440136, 148.5015073091980184 ) ) ;
#73969 = CARTESIAN_POINT ( 'NONE',  ( -27.26082647600000186, 1435.920819023299828, 136.5169790846980220 ) ) ;
#73970 = CARTESIAN_POINT ( 'NONE',  ( 10.96698248110000051, 1442.551897621980061, 185.4780326627980003 ) ) ;
#73971 = ORIENTED_EDGE ( 'NONE', *, *, #39743, .T. ) ;
#73972 = CARTESIAN_POINT ( 'NONE',  ( -1.835774698489999857, 1484.769563356690014, 198.4308759197990071 ) ) ;
#73973 = CARTESIAN_POINT ( 'NONE',  ( -11.60004869885203860, 1428.965959225140750, 137.0999999980979851 ) ) ;
#73974 = CARTESIAN_POINT ( 'NONE',  ( -108.4397519767807552, 1383.495406804093136, 310.9866756129748069 ) ) ;
#73975 = CARTESIAN_POINT ( 'NONE',  ( -11.40503445839999941, 1490.739836597089834, 209.6941760096060250 ) ) ;
#73976 = EDGE_CURVE ( 'NONE', #87520, #96030, #86341, .T. ) ;
#73977 = CARTESIAN_POINT ( 'NONE',  ( -1.297832609859999931, 1452.391379596130037, 183.7169094889979988 ) ) ;
#73978 = CARTESIAN_POINT ( 'NONE',  ( 14.88455046320870068, 1507.555441264370074, 232.3243942964739972 ) ) ;
#73979 = CARTESIAN_POINT ( 'NONE',  ( 39.98720484010659248, 1424.431172289532697, 269.1289939770674664 ) ) ;
#73980 = CARTESIAN_POINT ( 'NONE',  ( -19.57278477748463530, 1493.745073078330051, 189.3793122366375030 ) ) ;
#73981 = CARTESIAN_POINT ( 'NONE',  ( -13.67445017210000024, 1380.322169305999978, 210.0770191355990164 ) ) ;
#73982 = CARTESIAN_POINT ( 'NONE',  ( -21.96543842109194600, 1523.313115944345327, 182.9844783913652861 ) ) ;
#73983 = CARTESIAN_POINT ( 'NONE',  ( -51.00415357460500587, 1385.022678461219812, 226.8415894493760163 ) ) ;
#73984 = CARTESIAN_POINT ( 'NONE',  ( -19.37774363895776730, 1525.878013734318984, 236.8539400710568259 ) ) ;
#73985 = CARTESIAN_POINT ( 'NONE',  ( -26.79413315976150045, 1435.433175095809929, 135.2874648155150226 ) ) ;
#73986 = EDGE_LOOP ( 'NONE', ( #34214, #106005, #36737, #83374 ) ) ;
#73987 = CARTESIAN_POINT ( 'NONE',  ( 16.56942828594079842, 1526.189892541618974, 182.6454327952257302 ) ) ;
#73988 = CARTESIAN_POINT ( 'NONE',  ( -16.18192080235260022, 1409.728958692500100, 226.0642444559119895 ) ) ;
#73990 = ORIENTED_EDGE ( 'NONE', *, *, #93355, .T. ) ;
#73989 = CARTESIAN_POINT ( 'NONE',  ( -11.75869035857540013, 1519.551704408389924, 190.9442076533970010 ) ) ;
#73991 = DIRECTION ( 'NONE',  ( 3.772597702940000410E-15, 3.330669073880000444E-15, -1.000000000000000000 ) ) ;
#73992 = CARTESIAN_POINT ( 'NONE',  ( 10.01012151112310100, 1469.368595336919952, 209.9818033434729898 ) ) ;
#73993 = B_SPLINE_CURVE_WITH_KNOTS ( 'NONE', 5,
 ( #41860, #35111, #34007, #76013, #77135, #102304, #110166, #49727, #16621, #42409, #25591, #17726, #59782, #93902, #17168 ),
 .UNSPECIFIED., .F., .F.,
 ( 6, 3, 3, 3, 6 ),
 ( 7.637039622810000594, 10.13387562650000007, 11.38229362830000113, 12.23404602909999994, 12.63071163020000043 ),
 .UNSPECIFIED. ) ;
#73994 = FACE_OUTER_BOUND ( 'NONE', #40363, .T. ) ;
#73995 = CARTESIAN_POINT ( 'NONE',  ( -109.6606343030000090, 1384.812795754960007, 311.3218902852589736 ) ) ;
#73996 = DIRECTION ( 'NONE',  ( 1.439455173507210273E-14, 1.000000000000000000, 2.465190328815660140E-31 ) ) ;
#73997 = CARTESIAN_POINT ( 'NONE',  ( 0.4259571265750000113, 1466.740460378930038, 235.5880773660980196 ) ) ;
#73998 = CARTESIAN_POINT ( 'NONE',  ( 18.08473414950000091, 1409.544593222829917, 221.2175231340980019 ) ) ;
#73999 = LINE ( 'NONE', #66171, #85911 ) ;
#74000 = CARTESIAN_POINT ( 'NONE',  ( -19.67777960560400174, 1467.001721752909816, 204.2858066586710208 ) ) ;
#74001 = CARTESIAN_POINT ( 'NONE',  ( -17.17385843950000179, 1423.847787907029897, 228.5629967713979909 ) ) ;
#74003 = CARTESIAN_POINT ( 'NONE',  ( 1.228114002177200126, 1450.757138880049979, 181.5372592238319953 ) ) ;
#74002 = CARTESIAN_POINT ( 'NONE',  ( -4.551369695278060235, 1511.401872466681198, 200.7475796568508599 ) ) ;
#74004 = CARTESIAN_POINT ( 'NONE',  ( 26.57998359885230144, 1469.327412704790049, 209.4675454856640044 ) ) ;
#74005 = CARTESIAN_POINT ( 'NONE',  ( -119.7254833230812636, 1314.643966242390889, 293.5583688343593280 ) ) ;
#74006 = CARTESIAN_POINT ( 'NONE',  ( 3.820260774390000039E-10, 1453.313060387329870, 228.7984261690980077 ) ) ;
#74007 = B_SPLINE_CURVE_WITH_KNOTS ( 'NONE', 3,
 ( #108109, #108669, #39818, #40908 ),
 .UNSPECIFIED., .F., .F.,
 ( 4, 4 ),
 ( 29.60747119820000250, 29.67279265790000053 ),
 .UNSPECIFIED. ) ;
#74008 = CARTESIAN_POINT ( 'NONE',  ( -17.55491153119999836, 1504.812299793789862, 208.9605407232590153 ) ) ;
#74009 = CARTESIAN_POINT ( 'NONE',  ( -5.023678250220539709, 1375.295974637168456, 203.5210896577872859 ) ) ;
#74010 = CARTESIAN_POINT ( 'NONE',  ( -5.786527600464999033, 1517.025653221279981, 205.6708125431369751 ) ) ;
#74011 = CARTESIAN_POINT ( 'NONE',  ( -6.599338478058309754, 1485.999004717200023, 182.7565567968090079 ) ) ;
#74012 = EDGE_LOOP ( 'NONE', ( #79887, #50378, #982, #83666, #24951 ) ) ;
#74013 = CARTESIAN_POINT ( 'NONE',  ( 2.640434834157764143, 1526.748660780343471, 176.9315852594520777 ) ) ;
#74015 = ORIENTED_EDGE ( 'NONE', *, *, #74452, .F. ) ;
#74014 = CARTESIAN_POINT ( 'NONE',  ( -68.54059710952350315, 1379.747571644130176, 280.1307283583089998 ) ) ;
#74016 = EDGE_LOOP ( 'NONE', ( #2091, #16437, #87896, #31022, #14776 ) ) ;
#74017 = CARTESIAN_POINT ( 'NONE',  ( -8.417565570956876186, 1381.789049435770949, 218.2528661022787162 ) ) ;
#74018 = ORIENTED_EDGE ( 'NONE', *, *, #49453, .T. ) ;
#74019 = CARTESIAN_POINT ( 'NONE',  ( -11.81780673814840021, 1522.051704408389924, 222.7166774759110126 ) ) ;
#74020 = ADVANCED_FACE ( 'NONE', ( #64362 ), #59786, .T. ) ;
#74021 = CARTESIAN_POINT ( 'NONE',  ( 12.53292608669999986, 1500.050071955789917, 207.1420395195890194 ) ) ;
#74023 = CARTESIAN_POINT ( 'NONE',  ( 15.93480775089659751, 1410.857278985090034, 191.5296905502239895 ) ) ;
#74022 = CARTESIAN_POINT ( 'NONE',  ( -10.81674490862216587, 1424.920146621146387, 144.2681340705726996 ) ) ;
#74024 = EDGE_CURVE ( 'NONE', #37961, #29868, #84449, .T. ) ;
#74025 = CARTESIAN_POINT ( 'NONE',  ( 6.951517132375000685, 1517.194816588360027, 210.2467400204669730 ) ) ;
#74026 = ADVANCED_FACE ( 'NONE', ( #109116 ), #28557, .T. ) ;
#74027 = CARTESIAN_POINT ( 'NONE',  ( -107.1098322795840119, 1378.913060387289988, 307.3359821571719976 ) ) ;
#74028 = DIRECTION ( 'NONE',  ( 3.469446951953611033E-14, 0.000000000000000000, 1.000000000000000000 ) ) ;
#74029 = EDGE_CURVE ( 'NONE', #28705, #96418, #2715, .T. ) ;
#74030 = CARTESIAN_POINT ( 'NONE',  ( 12.45931607057640100, 1501.250537210039965, 211.6676667882360050 ) ) ;
#74031 = EDGE_CURVE ( 'NONE', #54902, #36343, #60365, .T. ) ;
#74032 = CARTESIAN_POINT ( 'NONE',  ( 38.87405678795120423, 1449.786581495179917, 134.0999999981590065 ) ) ;
#74033 = FACE_OUTER_BOUND ( 'NONE', #107056, .T. ) ;
#74034 = ORIENTED_EDGE ( 'NONE', *, *, #74444, .F. ) ;
#74035 = CARTESIAN_POINT ( 'NONE',  ( -4.705736654490000781, 1479.984769897790102, 230.9466533013989817 ) ) ;
#74036 = CARTESIAN_POINT ( 'NONE',  ( -18.64140136670000203, 1458.043073665729935, 227.4221190980979941 ) ) ;
#74037 = ORIENTED_EDGE ( 'NONE', *, *, #61122, .F. ) ;
#74038 = ORIENTED_EDGE ( 'NONE', *, *, #51945, .T. ) ;
#74039 = CIRCLE ( 'NONE', #107978, 7.999657266239995401 ) ;
#74040 = EDGE_CURVE ( 'NONE', #58638, #4755, #34021, .T. ) ;
#74041 = CARTESIAN_POINT ( 'NONE',  ( 7.859233469507785230, 1410.563491206050458, 230.5393502882801897 ) ) ;
#74042 = CARTESIAN_POINT ( 'NONE',  ( 3.774742873677630645E-15, 1432.353321343819971, 155.3998100167600001 ) ) ;
#74043 = DIRECTION ( 'NONE',  ( 0.000000000000000000, 0.000000000000000000, -1.000000000000000000 ) ) ;
#74044 = CARTESIAN_POINT ( 'NONE',  ( -18.42382187532859916, 1508.551704391109979, 210.1329842148610112 ) ) ;
#74045 = CARTESIAN_POINT ( 'NONE',  ( -2.500000000000000000, 1439.624612762049992, 169.0979939332570154 ) ) ;
#74046 = CARTESIAN_POINT ( 'NONE',  ( -14.49997346389999997, 1379.670736723790014, 208.2214565508510020 ) ) ;
#74047 = CARTESIAN_POINT ( 'NONE',  ( 40.71747596219820053, 1448.637563214439979, 135.0591086893190038 ) ) ;
#74048 = CARTESIAN_POINT ( 'NONE',  ( -8.986359071028783063, 1482.816979524136059, 227.9996318485843005 ) ) ;
#74049 = PLANE ( 'NONE',  #40940 ) ;
#74050 = CYLINDRICAL_SURFACE ( 'NONE', #18133, 0.9999999999999976685 ) ;
#74051 = ADVANCED_FACE ( 'NONE', ( #86650 ), #104003, .F. ) ;
#74052 = CARTESIAN_POINT ( 'NONE',  ( -67.67528647966889821, 1384.722340586130031, 260.9666397543829817 ) ) ;
#74053 = ORIENTED_EDGE ( 'NONE', *, *, #82556, .T. ) ;
#74054 = CARTESIAN_POINT ( 'NONE',  ( 4.615644804385000022, 1517.009964551830080, 202.1744681489270192 ) ) ;
#74055 = CARTESIAN_POINT ( 'NONE',  ( 3.447128460625000113, 1516.778853242349896, 207.9866608880570027 ) ) ;
#74056 = ORIENTED_EDGE ( 'NONE', *, *, #110696, .T. ) ;
#74057 = CARTESIAN_POINT ( 'NONE',  ( 36.80170786347940037, 1440.913060387330006, 263.3930352349019586 ) ) ;
#74058 = B_SPLINE_CURVE_WITH_KNOTS ( 'NONE', 3,
 ( #6461, #15931, #74239, #23791, #74780, #24346, #84261, #50134, #82622, #92114 ),
 .UNSPECIFIED., .F., .F.,
 ( 4, 2, 2, 2, 4 ),
 ( 0.000000000000000000, 0.2500000000000000000, 0.5000000000000000000, 0.7500000000000000000, 1.000000000000000000 ),
 .UNSPECIFIED. ) ;
#74059 = CARTESIAN_POINT ( 'NONE',  ( -0.0002133035632435401063, 1452.198735795263474, 153.8525164413085804 ) ) ;
#74060 = ORIENTED_EDGE ( 'NONE', *, *, #76681, .T. ) ;
#74061 = CARTESIAN_POINT ( 'NONE',  ( -33.92644755664575484, 1451.728309075015204, 135.1499336227579420 ) ) ;
#74062 = CARTESIAN_POINT ( 'NONE',  ( 8.060623735539611090, 1428.631035214050144, 214.1143366338490068 ) ) ;
#74063 = DIRECTION ( 'NONE',  ( 0.9858563016923833633, 0.000000000000000000, 0.1675928173085483863 ) ) ;
#74064 = EDGE_CURVE ( 'NONE', #61100, #53370, #42990, .T. ) ;
#74065 = CARTESIAN_POINT ( 'NONE',  ( 33.93019615848945847, 1512.187213306747481, 197.6607374645996060 ) ) ;
#74066 = CARTESIAN_POINT ( 'NONE',  ( -12.87559654649999885, 1416.820969729929857, 221.9332893899980093 ) ) ;
#74067 = CARTESIAN_POINT ( 'NONE',  ( -107.4576978852700080, 1306.483669372790018, 307.4681403979390097 ) ) ;
#74068 = CARTESIAN_POINT ( 'NONE',  ( -2.864908171889999799, 1508.665746313929958, 180.3512637796979732 ) ) ;
#74069 = EDGE_CURVE ( 'NONE', #52697, #15766, #88867, .T. ) ;
#74070 = CARTESIAN_POINT ( 'NONE',  ( -11.87595595039999807, 1433.006363244510112, 146.4341588726979921 ) ) ;
#74071 = PLANE ( 'NONE',  #85725 ) ;
#74073 = CARTESIAN_POINT ( 'NONE',  ( -11.60004869885203860, 1422.222932908415032, 137.0999999980989230 ) ) ;
#74072 = CARTESIAN_POINT ( 'NONE',  ( 13.98523055529999937, 1460.766604684630011, 232.5051451957979793 ) ) ;
#74074 = CARTESIAN_POINT ( 'NONE',  ( 0.000000000000000000, 1526.382868172863937, 209.1218459616979999 ) ) ;
#74075 = PRESENTATION_LAYER_ASSIGNMENT (  '', '', ( #102645 ) ) ;
#74076 = CARTESIAN_POINT ( 'NONE',  ( 7.329925222404999552, 1516.833976295079992, 216.8387248732070134 ) ) ;
#74077 = VERTEX_POINT ( 'NONE', #73737 ) ;
#74078 = EDGE_CURVE ( 'NONE', #106610, #66046, #39472, .T. ) ;
#74079 = LINE ( 'NONE', #57831, #8624 ) ;
#74080 = CARTESIAN_POINT ( 'NONE',  ( -0.08433784210662320646, 1508.474253462899924, 180.2861765906610003 ) ) ;
#74081 = CARTESIAN_POINT ( 'NONE',  ( 19.24684531284998457, 1443.257586225273144, 213.2797261564643634 ) ) ;
#74082 = CARTESIAN_POINT ( 'NONE',  ( -7.322709724964999722, 1516.596789218710001, 212.3828531017969965 ) ) ;
#74083 = CARTESIAN_POINT ( 'NONE',  ( 18.59400664349999843, 1508.850372361629979, 188.2535539507980218 ) ) ;
#74084 = CARTESIAN_POINT ( 'NONE',  ( -11.60004869885203682, 1426.433005303874552, 138.8017569497143029 ) ) ;
#74086 = EDGE_LOOP ( 'NONE', ( #57187, #9991, #107336, #62353 ) ) ;
#74085 = CARTESIAN_POINT ( 'NONE',  ( -12.16530128034490055, 1501.737063442450108, 211.5189884477989892 ) ) ;
#74087 = CARTESIAN_POINT ( 'NONE',  ( -17.24701964721560543, 1523.844782250842172, 237.3932573007202222 ) ) ;
#74088 = CARTESIAN_POINT ( 'NONE',  ( 23.21471032630000053, 1448.940680683610026, 217.4907001339380201 ) ) ;
#74089 = CARTESIAN_POINT ( 'NONE',  ( -11.84024944870000162, 1430.562290793029888, 149.6945522165979980 ) ) ;
#74090 = CARTESIAN_POINT ( 'NONE',  ( -15.80167951410000171, 1415.804990609770130, 209.5032351745619792 ) ) ;
#74091 = CARTESIAN_POINT ( 'NONE',  ( -66.58099742339999239, 1379.774555183159919, 276.6312621969589713 ) ) ;
#74092 = CARTESIAN_POINT ( 'NONE',  ( -5.923682464646780943, 1522.051704408389924, 223.8623791742500089 ) ) ;
#74093 = CARTESIAN_POINT ( 'NONE',  ( 7.758184319229999737, 1421.576654411539948, 195.8091089427989857 ) ) ;
#74094 = CARTESIAN_POINT ( 'NONE',  ( 12.39622442890000009, 1445.662712069799909, 187.7408842649980159 ) ) ;
#74095 = B_SPLINE_CURVE_WITH_KNOTS ( 'NONE', 3,
 ( #85072, #59361, #43095, #33018, #8364, #25708, #33559, #24052, #94577, #102971, #67204, #68318, #101864, #41989, #59909, #77256, #26269, #16201, #60459, #94030, #49847, #58246, #17852, #66660, #92368, #83978, #101303, #58790, #36888 ),
 .UNSPECIFIED., .F., .F.,
 ( 4, 2, 2, 2, 1, 1, 2, 2, 2, 2, 1, 1, 1, 2, 2, 2, 4 ),
 ( 0.000000000000000000, 0.2499999999996999067, 0.3749999999995535238, 0.4374999999994803046, 0.4687499999995227706, 0.4843749999995431432, 0.4921874999994815814, 0.4999999999994200195, 0.6249999999994992894, 0.6874999999994761968, 0.7187499999994140243, 0.7343749999993890443, 0.7421874999993431921, 0.7460937499993604005, 0.7499999999993776090, 0.8749999999996888045, 1.000000000000000000 ),
 .UNSPECIFIED. ) ;
#74097 = CARTESIAN_POINT ( 'NONE',  ( -6.075418287417217122, 1422.570870580908149, 139.1419350296167750 ) ) ;
#74096 = CARTESIAN_POINT ( 'NONE',  ( -21.39643523319999829, 1470.084198994129792, 223.9144824582980107 ) ) ;
#74098 = CARTESIAN_POINT ( 'NONE',  ( -2.596287949829999775, 1485.851551602029986, 182.3980973359980169 ) ) ;
#74099 = EDGE_LOOP ( 'NONE', ( #31633, #76938, #102616, #109693 ) ) ;
#74100 = CARTESIAN_POINT ( 'NONE',  ( -5.011678876155000850, 1516.989560013210166, 205.8658785457569991 ) ) ;
#74101 = CARTESIAN_POINT ( 'NONE',  ( 12.70479734420000106, 1407.160844702129907, 267.1691044294979633 ) ) ;
#74102 = CARTESIAN_POINT ( 'NONE',  ( 0.04703880850090000343, 1408.914703018729824, 186.4620821680980214 ) ) ;
#74103 = CARTESIAN_POINT ( 'NONE',  ( 17.80682964389999867, 1410.881321328729882, 193.1487614658980192 ) ) ;
#74104 = EDGE_CURVE ( 'NONE', #103213, #80324, #18727, .T. ) ;
#74105 = CARTESIAN_POINT ( 'NONE',  ( 24.52504064068541823, 1438.798626852492362, 212.6115771953019191 ) ) ;
#74106 = EDGE_CURVE ( 'NONE', #24288, #100109, #89546, .T. ) ;
#74107 = CARTESIAN_POINT ( 'NONE',  ( 1.989421934769288303, 1464.165607546044384, 199.5054174974058299 ) ) ;
#74108 = CARTESIAN_POINT ( 'NONE',  ( -0.4967073565345429542, 1415.438070636819930, 233.3911243540180180 ) ) ;
#74109 = DIRECTION ( 'NONE',  ( -0.2907001422290489967, -0.4501984363202189976, 0.8442835988237840095 ) ) ;
#74110 = CARTESIAN_POINT ( 'NONE',  ( -0.5709835574781669809, 1450.893121202140037, 154.5155306351130093 ) ) ;
#74111 = CARTESIAN_POINT ( 'NONE',  ( -12.33291429870000044, 1446.185421286020073, 187.5047377990980237 ) ) ;
#74112 = CARTESIAN_POINT ( 'NONE',  ( -19.85687491537112948, 1485.534782846681765, 190.5734348709216022 ) ) ;
#74113 = CARTESIAN_POINT ( 'NONE',  ( -14.14026437170590000, 1415.666200591660072, 221.0665809521190113 ) ) ;
#74114 = CARTESIAN_POINT ( 'NONE',  ( -10.92081006369999940, 1499.922668861390093, 212.8248374489089940 ) ) ;
#74115 = CARTESIAN_POINT ( 'NONE',  ( -8.276897555935638806, 1409.202096019020019, 196.6540098276539936 ) ) ;
#74116 = AXIS2_PLACEMENT_3D ( 'NONE', #86294, #93575, #16850 ) ;
#74117 = EDGE_CURVE ( 'NONE', #28394, #11116, #81608, .T. ) ;
#74118 = CARTESIAN_POINT ( 'NONE',  ( 10.88870480703258181, 1425.078866303880886, 139.1353458172395392 ) ) ;
#74119 = CARTESIAN_POINT ( 'NONE',  ( 2.500000056489999789, 1440.197744908439972, 166.9350760962979905 ) ) ;
#74120 = CARTESIAN_POINT ( 'NONE',  ( -2.086529340449999825, 1475.285345059530073, 269.4971841000979680 ) ) ;
#74121 = CARTESIAN_POINT ( 'NONE',  ( -4.228535446720999680, 1446.279644958110111, 165.3431147484849930 ) ) ;
#74122 = DIRECTION ( 'NONE',  ( 0.01258894674767200433, 0.9999149092275962936, 0.003419462553138305841 ) ) ;
#74123 = CARTESIAN_POINT ( 'NONE',  ( 13.74310390781900004, 1522.051704408389924, 217.0905615615409943 ) ) ;
#74124 = CARTESIAN_POINT ( 'NONE',  ( -53.35900147057170528, 1384.724215327180218, 268.5776327521460303 ) ) ;
#74125 = CARTESIAN_POINT ( 'NONE',  ( -106.7981877087919997, 1391.913060387289988, 302.1811662082889711 ) ) ;
#74126 = AXIS2_PLACEMENT_3D ( 'NONE', #30878, #89688, #47700 ) ;
#74127 = LINE ( 'NONE', #30996, #18159 ) ;
#74128 = B_SPLINE_SURFACE_WITH_KNOTS ( 'NONE', 5, 5, ( 
 ( #108927, #75877, #32217, #83175, #24350, #67496 ),
 ( #40065, #5919, #58536, #31656, #92661, #6465 ),
 ( #15936, #109483, #40614, #74785, #42271, #92120 ),
 ( #50139, #24884, #84266, #41716, #110025, #33301 ),
 ( #101600, #17024, #110575, #33860, #102160, #51222 ),
 ( #10318, #85355, #68593, #94881, #78077, #60190 ),
 ( #840, #17588, #25992, #69148, #1380, #94309 ),
 ( #28231, #102698, #35522, #61320, #51787, #43932 ),
 ( #53456, #103253, #76988, #36635, #70831, #27682 ) ),
 .UNSPECIFIED., .F., .F., .F.,
 ( 6, 3, 6 ),
 ( 6, 6 ),
 ( 0.000000000000000000, 1.406546626929999988, 2.813093253849999975 ),
 ( 0.000000000000000000, 2.000000000000000000 ),
 .UNSPECIFIED. ) ;
#74129 = CARTESIAN_POINT ( 'NONE',  ( 12.30756928984159870, 1491.905514282249896, 208.5176378714709813 ) ) ;
#74130 = CARTESIAN_POINT ( 'NONE',  ( -19.34601893677229967, 1526.333389948038530, 185.2009018889136200 ) ) ;
#74131 = CARTESIAN_POINT ( 'NONE',  ( 8.374229031442469662, 1511.401878032981131, 204.5705829445117274 ) ) ;
#74132 = CARTESIAN_POINT ( 'NONE',  ( 4.900006679340000559, 1499.255191946190052, 229.7873568473989963 ) ) ;
#74133 = CARTESIAN_POINT ( 'NONE',  ( 12.86007276073260108, 1421.274266495399843, 205.3533571373839948 ) ) ;
#74134 = EDGE_CURVE ( 'NONE', #39656, #101005, #90939, .T. ) ;
#74135 = CARTESIAN_POINT ( 'NONE',  ( -41.06045305519999289, 1425.496138736429884, 269.1004795120979907 ) ) ;
#74136 = EDGE_LOOP ( 'NONE', ( #37139, #14961, #85029, #91177, #58286, #22787 ) ) ;
#74137 = B_SPLINE_SURFACE_WITH_KNOTS ( 'NONE', 5, 1, ( 
 ( #106195, #72604 ),
 ( #29477, #105663 ),
 ( #64215, #63672 ),
 ( #13212, #47402 ),
 ( #4825, #38971 ),
 ( #73150, #107293 ) ),
 .UNSPECIFIED., .F., .F., .F.,
 ( 6, 6 ),
 ( 2, 2 ),
 ( 0.000000000000000000, 17.81543997039999994 ),
 ( 0.000000000000000000, 14.00000000000000000 ),
 .UNSPECIFIED. ) ;
#74138 = CARTESIAN_POINT ( 'NONE',  ( -8.494778598486192323, 1410.581904811623190, 230.3839334887708503 ) ) ;
#74139 = CARTESIAN_POINT ( 'NONE',  ( -13.59453042928210031, 1507.871302099940067, 209.3931762073830214 ) ) ;
#74140 = CARTESIAN_POINT ( 'NONE',  ( 20.81805263692159969, 1457.016373647149976, 206.8941932428749908 ) ) ;
#74142 = CARTESIAN_POINT ( 'NONE',  ( -1.547462741870939906, 1414.913060391199906, 225.9340804956229931 ) ) ;
#74141 = CARTESIAN_POINT ( 'NONE',  ( 11.54052597689999970, 1425.927346755429880, 137.4287998514980131 ) ) ;
#74143 = CARTESIAN_POINT ( 'NONE',  ( 17.72016947435118084, 1524.201816949777140, 237.7555919081156617 ) ) ;
#74144 = CARTESIAN_POINT ( 'NONE',  ( 12.66727660429999958, 1410.284599989729941, 190.2680586556980131 ) ) ;
#74145 = EDGE_CURVE ( 'NONE', #90411, #97290, #66441, .T. ) ;
#74146 = CARTESIAN_POINT ( 'NONE',  ( -4.686874221129999185, 1454.311615498590072, 200.8248795411589924 ) ) ;
#74147 = CARTESIAN_POINT ( 'NONE',  ( -7.331183129075000693, 1516.882217593000178, 202.1801186797769674 ) ) ;
#74148 = CARTESIAN_POINT ( 'NONE',  ( 7.647272590590000974, 1426.541769689450120, 212.1576498646190032 ) ) ;
#74149 = CARTESIAN_POINT ( 'NONE',  ( -13.15726454016349933, 1414.996443537369942, 220.4820293315119955 ) ) ;
#74150 = CARTESIAN_POINT ( 'NONE',  ( 16.20447078603499946, 1512.376261820769969, 197.7654888015669883 ) ) ;
#74151 = CIRCLE ( 'NONE', #31444, 1.000000000000000888 ) ;
#74152 = FACE_BOUND ( 'NONE', #36967, .T. ) ;
#74153 = CARTESIAN_POINT ( 'NONE',  ( -28.76043848733170094, 1380.228231663270208, 215.0391681145920018 ) ) ;
#74154 = CARTESIAN_POINT ( 'NONE',  ( 21.22263075940009713, 1509.591229450340052, 229.2473791923050044 ) ) ;
#74156 = ORIENTED_EDGE ( 'NONE', *, *, #90539, .F. ) ;
#74155 = CARTESIAN_POINT ( 'NONE',  ( 17.38482601099109814, 1410.884446382940041, 192.4603632472940262 ) ) ;
#74157 = ORIENTED_EDGE ( 'NONE', *, *, #41416, .T. ) ;
#74158 = CARTESIAN_POINT ( 'NONE',  ( -5.426610168820000801, 1398.074626792930076, 221.4287301764979929 ) ) ;
#74159 = CARTESIAN_POINT ( 'NONE',  ( -21.03404397679999960, 1411.006872173530155, 218.3490652940980112 ) ) ;
#74160 = EDGE_LOOP ( 'NONE', ( #41335, #60432, #55341, #50192 ) ) ;
#74161 = CARTESIAN_POINT ( 'NONE',  ( -12.78521579352120874, 1444.986520829063011, 169.4510614378021103 ) ) ;
#74162 = EDGE_CURVE ( 'NONE', #345, #30629, #39914, .T. ) ;
#74163 = CARTESIAN_POINT ( 'NONE',  ( -24.72367498159999855, 1509.776430142329900, 194.9388027315980025 ) ) ;
#74164 = CARTESIAN_POINT ( 'NONE',  ( -7.774021443175000101, 1512.205735116489905, 211.9443100603170080 ) ) ;
#74166 = DIRECTION ( 'NONE',  ( 0.9858563016923833633, 0.000000000000000000, 0.1675928173085483863 ) ) ;
#74165 = CARTESIAN_POINT ( 'NONE',  ( 2.989015302459999912, 1446.190165938789960, 199.4457794469589942 ) ) ;
#74167 = AXIS2_PLACEMENT_3D ( 'NONE', #55779, #12085, #97745 ) ;
#74168 = CARTESIAN_POINT ( 'NONE',  ( 0.5282840713740000194, 1449.243076562319857, 183.4277266703979876 ) ) ;
#74169 = ADVANCED_FACE ( 'NONE', ( #42312 ), #70590, .F. ) ;
#74170 = CARTESIAN_POINT ( 'NONE',  ( -3.240770211191819961, 1463.391176810840079, 199.8726916786840206 ) ) ;
#74171 = CARTESIAN_POINT ( 'NONE',  ( 7.722580314274999580, 1517.051704408389924, 209.1218459511669892 ) ) ;
#74172 = FILL_AREA_STYLE_COLOUR ( '', #43160 ) ;
#74173 = CARTESIAN_POINT ( 'NONE',  ( 10.86624720370559949, 1396.292518101280166, 211.2454897527340165 ) ) ;
#74174 = CARTESIAN_POINT ( 'NONE',  ( 1.163296394699999903, 1415.996778985530000, 190.3611342671979969 ) ) ;
#74175 = CARTESIAN_POINT ( 'NONE',  ( 11.54437222630000015, 1429.905666691229953, 150.7682469490980282 ) ) ;
#74176 = ORIENTED_EDGE ( 'NONE', *, *, #106852, .T. ) ;
#74177 = CARTESIAN_POINT ( 'NONE',  ( 12.96886119409670002, 1435.558602358280041, 150.5951603274380091 ) ) ;
#74178 = CARTESIAN_POINT ( 'NONE',  ( 1.694697516987165420, 1450.498567134253790, 181.7745810472625578 ) ) ;
#74179 = ORIENTED_EDGE ( 'NONE', *, *, #55101, .T. ) ;
#74180 = ORIENTED_EDGE ( 'NONE', *, *, #66456, .T. ) ;
#74181 = CARTESIAN_POINT ( 'NONE',  ( 9.786977751178733698, 1521.951704408389787, 226.9642986345448890 ) ) ;
#74182 = CARTESIAN_POINT ( 'NONE',  ( 8.653423937779999520, 1367.169888897630017, 207.6218459616989946 ) ) ;
#74183 = CARTESIAN_POINT ( 'NONE',  ( -109.9907908981719231, 1385.097515532879925, 311.4537231510988136 ) ) ;
#74184 = CARTESIAN_POINT ( 'NONE',  ( 7.718134629434999283, 1516.881930554049859, 216.4517759834270123 ) ) ;
#74185 = CARTESIAN_POINT ( 'NONE',  ( -13.76314899857599983, 1380.295045644700167, 209.3459254739570099 ) ) ;
#74186 = ADVANCED_FACE ( 'NONE', ( #103297 ), #25775, .F. ) ;
#74187 = EDGE_CURVE ( 'NONE', #32820, #39464, #65747, .T. ) ;
#74188 = B_SPLINE_CURVE_WITH_KNOTS ( 'NONE', 5,
 ( #34430, #42279, #8659, #51795, #33868, #26002 ),
 .UNSPECIFIED., .F., .F.,
 ( 6, 6 ),
 ( -1.999999981381699987, 0.000000000000000000 ),
 .UNSPECIFIED. ) ;
#74189 = ORIENTED_EDGE ( 'NONE', *, *, #79743, .F. ) ;
#74190 = CARTESIAN_POINT ( 'NONE',  ( -11.44093224520000085, 1503.454049389589727, 207.5539012139990120 ) ) ;
#74191 = CARTESIAN_POINT ( 'NONE',  ( 17.71193101166619854, 1519.551704408389924, 196.6727161458730109 ) ) ;
#74192 = CARTESIAN_POINT ( 'NONE',  ( -29.63091391959999754, 1379.920694154159946, 213.7170380699990062 ) ) ;
#74193 = CARTESIAN_POINT ( 'NONE',  ( -2.492130661305000050, 1516.778761582560037, 205.6761608547170113 ) ) ;
#74194 = VERTEX_POINT ( 'NONE', #39426 ) ;
#74195 = CARTESIAN_POINT ( 'NONE',  ( -7.337297350114999617, 1517.135701590510052, 208.3821536943570152 ) ) ;
#74196 = CARTESIAN_POINT ( 'NONE',  ( -9.126765308707120994, 1450.806276981840028, 207.6833491750169856 ) ) ;
#74197 = CARTESIAN_POINT ( 'NONE',  ( -16.29362902913419120, 1412.794248246716506, 269.3703535479344851 ) ) ;
#74198 = CARTESIAN_POINT ( 'NONE',  ( 6.462730625455000322, 1512.074228085019968, 217.6482617061570011 ) ) ;
#74200 = ORIENTED_EDGE ( 'NONE', *, *, #96960, .T. ) ;
#74199 = CARTESIAN_POINT ( 'NONE',  ( 0.2193365490036129906, 1416.521607925270018, 227.1760551913189659 ) ) ;
#74201 = ADVANCED_FACE ( 'NONE', ( #32130 ), #66315, .F. ) ;
#74202 = CARTESIAN_POINT ( 'NONE',  ( 2.500000000000000000, 1419.382882622020134, 144.1048175974189860 ) ) ;
#74203 = CARTESIAN_POINT ( 'NONE',  ( -31.32171718324010357, 1440.913060388459826, 242.2919686410689906 ) ) ;
#74204 = AXIS2_PLACEMENT_3D ( 'NONE', #54786, #13842, #48590 ) ;
#74205 = CARTESIAN_POINT ( 'NONE',  ( -32.09555170170000338, 1384.821019989420165, 229.9571600258589967 ) ) ;
#74206 = CARTESIAN_POINT ( 'NONE',  ( -0.1883026784911550067, 1465.099972048609970, 237.0083040624210184 ) ) ;
#74207 = B_SPLINE_CURVE_WITH_KNOTS ( 'NONE', 5,
 ( #103845, #102709, #10898, #96557, #103263, #94320 ),
 .UNSPECIFIED., .F., .F.,
 ( 6, 6 ),
 ( -1.452619041900000019, -1.364055982389089650E-06 ),
 .UNSPECIFIED. ) ;
#74208 = CARTESIAN_POINT ( 'NONE',  ( 5.402393448019999767, 1407.889686284330082, 270.1311850753980366 ) ) ;
#74210 = ADVANCED_FACE ( 'NONE', ( #93663 ), #18673, .F. ) ;
#74209 = VECTOR ( 'NONE', #55073, 999.9999999999998863 ) ;
#74211 = CARTESIAN_POINT ( 'NONE',  ( -3.254401441735000233, 1516.919782530640077, 213.1645757730269963 ) ) ;
#74212 = AXIS2_PLACEMENT_3D ( 'NONE', #72877, #39817, #13482 ) ;
#74213 = CARTESIAN_POINT ( 'NONE',  ( 22.80370811929999775, 1409.709376436929915, 209.3213622003410137 ) ) ;
#74214 = CARTESIAN_POINT ( 'NONE',  ( -20.24816999180000110, 1507.884035326030016, 189.2341655923979999 ) ) ;
#74215 = CARTESIAN_POINT ( 'NONE',  ( 2.395822483399999925, 1441.661856669790041, 218.7568551047190226 ) ) ;
#74216 = CARTESIAN_POINT ( 'NONE',  ( -7.709125739314820258, 1516.537893464249919, 211.6437737813369893 ) ) ;
#74217 = CARTESIAN_POINT ( 'NONE',  ( 5.013429356055000063, 1517.123342927159911, 210.2437967141769946 ) ) ;
#74218 = DIRECTION ( 'NONE',  ( 1.000000000000000000, -0.000000000000000000, 1.224646799147353207E-16 ) ) ;
#74219 = B_SPLINE_CURVE_WITH_KNOTS ( 'NONE', 3,
 ( #37745, #62427, #95991, #70837 ),
 .UNSPECIFIED., .F., .F.,
 ( 4, 4 ),
 ( 7.974131824220000553, 16.25123407829999778 ),
 .UNSPECIFIED. ) ;
#74220 = FACE_OUTER_BOUND ( 'NONE', #40109, .T. ) ;
#74221 = CARTESIAN_POINT ( 'NONE',  ( 10.97048253690000053, 1432.408103991110011, 151.7701133072980042 ) ) ;
#74223 = ORIENTED_EDGE ( 'NONE', *, *, #74104, .F. ) ;
#74222 = CARTESIAN_POINT ( 'NONE',  ( -39.64020011839999569, 1388.419118112470187, 238.6562341694589975 ) ) ;
#74224 = CARTESIAN_POINT ( 'NONE',  ( -53.58581700929299529, 1385.100721272199962, 269.0214992842330162 ) ) ;
#74225 = CARTESIAN_POINT ( 'NONE',  ( 30.31940284292408805, 1523.382868172864164, 195.7503880523414352 ) ) ;
#74226 = LINE ( 'NONE', #83155, #19923 ) ;
#74227 = CARTESIAN_POINT ( 'NONE',  ( -2.079673249558308346, 1495.029477387638508, 220.0949141771806126 ) ) ;
#74228 = CARTESIAN_POINT ( 'NONE',  ( -5.439673085259999041, 1437.306888043809977, 154.7134238268980084 ) ) ;
#74229 = CARTESIAN_POINT ( 'NONE',  ( 12.74373164180000018, 1426.782509952399778, 204.7461156749990039 ) ) ;
#74230 = CARTESIAN_POINT ( 'NONE',  ( -11.90000415720300175, 1434.913060496859998, 147.6452464505769910 ) ) ;
#74232 = DIRECTION ( 'NONE',  ( 0.2302114497549562488, 0.7071067811868637643, 0.6685825965438183527 ) ) ;
#74231 = CARTESIAN_POINT ( 'NONE',  ( -4.616272334694999202, 1517.030858226499959, 216.4568033268070053 ) ) ;
#74233 = CARTESIAN_POINT ( 'NONE',  ( -32.38845791999504797, 1523.382868172864164, 202.1182848005516348 ) ) ;
#74234 = CARTESIAN_POINT ( 'NONE',  ( 32.99911596133151193, 1524.244163922423695, 222.0809728102182135 ) ) ;
#74235 = ORIENTED_EDGE ( 'NONE', *, *, #48155, .T. ) ;
#74236 = CARTESIAN_POINT ( 'NONE',  ( -0.01073133209419849937, 1516.939491476980038, 201.7897819926569980 ) ) ;
#74237 = CARTESIAN_POINT ( 'NONE',  ( -15.26322412056499900, 1511.857118786289902, 221.3099577525670156 ) ) ;
#74238 = ORIENTED_EDGE ( 'NONE', *, *, #70755, .T. ) ;
#74239 = CARTESIAN_POINT ( 'NONE',  ( 6.036759309035796939, 1509.035273820309612, 216.5824821311529433 ) ) ;
#74240 = AXIS2_PLACEMENT_3D ( 'NONE', #77756, #78299, #1612 ) ;
#74241 = CARTESIAN_POINT ( 'NONE',  ( 24.39988810369999683, 1444.709222782450070, 214.8827041012880272 ) ) ;
#74242 = CARTESIAN_POINT ( 'NONE',  ( 7.922665854446364619, 1438.183228455332710, 153.7218973692720283 ) ) ;
#74243 = CARTESIAN_POINT ( 'NONE',  ( 9.367332565670180244, 1425.287430459912912, 195.5756684483055494 ) ) ;
#74244 = CARTESIAN_POINT ( 'NONE',  ( -1.009278519650000039, 1444.031905486989899, 218.1361756941589931 ) ) ;
#74245 = CARTESIAN_POINT ( 'NONE',  ( 15.20786797544739422, 1420.724135117424112, 227.8586414243133902 ) ) ;
#74246 = CARTESIAN_POINT ( 'NONE',  ( 39.87271423621129429, 1446.097205234940020, 136.7849415641429971 ) ) ;
#74247 = CARTESIAN_POINT ( 'NONE',  ( -18.79768836659999565, 1425.701458444829996, 225.3470275129980109 ) ) ;
#74248 = CARTESIAN_POINT ( 'NONE',  ( -23.41638159929999929, 1435.743789844690127, 140.4321931749979910 ) ) ;
#74249 = CARTESIAN_POINT ( 'NONE',  ( -107.0577634130000035, 1388.202339906730003, 298.5958247604589815 ) ) ;
#74250 = CARTESIAN_POINT ( 'NONE',  ( 17.96015235289999978, 1488.325118637129890, 189.1250949044980132 ) ) ;
#74251 = CARTESIAN_POINT ( 'NONE',  ( -105.4593524120000012, 1391.263056100180165, 303.4133042968589962 ) ) ;
#74252 = AXIS2_PLACEMENT_3D ( 'NONE', #42771, #103782, #33252 ) ;
#74253 = CARTESIAN_POINT ( 'NONE',  ( -33.82528723393350845, 1458.993493484178998, 269.5158104617022445 ) ) ;
#74254 = VERTEX_POINT ( 'NONE', #94226 ) ;
#74255 = LINE ( 'NONE', #108386, #15705 ) ;
#74256 = CARTESIAN_POINT ( 'NONE',  ( 1.756561144747210293E-16, 1391.913060387289988, 209.1218459572589836 ) ) ;
#74257 = CARTESIAN_POINT ( 'NONE',  ( 11.26824400833899986, 1470.496689712369971, 207.5795241769199890 ) ) ;
#74258 = CARTESIAN_POINT ( 'NONE',  ( -8.010413950200000244, 1453.313060387329870, 227.4940039322979999 ) ) ;
#74259 = CARTESIAN_POINT ( 'NONE',  ( -1.065145167260631354, 1486.514686996405544, 181.6828421078873248 ) ) ;
#74260 = CARTESIAN_POINT ( 'NONE',  ( -13.03778803710101997, 1442.976472216123284, 186.5873176571947738 ) ) ;
#74261 = B_SPLINE_SURFACE_WITH_KNOTS ( 'NONE', 5, 5, ( 
 ( #57728, #74522, #40341, #56056, #90746, #48216, #14025, #56610, #41461 ),
 ( #90183, #14583, #33037, #31940, #58265, #15659, #75623, #82355, #5655 ),
 ( #75073, #48771, #99680, #81784, #91846, #5086, #15123, #83997, #82897 ),
 ( #13466, #32507, #99129, #6734, #31388, #22408, #39803, #22972, #57178 ),
 ( #39239, #65569, #73414, #91300, #107550, #100782, #109222, #73963, #30837 ),
 ( #66135, #66677, #108653, #109757, #108093, #24073, #67225, #92386, #100256 ) ),
 .UNSPECIFIED., .F., .F., .F.,
 ( 6, 6 ),
 ( 6, 3, 6 ),
 ( 39.30568950680000029, 56.26183429820000015 ),
 ( 0.000000000000000000, 1.000000000000000000, 2.000000000000000000 ),
 .UNSPECIFIED. ) ;
#74262 = CARTESIAN_POINT ( 'NONE',  ( -9.978843980182551476, 1439.175531641559928, 209.1458737907410068 ) ) ;
#74263 = CARTESIAN_POINT ( 'NONE',  ( 2.947604512712040048, 1495.328382756780002, 220.7041825259470045 ) ) ;
#74264 = DIRECTION ( 'NONE',  ( -0.000000000000000000, -1.000000000000000000, -0.000000000000000000 ) ) ;
#74265 = CARTESIAN_POINT ( 'NONE',  ( -14.43789412238549907, 1415.677402204810051, 205.2933806555749925 ) ) ;
#74266 = CARTESIAN_POINT ( 'NONE',  ( 24.53658740500000235, 1435.634184005399902, 137.4974649685979955 ) ) ;
#74267 =( BOUNDED_CURVE ( )  B_SPLINE_CURVE ( 3, ( #20669, #37498, #97400, #54870 ),
 .UNSPECIFIED., .F., .F. ) 
 B_SPLINE_CURVE_WITH_KNOTS ( ( 4, 4 ),
 ( 2.890157662648249914, 3.288561242448070132 ),
 .UNSPECIFIED. ) 
 CURVE ( )  GEOMETRIC_REPRESENTATION_ITEM ( )  RATIONAL_B_SPLINE_CURVE ( ( 1.000000000000000000, 0.9868165636475595415, 0.9868165636475595415, 1.000000000000000000 ) ) 
 REPRESENTATION_ITEM ( '' )  );
#74268 = CARTESIAN_POINT ( 'NONE',  ( -18.17365796220000007, 1441.208305948289762, 213.5442559039389891 ) ) ;
#74270 = VERTEX_POINT ( 'NONE', #42190 ) ;
#74269 = CARTESIAN_POINT ( 'NONE',  ( -4.026786250540000722, 1408.413060387330006, 121.6099336315979969 ) ) ;
#74271 = EDGE_CURVE ( 'NONE', #328, #26746, #109252, .T. ) ;
#74272 = CARTESIAN_POINT ( 'NONE',  ( -98.72417372059999252, 1381.942632977169751, 297.0446025502590146 ) ) ;
#74273 = CARTESIAN_POINT ( 'NONE',  ( 12.82673415024670049, 1512.305164330090065, 224.2762155789449992 ) ) ;
#74274 = ORIENTED_EDGE ( 'NONE', *, *, #53075, .T. ) ;
#74275 = ORIENTED_EDGE ( 'NONE', *, *, #54969, .T. ) ;
#74276 = CARTESIAN_POINT ( 'NONE',  ( -12.69354645500000167, 1502.230858064689983, 210.5965602401589933 ) ) ;
#74277 = DIRECTION ( 'NONE',  ( 0.000000000000000000, 1.000000000000000000, 0.000000000000000000 ) ) ;
#74279 = CARTESIAN_POINT ( 'NONE',  ( -23.04246322899999910, 1448.885557893680016, 216.4413416304380178 ) ) ;
#74278 = CARTESIAN_POINT ( 'NONE',  ( 5.456719627610000067, 1455.595244131089885, 218.2350948550090095 ) ) ;
#74280 = CARTESIAN_POINT ( 'NONE',  ( -20.01144489670000226, 1507.902391332829893, 188.9701987092980175 ) ) ;
#74281 = CARTESIAN_POINT ( 'NONE',  ( -11.50373587760000049, 1433.458593519129863, 151.2690138048979804 ) ) ;
#74282 = CARTESIAN_POINT ( 'NONE',  ( -4.219439023932549659, 1446.230224804030058, 183.1418048969109975 ) ) ;
#74283 = CARTESIAN_POINT ( 'NONE',  ( 9.285715353111019255, 1464.591735933340033, 212.3819174308400193 ) ) ;
#74284 = CARTESIAN_POINT ( 'NONE',  ( -27.11119864980000216, 1438.398422475539974, 136.9641100155979814 ) ) ;
#74285 = CARTESIAN_POINT ( 'NONE',  ( -24.32490777769999823, 1438.502494616239801, 211.0439858967079942 ) ) ;
#74286 = CARTESIAN_POINT ( 'NONE',  ( -3.707546501630690106, 1454.065007432690209, 199.3225983413989866 ) ) ;
#74287 = CARTESIAN_POINT ( 'NONE',  ( 1.916752472390000017, 1450.614851703330260, 182.7228952166980207 ) ) ;
#74288 = CARTESIAN_POINT ( 'NONE',  ( 8.663307226700800001, 1364.047708251303447, 207.6218459616988241 ) ) ;
#74289 = CARTESIAN_POINT ( 'NONE',  ( 33.72300830903895275, 1524.397344074319108, 198.6568221122816453 ) ) ;
#74291 = ORIENTED_EDGE ( 'NONE', *, *, #18490, .F. ) ;
#74290 = CARTESIAN_POINT ( 'NONE',  ( -1.866069976159590112E-09, 1413.704851968730054, 248.6276318723759857 ) ) ;
#74292 = ORIENTED_EDGE ( 'NONE', *, *, #99580, .T. ) ;
#74293 = CARTESIAN_POINT ( 'NONE',  ( -11.86352235238380004, 1432.155850026679900, 149.9794201586200018 ) ) ;
#74294 = AXIS2_PLACEMENT_3D ( 'NONE', #68219, #102324, #59802 ) ;
#74295 = CARTESIAN_POINT ( 'NONE',  ( 19.36069530197559985, 1498.614194606489946, 221.8424376627909851 ) ) ;
#74296 = CARTESIAN_POINT ( 'NONE',  ( -4.281468237010000344, 1473.749348323329968, 270.2892484966980078 ) ) ;
#74297 = CARTESIAN_POINT ( 'NONE',  ( -1.546949757679999760, 1416.828040475729949, 228.0209010782980101 ) ) ;
#74298 = CARTESIAN_POINT ( 'NONE',  ( -8.881784196999999612E-15, 1434.913060387330006, 126.8032249175980155 ) ) ;
#74299 = CARTESIAN_POINT ( 'NONE',  ( -5.013264356158945390, 1375.417427871223254, 214.7179447576116900 ) ) ;
#74300 = CARTESIAN_POINT ( 'NONE',  ( 4.327853128026699636, 1515.125728221819827, 209.9038229511910174 ) ) ;
#74301 = EDGE_CURVE ( 'NONE', #39623, #47286, #86389, .T. ) ;
#74302 = CARTESIAN_POINT ( 'NONE',  ( -7.279378368329999738, 1479.856447813089972, 209.7098936948849826 ) ) ;
#74303 = B_SPLINE_SURFACE_WITH_KNOTS ( 'NONE', 5, 5, ( 
 ( #68741, #96689, #70966, #27266, #96122, #42974 ),
 ( #9909, #19396, #87745, #52487, #105081, #36222 ),
 ( #51927, #984, #70407, #35109, #86069, #35661 ),
 ( #36774, #77133, #104526, #17725, #28370, #439 ),
 ( #34560, #45194, #43529, #94446, #102845, #53600 ),
 ( #69292, #86615, #79335, #103396, #2646, #95573 ) ),
 .UNSPECIFIED., .F., .F., .F.,
 ( 6, 6 ),
 ( 6, 6 ),
 ( 30.67014437039999919, 168.1723206030000028 ),
 ( 0.000000000000000000, 2.000000000000000000 ),
 .UNSPECIFIED. ) ;
#74304 = CARTESIAN_POINT ( 'NONE',  ( 18.25317160297629826, 1431.535582262299840, 208.0285350045080008 ) ) ;
#74305 = CARTESIAN_POINT ( 'NONE',  ( -3.620275138579999830, 1456.955153447490147, 217.9164953791890014 ) ) ;
#74306 = CARTESIAN_POINT ( 'NONE',  ( 10.02176186326848040, 1364.879735892741792, 210.6218459616991936 ) ) ;
#74307 = CARTESIAN_POINT ( 'NONE',  ( -37.50711329737600153, 1420.224927873189927, 268.4873400273870061 ) ) ;
#74308 = ADVANCED_FACE ( 'NONE', ( #85839 ), #8797, .T. ) ;
#74309 = ORIENTED_EDGE ( 'NONE', *, *, #18488, .F. ) ;
#74310 = CARTESIAN_POINT ( 'NONE',  ( -4.327152622306649654, 1515.152479455989806, 209.4468724884619917 ) ) ;
#74311 = ORIENTED_EDGE ( 'NONE', *, *, #98337, .F. ) ;
#74312 = ORIENTED_EDGE ( 'NONE', *, *, #41906, .F. ) ;
#74313 = CARTESIAN_POINT ( 'NONE',  ( 6.562635822504999439, 1517.111322026010157, 211.9927976380170094 ) ) ;
#74314 = EDGE_CURVE ( 'NONE', #95189, #43597, #100262, .T. ) ;
#74315 = CARTESIAN_POINT ( 'NONE',  ( -7.105427357599999217E-15, 1425.413060387329779, 188.2701767054980166 ) ) ;
#74316 = CARTESIAN_POINT ( 'NONE',  ( 4.363122647530000009, 1418.913060387330006, 172.2701767054979882 ) ) ;
#74318 = CARTESIAN_POINT ( 'NONE',  ( -17.64167022720579681, 1419.649359460465575, 207.0478719141029273 ) ) ;
#74317 = CARTESIAN_POINT ( 'NONE',  ( -3.253141175365000137, 1516.858171774179937, 212.3894494859370070 ) ) ;
#74319 = CARTESIAN_POINT ( 'NONE',  ( -17.46563763389999835, 1440.441821941650232, 190.8018186351980034 ) ) ;
#74320 = EDGE_CURVE ( 'NONE', #30404, #29269, #17935, .T. ) ;
#74321 = CARTESIAN_POINT ( 'NONE',  ( 3.453399489167784608, 1420.336197137674162, 144.1207137702020873 ) ) ;
#74322 = ORIENTED_EDGE ( 'NONE', *, *, #78179, .T. ) ;
#74323 = CARTESIAN_POINT ( 'NONE',  ( -26.64524886190000075, 1436.744926164489925, 136.7854674159979993 ) ) ;
#74324 = VECTOR ( 'NONE', #33134, 1000.000000000000000 ) ;
#74325 = CARTESIAN_POINT ( 'NONE',  ( -2.292307268505000106, 1516.548716157039962, 202.1882291110970300 ) ) ;
#74326 = DIRECTION ( 'NONE',  ( 0.2054769195713296304, 0.000000000000000000, 0.9786619618251631847 ) ) ;
#74328 = TOROIDAL_SURFACE ( 'NONE', #8112, 1.000000000000000000, 1.000000000000000000 ) ;
#74327 = LINE ( 'NONE', #81582, #45437 ) ;
#74329 = CARTESIAN_POINT ( 'NONE',  ( 0.05087731831460000353, 1408.368774904629845, 195.5796676385980106 ) ) ;
#74330 = DIRECTION ( 'NONE',  ( -0.4857256630471089576, -0.7475168770206177538, 0.4530884006756178972 ) ) ;
#74331 = CARTESIAN_POINT ( 'NONE',  ( -5.077127106479999874, 1398.064300162629934, 197.0820720787980065 ) ) ;
#74333 = ORIENTED_EDGE ( 'NONE', *, *, #32256, .T. ) ;
#74332 = CARTESIAN_POINT ( 'NONE',  ( -7.950364260026115737, 1365.038675628758710, 209.6218459617148824 ) ) ;
#74334 = ORIENTED_EDGE ( 'NONE', *, *, #91748, .T. ) ;
#74335 = CARTESIAN_POINT ( 'NONE',  ( -11.87109248081550028, 1432.710597699950085, 149.9814569640180082 ) ) ;
#74336 = CARTESIAN_POINT ( 'NONE',  ( 3.777455811129835084, 1425.600239829200063, 185.2244255622378262 ) ) ;
#74337 = CARTESIAN_POINT ( 'NONE',  ( 10.81529792403469870, 1460.553129422620032, 207.5316501181210072 ) ) ;
#74338 = CARTESIAN_POINT ( 'NONE',  ( 2.864888263988467632, 1368.214942817531437, 207.6218459616987957 ) ) ;
#74339 = CARTESIAN_POINT ( 'NONE',  ( -0.6863442344880000823, 1485.336931685030095, 181.8984760979980138 ) ) ;
#74340 = EDGE_CURVE ( 'NONE', #99409, #15055, #94862, .T. ) ;
#74341 = CARTESIAN_POINT ( 'NONE',  ( -4.608146819384999482, 1516.677239312369920, 211.4179708211670174 ) ) ;
#74342 = CARTESIAN_POINT ( 'NONE',  ( -68.78852321903210054, 1379.747967857259937, 280.2968415580110673 ) ) ;
#74343 = CARTESIAN_POINT ( 'NONE',  ( 5.459750082109999347, 1438.302868353570148, 154.7313708644979897 ) ) ;
#74344 = CARTESIAN_POINT ( 'NONE',  ( 5.039568361674230168, 1440.423861375179968, 217.2666807852390036 ) ) ;
#74345 = LINE ( 'NONE', #84904, #9206 ) ;
#74346 = CARTESIAN_POINT ( 'NONE',  ( 7.564413961465000114, 1511.011611623900080, 205.8421879128569856 ) ) ;
#74347 = CARTESIAN_POINT ( 'NONE',  ( -2.881548462575000080, 1516.909589401870107, 206.8382752989369919 ) ) ;
#74348 = EDGE_CURVE ( 'NONE', #45663, #68424, #108187, .T. ) ;
#74349 = ORIENTED_EDGE ( 'NONE', *, *, #93178, .T. ) ;
#74350 = DIRECTION ( 'NONE',  ( -1.755985294532469921E-16, 1.000000000000000000, -1.338183447452831989E-16 ) ) ;
#74351 = CARTESIAN_POINT ( 'NONE',  ( -11.01123599387699947, 1428.984116122770047, 91.31161349935790383 ) ) ;
#74352 = CARTESIAN_POINT ( 'NONE',  ( -19.59613263891256452, 1457.072187391607486, 225.8973385439780088 ) ) ;
#74353 = VERTEX_POINT ( 'NONE', #57085 ) ;
#74354 = DIRECTION ( 'NONE',  ( -0.6709778558543728622, 0.000000000000000000, 0.7414773880254666993 ) ) ;
#74355 = CARTESIAN_POINT ( 'NONE',  ( 13.02629732915830019, 1434.894639379329874, 149.7937853367240280 ) ) ;
#74356 = CARTESIAN_POINT ( 'NONE',  ( 13.57674101270000122, 1415.245980409429876, 197.2205466607979929 ) ) ;
#74357 = CARTESIAN_POINT ( 'NONE',  ( -17.48895720149999988, 1417.651609471990014, 206.3668144019989938 ) ) ;
#74358 = CARTESIAN_POINT ( 'NONE',  ( 4.500000000000000000, 1448.210448412289907, 182.3842140122979743 ) ) ;
#74359 = CARTESIAN_POINT ( 'NONE',  ( 11.78824854703250047, 1517.151704408390060, 211.4132493584619965 ) ) ;
#74360 = CARTESIAN_POINT ( 'NONE',  ( 7.340611670529999522, 1487.529895563990067, 201.1154889873190257 ) ) ;
#74361 = CARTESIAN_POINT ( 'NONE',  ( 30.61443310237131499, 1523.382868172863937, 221.8243310972799236 ) ) ;
#74362 = CARTESIAN_POINT ( 'NONE',  ( 24.33332407789799134, 1445.509459226046147, 214.1965185073686939 ) ) ;
#74363 = CARTESIAN_POINT ( 'NONE',  ( 40.26322134699998401, 1439.095365326212459, 135.2291194917982295 ) ) ;
#74364 = CARTESIAN_POINT ( 'NONE',  ( 16.57641951891043419, 1409.993768444886882, 226.3203854180307815 ) ) ;
#74365 = CARTESIAN_POINT ( 'NONE',  ( -2.290886304614999869, 1517.184383877180153, 216.4605998004670084 ) ) ;
#74366 = ORIENTED_EDGE ( 'NONE', *, *, #41982, .F. ) ;
#74367 = CARTESIAN_POINT ( 'NONE',  ( -17.63541786559999736, 1417.743836435179901, 206.3821828179090119 ) ) ;
#74368 = CARTESIAN_POINT ( 'NONE',  ( -44.93136599389160324, 1440.913052653349951, 269.6838063022050278 ) ) ;
#74369 = CARTESIAN_POINT ( 'NONE',  ( 2.077546474020000034, 1420.933967010829974, 184.3471949240980052 ) ) ;
#74370 = CARTESIAN_POINT ( 'NONE',  ( -14.35866385045889970, 1508.448434989210000, 216.0828215529409988 ) ) ;
#74371 = CIRCLE ( 'NONE', #29659, 0.9999999999999015232 ) ;
#74372 = CARTESIAN_POINT ( 'NONE',  ( -3.410173980340000188, 1476.067642529390241, 219.2827969570990092 ) ) ;
#74373 = CARTESIAN_POINT ( 'NONE',  ( -0.05334543264060000178, 1509.045412427330120, 179.1219820337979911 ) ) ;
#74374 = LINE ( 'NONE', #65977, #42489 ) ;
#74375 = CARTESIAN_POINT ( 'NONE',  ( -3.924179544107323281, 1508.147948383610583, 220.6842618796573845 ) ) ;
#74376 = CARTESIAN_POINT ( 'NONE',  ( -2.500000000000000000, 1428.057245272730142, 156.8186834866980064 ) ) ;
#74377 = CARTESIAN_POINT ( 'NONE',  ( -1.465977870436109942, 1455.136833094290068, 198.7136623775919873 ) ) ;
#74378 = DIRECTION ( 'NONE',  ( -0.9455185755993178454, 0.000000000000000000, 0.3255681544571539243 ) ) ;
#74379 = B_SPLINE_SURFACE_WITH_KNOTS ( 'NONE', 5, 1, ( 
 ( #50541, #24202 ),
 ( #694, #41017 ),
 ( #60052, #34272 ),
 ( #100905, #52203 ),
 ( #41585, #7965 ),
 ( #32628, #60608 ) ),
 .UNSPECIFIED., .F., .F., .F.,
 ( 6, 6 ),
 ( 2, 2 ),
 ( 0.000000000000000000, 16.62916768389999689 ),
 ( 0.000000000000000000, 14.00000000000000000 ),
 .UNSPECIFIED. ) ;
#74380 = CARTESIAN_POINT ( 'NONE',  ( 35.00939270688730431, 1440.913060385989866, 250.9518149144350332 ) ) ;
#74382 = CARTESIAN_POINT ( 'NONE',  ( -4.455702694979999379, 1476.149614445790121, 218.6586916280889739 ) ) ;
#74381 = CARTESIAN_POINT ( 'NONE',  ( -109.1689158750000104, 1385.013785682389880, 297.1335957845589633 ) ) ;
#74383 = CARTESIAN_POINT ( 'NONE',  ( -3.909710721586109550, 1522.051704408389924, 197.7672215555029993 ) ) ;
#74384 = ORIENTED_EDGE ( 'NONE', *, *, #7293, .F. ) ;
#74385 = ORIENTED_EDGE ( 'NONE', *, *, #19277, .F. ) ;
#74386 = CARTESIAN_POINT ( 'NONE',  ( 6.680902021104210498, 1440.813589410888653, 214.8934479320009245 ) ) ;
#74387 = CARTESIAN_POINT ( 'NONE',  ( -19.47602705472021967, 1485.559858681225023, 189.9955089004985780 ) ) ;
#74388 = CARTESIAN_POINT ( 'NONE',  ( -1.927340254199999769, 1443.937843298589996, 199.6634601012389965 ) ) ;
#74389 = CARTESIAN_POINT ( 'NONE',  ( 7.871286969770000752, 1423.706537194029806, 195.8927146150989813 ) ) ;
#74390 = CARTESIAN_POINT ( 'NONE',  ( -0.8775825618903739800, 1380.371560387289946, 209.6012715003031985 ) ) ;
#74391 = CARTESIAN_POINT ( 'NONE',  ( 0.000000000000000000, 1512.187213306747481, 209.1218459616979999 ) ) ;
#74392 = CARTESIAN_POINT ( 'NONE',  ( 0.7436733002139179760, 1508.551704408389924, 219.9150180538129860 ) ) ;
#74393 = CARTESIAN_POINT ( 'NONE',  ( -49.07962222725669932, 1383.813429589529960, 259.4477374396440155 ) ) ;
#74394 = AXIS2_PLACEMENT_3D ( 'NONE', #59646, #5656, #31389 ) ;
#74395 = CARTESIAN_POINT ( 'NONE',  ( -4.987078422688609791, 1508.551704408389924, 206.6339250122549913 ) ) ;
#74396 = CARTESIAN_POINT ( 'NONE',  ( -14.41709712029999935, 1471.312091222230038, 193.4155243667980244 ) ) ;
#74397 = DIRECTION ( 'NONE',  ( 0.000000000000000000, 0.000000000000000000, -1.000000000000000000 ) ) ;
#74398 = CARTESIAN_POINT ( 'NONE',  ( 10.65708661477679975, 1491.469129873149996, 211.9150438862110093 ) ) ;
#74400 = VERTEX_POINT ( 'NONE', #64928 ) ;
#74399 = CARTESIAN_POINT ( 'NONE',  ( 0.1234260537299990135, 1456.953841043490229, 219.7696534638990045 ) ) ;
#74401 = CARTESIAN_POINT ( 'NONE',  ( -1.287812843440000021, 1452.072817564129991, 183.7203104394979789 ) ) ;
#74402 = CARTESIAN_POINT ( 'NONE',  ( -37.20406409030000106, 1384.574232116320218, 210.1855829817990013 ) ) ;
#74403 = CARTESIAN_POINT ( 'NONE',  ( 4.733838391792250633, 1508.551704408389924, 205.5349709131090208 ) ) ;
#74404 = VERTEX_POINT ( 'NONE', #66039 ) ;
#74405 = ORIENTED_EDGE ( 'NONE', *, *, #66692, .F. ) ;
#74406 = AXIS2_PLACEMENT_3D ( 'NONE', #19081, #94708, #10154 ) ;
#74407 =( BOUNDED_CURVE ( )  B_SPLINE_CURVE ( 3, ( #76007, #100107, #23388, #83853 ),
 .UNSPECIFIED., .F., .T. ) 
 B_SPLINE_CURVE_WITH_KNOTS ( ( 4, 4 ),
 ( 2.890157727407254740, 3.288561306705124920 ),
 .UNSPECIFIED. ) 
 CURVE ( )  GEOMETRIC_REPRESENTATION_ITEM ( )  RATIONAL_B_SPLINE_CURVE ( ( 1.000000000000000000, 0.9868165636806693897, 0.9868165636806693897, 1.000000000000000000 ) ) 
 REPRESENTATION_ITEM ( '' )  );
#74408 = DIRECTION ( 'NONE',  ( -0.2673318221160059793, 0.3729039878434610156, -0.8885247957905170191 ) ) ;
#74409 = CARTESIAN_POINT ( 'NONE',  ( -3.983717799494409295, 1515.551844914359890, 206.7919068544310051 ) ) ;
#74411 = CARTESIAN_POINT ( 'NONE',  ( 11.88383461994949997, 1433.642778044820034, 147.6544717983980206 ) ) ;
#74410 = CARTESIAN_POINT ( 'NONE',  ( -11.48266949309999951, 1442.832333866149838, 147.8781297902980043 ) ) ;
#74412 = CARTESIAN_POINT ( 'NONE',  ( -5.976488786809999176, 1464.287555164190053, 199.8460616603990161 ) ) ;
#74413 = CARTESIAN_POINT ( 'NONE',  ( -105.5912118399999997, 1378.611694080989992, 302.9832659653590099 ) ) ;
#74414 = DIRECTION ( 'NONE',  ( 0.000000000000000000, 0.000000000000000000, 1.000000000000000000 ) ) ;
#74415 = CARTESIAN_POINT ( 'NONE',  ( -14.58361734293779932, 1508.551704408389924, 215.2898793084600015 ) ) ;
#74416 = CARTESIAN_POINT ( 'NONE',  ( -8.301987938657498844, 1512.913060387330006, 185.0111222839169898 ) ) ;
#74417 = CARTESIAN_POINT ( 'NONE',  ( 18.52259402964000046, 1425.591791501662101, 225.5512587368259858 ) ) ;
#74418 = FACE_OUTER_BOUND ( 'NONE', #23605, .T. ) ;
#74419 = CARTESIAN_POINT ( 'NONE',  ( 7.823841191072109069, 1434.286212867250015, 204.6742520563170160 ) ) ;
#74420 = CARTESIAN_POINT ( 'NONE',  ( 11.76966145709999978, 1432.350018154600093, 150.8118972717979887 ) ) ;
#74421 = CARTESIAN_POINT ( 'NONE',  ( -4.161605034536901115, 1448.982995605119868, 185.0801909513209864 ) ) ;
#74422 = ORIENTED_EDGE ( 'NONE', *, *, #56997, .F. ) ;
#74423 = B_SPLINE_CURVE_WITH_KNOTS ( 'NONE', 3,
 ( #20933, #69738, #103856, #70297, #61889, #65726, #32109, #14191, #89806, #100411, #4700, #30999, #99289, #23139, #89259, #64635, #47264, #66295, #21474, #12554, #56770, #14748, #90907, #83064, #73020, #22016, #80866, #99846, #38295, #22565, #46732, #55684, #13077, #74131, #47813, #4165, #90344, #72475, #55139, #81948, #30451, #57343, #31548, #98756, #73584, #48378, #91467, #81386, #48935 ),
 .UNSPECIFIED., .F., .F.,
 ( 4, 2, 1, 2, 2, 2, 1, 1, 2, 2, 2, 2, 1, 1, 1, 2, 2, 2, 2, 1, 1, 1, 2, 2, 2, 1, 1, 2, 2, 4 ),
 ( 0.000000000000000000, 0.06250000000038768988, 0.09375000000058156258, 0.1093750000005562634, 0.1250000000005309642, 0.1875000000006294132, 0.2187500000006786516, 0.2343750000007824574, 0.2421875000008341661, 0.2500000000008858470, 0.3750000000014287460, 0.4375000000016672219, 0.4687500000017752466, 0.4843750000018290369, 0.4921875000018212098, 0.4960937500018174906, 0.5000000000018137714, 0.6250000000016393553, 0.6875000000015790702, 0.7187500000015458745, 0.7343750000015293322, 0.7421875000015359936, 0.7460937500015292212, 0.7500000000015223378, 0.8125000000012090329, 0.8437500000010399459, 0.8593750000009554579, 0.8671875000009101608, 0.8750000000008649748, 1.000000000000000000 ),
 .UNSPECIFIED. ) ;
#74424 = CARTESIAN_POINT ( 'NONE',  ( 3.677837710089999800E-15, 1426.566393376330097, 144.1938086916980239 ) ) ;
#74425 = CARTESIAN_POINT ( 'NONE',  ( 18.16363651209229957, 1457.500868343169941, 229.3031588784930079 ) ) ;
#74426 = CARTESIAN_POINT ( 'NONE',  ( -12.17235240719999823, 1434.042297368109985, 149.7137827380979900 ) ) ;
#74427 = CARTESIAN_POINT ( 'NONE',  ( 1.477069687100340089E-10, 1465.967699521269878, 241.3588474068609742 ) ) ;
#74428 = EDGE_CURVE ( 'NONE', #65751, #81551, #28766, .T. ) ;
#74429 = CARTESIAN_POINT ( 'NONE',  ( -20.53900256050109618, 1505.889087235659872, 190.4466324654250116 ) ) ;
#74430 = CARTESIAN_POINT ( 'NONE',  ( -14.99991866480000091, 1420.433500232019924, 212.5351666037989844 ) ) ;
#74431 = CARTESIAN_POINT ( 'NONE',  ( -109.1023536789999895, 1387.345544197499976, 310.8967553272590294 ) ) ;
#74432 = CARTESIAN_POINT ( 'NONE',  ( -0.9046723551649999973, 1484.832931805229919, 182.0120543415980023 ) ) ;
#74433 = CARTESIAN_POINT ( 'NONE',  ( -8.622403150219998480, 1362.632156860360055, 207.6218459616989946 ) ) ;
#74434 = CARTESIAN_POINT ( 'NONE',  ( -45.63701710503070075, 1440.701692410139913, 268.9748479612790106 ) ) ;
#74435 = CARTESIAN_POINT ( 'NONE',  ( -21.29751270369999716, 1429.161938467929986, 221.7940764617979994 ) ) ;
#74436 = CARTESIAN_POINT ( 'NONE',  ( -20.13089310500000195, 1488.371301023830028, 192.3463370429979875 ) ) ;
#74437 = CARTESIAN_POINT ( 'NONE',  ( 2.863787855735000054, 1516.788317650260069, 207.4054531903269947 ) ) ;
#74438 = CARTESIAN_POINT ( 'NONE',  ( 2.867497623927549810, 1409.013195610850062, 223.6255212523830096 ) ) ;
#74439 = CARTESIAN_POINT ( 'NONE',  ( 29.00779973304118897, 1526.382868172864164, 200.9494832830835378 ) ) ;
#74440 = CARTESIAN_POINT ( 'NONE',  ( 5.973824899667066646, 1425.157018348714246, 226.5484819897127124 ) ) ;
#74441 = CARTESIAN_POINT ( 'NONE',  ( 6.864181478733449637, 1424.874072653679832, 213.4309032859040087 ) ) ;
#74442 = AXIS2_PLACEMENT_3D ( 'NONE', #34481, #94364, #96040 ) ;
#74443 = ORIENTED_EDGE ( 'NONE', *, *, #44566, .T. ) ;
#74444 = EDGE_CURVE ( 'NONE', #105289, #22747, #42755, .T. ) ;
#74445 = CARTESIAN_POINT ( 'NONE',  ( 4.804950790719999532, 1416.130848190230154, 240.4142139981979938 ) ) ;
#74446 = CARTESIAN_POINT ( 'NONE',  ( -0.5624690339869999889, 1416.828040475229955, 227.7677324846980014 ) ) ;
#74448 = DIRECTION ( 'NONE',  ( 0.000000000000000000, -1.000000000000000000, 0.000000000000000000 ) ) ;
#74447 = CARTESIAN_POINT ( 'NONE',  ( -2.498001343329999901, 1464.114461778829991, 182.6719732163979870 ) ) ;
#74449 = CARTESIAN_POINT ( 'NONE',  ( 14.45783227242900004, 1416.839692127189892, 196.8516148535319985 ) ) ;
#74450 = CARTESIAN_POINT ( 'NONE',  ( -9.545816653860001111, 1416.905270227430037, 240.4008508676979829 ) ) ;
#74451 = DIRECTION ( 'NONE',  ( 0.03489949670250479252, 0.9993908270190956511, 0.000000000000000000 ) ) ;
#74452 = EDGE_CURVE ( 'NONE', #94689, #73642, #91336, .T. ) ;
#74453 = CARTESIAN_POINT ( 'NONE',  ( -21.97965021947160125, 1452.145514088490017, 140.5363500159340049 ) ) ;
#74454 = CARTESIAN_POINT ( 'NONE',  ( -18.90776592919999644, 1416.839648759230158, 208.2177104760110069 ) ) ;
#74455 = VERTEX_POINT ( 'NONE', #12843 ) ;
#74456 = CARTESIAN_POINT ( 'NONE',  ( -107.2926799547009864, 1378.913060387329779, 300.7951754864200211 ) ) ;
#74457 = DIRECTION ( 'NONE',  ( -3.247745162871014848E-19, -1.000000000000000000, -7.717164782866489769E-18 ) ) ;
#74458 = CARTESIAN_POINT ( 'NONE',  ( 16.39875021229349983, 1422.270930245990030, 227.2883076116929999 ) ) ;
#74459 = CARTESIAN_POINT ( 'NONE',  ( -3.180365954810094209, 1370.226539215819685, 208.0370721656823321 ) ) ;
#74460 = EDGE_LOOP ( 'NONE', ( #83011, #73064, #93577, #48627, #29691 ) ) ;
#74461 = ORIENTED_EDGE ( 'NONE', *, *, #74024, .F. ) ;
#74462 = CARTESIAN_POINT ( 'NONE',  ( -39.76527504970000138, 1384.717239764220039, 212.4523225820389882 ) ) ;
#74463 = CARTESIAN_POINT ( 'NONE',  ( -22.67876275168039868, 1409.704989955349902, 209.2849217834479987 ) ) ;
#74464 = ORIENTED_EDGE ( 'NONE', *, *, #881, .T. ) ;
#74465 = CARTESIAN_POINT ( 'NONE',  ( 4.333389510011039114, 1508.551704407329908, 204.4537291618960069 ) ) ;
#74466 = CARTESIAN_POINT ( 'NONE',  ( 6.536123391264514026, 1446.776743555406711, 154.4253092722253200 ) ) ;
#74467 = CARTESIAN_POINT ( 'NONE',  ( -5.850656168700000492, 1507.636149491230071, 236.0722295150979733 ) ) ;
#74469 = AXIS2_PLACEMENT_3D ( 'NONE', #99356, #72537, #47324 ) ;
#74468 = CARTESIAN_POINT ( 'NONE',  ( 4.492641946539720266, 1508.880976916049804, 212.2392405230349937 ) ) ;
#74470 = AXIS2_PLACEMENT_3D ( 'NONE', #99566, #30722, #13349 ) ;
#74471 = CARTESIAN_POINT ( 'NONE',  ( 43.38413226852659932, 1452.743835328579962, 268.5823572257330056 ) ) ;
#74472 = CARTESIAN_POINT ( 'NONE',  ( -3.861651061951890007, 1508.610718263850003, 204.4420517364369800 ) ) ;
#74473 = CARTESIAN_POINT ( 'NONE',  ( -6.730034279650000784, 1426.619567491610042, 203.0656631102989991 ) ) ;
#74474 = CARTESIAN_POINT ( 'NONE',  ( 1.120543697654999837, 1517.073005577650065, 205.0775260448770041 ) ) ;
#74475 = EDGE_CURVE ( 'NONE', #2114, #99633, #46738, .T. ) ;
#74476 = VERTEX_POINT ( 'NONE', #47024 ) ;
#74477 = CARTESIAN_POINT ( 'NONE',  ( 2.470168521978398424, 1523.382868172864164, 175.3649660270905315 ) ) ;
#74478 = CARTESIAN_POINT ( 'NONE',  ( 0.1955981723673640149, 1414.913060387329779, 225.1861338915940109 ) ) ;
#74479 = CARTESIAN_POINT ( 'NONE',  ( 12.82354616867442054, 1442.855160287932449, 186.8966734488652435 ) ) ;
#74480 = ORIENTED_EDGE ( 'NONE', *, *, #57642, .T. ) ;
#74481 = CARTESIAN_POINT ( 'NONE',  ( -437.6900670641260263, 1424.998713256100018, 209.1045946275809797 ) ) ;
#74482 = CARTESIAN_POINT ( 'NONE',  ( 26.83593419056240137, 1450.879312558440006, 136.4219504817619963 ) ) ;
#74483 = CARTESIAN_POINT ( 'NONE',  ( -13.40617548155469940, 1512.633419863009976, 193.8191794496820251 ) ) ;
#74484 = CARTESIAN_POINT ( 'NONE',  ( 1.863634235144320028, 1452.847980845800066, 152.4700529009420222 ) ) ;
#74485 = CARTESIAN_POINT ( 'NONE',  ( 9.564368764730000194, 1420.652513758999930, 197.0358326467990082 ) ) ;
#74486 = CARTESIAN_POINT ( 'NONE',  ( 17.22271612299999788, 1410.011821425830249, 192.5801709317979942 ) ) ;
#74487 = CARTESIAN_POINT ( 'NONE',  ( -9.442246275039069658, 1493.175626386839895, 201.2440496806180192 ) ) ;
#74488 = CARTESIAN_POINT ( 'NONE',  ( -4.748472660380000043, 1496.422918367389912, 198.9435340602989868 ) ) ;
#74489 = CARTESIAN_POINT ( 'NONE',  ( 0.03683352690712138333, 1409.764797560680563, 233.0950034937904150 ) ) ;
#74491 = CARTESIAN_POINT ( 'NONE',  ( 6.646318662569999702, 1378.413060387289988, 209.1218459647943746 ) ) ;
#74490 = CARTESIAN_POINT ( 'NONE',  ( -13.32966728119899891, 1434.904994951539948, 148.9243255523419975 ) ) ;
#74492 = CARTESIAN_POINT ( 'NONE',  ( 10.77287936046479899, 1425.076563501110058, 206.5335355432609958 ) ) ;
#74493 = CARTESIAN_POINT ( 'NONE',  ( -12.55357009390000123, 1380.105834429130255, 214.3611497310990046 ) ) ;
#74494 = CARTESIAN_POINT ( 'NONE',  ( -7.668984248404999704, 1514.216129015420165, 202.9976746052270187 ) ) ;
#74495 = ORIENTED_EDGE ( 'NONE', *, *, #49785, .T. ) ;
#74496 = CARTESIAN_POINT ( 'NONE',  ( 14.35418281379999961, 1430.829918313929966, 214.3676144195279676 ) ) ;
#74497 = DIRECTION ( 'NONE',  ( -0.7067692896845355621, 0.03085827994953252440, -0.7067707815956835171 ) ) ;
#74498 = CARTESIAN_POINT ( 'NONE',  ( -102.5889311002350155, 1384.940216307899846, 311.0676245730850269 ) ) ;
#74499 = CARTESIAN_POINT ( 'NONE',  ( -8.753431510080000422, 1385.526834493349952, 199.9255429183990032 ) ) ;
#74500 = CARTESIAN_POINT ( 'NONE',  ( 10.63130018098530094, 1427.874628198720075, 210.9979093251330085 ) ) ;
#74502 = ORIENTED_EDGE ( 'NONE', *, *, #19994, .F. ) ;
#74501 = CARTESIAN_POINT ( 'NONE',  ( 11.26113244141030023, 1425.135562406779854, 203.0046430561289981 ) ) ;
#74503 = CARTESIAN_POINT ( 'NONE',  ( 1.057929922660000077, 1429.578271572490166, 217.3710875290090030 ) ) ;
#74504 = CARTESIAN_POINT ( 'NONE',  ( 4.714294778569999749E-15, 1435.943783413959864, 150.5249316333980119 ) ) ;
#74505 = CARTESIAN_POINT ( 'NONE',  ( -17.00797328670000397, 1417.537217351680056, 207.7155449971589860 ) ) ;
#74506 = CARTESIAN_POINT ( 'NONE',  ( -12.78723757166081754, 1416.835806642020316, 195.5393902064313636 ) ) ;
#74507 = CARTESIAN_POINT ( 'NONE',  ( 11.07527106835961916, 1414.913060387329779, 220.8418235494980877 ) ) ;
#74508 = CARTESIAN_POINT ( 'NONE',  ( -13.10606021074817207, 1517.151704408390060, 192.4222450282478292 ) ) ;
#74509 = CARTESIAN_POINT ( 'NONE',  ( -1.693092047772239983, 1443.235800395060096, 218.9922115469449864 ) ) ;
#74510 = CARTESIAN_POINT ( 'NONE',  ( 17.29393938232459860, 1523.621879633029039, 180.8572348224458608 ) ) ;
#74511 = CARTESIAN_POINT ( 'NONE',  ( 0.6370436997426999204, 1517.151704408390060, 200.3909606286928238 ) ) ;
#74512 = CARTESIAN_POINT ( 'NONE',  ( 13.40512367049999831, 1419.762041482030099, 228.7767913457980171 ) ) ;
#74513 = CARTESIAN_POINT ( 'NONE',  ( -18.39408727770000240, 1486.478860455830045, 188.6611279849980178 ) ) ;
#74514 = CARTESIAN_POINT ( 'NONE',  ( 5.587699803720799885, 1473.877678908759890, 219.0867832512670077 ) ) ;
#74515 = CARTESIAN_POINT ( 'NONE',  ( -16.64778341059999889, 1409.494413794329830, 224.2640771540980040 ) ) ;
#74516 = CARTESIAN_POINT ( 'NONE',  ( -20.69303424980000372, 1486.764600954290017, 209.1218459616989946 ) ) ;
#74517 = CARTESIAN_POINT ( 'NONE',  ( -2.497138374290000407, 1474.686822087490100, 216.2214433156790108 ) ) ;
#74518 = CARTESIAN_POINT ( 'NONE',  ( 0.000000000000000000, 1523.382868172864164, 209.1218459616979999 ) ) ;
#74519 = CARTESIAN_POINT ( 'NONE',  ( 6.536538287287070992E-07, 1407.436810216500135, 196.0562222547989961 ) ) ;
#74520 = DIRECTION ( 'NONE',  ( -0.2113515706023144647, 0.000000000000000000, 0.9774101051267757301 ) ) ;
#74521 = CARTESIAN_POINT ( 'NONE',  ( 11.69992642896390045, 1435.514533225360083, 225.6365413922099776 ) ) ;
#74522 = CARTESIAN_POINT ( 'NONE',  ( -1.075903594600000179, 1414.913060387329779, 226.3952325314980101 ) ) ;
#74523 = CARTESIAN_POINT ( 'NONE',  ( 0.1945320816990730173, 1466.113474688809902, 182.6906957989669991 ) ) ;
#74525 = VERTEX_POINT ( 'NONE', #6653 ) ;
#74524 = CARTESIAN_POINT ( 'NONE',  ( -0.1955981723043500320, 1414.913060387329779, 193.0575580317509718 ) ) ;
#74526 = CARTESIAN_POINT ( 'NONE',  ( -27.73483395940000307, 1444.994950788470987, 161.2078980334979690 ) ) ;
#74527 = CARTESIAN_POINT ( 'NONE',  ( -28.07727371017839957, 1509.147381901259905, 210.7551250638759655 ) ) ;
#74528 = CARTESIAN_POINT ( 'NONE',  ( 13.50082440470000122, 1434.968962347899833, 149.4780432086979829 ) ) ;
#74529 = CARTESIAN_POINT ( 'NONE',  ( -41.59656558017320549, 1442.666623283399986, 134.0999999980969903 ) ) ;
#74530 = CARTESIAN_POINT ( 'NONE',  ( -6.123233995736771213E-16, 1379.913060387289988, 209.1218459616989946 ) ) ;
#74531 = ORIENTED_EDGE ( 'NONE', *, *, #48928, .F. ) ;
#74532 = CARTESIAN_POINT ( 'NONE',  ( -17.19739463999671614, 1525.960063244516959, 181.9833109756550300 ) ) ;
#74533 = CARTESIAN_POINT ( 'NONE',  ( 5.561733859871847763, 1387.291117539184825, 209.1218459616989946 ) ) ;
#74534 = CARTESIAN_POINT ( 'NONE',  ( -104.0123117872064142, 1380.205049092886156, 306.5154211266013817 ) ) ;
#74535 = FACE_OUTER_BOUND ( 'NONE', #28146, .T. ) ;
#74536 = CARTESIAN_POINT ( 'NONE',  ( 9.146237114798470458, 1449.998848199699978, 208.1168068718100130 ) ) ;
#74537 = CARTESIAN_POINT ( 'NONE',  ( 40.48954223343692860, 1425.136313467639638, 269.1159157282953061 ) ) ;
#74538 = CARTESIAN_POINT ( 'NONE',  ( 21.84849975889999740, 1489.480617680729893, 209.7146558588220273 ) ) ;
#74539 = CARTESIAN_POINT ( 'NONE',  ( -12.30840189449999933, 1378.376159634960231, 209.8321859945540098 ) ) ;
#74540 = CARTESIAN_POINT ( 'NONE',  ( 2.500000001190000098, 1425.952486855329880, 183.8951078798980063 ) ) ;
#74541 = CARTESIAN_POINT ( 'NONE',  ( -65.89688115222600118, 1385.091299999440025, 257.0426204345699830 ) ) ;
#74542 = CARTESIAN_POINT ( 'NONE',  ( 1.338019653377509943, 1431.361302561429966, 218.5179672105229827 ) ) ;
#74543 = CARTESIAN_POINT ( 'NONE',  ( -24.83643123910302464, 1443.481921562399293, 210.6071950037623708 ) ) ;
#74544 = ORIENTED_EDGE ( 'NONE', *, *, #15352, .F. ) ;
#74545 = CARTESIAN_POINT ( 'NONE',  ( 16.50400130224750583, 1525.907212628473644, 181.9890130758377040 ) ) ;
#74546 = CARTESIAN_POINT ( 'NONE',  ( -15.99166196625810166, 1409.471479983660174, 225.2129078530250013 ) ) ;
#74548 = ORIENTED_EDGE ( 'NONE', *, *, #34733, .T. ) ;
#74547 = CARTESIAN_POINT ( 'NONE',  ( 4.061051490899999727, 1501.418159739390148, 230.0899566632990059 ) ) ;
#74549 = CARTESIAN_POINT ( 'NONE',  ( 4.873735476160000246, 1472.089320948289924, 218.0431589096889695 ) ) ;
#74550 = CARTESIAN_POINT ( 'NONE',  ( 11.39904368536729962, 1471.112668423910009, 209.6179614837379859 ) ) ;
#74551 = CARTESIAN_POINT ( 'NONE',  ( 23.45884178989999924, 1509.732261194629928, 225.1742078074979929 ) ) ;
#74552 = CARTESIAN_POINT ( 'NONE',  ( -109.4716062389999962, 1384.569436532440022, 311.2688442282590131 ) ) ;
#74553 = CARTESIAN_POINT ( 'NONE',  ( -11.05399937894872409, 1492.687025461389339, 208.1826818617392121 ) ) ;
#74554 = CARTESIAN_POINT ( 'NONE',  ( 0.6844602914180001330, 1466.314900821229912, 235.5924101916979794 ) ) ;
#74555 = CARTESIAN_POINT ( 'NONE',  ( 16.87240681180000124, 1409.502257816329802, 222.1138738933979937 ) ) ;
#74556 = CARTESIAN_POINT ( 'NONE',  ( -2.423460974664930045, 1412.654287068640087, 186.3965991398220012 ) ) ;
#74557 = CARTESIAN_POINT ( 'NONE',  ( -16.87496977620000038, 1423.389150575329950, 227.5705651359979811 ) ) ;
#74558 = CARTESIAN_POINT ( 'NONE',  ( -3.215705694400522674, 1511.798535855272576, 201.1683149189278197 ) ) ;
#74559 = CARTESIAN_POINT ( 'NONE',  ( 7.184742850290000149, 1480.879511957389923, 207.6765937235290096 ) ) ;
#74560 = CARTESIAN_POINT ( 'NONE',  ( -96.21470915085022568, 1331.448250124730293, 308.6099712340398469 ) ) ;
#74561 = CARTESIAN_POINT ( 'NONE',  ( -4.440892098499999806E-15, 1519.913060387329779, 231.7062449670980300 ) ) ;
#74562 = CARTESIAN_POINT ( 'NONE',  ( 9.842969107810001006, 1365.740588703660023, 210.6218459616991936 ) ) ;
#74563 = CARTESIAN_POINT ( 'NONE',  ( -3.266349512195000138, 1516.797038924770050, 205.0935381919470046 ) ) ;
#74564 = CARTESIAN_POINT ( 'NONE',  ( -8.375290140818398399, 1485.147173385050110, 184.2408640538430120 ) ) ;
#74565 = ORIENTED_EDGE ( 'NONE', *, *, #47494, .F. ) ;
#74566 = CARTESIAN_POINT ( 'NONE',  ( -1.572308128563102869, 1420.974599004695847, 183.2802011453454440 ) ) ;
#74568 = ORIENTED_EDGE ( 'NONE', *, *, #107818, .F. ) ;
#74567 = CARTESIAN_POINT ( 'NONE',  ( -68.58923311738080031, 1379.747637154969880, 280.1848937903309888 ) ) ;
#74569 = EDGE_LOOP ( 'NONE', ( #108917, #8721, #24446, #29308 ) ) ;
#74570 = CARTESIAN_POINT ( 'NONE',  ( -8.055471353928528089, 1382.512276592904755, 218.5978840298738817 ) ) ;
#74571 = EDGE_LOOP ( 'NONE', ( #38898, #59997, #49503, #51837, #48551 ) ) ;
#74572 = CYLINDRICAL_SURFACE ( 'NONE', #65296, 0.9999999999999970024 ) ;
#74573 = CARTESIAN_POINT ( 'NONE',  ( -22.14275666580000035, 1410.906117103929773, 202.5124468041880164 ) ) ;
#74574 = B_SPLINE_CURVE_WITH_KNOTS ( 'NONE', 5,
 ( #59558, #84186, #16407, #93672, #41646, #50058 ),
 .UNSPECIFIED., .F., .F.,
 ( 6, 6 ),
 ( 0.000000000000000000, 1.000000000000000000 ),
 .UNSPECIFIED. ) ;
#74576 = CARTESIAN_POINT ( 'NONE',  ( 15.94649789270860119, 1409.495428613550075, 192.6881838021419924 ) ) ;
#74575 = CARTESIAN_POINT ( 'NONE',  ( -10.82013115906650036, 1424.918091613318893, 144.4803130008261007 ) ) ;
#74577 = CARTESIAN_POINT ( 'NONE',  ( 0.01012488564660149991, 1516.989863902050047, 210.2497743036369968 ) ) ;
#74578 = CARTESIAN_POINT ( 'NONE',  ( 39.00001286119130128, 1437.776791841900149, 135.9885178820470060 ) ) ;
#74579 = CARTESIAN_POINT ( 'NONE',  ( -106.6474845526250022, 1378.913060387289988, 306.6623049594010126 ) ) ;
#74580 = DIRECTION ( 'NONE',  ( 0.6480245870892075155, -1.644245901462725924E-32, -0.7616194158028418704 ) ) ;
#74581 = CARTESIAN_POINT ( 'NONE',  ( 11.49474869997571247, 1464.050871868342483, 231.7668017734373791 ) ) ;
#74582 = DIRECTION ( 'NONE',  ( 1.000000000000000000, 0.000000000000000000, 0.000000000000000000 ) ) ;
#74583 = AXIS2_PLACEMENT_3D ( 'NONE', #68174, #91134, #25562 ) ;
#74584 = CARTESIAN_POINT ( 'NONE',  ( 34.34692909021160290, 1451.701922534439973, 134.0999999981429767 ) ) ;
#74585 = FACE_OUTER_BOUND ( 'NONE', #69376, .T. ) ;
#74586 = ORIENTED_EDGE ( 'NONE', *, *, #87815, .F. ) ;
#74587 = CARTESIAN_POINT ( 'NONE',  ( 20.33643750519999926, 1475.138452888789971, 218.0161091832190152 ) ) ;
#74588 = CARTESIAN_POINT ( 'NONE',  ( -18.72407806909999906, 1458.246133455830204, 227.3156640602979905 ) ) ;
#74589 = VERTEX_POINT ( 'NONE', #43030 ) ;
#74590 = ORIENTED_EDGE ( 'NONE', *, *, #27539, .F. ) ;
#74591 = CARTESIAN_POINT ( 'NONE',  ( -2.680760545863249966, 1370.258219039080814, 211.4729122695361241 ) ) ;
#74592 = CARTESIAN_POINT ( 'NONE',  ( -2.938318217019999956, 1419.338735643829978, 183.9627234138980043 ) ) ;
#74593 = CARTESIAN_POINT ( 'NONE',  ( 12.64235333510859860, 1500.251838740290168, 207.9986088160900124 ) ) ;
#74594 = CARTESIAN_POINT ( 'NONE',  ( -3.240679945760000180, 1484.702199250929880, 183.3401715852980089 ) ) ;
#74595 = CARTESIAN_POINT ( 'NONE',  ( -2.500000000000079936, 1439.283173988879980, 159.9470331267719985 ) ) ;
#74596 = CARTESIAN_POINT ( 'NONE',  ( 2.330134126090002145, 1515.193466806515744, 204.7957666309817455 ) ) ;
#74597 = AXIS2_PLACEMENT_3D ( 'NONE', #16105, #59260, #7723 ) ;
#74598 = CARTESIAN_POINT ( 'NONE',  ( -13.16532433220000087, 1379.531301371890095, 208.2880016088489867 ) ) ;
#74599 = CARTESIAN_POINT ( 'NONE',  ( 38.81202644819820335, 1450.612734570869861, 134.4205495056820041 ) ) ;
#74600 = DIRECTION ( 'NONE',  ( -0.6736849260863837507, 0.000000000000000000, 0.7390186874254154326 ) ) ;
#74601 = CARTESIAN_POINT ( 'NONE',  ( -5.510910596163090542E-16, 1508.551704408389924, 213.6218459616989946 ) ) ;
#74602 = CARTESIAN_POINT ( 'NONE',  ( 33.05507863147482794, 1442.773887286371291, 154.3538505727091206 ) ) ;
#74603 = CARTESIAN_POINT ( 'NONE',  ( -73.83428086117611144, 1384.760717133270191, 273.3968393063270241 ) ) ;
#74604 = ORIENTED_EDGE ( 'NONE', *, *, #103310, .F. ) ;
#74605 =( BOUNDED_CURVE ( )  B_SPLINE_CURVE ( 5, ( #39036, #40155, #13279, #73782, #74338, #47470 ),
 .UNSPECIFIED., .F., .T. ) 
 B_SPLINE_CURVE_WITH_KNOTS ( ( 6, 6 ),
 ( 0.000000000000000000, 1.000000000000000000 ),
 .UNSPECIFIED. ) 
 CURVE ( )  GEOMETRIC_REPRESENTATION_ITEM ( )  RATIONAL_B_SPLINE_CURVE ( ( 0.2500000000000000000, 0.2499999999993640087, 0.2999999999990460298, 0.3999999999987279842, 0.5999999999987279953, 1.000000000000000000 ) ) 
 REPRESENTATION_ITEM ( '' )  );
#74606 = CARTESIAN_POINT ( 'NONE',  ( 6.554151426245000245, 1516.906641539930206, 201.7900338461269882 ) ) ;
#74607 = CARTESIAN_POINT ( 'NONE',  ( 1.119592181715000079, 1516.958737650239982, 207.9859471464170326 ) ) ;
#74608 = VERTEX_POINT ( 'NONE', #102901 ) ;
#74609 = CARTESIAN_POINT ( 'NONE',  ( 36.18824964826809776, 1440.913060387330006, 262.5531867102749857 ) ) ;
#74610 = CARTESIAN_POINT ( 'NONE',  ( -0.0007986355180737672761, 1451.919156408470826, 154.0006015666134260 ) ) ;
#74611 = ORIENTED_EDGE ( 'NONE', *, *, #41795, .F. ) ;
#74612 = CARTESIAN_POINT ( 'NONE',  ( -14.15566883900000050, 1416.254459047329874, 221.6674824254980081 ) ) ;
#74613 = CARTESIAN_POINT ( 'NONE',  ( -8.612924558394999153, 1512.851027864960088, 211.3708094598169964 ) ) ;
#74614 = DIRECTION ( 'NONE',  ( 0.000000000000000000, 0.000000000000000000, -1.000000000000000000 ) ) ;
#74615 = CARTESIAN_POINT ( 'NONE',  ( -9.276727106389110133, 1461.679952532089828, 206.2486811414470083 ) ) ;
#74616 = CARTESIAN_POINT ( 'NONE',  ( -12.51099981740000011, 1416.825784017230035, 222.1450729860980005 ) ) ;
#74617 = CARTESIAN_POINT ( 'NONE',  ( -5.495614756258980549, 1510.802068165409992, 201.5298705880650232 ) ) ;
#74618 = DIRECTION ( 'NONE',  ( -1.755985294532469921E-16, 1.000000000000000000, -1.338183447452831989E-16 ) ) ;
#74619 = CARTESIAN_POINT ( 'NONE',  ( -12.40443716549999920, 1434.419911639550037, 147.1503489169979844 ) ) ;
#74621 = EDGE_CURVE ( 'NONE', #84259, #79128, #36018, .T. ) ;
#74620 = CARTESIAN_POINT ( 'NONE',  ( -21.41029105011889300, 1526.329757971582922, 184.2230555347968561 ) ) ;
#74623 = CARTESIAN_POINT ( 'NONE',  ( 2.531940903048510086E-08, 1457.850589566970029, 229.0733431205499926 ) ) ;
#74622 = CARTESIAN_POINT ( 'NONE',  ( 12.66475911230000051, 1461.490340252930082, 232.8294749871980116 ) ) ;
#74624 = CARTESIAN_POINT ( 'NONE',  ( -11.18076303840566865, 1522.051704408389924, 213.9857921429048417 ) ) ;
#74625 = CARTESIAN_POINT ( 'NONE',  ( -6.554151464375000735, 1516.906641539930206, 216.4536580562070185 ) ) ;
#74626 = EDGE_LOOP ( 'NONE', ( #58600, #76180 ) ) ;
#74627 = CARTESIAN_POINT ( 'NONE',  ( -22.63977338456492916, 1409.703622513127584, 209.3606416856607382 ) ) ;
#74628 = CARTESIAN_POINT ( 'NONE',  ( -0.1451720414164340001, 1507.596876506829858, 180.8216655926840133 ) ) ;
#74629 = CARTESIAN_POINT ( 'NONE',  ( 0.4614184642274221093, 1516.800601748523150, 216.8378509299481038 ) ) ;
#74630 = CARTESIAN_POINT ( 'NONE',  ( 0.01327404799950150129, 1516.939877939420057, 212.5773418040870126 ) ) ;
#74631 = CARTESIAN_POINT ( 'NONE',  ( 18.52542017129999863, 1508.846193922329803, 188.2533944517980160 ) ) ;
#74632 = CARTESIAN_POINT ( 'NONE',  ( -6.531167973260561865, 1522.051704408389924, 216.7070295963201829 ) ) ;
#74634 = ORIENTED_EDGE ( 'NONE', *, *, #97902, .T. ) ;
#74633 = CARTESIAN_POINT ( 'NONE',  ( 4.679794176543860651, 1508.610718243669908, 212.9835092646939927 ) ) ;
#74635 = CARTESIAN_POINT ( 'NONE',  ( -1.488474718482915460, 1526.348417187222594, 178.3303222095513831 ) ) ;
#74636 = CARTESIAN_POINT ( 'NONE',  ( 3.376777021050000105, 1508.158926475389762, 220.2301072607990022 ) ) ;
#74637 = CARTESIAN_POINT ( 'NONE',  ( -10.96338982440000009, 1431.906653981850013, 151.7581583521979951 ) ) ;
#74638 = CARTESIAN_POINT ( 'NONE',  ( -2.470168521978398868, 1501.977400791986611, 242.8787258963054683 ) ) ;
#74639 = CARTESIAN_POINT ( 'NONE',  ( -4.792927608962380681, 1442.435446138249972, 201.1994192484410178 ) ) ;
#74640 = FACE_OUTER_BOUND ( 'NONE', #37529, .T. ) ;
#74641 = CARTESIAN_POINT ( 'NONE',  ( -7.326027882650599565, 1426.061615434360192, 203.3611598758510013 ) ) ;
#74642 = B_SPLINE_CURVE_WITH_KNOTS ( 'NONE', 5,
 ( #87786, #53079, #69892, #1570, #19443, #96731 ),
 .UNSPECIFIED., .F., .F.,
 ( 6, 6 ),
 ( -7.104449043337727865, 0.000000000000000000 ),
 .UNSPECIFIED. ) ;
#74643 = CARTESIAN_POINT ( 'NONE',  ( 12.98218568629999936, 1444.905773837279867, 186.8780337078979983 ) ) ;
#74645 = CARTESIAN_POINT ( 'NONE',  ( -10.73514660619479955, 1424.973046414658938, 139.1354236203746098 ) ) ;
#74644 = CARTESIAN_POINT ( 'NONE',  ( -19.99968608059999653, 1495.374354163629960, 228.2163264703980019 ) ) ;
#74647 = CARTESIAN_POINT ( 'NONE',  ( 18.87853829029999986, 1458.344553362990155, 213.8102309971890236 ) ) ;
#74646 = TOROIDAL_SURFACE ( 'NONE', #1266, 8.013264357029999729, 0.5000000000000000000 ) ;
#74648 = ORIENTED_EDGE ( 'NONE', *, *, #21983, .F. ) ;
#74649 = CARTESIAN_POINT ( 'NONE',  ( -7.337153806245000354, 1517.119374999550018, 205.8621166342670108 ) ) ;
#74650 = CARTESIAN_POINT ( 'NONE',  ( 14.64031841569999948, 1407.520860949229927, 268.3932868650979913 ) ) ;
#74651 = CARTESIAN_POINT ( 'NONE',  ( 0.1416802514830000082, 1408.918007970730059, 186.4630591869979810 ) ) ;
#74652 = CARTESIAN_POINT ( 'NONE',  ( 10.95672663321720108, 1490.269269208220067, 209.3699634639930025 ) ) ;
#74653 = ADVANCED_FACE ( 'NONE', ( #17224 ), #85551, .F. ) ;
#74654 = CARTESIAN_POINT ( 'NONE',  ( 24.64646478266137208, 1440.604980622881385, 212.4694330774556192 ) ) ;
#74655 = ADVANCED_FACE ( 'NONE', ( #102361 ), #3582, .F. ) ;
#74656 = CARTESIAN_POINT ( 'NONE',  ( -9.012915958852776299, 1388.961832031413678, 217.6296823903735174 ) ) ;
#74657 = CARTESIAN_POINT ( 'NONE',  ( 12.78690713350000152, 1416.828040475229955, 222.7042044314979989 ) ) ;
#74658 = EDGE_CURVE ( 'NONE', #101907, #40922, #77043, .T. ) ;
#74659 = CARTESIAN_POINT ( 'NONE',  ( -3.677613769069999778E-16, 1378.399971913189802, 209.1218459616989946 ) ) ;
#74660 = CARTESIAN_POINT ( 'NONE',  ( -2.314829430188050097, 1449.816261314480016, 155.0640873339540065 ) ) ;
#74661 = CARTESIAN_POINT ( 'NONE',  ( -1.639149609193548240, 1450.659151795366597, 183.2023271470939960 ) ) ;
#74662 = EDGE_CURVE ( 'NONE', #67570, #90273, #102026, .T. ) ;
#74663 = CARTESIAN_POINT ( 'NONE',  ( -19.76130828083433855, 1485.974801659758896, 190.2327744154961522 ) ) ;
#74664 = EDGE_CURVE ( 'NONE', #24304, #66906, #81517, .T. ) ;
#74665 = CARTESIAN_POINT ( 'NONE',  ( -14.43002663333860092, 1416.512142030599989, 221.3633489337159688 ) ) ;
#74666 = CARTESIAN_POINT ( 'NONE',  ( -4.324478665330000027, 1515.254593745989951, 209.8453557593589949 ) ) ;
#74667 = CARTESIAN_POINT ( 'NONE',  ( -14.35418281399999962, 1430.829918314029783, 214.3676144200779845 ) ) ;
#74668 = VECTOR ( 'NONE', #100382, 1000.000000000000114 ) ;
#74669 = DIRECTION ( 'NONE',  ( -0.000000000000000000, 1.000000000000000000, -0.000000000000000000 ) ) ;
#74670 = CARTESIAN_POINT ( 'NONE',  ( 2.704557286920000081, 1440.782450355879973, 168.7248561158979783 ) ) ;
#74671 = CARTESIAN_POINT ( 'NONE',  ( -4.970712357689999195, 1475.638404632529955, 266.9514863814980004 ) ) ;
#74672 = CARTESIAN_POINT ( 'NONE',  ( -11.28910848134292699, 1425.472454366105467, 139.1360123033548462 ) ) ;
#74673 = CARTESIAN_POINT ( 'NONE',  ( -19.45107472759999823, 1470.650217123529956, 191.6852195815980053 ) ) ;
#74674 = CARTESIAN_POINT ( 'NONE',  ( -11.88019884917019553, 1486.509635274632274, 184.3263142426127388 ) ) ;
#74675 = CARTESIAN_POINT ( 'NONE',  ( -55.66145447376079858, 1384.713837345919956, 273.0923277504820135 ) ) ;
#74676 = CARTESIAN_POINT ( 'NONE',  ( -107.1942030874700009, 1391.913060387289988, 301.3138641182989659 ) ) ;
#74677 = AXIS2_PLACEMENT_3D ( 'NONE', #20270, #54471, #105961 ) ;
#74678 = CARTESIAN_POINT ( 'NONE',  ( -21.48851227519999796, 1507.175870272490101, 211.5129893581290048 ) ) ;
#74679 = CARTESIAN_POINT ( 'NONE',  ( -106.8337455069999891, 1378.992203654629748, 300.5412270638589689 ) ) ;
#74680 = CARTESIAN_POINT ( 'NONE',  ( 32.21733215212998402, 1523.844782250843537, 216.7883898251401149 ) ) ;
#74681 = CARTESIAN_POINT ( 'NONE',  ( 24.04921872038306674, 1508.500196458096980, 195.9136755597566264 ) ) ;
#74682 = CARTESIAN_POINT ( 'NONE',  ( -1.009090409386799836, 1395.948298600919998, 220.0848352038350129 ) ) ;
#74683 = ADVANCED_FACE ( 'NONE', ( #73757 ), #47988, .T. ) ;
#74684 = CARTESIAN_POINT ( 'NONE',  ( -15.81341253836600025, 1421.037553285879994, 227.0412314586560001 ) ) ;
#74685 = CARTESIAN_POINT ( 'NONE',  ( -21.62164173326539895, 1521.951704408389787, 210.2163513712909833 ) ) ;
#74686 = VERTEX_POINT ( 'NONE', #107335 ) ;
#74687 = CARTESIAN_POINT ( 'NONE',  ( -7.497914047782630931, 1410.547968552112707, 230.8512428201019020 ) ) ;
#74689 = ADVANCED_FACE ( 'NONE', ( #90526 ), #107880, .F. ) ;
#74688 = CARTESIAN_POINT ( 'NONE',  ( -13.59199629040490009, 1508.179429147699921, 209.5634456311599934 ) ) ;
#74690 = CARTESIAN_POINT ( 'NONE',  ( -2.370970874524634286, 1427.002265528474027, 134.0999999980980135 ) ) ;
#74692 = CARTESIAN_POINT ( 'NONE',  ( -14.05435969296220122, 1379.579181450040096, 211.8388747788069963 ) ) ;
#74691 = DIRECTION ( 'NONE',  ( -0.7071067811865475727, 0.000000000000000000, 0.7071067811865475727 ) ) ;
#74693 = CARTESIAN_POINT ( 'NONE',  ( 9.905242068095489572, 1468.560492227489931, 207.6656469818879884 ) ) ;
#74694 = EDGE_CURVE ( 'NONE', #107294, #48829, #12763, .T. ) ;
#74695 = CARTESIAN_POINT ( 'NONE',  ( -29.33431687954604783, 1526.382868172863937, 201.1003846321129629 ) ) ;
#74696 = CARTESIAN_POINT ( 'NONE',  ( 3.452289182574999948, 1517.069378699710114, 202.5601595088670024 ) ) ;
#74697 = CARTESIAN_POINT ( 'NONE',  ( -6.681506626574450713, 1488.898881121549948, 189.3483665020969795 ) ) ;
#74699 = CYLINDRICAL_SURFACE ( 'NONE', #102965, 7.799999999999999822 ) ;
#74698 = CIRCLE ( 'NONE', #6809, 1.999999999999997780 ) ;
#74700 = CARTESIAN_POINT ( 'NONE',  ( 14.97406870653500022, 1513.863307887919973, 194.3519930166669951 ) ) ;
#74701 = CARTESIAN_POINT ( 'NONE',  ( -20.41709936247310253, 1418.495400755769879, 207.2248099484089892 ) ) ;
#74702 = CARTESIAN_POINT ( 'NONE',  ( -3.771520282370200317, 1380.389636976869951, 210.0680625258100065 ) ) ;
#74703 = CARTESIAN_POINT ( 'NONE',  ( 20.61223612676809935, 1508.367027694390117, 227.7934906704109892 ) ) ;
#74705 = ORIENTED_EDGE ( 'NONE', *, *, #13794, .T. ) ;
#74704 = CARTESIAN_POINT ( 'NONE',  ( -54.22704658621609752, 1379.707482379519888, 254.1827617957189602 ) ) ;
#74706 = VERTEX_POINT ( 'NONE', #72121 ) ;
#74707 = CARTESIAN_POINT ( 'NONE',  ( 11.37512727334929963, 1434.390363725699899, 151.4928147334219943 ) ) ;
#74708 = CARTESIAN_POINT ( 'NONE',  ( -11.59628660009999912, 1396.377029133129781, 211.2534838439580085 ) ) ;
#74709 = CARTESIAN_POINT ( 'NONE',  ( -19.55811020839999870, 1410.091525468729742, 221.3856977114979827 ) ) ;
#74710 = ORIENTED_EDGE ( 'NONE', *, *, #4362, .F. ) ;
#74711 = CARTESIAN_POINT ( 'NONE',  ( -13.50123011842539711, 1444.098455846193701, 169.3544814583405582 ) ) ;
#74712 = CARTESIAN_POINT ( 'NONE',  ( 22.41814969565213289, 1509.697587479513004, 228.1798637225821551 ) ) ;
#74713 = CARTESIAN_POINT ( 'NONE',  ( 22.08622291482331335, 1512.187213306747481, 184.4183880513174927 ) ) ;
#74715 = CARTESIAN_POINT ( 'NONE',  ( -13.87674170834680076, 1508.783404247360068, 183.8810751069530056 ) ) ;
#74714 = CARTESIAN_POINT ( 'NONE',  ( 1.581901184577762853, 1426.946688134061105, 134.0999999980979851 ) ) ;
#74716 = CARTESIAN_POINT ( 'NONE',  ( 0.8724072853540000283, 1429.775567651030087, 184.3285425289979855 ) ) ;
#74717 = CARTESIAN_POINT ( 'NONE',  ( -4.087663179609560160, 1462.748586608149935, 200.2519740037880069 ) ) ;
#74718 = CARTESIAN_POINT ( 'NONE',  ( -17.39983170771839838, 1417.829866268649994, 207.0843391556029758 ) ) ;
#74719 = CARTESIAN_POINT ( 'NONE',  ( 9.572892907575269561, 1396.247353193519984, 203.5817440233749949 ) ) ;
#74720 = CARTESIAN_POINT ( 'NONE',  ( 1.396725214909999790, 1415.041103191630100, 191.5122427437979979 ) ) ;
#74721 = CARTESIAN_POINT ( 'NONE',  ( 10.89169420240000008, 1427.021371490929823, 149.7235597410980006 ) ) ;
#74722 = CARTESIAN_POINT ( 'NONE',  ( 7.812244556781691607, 1509.186435478737394, 180.8337954617522882 ) ) ;
#74723 = ORIENTED_EDGE ( 'NONE', *, *, #37056, .T. ) ;
#74724 = CARTESIAN_POINT ( 'NONE',  ( 13.07453333027640063, 1436.035540400220043, 150.7116512640230042 ) ) ;
#74725 = EDGE_LOOP ( 'NONE', ( #58811, #26887, #69490, #4487 ) ) ;
#74726 = ORIENTED_EDGE ( 'NONE', *, *, #14548, .F. ) ;
#74727 = LINE ( 'NONE', #107760, #21549 ) ;
#74728 = CARTESIAN_POINT ( 'NONE',  ( -9.055072417550000807, 1464.016001224229967, 233.0040833371979829 ) ) ;
#74729 = AXIS2_PLACEMENT_3D ( 'NONE', #74256, #110586, #33872 ) ;
#74730 = CARTESIAN_POINT ( 'NONE',  ( -109.4932991490571084, 1386.884154433499134, 311.1438796777470088 ) ) ;
#74731 = CARTESIAN_POINT ( 'NONE',  ( -3.452289220704999551, 1517.069378699710114, 215.6835323934670328 ) ) ;
#74732 = CARTESIAN_POINT ( 'NONE',  ( -12.34520063366950104, 1378.885613852760116, 209.2790730372699954 ) ) ;
#74733 = EDGE_LOOP ( 'NONE', ( #18660, #34749, #44810, #42059 ) ) ;
#74734 = CARTESIAN_POINT ( 'NONE',  ( -11.44024719100000098, 1501.432053922590057, 208.7106206354860092 ) ) ;
#74735 = CARTESIAN_POINT ( 'NONE',  ( -37.47102956639999860, 1379.243633315240004, 218.9879198348490092 ) ) ;
#74736 = ORIENTED_EDGE ( 'NONE', *, *, #104329, .T. ) ;
#74737 = CARTESIAN_POINT ( 'NONE',  ( 7.322709686834999232, 1516.596789218710001, 205.8608388005369818 ) ) ;
#74738 = VERTEX_POINT ( 'NONE', #56394 ) ;
#74739 = CARTESIAN_POINT ( 'NONE',  ( 6.944466742375000834, 1516.939530130779985, 209.1105810159089913 ) ) ;
#74740 = CARTESIAN_POINT ( 'NONE',  ( -21.21436197740000296, 1509.702916646330095, 230.0075723124979845 ) ) ;
#74741 = CARTESIAN_POINT ( 'NONE',  ( -38.96076896855542770, 1429.469642160400554, 269.5922795220489547 ) ) ;
#74742 = CARTESIAN_POINT ( 'NONE',  ( 6.564976393265000709, 1512.035910181050212, 216.6257190735869926 ) ) ;
#74743 = ORIENTED_EDGE ( 'NONE', *, *, #101364, .T. ) ;
#74744 = CARTESIAN_POINT ( 'NONE',  ( 24.60632198259999726, 1440.982726376320215, 212.6699524588079839 ) ) ;
#74745 = CARTESIAN_POINT ( 'NONE',  ( -29.31706666688599938, 1440.913060386920051, 236.0794183928230154 ) ) ;
#74747 = CARTESIAN_POINT ( 'NONE',  ( -27.66920512940000165, 1384.171455447559993, 225.5844863493589969 ) ) ;
#74746 = AXIS2_PLACEMENT_3D ( 'NONE', #55669, #64621, #13064 ) ;
#74749 = EDGE_CURVE ( 'NONE', #41855, #39980, #6643, .T. ) ;
#74748 = CARTESIAN_POINT ( 'NONE',  ( 20.95983796500000196, 1494.619252927089747, 207.1496602654190156 ) ) ;
#74750 = EDGE_CURVE ( 'NONE', #6492, #55409, #70754, .T. ) ;
#74751 = CARTESIAN_POINT ( 'NONE',  ( 5.165173145674029520, 1410.469967527520112, 269.6177701542679870 ) ) ;
#74752 = CARTESIAN_POINT ( 'NONE',  ( -2.286446363765000100, 1517.042661899400173, 213.7475398352470108 ) ) ;
#74753 = CARTESIAN_POINT ( 'NONE',  ( 23.73237516220000032, 1410.130224032329807, 209.2990132785999720 ) ) ;
#74754 = CARTESIAN_POINT ( 'NONE',  ( -20.01700974779999953, 1508.374998501830078, 188.9474888133980244 ) ) ;
#74755 = CARTESIAN_POINT ( 'NONE',  ( 12.32716646574370145, 1492.190914138330072, 209.5898718627249764 ) ) ;
#74756 = AXIS2_PLACEMENT_3D ( 'NONE', #20293, #72387, #106516 ) ;
#74757 = CARTESIAN_POINT ( 'NONE',  ( -7.715720925248570339, 1516.789754148820066, 209.6216723975360026 ) ) ;
#74758 = CARTESIAN_POINT ( 'NONE',  ( -5.772978316675000166, 1516.659138130710289, 210.2536427808470023 ) ) ;
#74759 = CARTESIAN_POINT ( 'NONE',  ( 9.545106316202870644, 1434.678111609370035, 206.9724244943959945 ) ) ;
#74760 = CARTESIAN_POINT ( 'NONE',  ( 0.2920509773060000480, 1419.245382216430016, 184.6471073958980185 ) ) ;
#74761 = CARTESIAN_POINT ( 'NONE',  ( 3.921275451871176987, 1421.968795751384505, 139.1411894380421472 ) ) ;
#74763 = ORIENTED_EDGE ( 'NONE', *, *, #92242, .T. ) ;
#74762 = CARTESIAN_POINT ( 'NONE',  ( -61.90500753679999946, 1389.465434365910141, 278.4656905976589769 ) ) ;
#74764 = CARTESIAN_POINT ( 'NONE',  ( -46.41362929351480204, 1385.143899196999882, 254.3628368276549736 ) ) ;
#74765 = ADVANCED_FACE ( 'NONE', ( #85419 ), #8166, .T. ) ;
#74766 = CARTESIAN_POINT ( 'NONE',  ( 45.67186675490000169, 1440.913060379579974, 266.1886920260980105 ) ) ;
#74767 = DIRECTION ( 'NONE',  ( 0.000000000000000000, 0.000000000000000000, 1.000000000000000000 ) ) ;
#74768 = CARTESIAN_POINT ( 'NONE',  ( -16.98603957050000091, 1470.451033259130099, 228.5667712960980111 ) ) ;
#74769 = CARTESIAN_POINT ( 'NONE',  ( 5.161016356839920327, 1485.814728700380101, 218.5690746218629954 ) ) ;
#74770 = CARTESIAN_POINT ( 'NONE',  ( 12.01083267770000162, 1421.737728622410032, 206.5830778804790100 ) ) ;
#74771 = CYLINDRICAL_SURFACE ( 'NONE', #104105, 2.000000000000003553 ) ;
#74773 = CARTESIAN_POINT ( 'NONE',  ( -8.022894047070002088, 1384.893632254190152, 218.7875299896990100 ) ) ;
#74772 = CARTESIAN_POINT ( 'NONE',  ( -2.291514335905000088, 1517.194972660189933, 216.8481778957070105 ) ) ;
#74774 = CARTESIAN_POINT ( 'NONE',  ( -25.87869575008628686, 1450.783544060030181, 136.8232913390557144 ) ) ;
#74775 = CARTESIAN_POINT ( 'NONE',  ( 10.10004869885234058, 1422.222932908421171, 137.0999999980978430 ) ) ;
#74776 = VECTOR ( 'NONE', #80041, 1000.000000000000114 ) ;
#74777 = ORIENTED_EDGE ( 'NONE', *, *, #54196, .T. ) ;
#74778 = CARTESIAN_POINT ( 'NONE',  ( 7.326795523374999952, 1516.760434454289907, 203.3416138547669902 ) ) ;
#74779 = CARTESIAN_POINT ( 'NONE',  ( -15.36767547136500056, 1514.414736986979960, 224.4986524488670057 ) ) ;
#74780 = CARTESIAN_POINT ( 'NONE',  ( 6.742044461270444877, 1509.032357807656808, 216.2339689528981239 ) ) ;
#74781 = EDGE_CURVE ( 'NONE', #39868, #55319, #23382, .T. ) ;
#74782 = CARTESIAN_POINT ( 'NONE',  ( 21.16233094960000116, 1454.406918326630148, 221.8286195809980086 ) ) ;
#74783 = CARTESIAN_POINT ( 'NONE',  ( 10.94775415561070098, 1461.310702779670009, 209.6708789985609940 ) ) ;
#74784 = CARTESIAN_POINT ( 'NONE',  ( -5.441602405930001218, 1420.475810304129936, 186.6133007815980136 ) ) ;
#74785 = CARTESIAN_POINT ( 'NONE',  ( 4.297841960619999568, 1466.500008501689990, 218.4916883454490062 ) ) ;
#74786 = CARTESIAN_POINT ( 'NONE',  ( 3.851527341300000185, 1440.290862272119966, 184.6363558007980146 ) ) ;
#74787 = EDGE_CURVE ( 'NONE', #49270, #72812, #90853, .T. ) ;
#74788 = CARTESIAN_POINT ( 'NONE',  ( 40.02436149072349991, 1445.627823825280075, 136.8606774784030051 ) ) ;
#74789 = CARTESIAN_POINT ( 'NONE',  ( -20.08934789279999933, 1426.987235077529931, 222.3577178168980026 ) ) ;
#74790 = CARTESIAN_POINT ( 'NONE',  ( 10.68615365387295846, 1489.405825820419523, 206.7782173583013616 ) ) ;
#74791 = CARTESIAN_POINT ( 'NONE',  ( -105.7729677439999989, 1391.435361027740100, 301.9753519533589952 ) ) ;
#74792 = CARTESIAN_POINT ( 'NONE',  ( 15.36922853749999973, 1507.577586422630020, 186.8522449740979994 ) ) ;
#74793 = CARTESIAN_POINT ( 'NONE',  ( 20.49599333844836124, 1525.960063244517187, 184.3798832129035645 ) ) ;
#74794 = CARTESIAN_POINT ( 'NONE',  ( -30.89477149620823937, 1461.567857698084026, 269.4805871490156619 ) ) ;
#74795 = ORIENTED_EDGE ( 'NONE', *, *, #46404, .F. ) ;
#74796 = CARTESIAN_POINT ( 'NONE',  ( 0.8141018274779999730, 1430.453334911130241, 150.3332009510979788 ) ) ;
#74797 = CARTESIAN_POINT ( 'NONE',  ( -42.05335041385732353, 1427.628721445028987, 269.0743441695974525 ) ) ;
#74798 = EDGE_CURVE ( 'NONE', #90799, #70084, #41236, .T. ) ;
#74799 = AXIS2_PLACEMENT_3D ( 'NONE', #26745, #2689, #105123 ) ;
#74800 = CARTESIAN_POINT ( 'NONE',  ( -4.678149183724549687, 1508.611352722540005, 212.6094318194529933 ) ) ;
#74801 = CARTESIAN_POINT ( 'NONE',  ( 0.000000000000000000, 1414.421228241719973, 209.1218459616989946 ) ) ;
#74802 = CARTESIAN_POINT ( 'NONE',  ( -0.01334073050390000015, 1417.281753868929854, 234.8503427052979760 ) ) ;
#74803 = CARTESIAN_POINT ( 'NONE',  ( -13.09006439999744309, 1443.016537806267934, 186.6523555623594177 ) ) ;
#74804 = CARTESIAN_POINT ( 'NONE',  ( -9.405025281284439487, 1438.375388356170106, 210.4453402788009839 ) ) ;
#74805 = FACE_OUTER_BOUND ( 'NONE', #49838, .T. ) ;
#74806 = EDGE_CURVE ( 'NONE', #94930, #56950, #101415, .T. ) ;
#74807 = CARTESIAN_POINT ( 'NONE',  ( -1.160519492789278573, 1415.499451156714713, 233.2391781844445404 ) ) ;
#74808 = CARTESIAN_POINT ( 'NONE',  ( -14.91790798717360111, 1415.677402202029953, 207.0650159394080276 ) ) ;
#74809 = CARTESIAN_POINT ( 'NONE',  ( -9.650684282758110299, 1460.400330742749929, 209.4245232134740036 ) ) ;
#74810 = CARTESIAN_POINT ( 'NONE',  ( -12.90463020832708452, 1442.893833669162404, 169.4357342695923592 ) ) ;
#74812 = VERTEX_POINT ( 'NONE', #83236 ) ;
#74811 = CARTESIAN_POINT ( 'NONE',  ( -15.05358279999999915, 1410.831827720429828, 226.7261506157979909 ) ) ;
#74813 = CARTESIAN_POINT ( 'NONE',  ( 0.6611933174841589933, 1415.434635989099888, 191.1758574623620177 ) ) ;
#74814 = CARTESIAN_POINT ( 'NONE',  ( 21.93662947122204443, 1509.528752753375102, 226.8343663891151323 ) ) ;
#74815 = VERTEX_POINT ( 'NONE', #40679 ) ;
#74816 = ORIENTED_EDGE ( 'NONE', *, *, #89132, .T. ) ;
#74817 = CARTESIAN_POINT ( 'NONE',  ( 17.06443472855709942, 1415.088506334920112, 209.4325226847720103 ) ) ;
#74818 = CARTESIAN_POINT ( 'NONE',  ( 13.19315069080000136, 1509.373775394329869, 234.6191799994980158 ) ) ;
#74820 = CARTESIAN_POINT ( 'NONE',  ( -24.34117855639999917, 1445.812453778969939, 216.4489897547180135 ) ) ;
#74819 = CARTESIAN_POINT ( 'NONE',  ( 3.592245589920000093, 1454.165506685890023, 217.7999889770889865 ) ) ;
#74821 = CARTESIAN_POINT ( 'NONE',  ( -7.173910393199999902, 1445.489765703290232, 216.0073357348389891 ) ) ;
#74822 = EDGE_CURVE ( 'NONE', #91400, #97154, #108997, .T. ) ;
#74823 = AXIS2_PLACEMENT_3D ( 'NONE', #21040, #12111, #12668 ) ;
#74824 = CARTESIAN_POINT ( 'NONE',  ( -11.64622956740000070, 1433.292780563709812, 151.0149266372979753 ) ) ;
#74825 = CARTESIAN_POINT ( 'NONE',  ( -16.73628186595857059, 1526.382868172863937, 184.0591879540917546 ) ) ;
#74826 = CARTESIAN_POINT ( 'NONE',  ( 24.08426297012860218, 1411.115209414830133, 209.6325633951909708 ) ) ;
#74827 = AXIS2_PLACEMENT_3D ( 'NONE', #46033, #20242, #80718 ) ;
#74828 = CARTESIAN_POINT ( 'NONE',  ( -25.87016399559999869, 1438.590621495679898, 137.3979509201980136 ) ) ;
#74830 = ADVANCED_FACE ( 'NONE', ( #23858 ), #58050, .F. ) ;
#74829 = CARTESIAN_POINT ( 'NONE',  ( -24.36309863860000391, 1438.807150111159899, 211.0250922072579840 ) ) ;
#74831 = FACE_BOUND ( 'NONE', #3965, .T. ) ;
#74832 = CARTESIAN_POINT ( 'NONE',  ( 2.380479430399999874, 1449.688732974869936, 182.4840047008979980 ) ) ;
#74833 = CARTESIAN_POINT ( 'NONE',  ( 6.952323068159633301, 1363.756189849812017, 208.3718459617061285 ) ) ;
#74834 = CARTESIAN_POINT ( 'NONE',  ( -29.86499995759902859, 1510.066214768678947, 213.4342127740283388 ) ) ;
#74836 = ORIENTED_EDGE ( 'NONE', *, *, #44618, .T. ) ;
#74835 = CARTESIAN_POINT ( 'NONE',  ( -2.638813393498400254E-09, 1414.425016002700204, 246.3383374633879725 ) ) ;
#74837 = ORIENTED_EDGE ( 'NONE', *, *, #57715, .T. ) ;
#74838 = CARTESIAN_POINT ( 'NONE',  ( -11.77304318683200002, 1427.201803926489902, 146.6198829697760004 ) ) ;
#74839 = AXIS2_PLACEMENT_3D ( 'NONE', #21966, #14140, #99794 ) ;
#74840 = CARTESIAN_POINT ( 'NONE',  ( -21.43898449730000166, 1507.201558673590171, 216.1670088357489874 ) ) ;
#74841 = CARTESIAN_POINT ( 'NONE',  ( -4.986174233689999902, 1473.385195802330145, 270.3887730020979916 ) ) ;
#74842 = CARTESIAN_POINT ( 'NONE',  ( -110.0634396883849888, 1384.924418016600157, 296.9511783967739689 ) ) ;
#74843 = CARTESIAN_POINT ( 'NONE',  ( -101.7585531180924079, 1320.102705746889797, 310.5815973742185747 ) ) ;
#74845 = CARTESIAN_POINT ( 'NONE',  ( -9.878129727571689500, 1422.666951092116960, 210.6716409553268079 ) ) ;
#74844 = B_SPLINE_CURVE_WITH_KNOTS ( 'NONE', 3,
 ( #109017, #15473, #41794, #926, #43469, #35049 ),
 .UNSPECIFIED., .F., .F.,
 ( 4, 2, 4 ),
 ( 1.353581492229530087E-06, 0.01184126496313610104, 0.02355708206288909673 ),
 .UNSPECIFIED. ) ;
#74846 = CARTESIAN_POINT ( 'NONE',  ( 1.191524307911316916, 1526.382868172864164, 239.2353018730791518 ) ) ;
#74847 = CARTESIAN_POINT ( 'NONE',  ( -8.602127442139998692, 1384.796933599069916, 199.8703343037190052 ) ) ;
#74848 = CARTESIAN_POINT ( 'NONE',  ( -113.4589914632272354, 1379.913060387289988, 306.7211498618012229 ) ) ;
#74849 = CARTESIAN_POINT ( 'NONE',  ( -3.300861552920000275, 1457.646899589489976, 218.4769539783190169 ) ) ;
#74850 = CARTESIAN_POINT ( 'NONE',  ( 10.91103383375193481, 1363.518622284593221, 210.6218459617030021 ) ) ;
#74851 = CARTESIAN_POINT ( 'NONE',  ( -43.87218737955609527, 1429.907377119439843, 267.0500106768220121 ) ) ;
#74852 = ORIENTED_EDGE ( 'NONE', *, *, #21709, .T. ) ;
#74853 = CARTESIAN_POINT ( 'NONE',  ( -4.328003007221890464, 1515.120004566319949, 209.9804044844569830 ) ) ;
#74854 = B_SPLINE_CURVE_WITH_KNOTS ( 'NONE', 3,
 ( #56016, #73366, #56567, #64431, #99088, #90140, #22925, #72820, #73920, #66085 ),
 .UNSPECIFIED., .F., .F.,
 ( 4, 2, 2, 2, 4 ),
 ( 0.000000000000000000, 0.2500000000000000000, 0.5000000000000000000, 0.7500000000000000000, 1.000000000000000000 ),
 .UNSPECIFIED. ) ;
#74855 = VERTEX_POINT ( 'NONE', #9833 ) ;
#74856 = EDGE_LOOP ( 'NONE', ( #24849, #99632, #87060, #61930 ) ) ;
#74857 = CARTESIAN_POINT ( 'NONE',  ( 1.716392741775000008, 1516.788317650260069, 211.9856338259669997 ) ) ;
#74858 = CARTESIAN_POINT ( 'NONE',  ( 4.687027516810611694, 1423.666285210286560, 183.9319128431047261 ) ) ;
#74859 = CARTESIAN_POINT ( 'NONE',  ( -20.49599333844893678, 1525.960063244516959, 184.3798832129038203 ) ) ;
#74860 = VECTOR ( 'NONE', #33901, 1000.000000000000227 ) ;
#74862 = CARTESIAN_POINT ( 'NONE',  ( -2.370970874524632510, 1427.002265528473799, 137.0999999980979851 ) ) ;
#74861 = CARTESIAN_POINT ( 'NONE',  ( -4.609996619675000851, 1516.769879638719885, 212.5810025483170023 ) ) ;
#74863 = CARTESIAN_POINT ( 'NONE',  ( -15.12939613400000027, 1455.450849537030081, 188.6308199800980105 ) ) ;
#74864 = DIRECTION ( 'NONE',  ( 9.156846217086110244E-47, -1.000000000000000000, 1.836970198721029688E-16 ) ) ;
#74865 = EDGE_LOOP ( 'NONE', ( #105976, #74464, #59317, #77335 ) ) ;
#74866 = CARTESIAN_POINT ( 'NONE',  ( -26.81148555899999764, 1435.638120290539973, 136.0770497519980040 ) ) ;
#74867 = CARTESIAN_POINT ( 'NONE',  ( -2.874588960795000148, 1516.606339319019980, 202.5748942495170013 ) ) ;
#74868 = CARTESIAN_POINT ( 'NONE',  ( -41.57727730138044109, 1445.035122391737787, 135.5177457120996110 ) ) ;
#74869 = CARTESIAN_POINT ( 'NONE',  ( -40.61359552661080130, 1384.584710295609966, 213.5025725185709859 ) ) ;
#74870 = CARTESIAN_POINT ( 'NONE',  ( -42.72426141366479868, 1430.577730169959978, 270.2287312818410214 ) ) ;
#74871 = CARTESIAN_POINT ( 'NONE',  ( 5.161277996873639751, 1424.205379132380131, 193.2953224460849810 ) ) ;
#74872 = CARTESIAN_POINT ( 'NONE',  ( -2.228622948780000446, 1395.990885615630077, 198.2489192474980086 ) ) ;
#74874 = ORIENTED_EDGE ( 'NONE', *, *, #72677, .T. ) ;
#74873 = CARTESIAN_POINT ( 'NONE',  ( -38.60856581307790236, 1443.613625294319945, 137.1750438966080026 ) ) ;
#74875 = ORIENTED_EDGE ( 'NONE', *, *, #324, .T. ) ;
#74876 = CARTESIAN_POINT ( 'NONE',  ( 0.3174014934009999900, 1451.682253938030044, 183.0610148633980145 ) ) ;
#74877 = CARTESIAN_POINT ( 'NONE',  ( -28.97303002314116682, 1526.186458717541882, 220.8123550170195699 ) ) ;
#74878 = CARTESIAN_POINT ( 'NONE',  ( 1.581629459946789940, 1425.904611509570032, 191.1542090707819739 ) ) ;
#74879 = EDGE_CURVE ( 'NONE', #98801, #100321, #57403, .T. ) ;
#74880 = CARTESIAN_POINT ( 'NONE',  ( -25.03982234340000090, 1436.292317311149873, 137.6710093398980064 ) ) ;
#74881 = CARTESIAN_POINT ( 'NONE',  ( -24.66797713489999921, 1441.969358036629956, 210.7253539414180068 ) ) ;
#74882 = B_SPLINE_CURVE_WITH_KNOTS ( 'NONE', 3,
 ( #34851, #69040, #52230, #28108 ),
 .UNSPECIFIED., .F., .F.,
 ( 4, 4 ),
 ( 0.000000000000000000, 0.0002960034161023843515 ),
 .UNSPECIFIED. ) ;
#74883 = CARTESIAN_POINT ( 'NONE',  ( -3.251611363945000388, 1516.779243033999819, 211.4202154400570066 ) ) ;
#74884 = CARTESIAN_POINT ( 'NONE',  ( -68.78640996459999712, 1379.747964976010053, 280.2617497814590024 ) ) ;
#74885 = CARTESIAN_POINT ( 'NONE',  ( -2.355747397201679583, 1484.256314648310081, 183.1724393876219779 ) ) ;
#74886 = CARTESIAN_POINT ( 'NONE',  ( 8.580955436158870242, 1438.351440300460126, 210.6486608506509981 ) ) ;
#74887 = CARTESIAN_POINT ( 'NONE',  ( 3.751161017837588041, 1440.869524849231766, 156.4631710623298204 ) ) ;
#74888 = CARTESIAN_POINT ( 'NONE',  ( 2.864043418315000089, 1516.811292230880099, 206.8228319013669818 ) ) ;
#74889 = ORIENTED_EDGE ( 'NONE', *, *, #12469, .F. ) ;
#74890 = CARTESIAN_POINT ( 'NONE',  ( -7.965999071544743515, 1384.920974961468573, 199.4892359573080682 ) ) ;
#74891 = CARTESIAN_POINT ( 'NONE',  ( -8.588688654723730664, 1437.818490182359938, 207.9409985343149856 ) ) ;
#74892 = CARTESIAN_POINT ( 'NONE',  ( -13.36052273939999857, 1384.881792980340151, 218.9673617354289945 ) ) ;
#74893 = ORIENTED_EDGE ( 'NONE', *, *, #52190, .F. ) ;
#74894 = CARTESIAN_POINT ( 'NONE',  ( 21.53981368633935745, 1523.542365884049104, 234.3096115065364984 ) ) ;
#74895 = EDGE_CURVE ( 'NONE', #53103, #14695, #62832, .T. ) ;
#74896 = CARTESIAN_POINT ( 'NONE',  ( 12.88043371926620040, 1435.836274709469990, 150.7661302149069797 ) ) ;
#74897 = B_SPLINE_SURFACE_WITH_KNOTS ( 'NONE', 5, 5, ( 
 ( #50917, #108608, #101838, #25133, #100738, #85048 ),
 ( #24022, #103506, #26808, #53136, #68840, #52582 ),
 ( #71058, #85593, #95121, #1082, #45292, #52025 ),
 ( #86716, #17269, #10008, #60433, #60995, #86165 ),
 ( #78890, #2196, #96225, #95672, #104065, #36865 ),
 ( #9457, #2744, #59878, #18385, #70505, #44179 ) ),
 .UNSPECIFIED., .F., .F., .F.,
 ( 6, 6 ),
 ( 6, 6 ),
 ( 7.548656686150499340, 12.57640183258060063 ),
 ( 0.000000000000000000, 0.5000176499934450014 ),
 .UNSPECIFIED. ) ;
#74898 = CARTESIAN_POINT ( 'NONE',  ( 13.36059434040000049, 1414.988017874730076, 197.8813517676980211 ) ) ;
#74899 = CARTESIAN_POINT ( 'NONE',  ( 15.68481150160000048, 1430.205911231830214, 190.9194062192979970 ) ) ;
#74900 = CARTESIAN_POINT ( 'NONE',  ( 23.84533589473599946, 1452.080362908450070, 136.9869410992479857 ) ) ;
#74901 = EDGE_CURVE ( 'NONE', #69928, #103394, #52963, .T. ) ;
#74902 = CARTESIAN_POINT ( 'NONE',  ( 3.545671383367217100, 1450.748354634506541, 184.0780438961519678 ) ) ;
#74903 = CARTESIAN_POINT ( 'NONE',  ( 6.910350421100000418, 1487.761360645689820, 200.5560116829490198 ) ) ;
#74904 = CARTESIAN_POINT ( 'NONE',  ( -3.344817776469899862, 1476.714814503689922, 199.3081550772679975 ) ) ;
#74905 = CARTESIAN_POINT ( 'NONE',  ( 24.55734822141088003, 1443.697998701720280, 213.2430772723361372 ) ) ;
#74906 = CARTESIAN_POINT ( 'NONE',  ( -3.805396659119999914, 1495.647976226690162, 219.6495707272989932 ) ) ;
#74907 = STYLED_ITEM ( 'NONE', ( #82809 ), #45166 ) ;
#74908 = CARTESIAN_POINT ( 'NONE',  ( -1.731498172528467938, 1450.471748407974928, 182.5592355860798648 ) ) ;
#74909 = CARTESIAN_POINT ( 'NONE',  ( -6.941100315875000426, 1516.858069504249897, 216.0654486236869900 ) ) ;
#74910 = ORIENTED_EDGE ( 'NONE', *, *, #88529, .T. ) ;
#74911 = DIRECTION ( 'NONE',  ( -1.000000000000000000, 0.000000000000000000, 0.000000000000000000 ) ) ;
#74912 = CARTESIAN_POINT ( 'NONE',  ( -16.87197715709999812, 1420.411836349220039, 203.4718720851689966 ) ) ;
#74913 = AXIS2_PLACEMENT_3D ( 'NONE', #36383, #70571, #27984 ) ;
#74914 = CARTESIAN_POINT ( 'NONE',  ( 2.378562897450000158, 1421.262547136429930, 183.2548472359979996 ) ) ;
#74915 =( BOUNDED_SURFACE ( )  B_SPLINE_SURFACE ( 3, 2, ( 
 ( #12951, #47132, #82918 ),
 ( #38707, #4573, #90767 ),
 ( #14047, #82378, #5678 ),
 ( #73984, #65590, #32527 ),
 ( #6755, #49334, #59400 ),
 ( #75095, #66699, #16784 ),
 ( #100278, #33061, #57750 ),
 ( #101344, #84019, #102463 ),
 ( #43137, #67249, #58832 ),
 ( #25753, #108674, #40915 ) ),
 .UNSPECIFIED., .F., .F., .F. ) 
 B_SPLINE_SURFACE_WITH_KNOTS ( ( 4, 2, 2, 2, 4 ),
 ( 3, 3 ),
 ( 1.570796326794896558, 1.963495408493620697, 2.356194490192344837, 2.748893571891068976, 3.141592653589793116 ),
 ( 0.000000000000000000, 1.000000000000000000 ),
 .UNSPECIFIED. ) 
 GEOMETRIC_REPRESENTATION_ITEM ( )  RATIONAL_B_SPLINE_SURFACE ( (
 ( 1.000000000000000000, 0.7071067811865904273, 1.000000000000000000),
 ( 1.000000000000000000, 0.7166207884824742358, 1.000000000000000000),
 ( 1.000000000000000000, 0.7259222650903540686, 1.000000000000000000),
 ( 1.000000000000000000, 0.7428408967933899376, 1.000000000000000000),
 ( 1.000000000000000000, 0.7504512394528214392, 1.000000000000000000),
 ( 1.000000000000000000, 0.7630177051946679390, 1.000000000000000000),
 ( 1.000000000000000000, 0.7679730451967922145, 1.000000000000000000),
 ( 1.000000000000000000, 0.7746454561802565975, 1.000000000000000000),
 ( 1.000000000000000000, 0.7763684247031245045, 1.000000000000000000),
 ( 1.000000000000000000, 0.7763623250684338339, 1.000000000000000000) ) ) 
 REPRESENTATION_ITEM ( '' )  SURFACE ( )  );
#74916 = CARTESIAN_POINT ( 'NONE',  ( -1.402942795860000036, 1473.972991866589837, 219.3058795016989961 ) ) ;
#74917 = CARTESIAN_POINT ( 'NONE',  ( -11072.05219665070763, 50.13405481564041821, -8413.031381324366521 ) ) ;
#74918 = CARTESIAN_POINT ( 'NONE',  ( 1.914156658600000060, 1431.087920121590059, 199.8421650995689731 ) ) ;
#74919 = CARTESIAN_POINT ( 'NONE',  ( -6.400436228969967445, 1508.335654507707204, 219.9811977713085582 ) ) ;
#74920 = CARTESIAN_POINT ( 'NONE',  ( 18.72518989680000345, 1416.274718422629803, 209.8658817986590179 ) ) ;
#74922 = EDGE_CURVE ( 'NONE', #96418, #63858, #2, .T. ) ;
#74921 = CARTESIAN_POINT ( 'NONE',  ( -1.966553775129000314, 1454.917737290639934, 198.8051624357930223 ) ) ;
#74923 = CARTESIAN_POINT ( 'NONE',  ( -9.429479337035831822E-07, 1408.510422154009802, 222.8906800396250105 ) ) ;
#74924 = CARTESIAN_POINT ( 'NONE',  ( 38.81943119499100447, 1440.913060376880139, 257.5592801587829968 ) ) ;
#74926 = DIRECTION ( 'NONE',  ( 0.4999999999998399058, 0.7071067811867739472, 0.4999999999998399058 ) ) ;
#74925 = CARTESIAN_POINT ( 'NONE',  ( -10.93154302307010006, 1470.132843826959970, 212.2379041850950046 ) ) ;
#74927 = LINE ( 'NONE', #22820, #36730 ) ;
#74928 = ORIENTED_EDGE ( 'NONE', *, *, #92600, .T. ) ;
#74929 = ADVANCED_FACE ( 'NONE', ( #60824 ), #53607, .T. ) ;
#74930 = ORIENTED_EDGE ( 'NONE', *, *, #81221, .F. ) ;
#74931 = CARTESIAN_POINT ( 'NONE',  ( 5.262016255162093259, 1441.844739931066215, 216.2609436936466238 ) ) ;
#74932 = ADVANCED_FACE ( 'NONE', ( #42897 ), #27195, .F. ) ;
#74933 = CARTESIAN_POINT ( 'NONE',  ( -19.67949054060972003, 1485.238787255277430, 190.3370324724980662 ) ) ;
#74934 = CARTESIAN_POINT ( 'NONE',  ( -1.435439190950000166, 1443.368777369690179, 200.1970386830489872 ) ) ;
#74935 = CARTESIAN_POINT ( 'NONE',  ( -0.5620977654635980203, 1416.851343899799986, 227.7685710128770040 ) ) ;
#74936 = CARTESIAN_POINT ( 'NONE',  ( 1.747240526076377476, 1508.468491276751138, 237.2463171574812293 ) ) ;
#74937 = CARTESIAN_POINT ( 'NONE',  ( 26.95974481528090649, 1509.967011703660091, 222.3600134204636163 ) ) ;
#74938 = B_SPLINE_CURVE_WITH_KNOTS ( 'NONE', 3,
 ( #32040, #82455, #38782, #5752, #72958, #39894, #74062, #64575, #48871, #6288, #55070, #100875, #60019, #9039, #32599, #76250, #662, #66776, #91943, #40987, #33133, #93038, #101982, #93579, #51058 ),
 .UNSPECIFIED., .F., .F.,
 ( 4, 3, 3, 3, 3, 3, 3, 3, 4 ),
 ( -9.314730572460000246, -9.152340534729230370, -7.863899930683609263, -6.569977427668559855, -5.272424565628810456, -3.924989230018409714, -2.618936221757099503, -1.310405461081899148, 0.000000000000000000 ),
 .UNSPECIFIED. ) ;
#74939 = EDGE_CURVE ( 'NONE', #7907, #83109, #48287, .T. ) ;
#74940 = CARTESIAN_POINT ( 'NONE',  ( -0.2978291352960920069, 1508.551704408389924, 220.0371209971259816 ) ) ;
#74941 = CARTESIAN_POINT ( 'NONE',  ( 18.40343465886133600, 1525.402221411349956, 179.8532301504589839 ) ) ;
#74942 = CARTESIAN_POINT ( 'NONE',  ( -36.89664068000400476, 1383.832789048189852, 236.6899286370959885 ) ) ;
#74943 = CARTESIAN_POINT ( 'NONE',  ( -5.181410188784999704, 1510.418062979269962, 201.5729736320070060 ) ) ;
#74944 = CARTESIAN_POINT ( 'NONE',  ( 5.360248604747719803, 1422.242465614079947, 144.1680528682020110 ) ) ;
#74945 = CARTESIAN_POINT ( 'NONE',  ( -11.91268647012529946, 1502.145580229700045, 208.8923034686130222 ) ) ;
#74946 = CARTESIAN_POINT ( 'NONE',  ( 10.90310790672270080, 1491.867556085790056, 211.5980998715699855 ) ) ;
#74948 = ORIENTED_EDGE ( 'NONE', *, *, #102175, .F. ) ;
#74947 = CARTESIAN_POINT ( 'NONE',  ( -2.705951369970000187, 1457.026427619289962, 218.3778972485089866 ) ) ;
#74949 = CARTESIAN_POINT ( 'NONE',  ( 0.5779273184081700210, 1517.151704408390060, 232.1634304495918002 ) ) ;
#74950 = CARTESIAN_POINT ( 'NONE',  ( -57.78400604769999660, 1379.993142806879860, 268.6303832713589372 ) ) ;
#74951 = CARTESIAN_POINT ( 'NONE',  ( -0.7593982673170009967, 1430.316802068590050, 217.4503154216889982 ) ) ;
#74952 = ORIENTED_EDGE ( 'NONE', *, *, #38978, .F. ) ;
#74953 = VERTEX_POINT ( 'NONE', #87096 ) ;
#74954 = CARTESIAN_POINT ( 'NONE',  ( -7.832093571712239743, 1386.408921254229881, 218.8164462652940188 ) ) ;
#74955 = CARTESIAN_POINT ( 'NONE',  ( 35.78517889623469728, 1437.356590274589962, 136.5362015133650004 ) ) ;
#74957 = CARTESIAN_POINT ( 'NONE',  ( 1.137831829869999867, 1408.952794351630018, 231.4765879240979984 ) ) ;
#74956 = DIRECTION ( 'NONE',  ( -0.9455185755993178454, 0.000000000000000000, 0.3255681544571539243 ) ) ;
#74958 = ADVANCED_FACE ( 'NONE', ( #906 ), #79522, .F. ) ;
#74959 = CARTESIAN_POINT ( 'NONE',  ( 7.211935934568218798, 1522.051704408389924, 224.6757451961901495 ) ) ;
#74960 = CARTESIAN_POINT ( 'NONE',  ( -106.4588356590000018, 1379.450307938419883, 300.3490905575590091 ) ) ;
#74961 = DIRECTION ( 'NONE',  ( 0.4090087482554252696, -0.000000000000000000, -0.9125304618753996566 ) ) ;
#74962 = CARTESIAN_POINT ( 'NONE',  ( -10.19854404760319966, 1508.551704408389924, 218.1794582448719950 ) ) ;
#74963 = CARTESIAN_POINT ( 'NONE',  ( 10.09968471107369936, 1409.265749149070189, 198.0954670411109930 ) ) ;
#74964 = CARTESIAN_POINT ( 'NONE',  ( 18.03149116639599825, 1424.668758022952034, 225.2946740050300036 ) ) ;
#74965 = CARTESIAN_POINT ( 'NONE',  ( 18.87853829029999986, 1458.344553362990155, 213.8102309971890236 ) ) ;
#74966 = ADVANCED_FACE ( 'NONE', ( #20974 ), #42838, .T. ) ;
#74967 = CARTESIAN_POINT ( 'NONE',  ( 3.974452695383380085, 1433.901817095809974, 201.5205318130460341 ) ) ;
#74968 = CARTESIAN_POINT ( 'NONE',  ( -2.500000000000000000, 1439.447167954220049, 162.2860246256229857 ) ) ;
#74969 = AXIS2_PLACEMENT_3D ( 'NONE', #84011, #7312, #101336 ) ;
#74970 = CARTESIAN_POINT ( 'NONE',  ( -2.497948021501850135, 1449.239010218830117, 183.3628261147359808 ) ) ;
#74971 = ORIENTED_EDGE ( 'NONE', *, *, #83036, .F. ) ;
#74972 = EDGE_CURVE ( 'NONE', #60117, #59101, #72516, .T. ) ;
#74973 = CARTESIAN_POINT ( 'NONE',  ( 3.946018174590000300E-15, 1427.166763959530044, 147.9649995502979891 ) ) ;
#74974 = CARTESIAN_POINT ( 'NONE',  ( -5.510229795562198163, 1427.334330648820014, 134.0999999980980135 ) ) ;
#74975 = CARTESIAN_POINT ( 'NONE',  ( -12.84242185500000133, 1435.935690871960105, 150.8114634387980004 ) ) ;
#74976 = CIRCLE ( 'NONE', #26665, 1.999999999999998890 ) ;
#74977 = CARTESIAN_POINT ( 'NONE',  ( -7.722580352405000070, 1517.051704408389924, 207.5526846776770071 ) ) ;
#74978 = CARTESIAN_POINT ( 'NONE',  ( 0.3106507903294934980, 1515.598599846736306, 213.1604233196099756 ) ) ;
#74979 = DIRECTION ( 'NONE',  ( -0.000000000000000000, -1.000000000000000000, -0.000000000000000000 ) ) ;
#74980 = CARTESIAN_POINT ( 'NONE',  ( -109.3083912430000026, 1384.947610311819972, 311.2693625272590339 ) ) ;
#74981 = CARTESIAN_POINT ( 'NONE',  ( -1.213587419969999859, 1484.841083681130158, 182.2078730101980000 ) ) ;
#74982 = CARTESIAN_POINT ( 'NONE',  ( -9.351651288933469530, 1361.678816003299744, 210.6218459617030021 ) ) ;
#74983 = CARTESIAN_POINT ( 'NONE',  ( 4.900006679340000559, 1499.255191946190052, 229.7873568473989963 ) ) ;
#74984 = CARTESIAN_POINT ( 'NONE',  ( 2.029027972364500165, 1429.198891036370014, 217.1629461471520131 ) ) ;
#74985 = CARTESIAN_POINT ( 'NONE',  ( -7.675048655830000399, 1425.718923958530013, 206.0025236838089882 ) ) ;
#74986 = CARTESIAN_POINT ( 'NONE',  ( 3.261652286895000419, 1516.939580991450157, 209.1085619926769823 ) ) ;
#74987 = CARTESIAN_POINT ( 'NONE',  ( 4.305761763093079786, 1409.063420901319887, 223.2590317760309802 ) ) ;
#74988 = CARTESIAN_POINT ( 'NONE',  ( -1.887379141860000057E-14, 1421.846726402829972, 101.6565998076979866 ) ) ;
#74989 = CARTESIAN_POINT ( 'NONE',  ( 7.324673508793529741, 1425.042193375519901, 212.6072707562309745 ) ) ;
#74990 = VECTOR ( 'NONE', #35345, 1000.000000000000114 ) ;
#74991 = ORIENTED_EDGE ( 'NONE', *, *, #26521, .F. ) ;
#74992 = VECTOR ( 'NONE', #70168, 1000.000000000000114 ) ;
#74993 = CARTESIAN_POINT ( 'NONE',  ( 25.42954073489999800, 1428.064052004430096, 238.1443969920979953 ) ) ;
#74995 = CARTESIAN_POINT ( 'NONE',  ( -15.02944349056170026, 1512.205851781539877, 221.7001744404510077 ) ) ;
#74994 = CARTESIAN_POINT ( 'NONE',  ( -2.469785781769999744, 1452.697316747630111, 183.1533515108980055 ) ) ;
#74996 = CARTESIAN_POINT ( 'NONE',  ( -6.119584387729999797, 1461.516739551189858, 206.9548909377989787 ) ) ;
#74997 = CARTESIAN_POINT ( 'NONE',  ( -4.329448776040000446, 1515.064792882589927, 207.2788837304390199 ) ) ;
#74998 = CARTESIAN_POINT ( 'NONE',  ( 0.5000000000000000000, 1448.894380913990062, 169.0327022760979787 ) ) ;
#74999 = CARTESIAN_POINT ( 'NONE',  ( -14.69392519634950034, 1452.399937212599980, 148.0737491589720207 ) ) ;
#75000 = CARTESIAN_POINT ( 'NONE',  ( -18.95862648649999826, 1416.832348283729971, 207.7798716402180048 ) ) ;
#75001 = VERTEX_POINT ( 'NONE', #107204 ) ;
#75002 = CARTESIAN_POINT ( 'NONE',  ( -2.500000000000000000, 1419.382839489710022, 144.1073622044459910 ) ) ;
#75003 = DIRECTION ( 'NONE',  ( 0.000000000000000000, 0.000000000000000000, 1.000000000000000000 ) ) ;
#75004 = CARTESIAN_POINT ( 'NONE',  ( 16.26552582369990319, 1422.904278802180215, 227.8875789372550003 ) ) ;
#75005 = CARTESIAN_POINT ( 'NONE',  ( 11.40660427760000140, 1502.131503807389890, 207.7526879073789985 ) ) ;
#75006 = ORIENTED_EDGE ( 'NONE', *, *, #85135, .T. ) ;
#75007 = ORIENTED_EDGE ( 'NONE', *, *, #95918, .F. ) ;
#75008 = CARTESIAN_POINT ( 'NONE',  ( -85.85832257059999506, 1385.179345198489955, 289.6849318678590066 ) ) ;
#75009 = CARTESIAN_POINT ( 'NONE',  ( -22.93094644840109808, 1409.723536851819972, 208.9950183821200085 ) ) ;
#75010 = CARTESIAN_POINT ( 'NONE',  ( -3.826489878020000290, 1424.302205092830036, 185.3920305880980095 ) ) ;
#75011 = CIRCLE ( 'NONE', #59035, 12.34219900309999929 ) ;
#75012 = CARTESIAN_POINT ( 'NONE',  ( 7.626975074059999748, 1491.048095285289946, 210.5944414621689873 ) ) ;
#75013 = CARTESIAN_POINT ( 'NONE',  ( -10.00550473600000068, 1507.632999467629816, 234.5106451484979857 ) ) ;
#75014 = CARTESIAN_POINT ( 'NONE',  ( 4.544868981635990401, 1508.551704407889929, 213.0836524628859934 ) ) ;
#75015 = ORIENTED_EDGE ( 'NONE', *, *, #100368, .F. ) ;
#75016 = CARTESIAN_POINT ( 'NONE',  ( 43.45502302935310723, 1452.785528273959926, 266.7626567147260062 ) ) ;
#75017 = CARTESIAN_POINT ( 'NONE',  ( -4.833437595822498878, 1508.551704408439946, 205.2116919714409846 ) ) ;
#75018 = CARTESIAN_POINT ( 'NONE',  ( 0.01343953231439999965, 1420.440497145129939, 182.6621881913980019 ) ) ;
#75019 = CARTESIAN_POINT ( 'NONE',  ( 4.997573787194999895, 1516.742629295279812, 205.6633194342169872 ) ) ;
#75020 = VERTEX_POINT ( 'NONE', #80909 ) ;
#75021 = CARTESIAN_POINT ( 'NONE',  ( 18.94560633146422646, 1457.569462139888174, 226.8026088545746575 ) ) ;
#75022 = CARTESIAN_POINT ( 'NONE',  ( 15.03014119857349939, 1513.722010160979835, 194.4919335047299853 ) ) ;
#75023 = CARTESIAN_POINT ( 'NONE',  ( 9.809383389668809627, 1433.663778845850175, 224.8559793928490080 ) ) ;
#75024 = ORIENTED_EDGE ( 'NONE', *, *, #30281, .T. ) ;
#75026 = VECTOR ( 'NONE', #65334, 1000.000000000000114 ) ;
#75025 = CARTESIAN_POINT ( 'NONE',  ( -11.87165566641069958, 1481.759760406750047, 209.4550520684960020 ) ) ;
#75027 = CARTESIAN_POINT ( 'NONE',  ( 26.92382706682879956, 1450.690882430039892, 136.4499193319570054 ) ) ;
#75028 = CARTESIAN_POINT ( 'NONE',  ( -14.28356510322089790, 1513.356256558030054, 193.9291527242570226 ) ) ;
#75029 = CARTESIAN_POINT ( 'NONE',  ( 8.621399425004019790, 1503.742512659089925, 218.5082872257249846 ) ) ;
#75030 = CARTESIAN_POINT ( 'NONE',  ( 7.424966210989999205, 1422.119254455250029, 195.6160877161989902 ) ) ;
#75032 = B_SPLINE_SURFACE_WITH_KNOTS ( 'NONE', 5, 5, ( 
 ( #57849, #91977, #66806, #15252, #65694, #23106 ),
 ( #30968, #92516, #100907, #99812, #83566, #24205 ),
 ( #22535, #90872, #49985, #6859, #56736, #14160 ),
 ( #48346, #58391, #82485, #15784, #18556, #1243 ),
 ( #77394, #43245, #76284, #17442, #78494, #42682 ),
 ( #696, #86331, #25853, #27533, #25297, #93609 ),
 ( #60054, #85218, #93071, #103117, #35945, #16345 ),
 ( #34825, #1808, #52750, #102560, #76840, #77936 ),
 ( #33712, #18011, #50543, #69012, #8509, #94172 ) ),
 .UNSPECIFIED., .F., .F., .F.,
 ( 6, 3, 6 ),
 ( 6, 6 ),
 ( 3.171312204904120247, 5.447745999499999492, 7.724179794085880069 ),
 ( -2.050297588106100003E-05, 2.000000000000000000 ),
 .UNSPECIFIED. ) ;
#75031 = CARTESIAN_POINT ( 'NONE',  ( 1.066132977100159973, 1431.451844506829730, 218.5524226113819850 ) ) ;
#75033 = CARTESIAN_POINT ( 'NONE',  ( 10.25673954719900038, 1479.616108303600186, 205.9965886202919876 ) ) ;
#75034 = CARTESIAN_POINT ( 'NONE',  ( 2.069045789006210168, 1408.985313058389920, 186.9468566560059912 ) ) ;
#75036 = CARTESIAN_POINT ( 'NONE',  ( -9.849896899200842881, 1512.913060387330006, 185.5490084180013923 ) ) ;
#75035 = CARTESIAN_POINT ( 'NONE',  ( -13.70980395804599894, 1434.975228763560153, 148.6203963862629962 ) ) ;
#75037 = CARTESIAN_POINT ( 'NONE',  ( 11.79199745574979907, 1426.669443530059880, 206.5449107423220028 ) ) ;
#75038 = B_SPLINE_CURVE_WITH_KNOTS ( 'NONE', 5,
 ( #96791, #19506, #53711, #45297, #69399, #61546, #34660, #52587, #95677 ),
 .UNSPECIFIED., .F., .F.,
 ( 6, 3, 6 ),
 ( 0.8631819232519999385, 2.053866005980000242, 3.194084093449060191 ),
 .UNSPECIFIED. ) ;
#75039 = CARTESIAN_POINT ( 'NONE',  ( -10.86174217150000132, 1379.353463880399886, 215.1474020563989882 ) ) ;
#75040 = ORIENTED_EDGE ( 'NONE', *, *, #83689, .F. ) ;
#75041 = CARTESIAN_POINT ( 'NONE',  ( 13.84930592310000108, 1431.437219492539953, 209.1218459616979999 ) ) ;
#75042 = VECTOR ( 'NONE', #73525, 1000.000000000000114 ) ;
#75043 = CARTESIAN_POINT ( 'NONE',  ( 19.42500282749999840, 1440.913060387330006, 212.4633492400480179 ) ) ;
#75044 = CARTESIAN_POINT ( 'NONE',  ( 32.38114538885250226, 1523.604703353109699, 202.1233279672528624 ) ) ;
#75045 = B_SPLINE_SURFACE_WITH_KNOTS ( 'NONE', 5, 5, ( 
 ( #19170, #12984, #36553, #47167, #28150, #81295 ),
 ( #53376, #87522, #70750, #96465, #19745, #82419 ),
 ( #83493, #100838, #107060, #99188, #40950, #72921 ),
 ( #56668, #81844, #14645, #84051, #30893, #56112 ),
 ( #15178, #5713, #22468, #92440, #39858, #74021 ),
 ( #6789, #32559, #21916, #75127, #109275, #65072 ),
 ( #108155, #31445, #91901, #65628, #66735, #30344 ),
 ( #99742, #23033, #64535, #48831, #90804, #57783 ),
 ( #15716, #48275, #108710, #14085, #49917, #24127 ) ),
 .UNSPECIFIED., .F., .F., .F.,
 ( 6, 3, 6 ),
 ( 6, 6 ),
 ( 3.182123501530000009, 5.472533560919999651, 7.762943620309999737 ),
 ( 0.000000000000000000, 2.000000000000000000 ),
 .UNSPECIFIED. ) ;
#75046 = CARTESIAN_POINT ( 'NONE',  ( -9.189822540219999780, 1387.666581765899991, 200.6527716693889829 ) ) ;
#75047 = CARTESIAN_POINT ( 'NONE',  ( 9.844913728421918364, 1422.934237187859935, 210.2671035938940065 ) ) ;
#75048 = CARTESIAN_POINT ( 'NONE',  ( 11.17620620616699867, 1424.953917489370269, 203.0360129599930303 ) ) ;
#75049 = B_SPLINE_CURVE_WITH_KNOTS ( 'NONE', 5,
 ( #24217, #15264, #33725, #58403, #101467, #92528 ),
 .UNSPECIFIED., .F., .F.,
 ( 6, 6 ),
 ( 0.000000000000000000, 1.000000000000000000 ),
 .UNSPECIFIED. ) ;
#75050 = FACE_OUTER_BOUND ( 'NONE', #18220, .T. ) ;
#75051 = CARTESIAN_POINT ( 'NONE',  ( -38.34143788450000301, 1440.913060387330006, 265.6112250856980381 ) ) ;
#75052 = AXIS2_PLACEMENT_3D ( 'NONE', #82202, #5506, #22829 ) ;
#75053 = CARTESIAN_POINT ( 'NONE',  ( -9.107652377995819393, 1383.903739771440087, 218.5399116860239985 ) ) ;
#75055 = EDGE_CURVE ( 'NONE', #73175, #107075, #58992, .T. ) ;
#75054 = CARTESIAN_POINT ( 'NONE',  ( 11.19902647940000051, 1433.912128383429945, 151.6118626633980284 ) ) ;
#75056 = CARTESIAN_POINT ( 'NONE',  ( 38.34143791959999703, 1445.301772804310076, 265.6112249940979950 ) ) ;
#75057 = B_SPLINE_SURFACE_WITH_KNOTS ( 'NONE', 5, 5, ( 
 ( #107579, #108121, #13495, #71830, #107029, #31415 ),
 ( #12416, #56086, #57207, #46600, #89671, #30865 ),
 ( #4579, #65040, #63417, #65598, #63957, #99710 ),
 ( #14054, #80735, #105949, #4044, #99157, #98071 ),
 ( #98621, #22436, #21341, #81264, #21884, #38714 ),
 ( #90212, #48243, #58292, #48, #15151, #66705 ) ),
 .UNSPECIFIED., .F., .F., .F.,
 ( 6, 6 ),
 ( 6, 6 ),
 ( 0.9035843706480000126, 1.040557828610000124 ),
 ( 0.000000000000000000, 2.000000000000000000 ),
 .UNSPECIFIED. ) ;
#75058 = CARTESIAN_POINT ( 'NONE',  ( 0.6029167771809720300, 1450.892006063709914, 181.3029698405979957 ) ) ;
#75059 = CARTESIAN_POINT ( 'NONE',  ( -29.67167576298847109, 1526.344110814222859, 201.2571182723721961 ) ) ;
#75060 = CARTESIAN_POINT ( 'NONE',  ( -108.4006655237829619, 1388.767505148533473, 298.1061185306318180 ) ) ;
#75061 = CARTESIAN_POINT ( 'NONE',  ( -15.06280282045160135, 1422.388303761650150, 229.4662100962750060 ) ) ;
#75062 = DIRECTION ( 'NONE',  ( 0.7600087925167849923, -0.4999999999970537456, -0.4151946956550922052 ) ) ;
#75063 = CARTESIAN_POINT ( 'NONE',  ( 0.4794255386042003408, 1405.913060387330006, 209.9994285235883922 ) ) ;
#75064 = CARTESIAN_POINT ( 'NONE',  ( -16.38529143830000123, 1409.485247372730100, 224.6959630481979957 ) ) ;
#75065 = CIRCLE ( 'NONE', #57171, 4.000000000000003553 ) ;
#75066 = CARTESIAN_POINT ( 'NONE',  ( 23.34982412120000106, 1410.912491262029789, 212.3764570079079874 ) ) ;
#75067 = LINE ( 'NONE', #91841, #12744 ) ;
#75068 = CARTESIAN_POINT ( 'NONE',  ( -16.57803587077799889, 1409.491951770299920, 193.0403171756620111 ) ) ;
#75069 = ADVANCED_FACE ( 'NONE', ( #29935 ), #24190, .F. ) ;
#75070 = CARTESIAN_POINT ( 'NONE',  ( 1.129779230730000084, 1515.569191395689813, 205.1526891147690037 ) ) ;
#75071 = CARTESIAN_POINT ( 'NONE',  ( -2.582675909239641854, 1526.178928173327677, 175.9008252398585626 ) ) ;
#75072 = DIRECTION ( 'NONE',  ( -0.6736849260863841948, 0.000000000000000000, 0.7390186874254148774 ) ) ;
#75073 = CARTESIAN_POINT ( 'NONE',  ( -5.414686741919999768, 1414.913060387329779, 224.5644280759980234 ) ) ;
#75074 = CARTESIAN_POINT ( 'NONE',  ( 0.2010103898936379807, 1462.424627048520051, 182.8490255985700230 ) ) ;
#75076 = ORIENTED_EDGE ( 'NONE', *, *, #31936, .T. ) ;
#75075 = CARTESIAN_POINT ( 'NONE',  ( -3.177625270220000075, 1409.024025506930002, 224.1218459461979933 ) ) ;
#75077 = CARTESIAN_POINT ( 'NONE',  ( -20.75326766870000128, 1443.913060387330006, 176.0807405191980024 ) ) ;
#75078 = CARTESIAN_POINT ( 'NONE',  ( 3.347801439296141268, 1512.187213306747481, 242.0893193391992497 ) ) ;
#75079 = CARTESIAN_POINT ( 'NONE',  ( 11.94108349800000113, 1433.615462819619779, 149.6992079387979970 ) ) ;
#75080 = CARTESIAN_POINT ( 'NONE',  ( -41.02967923220330704, 1440.575676735369825, 134.0999999980680002 ) ) ;
#75081 = DIRECTION ( 'NONE',  ( 0.000000000000000000, 1.000000000000000000, 0.000000000000000000 ) ) ;
#75082 = ORIENTED_EDGE ( 'NONE', *, *, #97665, .T. ) ;
#75083 = CARTESIAN_POINT ( 'NONE',  ( -2.170627950300000109, 1485.611815725089855, 197.4219880479989797 ) ) ;
#75084 = CARTESIAN_POINT ( 'NONE',  ( 10.89260962470000038, 1478.390639884389884, 204.6475587744990037 ) ) ;
#75085 = CARTESIAN_POINT ( 'NONE',  ( -106.3938867745919765, 1381.879201070689533, 309.8074937847794104 ) ) ;
#75086 = CARTESIAN_POINT ( 'NONE',  ( -16.50400130224786466, 1525.907212628473644, 181.9890130758379030 ) ) ;
#75087 = CARTESIAN_POINT ( 'NONE',  ( -8.817122548632680079, 1437.178451963229918, 212.6735601864489809 ) ) ;
#75088 = CARTESIAN_POINT ( 'NONE',  ( 40.31042593601753055, 1424.878999494629170, 269.1206013125691356 ) ) ;
#75089 = VECTOR ( 'NONE', #32750, 1000.000000000000000 ) ;
#75090 = DIRECTION ( 'NONE',  ( -5.980589973904019347E-17, 1.000000000000000000, -1.736889445713099699E-16 ) ) ;
#75091 = CARTESIAN_POINT ( 'NONE',  ( -12.31045119110000030, 1378.376187955050000, 209.7947064970570068 ) ) ;
#75092 = CARTESIAN_POINT ( 'NONE',  ( 32.38845791999495560, 1523.382868172864164, 202.1182848005512085 ) ) ;
#75093 = CARTESIAN_POINT ( 'NONE',  ( -52.85310310605240147, 1385.029698763549959, 229.9496117000900028 ) ) ;
#75094 = ADVANCED_FACE ( 'NONE', ( #63585 ), #56810, .T. ) ;
#75095 = CARTESIAN_POINT ( 'NONE',  ( -20.17436656406251672, 1524.841055067849766, 237.7389007707605515 ) ) ;
#75096 = CARTESIAN_POINT ( 'NONE',  ( 11.49495574083080029, 1422.044481766739864, 209.9123749212659789 ) ) ;
#75097 = ORIENTED_EDGE ( 'NONE', *, *, #108527, .T. ) ;
#75098 = CARTESIAN_POINT ( 'NONE',  ( -33.91369284169999787, 1450.440667306779915, 136.2454489651980225 ) ) ;
#75099 = CARTESIAN_POINT ( 'NONE',  ( -15.92413569481509938, 1410.572088914639835, 226.6904944114299951 ) ) ;
#75101 = ORIENTED_EDGE ( 'NONE', *, *, #99936, .F. ) ;
#75100 = CARTESIAN_POINT ( 'NONE',  ( 2.673427297959769966, 1437.319176057519826, 227.4663404305809706 ) ) ;
#75102 = CARTESIAN_POINT ( 'NONE',  ( 5.133103592700000384, 1472.975266187489979, 218.0948351415289892 ) ) ;
#75103 = CARTESIAN_POINT ( 'NONE',  ( 10.50142226597180084, 1470.839680593169987, 210.1830287100939927 ) ) ;
#75104 = ADVANCED_FACE ( 'NONE', ( #98247 ), #43706, .T. ) ;
#75105 = CARTESIAN_POINT ( 'NONE',  ( -20.45839004848103926, 1410.987468509325026, 219.7938153870166218 ) ) ;
#75106 = CARTESIAN_POINT ( 'NONE',  ( -109.1338056169999930, 1384.841083573769993, 311.2641749022590147 ) ) ;
#75107 = CARTESIAN_POINT ( 'NONE',  ( -11.58478124459999847, 1415.063410489729904, 195.8970895505979968 ) ) ;
#75108 = CIRCLE ( 'NONE', #41118, 2.000000000000001776 ) ;
#75109 = CARTESIAN_POINT ( 'NONE',  ( 17.99954280510000260, 1410.904693935329988, 222.9872207667980035 ) ) ;
#75110 = CARTESIAN_POINT ( 'NONE',  ( -9.225907677606096868, 1517.051704408389924, 219.6631043460218393 ) ) ;
#75111 = CARTESIAN_POINT ( 'NONE',  ( -17.31663460169999880, 1423.877174748429979, 228.8047149553979978 ) ) ;
#75112 = CARTESIAN_POINT ( 'NONE',  ( -2.968355423891683387, 1512.111483631942974, 201.2327182046635983 ) ) ;
#75113 = CARTESIAN_POINT ( 'NONE',  ( 4.288117823509999482, 1445.747328214890103, 201.1375687007889894 ) ) ;
#75114 = CARTESIAN_POINT ( 'NONE',  ( -113.4000000000000057, 1320.102705746890251, 290.9564879300589837 ) ) ;
#75115 = CARTESIAN_POINT ( 'NONE',  ( 22.72745892751103369, 1509.726953286472281, 190.1320399485649375 ) ) ;
#75116 = CARTESIAN_POINT ( 'NONE',  ( -2.031588052790000098, 1454.893423854089860, 198.8069212169990010 ) ) ;
#75117 = CARTESIAN_POINT ( 'NONE',  ( 7.322105067625000352, 1516.572193931679976, 206.2485165713470110 ) ) ;
#75118 = CARTESIAN_POINT ( 'NONE',  ( -6.358210821802259716, 1484.708390028690019, 183.8747304888279928 ) ) ;
#75119 = ORIENTED_EDGE ( 'NONE', *, *, #69694, .F. ) ;
#75120 = DIRECTION ( 'NONE',  ( 0.000000000000000000, 0.000000000000000000, 1.000000000000000000 ) ) ;
#75121 = CARTESIAN_POINT ( 'NONE',  ( -4.244378810408340641, 1441.402155946249877, 162.0389632095809986 ) ) ;
#75123 = ORIENTED_EDGE ( 'NONE', *, *, #1753, .F. ) ;
#75122 = CARTESIAN_POINT ( 'NONE',  ( -68.63354038389999801, 1379.747798109390033, 280.2252688738590223 ) ) ;
#75124 = CARTESIAN_POINT ( 'NONE',  ( -17.86814680931840016, 1424.407636215880075, 228.2372741570307255 ) ) ;
#75125 = ORIENTED_EDGE ( 'NONE', *, *, #110155, .F. ) ;
#75126 = CARTESIAN_POINT ( 'NONE',  ( -16.25736646461311707, 1514.559393050436938, 223.9077632415501000 ) ) ;
#75127 = CARTESIAN_POINT ( 'NONE',  ( 11.78257430589999899, 1500.696465547190201, 207.7593786822990012 ) ) ;
#75129 = CARTESIAN_POINT ( 'NONE',  ( 15.81800194485040123, 1409.465360594919957, 192.8631252433119982 ) ) ;
#75128 = CARTESIAN_POINT ( 'NONE',  ( -10.81505178339999951, 1424.921174125060134, 144.1620446054460274 ) ) ;
#75130 = CARTESIAN_POINT ( 'NONE',  ( 1.136814033864999907, 1516.854133554269993, 211.4058994415870245 ) ) ;
#75131 = CARTESIAN_POINT ( 'NONE',  ( 38.16825441870970081, 1438.635335183450024, 136.6032594511559921 ) ) ;
#75132 = CIRCLE ( 'NONE', #107326, 1.000000000000000888 ) ;
#75133 = B_SPLINE_SURFACE_WITH_KNOTS ( 'NONE', 5, 1, ( 
 ( #66998, #49095 ),
 ( #23309, #6521 ),
 ( #40673, #32276 ),
 ( #109540, #49643 ),
 ( #74302, #65900 ),
 ( #90520, #82119 ) ),
 .UNSPECIFIED., .F., .F., .F.,
 ( 6, 6 ),
 ( 2, 2 ),
 ( 0.000000000000000000, 3.803024431209999889 ),
 ( 0.000000000000000000, 14.00000000000000000 ),
 .UNSPECIFIED. ) ;
#75134 = CARTESIAN_POINT ( 'NONE',  ( -106.8251098314479890, 1378.913060387289988, 306.9346524642279519 ) ) ;
#75135 = CARTESIAN_POINT ( 'NONE',  ( -1.507975160943080040, 1509.033140630240268, 179.3618957914489727 ) ) ;
#75136 = CARTESIAN_POINT ( 'NONE',  ( 8.727063097277033776, 1465.247437969211205, 232.8215983573240635 ) ) ;
#75137 = DIRECTION ( 'NONE',  ( 0.3081687959821757805, 0.7660444431188054848, 0.5640991972602825699 ) ) ;
#75138 = CARTESIAN_POINT ( 'NONE',  ( -12.53380499174499896, 1442.773887286369927, 169.4755105688890069 ) ) ;
#75139 = ORIENTED_EDGE ( 'NONE', *, *, #94937, .F. ) ;
#75140 = CARTESIAN_POINT ( 'NONE',  ( -19.58884347349999899, 1465.811382978989968, 204.1485388398990040 ) ) ;
#75141 = AXIS2_PLACEMENT_3D ( 'NONE', #81156, #89005, #61629 ) ;
#75142 = CARTESIAN_POINT ( 'NONE',  ( 3.629220049600000220, 1485.493215689190038, 199.0019176958990101 ) ) ;
#75143 = VERTEX_POINT ( 'NONE', #3546 ) ;
#75144 = ORIENTED_EDGE ( 'NONE', *, *, #56744, .T. ) ;
#75145 = DIRECTION ( 'NONE',  ( 0.000000000000000000, 0.000000000000000000, -1.000000000000000000 ) ) ;
#75146 = CARTESIAN_POINT ( 'NONE',  ( 10.56407631929999980, 1452.658139941989930, 209.7432180256290053 ) ) ;
#75147 = CARTESIAN_POINT ( 'NONE',  ( 0.03326171229690000342, 1452.996462166429865, 183.2389499340980024 ) ) ;
#75148 = CARTESIAN_POINT ( 'NONE',  ( -20.36206003818799815, 1507.989860361909905, 209.5068170956690210 ) ) ;
#75149 = CARTESIAN_POINT ( 'NONE',  ( -2.500000000000000000, 1439.384186984480039, 161.5055418259740065 ) ) ;
#75150 = CARTESIAN_POINT ( 'NONE',  ( -2.000000019065000245, 1517.051704408389924, 222.4523892994670007 ) ) ;
#75151 = B_SPLINE_CURVE_WITH_KNOTS ( 'NONE', 3,
 ( #13368, #4456, #49220, #56514, #29637, #39700, #21761, #99034, #73866, #55962, #21204, #30740, #15022 ),
 .UNSPECIFIED., .F., .F.,
 ( 4, 3, 3, 3, 4 ),
 ( -19.77813379760699775, -19.44850676187209970, -18.33858777542890195, -17.22488228015659928, -16.10949595319999972 ),
 .UNSPECIFIED. ) ;
#75152 = CARTESIAN_POINT ( 'NONE',  ( 11.76268527979999945, 1441.457099483779757, 188.0189021094980149 ) ) ;
#75153 = CARTESIAN_POINT ( 'NONE',  ( -14.35695723135263080, 1409.414416381394858, 225.2789668424194929 ) ) ;
#75154 = CARTESIAN_POINT ( 'NONE',  ( 6.541070334811199594, 1517.051704644130041, 212.7912326336579838 ) ) ;
#75155 = CARTESIAN_POINT ( 'NONE',  ( 25.00813785679999768, 1436.589730024439859, 137.9321018740980094 ) ) ;
#75156 = CARTESIAN_POINT ( 'NONE',  ( -11.92422106699999951, 1391.277242477369782, 212.8274739234090021 ) ) ;
#75157 = CARTESIAN_POINT ( 'NONE',  ( -84.36447712522229381, 1384.814979508860006, 288.1273280664730123 ) ) ;
#75158 = VERTEX_POINT ( 'NONE', #56122 ) ;
#75159 = CARTESIAN_POINT ( 'NONE',  ( -2.485217232065000115, 1516.534320418310244, 201.4128137944169907 ) ) ;
#75160 = CARTESIAN_POINT ( 'NONE',  ( 6.548200587644999793, 1516.632821972880038, 207.9912384682270101 ) ) ;
#75161 = ORIENTED_EDGE ( 'NONE', *, *, #9616, .F. ) ;
#75162 = CARTESIAN_POINT ( 'NONE',  ( 36.59185764445249589, 1440.913060387330006, 263.1072593421939700 ) ) ;
#75163 = CARTESIAN_POINT ( 'NONE',  ( -0.0007030488943480552033, 1451.930198993764179, 153.9960485520721534 ) ) ;
#75164 = VERTEX_POINT ( 'NONE', #96478 ) ;
#75165 = CARTESIAN_POINT ( 'NONE',  ( -13.28956057169999916, 1415.163755984229965, 220.9230430223980193 ) ) ;
#75166 = CARTESIAN_POINT ( 'NONE',  ( -11.50213147263169944, 1432.340329783160087, 151.2059272481280061 ) ) ;
#75167 = CARTESIAN_POINT ( 'NONE',  ( -17.45421023344330180, 1419.943788952030218, 205.7215592404089932 ) ) ;
#75168 = CARTESIAN_POINT ( 'NONE',  ( -9.903018300453069855, 1462.461387641800002, 206.7225876591880080 ) ) ;
#75169 = DIRECTION ( 'NONE',  ( -0.6736849260863841948, 0.000000000000000000, 0.7390186874254148774 ) ) ;
#75170 = CARTESIAN_POINT ( 'NONE',  ( 10.06269975749759915, 1469.306610116130059, 207.3997075874580105 ) ) ;
#75171 = CARTESIAN_POINT ( 'NONE',  ( -4.824413881312672459, 1468.483554383926275, 219.2781897695970201 ) ) ;
#75172 = CARTESIAN_POINT ( 'NONE',  ( 7.501852740990000434, 1494.251036354090274, 218.4424164909689807 ) ) ;
#75173 = CARTESIAN_POINT ( 'NONE',  ( 23.15595999055019760, 1424.857126420280110, 206.2044122327660034 ) ) ;
#75175 = FACE_OUTER_BOUND ( 'NONE', #109601, .T. ) ;
#75174 = CARTESIAN_POINT ( 'NONE',  ( 15.52105024970000002, 1459.722504423429882, 231.1950374654979896 ) ) ;
#75176 = CARTESIAN_POINT ( 'NONE',  ( -4.917407973280459643, 1422.446740859282954, 184.8124456577417334 ) ) ;
#75177 = B_SPLINE_SURFACE_WITH_KNOTS ( 'NONE', 5, 1, ( 
 ( #17798, #101814 ),
 ( #101251, #24550 ),
 ( #58738, #92877 ),
 ( #16154, #41936 ),
 ( #45269, #97296 ),
 ( #20031, #10539 ) ),
 .UNSPECIFIED., .F., .F., .F.,
 ( 6, 6 ),
 ( 2, 2 ),
 ( 0.000000000000000000, 3.199138346760000307 ),
 ( 0.000000000000000000, 14.00000000000000000 ),
 .UNSPECIFIED. ) ;
#75178 = CARTESIAN_POINT ( 'NONE',  ( 31.23437356469435144, 1512.187213306747481, 195.3468678195113739 ) ) ;
#75179 = ORIENTED_EDGE ( 'NONE', *, *, #104342, .F. ) ;
#75180 = DIRECTION ( 'NONE',  ( -1.836970198721029688E-16, -1.000000000000000000, 0.000000000000000000 ) ) ;
#75181 = CARTESIAN_POINT ( 'NONE',  ( -113.4000000000000057, 1391.913060387289988, 304.2218459572590064 ) ) ;
#75182 = CARTESIAN_POINT ( 'NONE',  ( 0.5608844116969206040, 1516.772451887518400, 216.8371137998956613 ) ) ;
#75183 = CARTESIAN_POINT ( 'NONE',  ( -7.324914956285000223, 1516.685667699390024, 213.7393364370070117 ) ) ;
#75184 = CARTESIAN_POINT ( 'NONE',  ( 3.586321559907979850, 1515.071394777460000, 213.2046241622850005 ) ) ;
#75185 = CARTESIAN_POINT ( 'NONE',  ( -11.12297507747387648, 1425.174378293636664, 138.4895836007016783 ) ) ;
#75187 = VERTEX_POINT ( 'NONE', #72394 ) ;
#75186 = CARTESIAN_POINT ( 'NONE',  ( -4.329448776040000446, 1515.064792882589927, 211.4519800877889963 ) ) ;
#75188 = CARTESIAN_POINT ( 'NONE',  ( -8.848479971949998912, 1384.899922694570023, 199.9247835823190087 ) ) ;
#75189 = AXIS2_PLACEMENT_3D ( 'NONE', #50787, #412, #34529 ) ;
#75190 = CYLINDRICAL_SURFACE ( 'NONE', #92495, 1.999999999999999556 ) ;
#75191 = CARTESIAN_POINT ( 'NONE',  ( -11.29090808720000005, 1431.527451484140101, 151.4782487668979911 ) ) ;
#75192 = CARTESIAN_POINT ( 'NONE',  ( -15.46336752740000087, 1415.677402202029953, 209.5779191499580065 ) ) ;
#75193 = FACE_OUTER_BOUND ( 'NONE', #91195, .T. ) ;
#75194 = CARTESIAN_POINT ( 'NONE',  ( -1.143529715360000064E-14, 1421.542806690330053, 144.1893924737979944 ) ) ;
#75195 = CARTESIAN_POINT ( 'NONE',  ( -5.460803535712269507, 1427.449714376620022, 201.5391232999229771 ) ) ;
#75196 = CARTESIAN_POINT ( 'NONE',  ( -2.500000000000000000, 1443.913060387330006, 150.6726614421979775 ) ) ;
#75198 = CARTESIAN_POINT ( 'NONE',  ( -11.86982405321400691, 1423.326458348926963, 137.0999999980979567 ) ) ;
#75197 = CARTESIAN_POINT ( 'NONE',  ( -25.84761762660000173, 1508.004946167130129, 217.5423480708579689 ) ) ;
#75199 = CARTESIAN_POINT ( 'NONE',  ( -1.831351330479999762, 1484.703635172929808, 182.8316381303979767 ) ) ;
#75200 = EDGE_LOOP ( 'NONE', ( #2347, #48986, #44635, #66751 ) ) ;
#75201 = CARTESIAN_POINT ( 'NONE',  ( -7.724732447025000504, 1517.133889586189980, 205.8614888033369823 ) ) ;
#75202 = CARTESIAN_POINT ( 'NONE',  ( 4.968383026439999739, 1406.259165937729904, 269.0361203054980024 ) ) ;
#75203 = DIRECTION ( 'NONE',  ( 0.000000000000000000, 0.000000000000000000, -1.000000000000000000 ) ) ;
#75204 = ADVANCED_FACE ( 'NONE', ( #88642 ), #102664, .F. ) ;
#75205 = CARTESIAN_POINT ( 'NONE',  ( 24.08566870183141262, 1435.968196123745429, 213.6274238454907106 ) ) ;
#75206 = CARTESIAN_POINT ( 'NONE',  ( 3.965334566925400761, 1454.048335879079787, 217.6203598810320159 ) ) ;
#75207 = CARTESIAN_POINT ( 'NONE',  ( -12.26364123840000175, 1375.886883438980021, 209.1218459572589836 ) ) ;
#75208 = DIRECTION ( 'NONE',  ( 1.000000000000000000, 0.000000000000000000, 0.000000000000000000 ) ) ;
#75209 = AXIS2_PLACEMENT_3D ( 'NONE', #38516, #19508, #30109 ) ;
#75210 = CARTESIAN_POINT ( 'NONE',  ( -15.08324830079999934, 1416.126940580989867, 205.9268786477289837 ) ) ;
#75211 = CARTESIAN_POINT ( 'NONE',  ( -12.96862445230000027, 1444.929287191270078, 186.6030988806980133 ) ) ;
#75212 = ADVANCED_FACE ( 'NONE', ( #91915 ), #57164, .T. ) ;
#75213 = CARTESIAN_POINT ( 'NONE',  ( -19.89217962195755263, 1485.003688521414915, 190.9128337503663317 ) ) ;
#75214 = B_SPLINE_SURFACE_WITH_KNOTS ( 'NONE', 5, 5, ( 
 ( #2408, #83468, #30317, #40925, #91879, #22438 ),
 ( #39273, #48244, #99158, #31974, #25622, #57760 ),
 ( #6763, #30866, #56087, #73446, #98622, #48804 ),
 ( #90213, #13497, #31417, #82387, #23566, #56639 ),
 ( #47687, #107580, #81815, #99711, #5117, #90774 ),
 ( #108683, #8823, #65042, #6218, #108122, #43008 ),
 ( #40370, #49343, #14617, #75103, #14056, #15152 ),
 ( #109251, #64505, #32535, #66706, #5686, #39830 ),
 ( #73992, #65599, #66165, #59814, #100815, #74550 ) ),
 .UNSPECIFIED., .F., .F., .F.,
 ( 6, 3, 6 ),
 ( 6, 6 ),
 ( 3.122008137489260093, 5.367142198119999819, 7.612276258760739545 ),
 ( -0.0004406524307360239786, 2.000000000000000000 ),
 .UNSPECIFIED. ) ;
#75215 = CARTESIAN_POINT ( 'NONE',  ( -16.21759533281229082, 1419.733967092127386, 209.9202815302434146 ) ) ;
#75216 = CARTESIAN_POINT ( 'NONE',  ( -5.294961033159999886, 1496.721944649390025, 219.0642768234689868 ) ) ;
#75217 = CARTESIAN_POINT ( 'NONE',  ( 0.01122475199670090046, 1477.924429480590106, 201.4578446915589893 ) ) ;
#75218 = CARTESIAN_POINT ( 'NONE',  ( -3.114882401780000087, 1426.979439823029907, 214.3676144197979738 ) ) ;
#75219 = CARTESIAN_POINT ( 'NONE',  ( 10.73498917976377243, 1424.972937926497934, 139.1354244534461202 ) ) ;
#75220 = DIRECTION ( 'NONE',  ( 0.000000000000000000, -1.000000000000000000, 0.000000000000000000 ) ) ;
#75221 = CARTESIAN_POINT ( 'NONE',  ( -1.764294607579999896, 1475.537171245129912, 269.2935847982979567 ) ) ;
#75222 = DIRECTION ( 'NONE',  ( -0.003573437736213522058, 0.9999913661844085366, -0.002120872317155135696 ) ) ;
#75223 = CARTESIAN_POINT ( 'NONE',  ( -14.72258237740398101, 1514.508948671113103, 192.8217237370948851 ) ) ;
#75224 = CARTESIAN_POINT ( 'NONE',  ( 17.17241001986483795, 1511.187213306747708, 179.6185504016043240 ) ) ;
#75225 = CARTESIAN_POINT ( 'NONE',  ( -43.38367995432890467, 1384.771901656779846, 248.3716437928619882 ) ) ;
#75226 = CARTESIAN_POINT ( 'NONE',  ( -30.98826378581289021, 1524.599984580802129, 221.8039704955955642 ) ) ;
#75227 = CIRCLE ( 'NONE', #53747, 1.999999999999998668 ) ;
#75228 = CARTESIAN_POINT ( 'NONE',  ( 11.48964235903519970, 1415.152886233159961, 222.8125005102990031 ) ) ;
#75229 = CARTESIAN_POINT ( 'NONE',  ( -107.7365696490000033, 1379.032352522900055, 299.3254846616590044 ) ) ;
#75230 = LINE ( 'NONE', #51677, #37588 ) ;
#75231 = CARTESIAN_POINT ( 'NONE',  ( -2.416613126592233485, 1507.334987533291041, 221.5267771657985918 ) ) ;
#75232 =( BOUNDED_CURVE ( )  B_SPLINE_CURVE ( 3, ( #38567, #72213, #55399, #13905 ),
 .UNSPECIFIED., .F., .F. ) 
 B_SPLINE_CURVE_WITH_KNOTS ( ( 4, 4 ),
 ( 2.354951096460577986, 3.925058729076146058 ),
 .UNSPECIFIED. ) 
 CURVE ( )  GEOMETRIC_REPRESENTATION_ITEM ( )  RATIONAL_B_SPLINE_CURVE ( ( 1.000000000000000000, 0.8049001529475701133, 0.8049001529475701133, 1.000000000000000000 ) ) 
 REPRESENTATION_ITEM ( '' )  );
#75233 = CARTESIAN_POINT ( 'NONE',  ( -22.51025611740000087, 1410.194216029730114, 203.9745233452079844 ) ) ;
#75234 = CARTESIAN_POINT ( 'NONE',  ( -10.42233989824366702, 1379.729316471301445, 202.4697405137477801 ) ) ;
#75235 = CARTESIAN_POINT ( 'NONE',  ( -15.64999484340200198, 1421.347476133591954, 227.1285184359570053 ) ) ;
#75236 = CARTESIAN_POINT ( 'NONE',  ( -35.67154068219999630, 1419.369011970829888, 269.2338164377980547 ) ) ;
#75237 = EDGE_LOOP ( 'NONE', ( #19239, #33870, #39496, #103773 ) ) ;
#75238 = CARTESIAN_POINT ( 'NONE',  ( -5.371346839175000554, 1520.551704408390151, 218.7599618298069970 ) ) ;
#75239 = CARTESIAN_POINT ( 'NONE',  ( 20.31210344360099995, 1432.638797527460156, 214.7986899441419837 ) ) ;
#75240 = CARTESIAN_POINT ( 'NONE',  ( -7.519244436443294433, 1510.642476678762705, 215.0516229487886335 ) ) ;
#75241 = CARTESIAN_POINT ( 'NONE',  ( 20.33509335567159937, 1432.834523802549938, 214.7556744266179862 ) ) ;
#75244 = CARTESIAN_POINT ( 'NONE',  ( -13.47873387835659997, 1379.610484773819962, 211.5873092184639859 ) ) ;
#75243 = VECTOR ( 'NONE', #69618, 1000.000000000000114 ) ;
#75242 = CARTESIAN_POINT ( 'NONE',  ( 10.77813231690000073, 1424.944499019330124, 141.8424095806979892 ) ) ;
#75245 = CARTESIAN_POINT ( 'NONE',  ( 17.36692773919801169, 1525.425665131968344, 237.0071470213579232 ) ) ;
#75246 = CARTESIAN_POINT ( 'NONE',  ( -6.541070373676360461, 1517.051704644259871, 205.4524592699869743 ) ) ;
#75247 = CARTESIAN_POINT ( 'NONE',  ( -17.71193101166619854, 1517.051704408389924, 221.5709757775249784 ) ) ;
#75248 = CARTESIAN_POINT ( 'NONE',  ( -11.17472318950760979, 1414.941152333697573, 196.0144180821544353 ) ) ;
#75249 = AXIS2_PLACEMENT_3D ( 'NONE', #105202, #97338, #20076 ) ;
#75250 = CARTESIAN_POINT ( 'NONE',  ( 4.612507273904999039, 1516.886345593249871, 204.1123678647870179 ) ) ;
#75251 = LINE ( 'NONE', #86800, #26723 ) ;
#75252 = CARTESIAN_POINT ( 'NONE',  ( -8.792429487396887566, 1398.173735791722265, 199.4398815334327537 ) ) ;
#75253 = CARTESIAN_POINT ( 'NONE',  ( 16.57141199633499795, 1514.216506490359961, 194.7449369304669915 ) ) ;
#75254 = CARTESIAN_POINT ( 'NONE',  ( -16.34717785500199838, 1420.685724369499894, 203.2930982450899933 ) ) ;
#75255 = CARTESIAN_POINT ( 'NONE',  ( -24.56185491079999750, 1376.959776039820099, 215.3443103757190329 ) ) ;
#75256 = CARTESIAN_POINT ( 'NONE',  ( 2.742048936847579998, 1367.348608298013232, 208.3718459617061285 ) ) ;
#75258 = VERTEX_POINT ( 'NONE', #58880 ) ;
#75257 = CARTESIAN_POINT ( 'NONE',  ( -29.83023120264250139, 1379.643204280620012, 217.9872659232200078 ) ) ;
#75259 = ORIENTED_EDGE ( 'NONE', *, *, #13323, .F. ) ;
#75260 = CARTESIAN_POINT ( 'NONE',  ( 11.97071048005270022, 1433.593009549930002, 149.8699161731940137 ) ) ;
#75261 = CARTESIAN_POINT ( 'NONE',  ( -10.12349441079999934, 1396.444906704929735, 216.2323542477279830 ) ) ;
#75262 = CARTESIAN_POINT ( 'NONE',  ( -21.78276643210000074, 1409.837828932429829, 213.4025661265980034 ) ) ;
#75263 = ORIENTED_EDGE ( 'NONE', *, *, #51030, .T. ) ;
#75264 = CARTESIAN_POINT ( 'NONE',  ( -13.50816072687143610, 1444.048915240285851, 169.3527851728482005 ) ) ;
#75265 = CARTESIAN_POINT ( 'NONE',  ( 21.68893548844135921, 1509.708255528440077, 229.4365290369073875 ) ) ;
#75266 = DIRECTION ( 'NONE',  ( -0.000000000000000000, -1.000000000000000000, -0.000000000000000000 ) ) ;
#75268 = CARTESIAN_POINT ( 'NONE',  ( -14.01968694497010048, 1509.108030625119909, 183.6010202189160054 ) ) ;
#75267 = CARTESIAN_POINT ( 'NONE',  ( 2.593334035529999859, 1445.992680618890063, 199.3398764938089869 ) ) ;
#75269 =( BOUNDED_CURVE ( )  B_SPLINE_CURVE ( 3, ( #27302, #1023, #10505, #12154 ),
 .UNSPECIFIED., .F., .T. ) 
 B_SPLINE_CURVE_WITH_KNOTS ( ( 4, 4 ),
 ( 2.650173097296665059, 3.567460430156555340 ),
 .UNSPECIFIED. ) 
 CURVE ( )  GEOMETRIC_REPRESENTATION_ITEM ( )  RATIONAL_B_SPLINE_CURVE ( ( 1.000000000000000000, 0.9311025432363498888, 0.9311025432363498888, 1.000000000000000000 ) ) 
 REPRESENTATION_ITEM ( '' )  );
#75270 = AXIS2_PLACEMENT_3D ( 'NONE', #79061, #104791, #2366 ) ;
#75271 = CARTESIAN_POINT ( 'NONE',  ( 0.7226347908460000191, 1449.242467270309817, 183.4668519528979971 ) ) ;
#75272 = CARTESIAN_POINT ( 'NONE',  ( -4.161829183451589920, 1463.201391561070068, 200.2643698894640067 ) ) ;
#75273 = CARTESIAN_POINT ( 'NONE',  ( -28.84709929359999947, 1507.919204203629988, 212.2396942135479776 ) ) ;
#75274 = CARTESIAN_POINT ( 'NONE',  ( 10.81179928114259958, 1396.290616737959908, 211.5056212398530135 ) ) ;
#75275 = CARTESIAN_POINT ( 'NONE',  ( 1.052431931509999918, 1415.163755984130148, 191.3800010946980024 ) ) ;
#75276 = CARTESIAN_POINT ( 'NONE',  ( 10.95104177029999981, 1431.009226238560132, 151.6519986001979987 ) ) ;
#75277 = CARTESIAN_POINT ( 'NONE',  ( 7.368183369116096060, 1509.171485936123418, 180.6959945992290670 ) ) ;
#75278 = ORIENTED_EDGE ( 'NONE', *, *, #65365, .F. ) ;
#75279 = CARTESIAN_POINT ( 'NONE',  ( 13.45926565268829833, 1434.961840340200069, 149.1575143944549779 ) ) ;
#75280 = VERTEX_POINT ( 'NONE', #1745 ) ;
#75281 = ORIENTED_EDGE ( 'NONE', *, *, #86512, .F. ) ;
#75282 = B_SPLINE_CURVE_WITH_KNOTS ( 'NONE', 5,
 ( #39665, #63781, #73833, #40211, #107960, #31257 ),
 .UNSPECIFIED., .F., .F.,
 ( 6, 6 ),
 ( -26.18269281474930210, -9.354787281509999275 ),
 .UNSPECIFIED. ) ;
#75283 = CARTESIAN_POINT ( 'NONE',  ( 3.669386717837979983, 1517.051704638620095, 202.5807756278150009 ) ) ;
#75284 = CARTESIAN_POINT ( 'NONE',  ( -11.28279764400000040, 1462.173053641429988, 233.6667625336980052 ) ) ;
#75285 = CARTESIAN_POINT ( 'NONE',  ( -107.9413468032178116, 1389.158540163861062, 309.9172676812428904 ) ) ;
#75286 = CARTESIAN_POINT ( 'NONE',  ( -2.870951705914999597, 1517.111322026010157, 215.6844817927369888 ) ) ;
#75287 = CARTESIAN_POINT ( 'NONE',  ( -7.953531051250857686, 1511.798535855328510, 212.3375516263953386 ) ) ;
#75288 = ORIENTED_EDGE ( 'NONE', *, *, #72062, .T. ) ;
#75289 = CARTESIAN_POINT ( 'NONE',  ( -12.35076168520000017, 1502.691457114289960, 208.7665132982610032 ) ) ;
#75290 = CARTESIAN_POINT ( 'NONE',  ( -1.802000870929999943, 1412.180318182730161, 185.9687240695979824 ) ) ;
#75291 = CARTESIAN_POINT ( 'NONE',  ( -7.592224575760000427, 1375.673697770030230, 207.5503173039290061 ) ) ;
#75292 = ADVANCED_FACE ( 'NONE', ( #68954 ), #105468, .T. ) ;
#75293 = ORIENTED_EDGE ( 'NONE', *, *, #41460, .T. ) ;
#75294 = CARTESIAN_POINT ( 'NONE',  ( -4.624099329465000352, 1516.962555622980062, 205.8665050058069994 ) ) ;
#75295 = ORIENTED_EDGE ( 'NONE', *, *, #95175, .T. ) ;
#75296 = CARTESIAN_POINT ( 'NONE',  ( -1.709766532154999963, 1516.959716008189844, 209.1345041580460133 ) ) ;
#75297 = CARTESIAN_POINT ( 'NONE',  ( -20.16473732820000109, 1508.103700725129784, 228.9069202426980212 ) ) ;
#75298 = EDGE_CURVE ( 'NONE', #40736, #23656, #36968, .T. ) ;
#75300 = EDGE_CURVE ( 'NONE', #27470, #110516, #50800, .T. ) ;
#75299 = CARTESIAN_POINT ( 'NONE',  ( -4.377978033840000727, 1409.571113459229991, 187.0373285412979953 ) ) ;
#75301 = CARTESIAN_POINT ( 'NONE',  ( 6.160280177405000224, 1511.773927532309926, 217.7619188583669825 ) ) ;
#75303 = ORIENTED_EDGE ( 'NONE', *, *, #44047, .T. ) ;
#75302 = CARTESIAN_POINT ( 'NONE',  ( -0.4156091144146349947, 1414.971513442450032, 225.9103026676290256 ) ) ;
#75304 = CARTESIAN_POINT ( 'NONE',  ( 19.28571478079999935, 1426.671932083830143, 223.6657923338979970 ) ) ;
#75305 = DIRECTION ( 'NONE',  ( 0.9455185755993178454, 0.000000000000000000, -0.3255681544571537578 ) ) ;
#75306 = CARTESIAN_POINT ( 'NONE',  ( -76.11462884880000956, 1384.355091197029878, 301.2025005888589817 ) ) ;
#75307 = CARTESIAN_POINT ( 'NONE',  ( -0.1360178087611779996, 1465.118855296690072, 238.1340914064880110 ) ) ;
#75308 = CARTESIAN_POINT ( 'NONE',  ( 7.287605107886430567, 1410.487174745140010, 269.8696506321609832 ) ) ;
#75310 = CARTESIAN_POINT ( 'NONE',  ( -6.937338783705000012, 1516.706638732659940, 213.7399656364970042 ) ) ;
#75309 = CIRCLE ( 'NONE', #109267, 1.999999999999999556 ) ;
#75311 = CARTESIAN_POINT ( 'NONE',  ( 23.58142271390000033, 1409.993431820429805, 209.1798619000200290 ) ) ;
#75312 = DIRECTION ( 'NONE',  ( 0.03489949670250207941, -0.9993908270190957621, 0.000000000000000000 ) ) ;
#75313 = CARTESIAN_POINT ( 'NONE',  ( -9.052499326103495392, 1423.899425168531707, 139.1406965814004764 ) ) ;
#75314 = CARTESIAN_POINT ( 'NONE',  ( 7.507423012266849938, 1508.880864730590019, 215.2619739013699984 ) ) ;
#75315 = CARTESIAN_POINT ( 'NONE',  ( 2.881325373965000214, 1517.003078582959688, 210.2407492406470055 ) ) ;
#75316 = CARTESIAN_POINT ( 'NONE',  ( 6.661338147749999709E-15, 1409.413060387330006, 271.1218459616979999 ) ) ;
#75317 = CARTESIAN_POINT ( 'NONE',  ( 0.1095215363050000001, 1420.452175220630124, 183.3292552232980199 ) ) ;
#75318 = AXIS2_PLACEMENT_3D ( 'NONE', #65668, #38788, #65119 ) ;
#75319 = CARTESIAN_POINT ( 'NONE',  ( 10.97434689771020011, 1432.635640446739899, 151.7699405381439988 ) ) ;
#75321 = ORIENTED_EDGE ( 'NONE', *, *, #59024, .T. ) ;
#75320 = CARTESIAN_POINT ( 'NONE',  ( -54.13887208369999371, 1385.096747890979941, 270.3642349231589606 ) ) ;
#75322 = CARTESIAN_POINT ( 'NONE',  ( -48.32414939222230288, 1385.132224470989740, 258.2732643174430223 ) ) ;
#75323 = CARTESIAN_POINT ( 'NONE',  ( 21.01925983530000153, 1472.811094121630049, 267.0604550193979776 ) ) ;
#75324 = DIRECTION ( 'NONE',  ( 0.000000000000000000, 0.000000000000000000, 1.000000000000000000 ) ) ;
#75325 = AXIS2_PLACEMENT_3D ( 'NONE', #40613, #84804, #92660 ) ;
#75326 = CARTESIAN_POINT ( 'NONE',  ( -2.256759385399999651, 1417.436677706029968, 235.4758680199980176 ) ) ;
#75327 = CARTESIAN_POINT ( 'NONE',  ( -2.502335351479658687, 1409.000443863340479, 194.1336473601319028 ) ) ;
#75328 = CARTESIAN_POINT ( 'NONE',  ( -22.76291043979999884, 1450.494225485409743, 218.6578027092980108 ) ) ;
#75329 = CARTESIAN_POINT ( 'NONE',  ( 1.442588533962650077, 1452.743361456999992, 183.4687140882980145 ) ) ;
#75330 = CIRCLE ( 'NONE', #102148, 7.999657266239995401 ) ;
#75332 = CARTESIAN_POINT ( 'NONE',  ( 9.196349486490202452, 1517.151704408390060, 214.4668224883511698 ) ) ;
#75331 = CARTESIAN_POINT ( 'NONE',  ( 2.291047489114999891, 1516.524310051880093, 216.8306159772470210 ) ) ;
#75333 = CARTESIAN_POINT ( 'NONE',  ( -113.4000000000000057, 1384.899971913130003, 304.2218459572590064 ) ) ;
#75334 = CARTESIAN_POINT ( 'NONE',  ( 1.842962231260000028, 1515.551704408389924, 205.2922258481490303 ) ) ;
#75335 = ORIENTED_EDGE ( 'NONE', *, *, #77509, .T. ) ;
#75336 = CARTESIAN_POINT ( 'NONE',  ( 5.002593359325000044, 1516.960844870249957, 202.5626772953570196 ) ) ;
#75337 = CARTESIAN_POINT ( 'NONE',  ( -15.64724543236500232, 1513.113451381389950, 223.4053766886669905 ) ) ;
#75338 = CARTESIAN_POINT ( 'NONE',  ( 29.22958591949999985, 1509.933780019529877, 206.4713313151879959 ) ) ;
#75339 = CARTESIAN_POINT ( 'NONE',  ( 23.25962669879999822, 1449.876265820790195, 217.4989437420879881 ) ) ;
#75340 = CARTESIAN_POINT ( 'NONE',  ( 8.737553414955298692, 1437.268927995063223, 153.2801379038078267 ) ) ;
#75341 = CARTESIAN_POINT ( 'NONE',  ( -3.179033946939999744, 1457.997354113189886, 219.3203918502989893 ) ) ;
#75342 = CARTESIAN_POINT ( 'NONE',  ( -0.8729764147290010046, 1444.456550671890000, 218.0453103216389934 ) ) ;
#75343 = CARTESIAN_POINT ( 'NONE',  ( 15.59609131893944145, 1421.004437767239551, 227.6468209294606027 ) ) ;
#75344 = TOROIDAL_SURFACE ( 'NONE', #9231, 1.000000000000000000, 1.000000000000000000 ) ;
#75345 = CARTESIAN_POINT ( 'NONE',  ( 29.70843182346579781, 1435.695031758189998, 136.0745602649149930 ) ) ;
#75346 = DIRECTION ( 'NONE',  ( -0.6736849260863841948, 0.000000000000000000, 0.7390186874254148774 ) ) ;
#75347 = CARTESIAN_POINT ( 'NONE',  ( -21.38922153579999730, 1429.213524300029803, 219.6571118298979854 ) ) ;
#75348 = CARTESIAN_POINT ( 'NONE',  ( -40.78917446724263840, 1456.261474242062377, 269.1081404453464074 ) ) ;
#75349 = CARTESIAN_POINT ( 'NONE',  ( -1.540849967930000064, 1430.630043029990020, 200.7745420285490070 ) ) ;
#75350 = CARTESIAN_POINT ( 'NONE',  ( -16.16168812540000133, 1413.305022623530022, 226.8025051581979881 ) ) ;
#75351 = CARTESIAN_POINT ( 'NONE',  ( 18.98249322451690446, 1526.382868172864164, 185.2725498412042953 ) ) ;
#75352 = AXIS2_PLACEMENT_3D ( 'NONE', #53750, #2782, #36902 ) ;
#75353 = CARTESIAN_POINT ( 'NONE',  ( -36.74716693956014524, 1455.731669175984734, 269.5566863843520764 ) ) ;
#75354 = ORIENTED_EDGE ( 'NONE', *, *, #39428, .F. ) ;
#75355 = CARTESIAN_POINT ( 'NONE',  ( -8.106555239546928249, 1438.741219031890068, 205.9368975051609993 ) ) ;
#75356 = DIRECTION ( 'NONE',  ( -1.755985294532469921E-16, 1.000000000000000000, -1.338183447452831989E-16 ) ) ;
#75357 = DIRECTION ( 'NONE',  ( 1.755985294532464991E-16, -1.000000000000000000, 1.338183447452830017E-16 ) ) ;
#75358 = CARTESIAN_POINT ( 'NONE',  ( 9.966104638080198086, 1428.054312288505116, 211.9051864186514820 ) ) ;
#75359 = CARTESIAN_POINT ( 'NONE',  ( -22.03465957474533354, 1512.187213306747481, 235.4136513321633117 ) ) ;
#75360 = CARTESIAN_POINT ( 'NONE',  ( -12.81686556575074754, 1444.973820179284985, 186.0349837055798901 ) ) ;
#75361 = CARTESIAN_POINT ( 'NONE',  ( -16.66231036550740541, 1523.604703353109699, 180.4882076302515372 ) ) ;
#75362 = CARTESIAN_POINT ( 'NONE',  ( 16.49514809540576366, 1525.343727714918259, 181.2134271599560691 ) ) ;
#75363 = AXIS2_PLACEMENT_3D ( 'NONE', #69955, #103510, #1087 ) ;
#75364 = DIRECTION ( 'NONE',  ( 0.000000000000000000, -1.000000000000000000, 0.000000000000000000 ) ) ;
#75365 = CARTESIAN_POINT ( 'NONE',  ( -14.06542466742875241, 1451.183651944110807, 150.3012616716959542 ) ) ;
#75366 = CARTESIAN_POINT ( 'NONE',  ( 25.19391193610000101, 1436.451707861340083, 137.5385279504980076 ) ) ;
#75367 = CARTESIAN_POINT ( 'NONE',  ( -12.74333518134357135, 1442.824178483951528, 169.4555743853381102 ) ) ;
#75369 = ORIENTED_EDGE ( 'NONE', *, *, #50873, .F. ) ;
#75368 = CARTESIAN_POINT ( 'NONE',  ( -14.29519668260000032, 1410.788278260029983, 226.8469779139979892 ) ) ;
#75370 = CARTESIAN_POINT ( 'NONE',  ( 0.02268235321126050100, 1415.088136167450102, 192.1344077303680251 ) ) ;
#75371 = CARTESIAN_POINT ( 'NONE',  ( 21.03123203779729877, 1507.789098030329797, 226.0655639048319756 ) ) ;
#75372 = ORIENTED_EDGE ( 'NONE', *, *, #48382, .F. ) ;
#75373 = ORIENTED_EDGE ( 'NONE', *, *, #100810, .F. ) ;
#75374 = CARTESIAN_POINT ( 'NONE',  ( -11.44024737950000059, 1501.432054422089777, 208.7106195065049974 ) ) ;
#75375 = CARTESIAN_POINT ( 'NONE',  ( -18.98249322453838417, 1526.382868172864164, 232.9711420821614070 ) ) ;
#75377 = CARTESIAN_POINT ( 'NONE',  ( -28.01911545579999796, 1440.913060392269927, 231.7019063163980093 ) ) ;
#75376 = CARTESIAN_POINT ( 'NONE',  ( 4.788126387470001077, 1455.785790442590041, 218.6153184129890121 ) ) ;
#75378 = CARTESIAN_POINT ( 'NONE',  ( -4.819998716129999750, 1445.927381020789880, 216.9237746421490272 ) ) ;
#75379 = CARTESIAN_POINT ( 'NONE',  ( -11.25532750870000065, 1433.153001996420016, 151.5352189930979989 ) ) ;
#75380 = EDGE_CURVE ( 'NONE', #18861, #30773, #101870, .T. ) ;
#75381 = CARTESIAN_POINT ( 'NONE',  ( -50.14839348009999753, 1380.010081756269983, 242.5009839091590038 ) ) ;
#75382 = LINE ( 'NONE', #13228, #85780 ) ;
#75383 = EDGE_CURVE ( 'NONE', #48151, #39586, #63310, .T. ) ;
#75384 = CARTESIAN_POINT ( 'NONE',  ( -2.686147501205254695, 1526.329757971589288, 241.8500438829907466 ) ) ;
#75385 = CARTESIAN_POINT ( 'NONE',  ( -24.38798815950000076, 1440.053814498560087, 212.0105281139480269 ) ) ;
#75386 = FACE_BOUND ( 'NONE', #103678, .T. ) ;
#75387 = STYLED_ITEM ( 'NONE', ( #48417 ), #19969 ) ;
#75388 = CARTESIAN_POINT ( 'NONE',  ( 8.476942927312379084, 1362.523913559699849, 210.6218459616987957 ) ) ;
#75389 = CARTESIAN_POINT ( 'NONE',  ( -28.89012903238323204, 1510.032946564538861, 217.2102799419582482 ) ) ;
#75391 = ORIENTED_EDGE ( 'NONE', *, *, #93122, .T. ) ;
#75390 = CARTESIAN_POINT ( 'NONE',  ( -9.230644300605730931E-10, 1416.774826112419987, 237.8701337189920082 ) ) ;
#75392 = EDGE_LOOP ( 'NONE', ( #44616, #41220, #32461, #55267, #10646 ) ) ;
#75393 = CARTESIAN_POINT ( 'NONE',  ( -11.84606637905420001, 1430.951851344180113, 149.8078499364760034 ) ) ;
#75394 = CARTESIAN_POINT ( 'NONE',  ( 19.46449505960000081, 1499.405048825090034, 221.7536591926989900 ) ) ;
#75395 = CARTESIAN_POINT ( 'NONE',  ( -7.559855553260000249, 1473.430876107429867, 270.2818740090979759 ) ) ;
#75396 = CARTESIAN_POINT ( 'NONE',  ( 12.45662817246929954, 1427.088122696140090, 206.6493147128259977 ) ) ;
#75398 = AXIS2_PLACEMENT_3D ( 'NONE', #61668, #26372, #79561 ) ;
#75397 = CARTESIAN_POINT ( 'NONE',  ( -107.9538559484733327, 1348.229899472569059, 307.1970880126511929 ) ) ;
#75399 = CARTESIAN_POINT ( 'NONE',  ( -14.65275159090117185, 1420.238444720549978, 213.8660283808354166 ) ) ;
#75400 = B_SPLINE_CURVE_WITH_KNOTS ( 'NONE', 3,
 ( #8303, #94513, #50878, #16142, #495, #43036, #34620, #76623, #16681, #69916, #59299, #101802, #42465, #110775, #76080, #68258, #26204, #104028, #102906, #26771 ),
 .UNSPECIFIED., .F., .F.,
 ( 4, 2, 2, 2, 1, 1, 1, 1, 2, 2, 2, 4 ),
 ( 0.000000000000000000, 0.2499999999997821742, 0.3749999999996731503, 0.4374999999996273536, 0.4687499999995982658, 0.4843749999995810573, 0.4921874999995723976, 0.4960937499995769495, 0.4980468749995792810, 0.4999999999995815569, 0.7499999999997908340, 1.000000000000000000 ),
 .UNSPECIFIED. ) ;
#75401 = CARTESIAN_POINT ( 'NONE',  ( 1.961418762360136681, 1526.143142182266047, 240.4212258933422675 ) ) ;
#75402 = CARTESIAN_POINT ( 'NONE',  ( 18.94015090468417739, 1456.918315522688317, 229.2628234610467359 ) ) ;
#75403 = DIRECTION ( 'NONE',  ( 0.000000000000000000, 1.000000000000000000, 0.000000000000000000 ) ) ;
#75404 = CARTESIAN_POINT ( 'NONE',  ( -20.65321958619999876, 1453.313060387329870, 208.1452065820600126 ) ) ;
#75405 = CARTESIAN_POINT ( 'NONE',  ( 10.95713404883475306, 1364.300541727352993, 207.6218459616987673 ) ) ;
#75406 = CARTESIAN_POINT ( 'NONE',  ( -12.08748390050469901, 1407.204040152260177, 266.9029471222330017 ) ) ;
#75407 = ORIENTED_EDGE ( 'NONE', *, *, #43441, .F. ) ;
#75408 = CARTESIAN_POINT ( 'NONE',  ( -4.327308595631589760, 1515.146523075020013, 209.5795434418390073 ) ) ;
#75409 = VERTEX_POINT ( 'NONE', #71728 ) ;
#75410 = VERTEX_POINT ( 'NONE', #96333 ) ;
#75411 = CARTESIAN_POINT ( 'NONE',  ( 7.338411959395000572, 1517.170512887980067, 211.6064236274570192 ) ) ;
#75412 = CIRCLE ( 'NONE', #70075, 1.999999999999999556 ) ;
#75413 = CARTESIAN_POINT ( 'NONE',  ( 4.919706779345196956, 1422.462138335776672, 184.3625360145741467 ) ) ;
#75414 = CARTESIAN_POINT ( 'NONE',  ( 5.169811769132760304, 1424.207592462389812, 193.2980118299309993 ) ) ;
#75415 = EDGE_CURVE ( 'NONE', #10931, #23627, #26764, .T. ) ;
#75417 = CARTESIAN_POINT ( 'NONE',  ( 2.175409717514719593E-31, 1397.551704408390151, 209.1218459616989946 ) ) ;
#75416 = CARTESIAN_POINT ( 'NONE',  ( 2.879642153204999833, 1516.812046502680005, 212.5681757458869754 ) ) ;
#75418 = CARTESIAN_POINT ( 'NONE',  ( -16.16311898949999915, 1470.468432338930143, 188.4789380148980058 ) ) ;
#75419 = CARTESIAN_POINT ( 'NONE',  ( -16.56024668282710266, 1489.054572897799972, 229.4033101248429887 ) ) ;
#75420 = ORIENTED_EDGE ( 'NONE', *, *, #101505, .T. ) ;
#75421 = CARTESIAN_POINT ( 'NONE',  ( -101.9210842609999901, 1379.177752269670009, 302.4435101425590346 ) ) ;
#75422 = ADVANCED_FACE ( 'NONE', ( #80077 ), #2652, .F. ) ;
#75423 = EDGE_CURVE ( 'NONE', #108598, #94471, #101352, .T. ) ;
#75424 = CARTESIAN_POINT ( 'NONE',  ( 3.258474578945000033, 1517.083030555940013, 202.5598499717069956 ) ) ;
#75425 = CIRCLE ( 'NONE', #50331, 2.000000000000001776 ) ;
#75426 = CARTESIAN_POINT ( 'NONE',  ( -0.5805478587719999917, 1457.956445075529928, 229.5817085818979990 ) ) ;
#75427 = EDGE_CURVE ( 'NONE', #103585, #98527, #73291, .T. ) ;
#75428 = CARTESIAN_POINT ( 'NONE',  ( -47.39586428316670208, 1384.608660850170054, 221.4693795585880025 ) ) ;
#75429 = CARTESIAN_POINT ( 'NONE',  ( -44.70567387637289869, 1440.913053093850067, 269.9105629710239782 ) ) ;
#75430 = CARTESIAN_POINT ( 'NONE',  ( -16.66936639845670598, 1523.382868172864164, 180.4828114240741570 ) ) ;
#75432 = ORIENTED_EDGE ( 'NONE', *, *, #16752, .F. ) ;
#75431 = CARTESIAN_POINT ( 'NONE',  ( -4.500000000000000000, 1425.929641636930000, 184.1455913746980002 ) ) ;
#75433 = CARTESIAN_POINT ( 'NONE',  ( 0.5697987610180000884, 1450.893162576140185, 181.2939918234980041 ) ) ;
#75434 = DIRECTION ( 'NONE',  ( -0.5030436214085368674, 0.000000000000000000, 0.8642610224695920218 ) ) ;
#75435 = EDGE_CURVE ( 'NONE', #13274, #42640, #100050, .T. ) ;
#75436 = DIRECTION ( 'NONE',  ( 0.9995237709234254808, 0.03085824620771311644, 1.984177796020841428E-13 ) ) ;
#75437 = CARTESIAN_POINT ( 'NONE',  ( -12.87169627017330065, 1435.949072046520087, 150.7991738863709941 ) ) ;
#75438 = CARTESIAN_POINT ( 'NONE',  ( -24.36381069329999960, 1441.240813755360023, 211.7027932903779970 ) ) ;
#75439 = CARTESIAN_POINT ( 'NONE',  ( -2.282301616165000269, 1516.836638729160086, 210.8392784184970026 ) ) ;
#75440 = CONICAL_SURFACE ( 'NONE', #21753, 12.50000000000000000, 0.02617993877989872875 ) ;
#75441 = CARTESIAN_POINT ( 'NONE',  ( -68.74147317429999759, 1379.748081684489989, 280.1371050876589948 ) ) ;
#75442 = CARTESIAN_POINT ( 'NONE',  ( -0.1414919709576896445, 1452.990816532969802, 183.2406312904289223 ) ) ;
#75443 = CARTESIAN_POINT ( 'NONE',  ( 6.754813038153810290, 1440.797395171449807, 214.9116427326270014 ) ) ;
#75444 = CARTESIAN_POINT ( 'NONE',  ( 3.203920217234287993, 1440.606318824109167, 157.0470840658564100 ) ) ;
#75445 = CARTESIAN_POINT ( 'NONE',  ( 2.863787855735000054, 1516.788317650260069, 207.4054531903269947 ) ) ;
#75446 = ORIENTED_EDGE ( 'NONE', *, *, #89780, .F. ) ;
#75447 = CARTESIAN_POINT ( 'NONE',  ( -2.244421813216840089, 1451.951705408559974, 184.5463975505989822 ) ) ;
#75449 = EDGE_CURVE ( 'NONE', #72812, #74476, #103658, .T. ) ;
#75448 = CARTESIAN_POINT ( 'NONE',  ( -9.119231684200059362, 1439.059512825920137, 208.3665791233769937 ) ) ;
#75450 = VECTOR ( 'NONE', #89566, 1000.000000000000000 ) ;
#75451 = CARTESIAN_POINT ( 'NONE',  ( -19.40858652965227904, 1457.338511877794417, 226.2137482204685455 ) ) ;
#75452 = VERTEX_POINT ( 'NONE', #60266 ) ;
#75453 = CARTESIAN_POINT ( 'NONE',  ( 20.22421167039999901, 1476.021596313489908, 210.1180608805510133 ) ) ;
#75454 = CARTESIAN_POINT ( 'NONE',  ( 13.04232454877760006, 1435.170642384910252, 150.2281921783049938 ) ) ;
#75455 = CARTESIAN_POINT ( 'NONE',  ( 12.33253873727779926, 1469.000856890969999, 231.6620758685679959 ) ) ;
#75456 = EDGE_CURVE ( 'NONE', #106669, #31574, #24975, .T. ) ;
#75457 = CARTESIAN_POINT ( 'NONE',  ( -4.251676037229999316, 1413.133656259280087, 207.7220070843589781 ) ) ;
#75458 = CARTESIAN_POINT ( 'NONE',  ( 12.37159932449999822, 1415.628674266529742, 222.5813136582980007 ) ) ;
#75459 = CARTESIAN_POINT ( 'NONE',  ( 9.904447724410001541, 1489.619655155790042, 203.3666065851589906 ) ) ;
#75460 = EDGE_CURVE ( 'NONE', #97581, #45814, #1777, .T. ) ;
#75461 = CARTESIAN_POINT ( 'NONE',  ( 4.210705291133630013, 1430.371004163770067, 217.6270284791030178 ) ) ;
#75462 = CARTESIAN_POINT ( 'NONE',  ( 4.221456909779160327, 1441.605107385089923, 169.1511311007560039 ) ) ;
#75464 = CARTESIAN_POINT ( 'NONE',  ( -11.97827956719999776, 1441.604408666619975, 150.7817505876979851 ) ) ;
#75463 = CARTESIAN_POINT ( 'NONE',  ( 5.784008635194999748, 1516.911981270829983, 214.1231845985469988 ) ) ;
#75465 = DIRECTION ( 'NONE',  ( 0.000000000000000000, -1.000000000000000000, 2.084285079594309782E-16 ) ) ;
#75466 = CARTESIAN_POINT ( 'NONE',  ( 5.780232077335000440, 1516.760434454289907, 216.4486414936069991 ) ) ;
#75467 = EDGE_LOOP ( 'NONE', ( #58730, #4740, #97259, #97390 ) ) ;
#75468 = CARTESIAN_POINT ( 'NONE',  ( -10.78869841497320081, 1414.913060387399810, 196.3854094717209762 ) ) ;
#75469 = CARTESIAN_POINT ( 'NONE',  ( 15.75929536665272224, 1409.463372041439243, 192.9545506605122114 ) ) ;
#75470 = EDGE_CURVE ( 'NONE', #7502, #41641, #15939, .T. ) ;
#75471 = FACE_OUTER_BOUND ( 'NONE', #85959, .T. ) ;
#75472 = CARTESIAN_POINT ( 'NONE',  ( -22.69876404240057965, 1501.977400791986611, 236.8953202675781426 ) ) ;
#75473 = DIRECTION ( 'NONE',  ( 0.000000000000000000, -0.5032391393578591332, 0.8641471915237364243 ) ) ;
#75474 = FACE_OUTER_BOUND ( 'NONE', #25396, .T. ) ;
#75475 = CARTESIAN_POINT ( 'NONE',  ( -11.37137302997330046, 1470.992257629510050, 208.1706243720159932 ) ) ;
#75476 = CARTESIAN_POINT ( 'NONE',  ( -6.470239033145795737, 1508.340629334880305, 219.9570550858604179 ) ) ;
#75477 = CARTESIAN_POINT ( 'NONE',  ( 17.27621958092441545, 1422.524277846433961, 226.6568626525910304 ) ) ;
#75478 = CARTESIAN_POINT ( 'NONE',  ( 18.31070135516566211, 1425.421135919995777, 224.8731613538174656 ) ) ;
#75479 = CARTESIAN_POINT ( 'NONE',  ( -10.96966316950000042, 1432.359729192660097, 151.7701366810979948 ) ) ;
#75480 = CARTESIAN_POINT ( 'NONE',  ( 44.76106499233450364, 1440.913060369829964, 265.2081040044519682 ) ) ;
#75482 = LINE ( 'NONE', #7695, #42594 ) ;
#75481 = CARTESIAN_POINT ( 'NONE',  ( -9.898190092519600469, 1471.698199896249889, 211.3831928317650295 ) ) ;
#75483 = DIRECTION ( 'NONE',  ( 0.9510565162951545304, 0.000000000000000000, 0.3090169943749447312 ) ) ;
#75484 = ORIENTED_EDGE ( 'NONE', *, *, #2658, .F. ) ;
#75485 = EDGE_LOOP ( 'NONE', ( #65395, #58348, #58268, #18768 ) ) ;
#75486 = CARTESIAN_POINT ( 'NONE',  ( -9.082054625942792114, 1506.560171907502763, 229.2575063132023558 ) ) ;
#75487 = VECTOR ( 'NONE', #26464, 999.9999999999998863 ) ;
#75488 = CARTESIAN_POINT ( 'NONE',  ( -14.74403395979999942, 1507.703932417990245, 209.3705301297690085 ) ) ;
#75489 = CARTESIAN_POINT ( 'NONE',  ( 7.526684039890001010, 1423.047588554429922, 195.6744588065990058 ) ) ;
#75490 = DIRECTION ( 'NONE',  ( -5.980589973904019347E-17, 1.000000000000000000, -1.736889445713099699E-16 ) ) ;
#75491 = CARTESIAN_POINT ( 'NONE',  ( -11.40384261557694856, 1425.336176176961089, 144.1584481726092122 ) ) ;
#75492 = ADVANCED_FACE ( 'NONE', ( #94385 ), #96512, .T. ) ;
#75493 = DIRECTION ( 'NONE',  ( 0.000000000000000000, -1.000000000000000000, 6.123233995736769734E-17 ) ) ;
#75494 = CARTESIAN_POINT ( 'NONE',  ( -3.906031934150000051, 1515.551704408389924, 207.6332190043490016 ) ) ;
#75495 = CARTESIAN_POINT ( 'NONE',  ( -69.24343105989969160, 1383.785972937140059, 293.9299002094780349 ) ) ;
#75496 = CARTESIAN_POINT ( 'NONE',  ( -14.97895622270000082, 1489.469559537229998, 192.8507424827979833 ) ) ;
#75497 = CARTESIAN_POINT ( 'NONE',  ( -15.20279581456499862, 1513.492015765619954, 193.2119433744669834 ) ) ;
#75498 = CARTESIAN_POINT ( 'NONE',  ( 12.02265620508110189, 1492.768319540230095, 211.9938273525619934 ) ) ;
#75500 = ORIENTED_EDGE ( 'NONE', *, *, #106537, .T. ) ;
#75499 = CARTESIAN_POINT ( 'NONE',  ( -2.341977691500000347, 1457.699844493290129, 219.5360100213989938 ) ) ;
#75501 = DIRECTION ( 'NONE',  ( 0.000000000000000000, 0.000000000000000000, 1.000000000000000000 ) ) ;
#75502 = AXIS2_PLACEMENT_3D ( 'NONE', #78487, #27523, #61708 ) ;
#75503 = CARTESIAN_POINT ( 'NONE',  ( -54.29265189920000267, 1383.804803630430115, 270.2912082677589751 ) ) ;
#75504 = CARTESIAN_POINT ( 'NONE',  ( -0.2725765502280009800, 1430.103961438589977, 217.4715266419189845 ) ) ;
#75505 = VERTEX_POINT ( 'NONE', #38896 ) ;
#75506 = ORIENTED_EDGE ( 'NONE', *, *, #70766, .F. ) ;
#75507 = CARTESIAN_POINT ( 'NONE',  ( -8.888812255142289231, 1385.314781883149863, 218.6605257023059892 ) ) ;
#75508 = DIRECTION ( 'NONE',  ( -1.577721810442025012E-32, -1.000000000000000000, 6.123233995736769734E-17 ) ) ;
#75510 = CARTESIAN_POINT ( 'NONE',  ( 0.8265244082521410185, 1408.941923255679967, 231.1644249228330068 ) ) ;
#75509 = FACE_OUTER_BOUND ( 'NONE', #8317, .T. ) ;
#75511 = CARTESIAN_POINT ( 'NONE',  ( 11.74542637677500068, 1479.756186535490087, 210.0649862889210056 ) ) ;
#75512 = CARTESIAN_POINT ( 'NONE',  ( -106.6838299039999924, 1381.594688875880138, 298.7333698723590487 ) ) ;
#75513 = EDGE_CURVE ( 'NONE', #89621, #9383, #13681, .T. ) ;
#75514 = CARTESIAN_POINT ( 'NONE',  ( 3.868582513889999852, 1449.766611533390005, 190.4179587020989857 ) ) ;
#75515 = CARTESIAN_POINT ( 'NONE',  ( -29.00779973304142345, 1526.382868172863937, 200.9494832830838789 ) ) ;
#75516 = CARTESIAN_POINT ( 'NONE',  ( -12.46763692646640109, 1508.551704408389924, 216.9465170557990064 ) ) ;
#75517 = CARTESIAN_POINT ( 'NONE',  ( 0.4463512173630010405, 1458.283482072889910, 202.2977778284289911 ) ) ;
#75518 = CARTESIAN_POINT ( 'NONE',  ( 0.8297112819069999423, 1408.942034543729960, 186.6238164324980175 ) ) ;
#75519 = CARTESIAN_POINT ( 'NONE',  ( 13.03373128269810088, 1424.818470566259975, 222.5271577161219909 ) ) ;
#75520 = CARTESIAN_POINT ( 'NONE',  ( 7.544839107842309822, 1434.691991358320138, 204.7085460358119917 ) ) ;
#75521 = CARTESIAN_POINT ( 'NONE',  ( -3.656266903649279865, 1441.517177768429974, 170.5484099602190042 ) ) ;
#75522 = AXIS2_PLACEMENT_3D ( 'NONE', #22246, #99514, #73240 ) ;
#75523 = CARTESIAN_POINT ( 'NONE',  ( -1.835529294006269962, 1450.383122819009941, 182.7749848618290116 ) ) ;
#75524 = EDGE_LOOP ( 'NONE', ( #71057, #8452, #82740, #98925 ) ) ;
#75525 = CARTESIAN_POINT ( 'NONE',  ( -4.310970535356173805, 1398.041661513277631, 196.6635432619665380 ) ) ;
#75526 = CARTESIAN_POINT ( 'NONE',  ( 19.08737576949210180, 1456.351080380050007, 226.3347076951879728 ) ) ;
#75527 = CARTESIAN_POINT ( 'NONE',  ( -8.861903497826141063, 1384.885539543426603, 218.6850719556965998 ) ) ;
#75528 = ADVANCED_FACE ( 'NONE', ( #39468 ), #36601, .T. ) ;
#75529 = CARTESIAN_POINT ( 'NONE',  ( 2.330134126678752526, 1515.492058413687573, 213.2603893528570893 ) ) ;
#75530 = CARTESIAN_POINT ( 'NONE',  ( 18.44118978608688764, 1436.374823392123290, 146.9772265392791439 ) ) ;
#75531 = CARTESIAN_POINT ( 'NONE',  ( 1.916663648440000145, 1477.644687901090037, 198.8912423860989804 ) ) ;
#75532 = CARTESIAN_POINT ( 'NONE',  ( -108.3701702990000086, 1386.736519522250092, 310.7981234312589436 ) ) ;
#75533 = CARTESIAN_POINT ( 'NONE',  ( -7.596320609278680358, 1510.929912129050081, 214.9254183270510055 ) ) ;
#75534 = CARTESIAN_POINT ( 'NONE',  ( -7.592149787980000397, 1361.964468435470053, 207.6218459616989946 ) ) ;
#75535 = CARTESIAN_POINT ( 'NONE',  ( 3.968827104744170331, 1517.051704408389924, 188.7040005449509863 ) ) ;
#75536 = CARTESIAN_POINT ( 'NONE',  ( 13.64863627425580006, 1508.988455644710029, 233.7698699238879954 ) ) ;
#75537 = EDGE_CURVE ( 'NONE', #85718, #95777, #67957, .T. ) ;
#75538 = CARTESIAN_POINT ( 'NONE',  ( -8.145910945669999847, 1424.779583588550167, 207.8601695130389828 ) ) ;
#75539 = CARTESIAN_POINT ( 'NONE',  ( 2.868112131164999745, 1516.855632454399938, 208.3641823986619954 ) ) ;
#75540 = CARTESIAN_POINT ( 'NONE',  ( 5.096730495175649800, 1407.739527309109917, 221.2177969142850031 ) ) ;
#75541 = CARTESIAN_POINT ( 'NONE',  ( 2.330134126767420266, 1515.064792882699976, 204.7923971855439902 ) ) ;
#75542 = CARTESIAN_POINT ( 'NONE',  ( 7.524442094865539943, 1425.458146191759852, 212.2002832223970188 ) ) ;
#75543 = CARTESIAN_POINT ( 'NONE',  ( -27.01669389746110284, 1451.969651449090179, 135.0017772683769977 ) ) ;
#75544 = ORIENTED_EDGE ( 'NONE', *, *, #26363, .F. ) ;
#75545 = CARTESIAN_POINT ( 'NONE',  ( 30.53571888390000311, 1438.952188675479874, 240.1260121752980012 ) ) ;
#75547 = CARTESIAN_POINT ( 'NONE',  ( -17.45344265050000132, 1410.019001388030119, 194.6345986913979971 ) ) ;
#75546 = CARTESIAN_POINT ( 'NONE',  ( -2.444993193446221014, 1524.972383263452912, 175.9711954026445824 ) ) ;
#75548 = ADVANCED_FACE ( 'NONE', ( #96431 ), #11581, .F. ) ;
#75549 = CARTESIAN_POINT ( 'NONE',  ( -2.441800263710489638, 1419.516450075849889, 186.0746046563270113 ) ) ;
#75550 = DIRECTION ( 'NONE',  ( -0.8383970168982891602, -0.5450600352768949497, 0.000000000000000000 ) ) ;
#75551 = CARTESIAN_POINT ( 'NONE',  ( 0.5987183461865049905, 1507.212886145319999, 186.4932301926239688 ) ) ;
#75552 = EDGE_CURVE ( 'NONE', #52837, #107294, #79184, .T. ) ;
#75553 = CARTESIAN_POINT ( 'NONE',  ( -20.52850840453259806, 1452.196189077299778, 142.6025761593519974 ) ) ;
#75554 = LINE ( 'NONE', #67153, #72212 ) ;
#75555 = VERTEX_POINT ( 'NONE', #81259 ) ;
#75556 = CARTESIAN_POINT ( 'NONE',  ( 10.92766316885620093, 1501.618323021010156, 205.6861136770480130 ) ) ;
#75557 = CARTESIAN_POINT ( 'NONE',  ( 16.91352249406399721, 1423.656902980690120, 228.6870985840920127 ) ) ;
#75558 = DIRECTION ( 'NONE',  ( 0.000000000000000000, 0.000000000000000000, -1.000000000000000000 ) ) ;
#75559 = ORIENTED_EDGE ( 'NONE', *, *, #100152, .T. ) ;
#75560 = ORIENTED_EDGE ( 'NONE', *, *, #38039, .T. ) ;
#75561 = CARTESIAN_POINT ( 'NONE',  ( -53.45887188369999876, 1384.635297440300064, 230.7554238970589893 ) ) ;
#75562 = CARTESIAN_POINT ( 'NONE',  ( -22.71281444701029884, 1409.706191629969908, 209.1573898883480069 ) ) ;
#75563 = EDGE_CURVE ( 'NONE', #110607, #102937, #37481, .T. ) ;
#75564 = ORIENTED_EDGE ( 'NONE', *, *, #16557, .F. ) ;
#75565 = CARTESIAN_POINT ( 'NONE',  ( -0.4885701619419999808, 1464.413060387330006, 229.7716327975979880 ) ) ;
#75566 = FACE_OUTER_BOUND ( 'NONE', #68554, .T. ) ;
#75567 = B_SPLINE_CURVE_WITH_KNOTS ( 'NONE', 3,
 ( #81233, #105915, #46019, #80147, #62276, #4013, #3467, #37595, #70689, #104801, #28647, #80704, #47107, #53887, #88023, #11307, #2922 ),
 .UNSPECIFIED., .F., .F.,
 ( 4, 2, 2, 2, 2, 1, 2, 2, 4 ),
 ( 0.000000000000000000, 0.2499999999999922284, 0.3749999999999876765, 0.4999999999999831246, 0.6249999999999785727, 0.6874999999999729106, 0.7187499999999863443, 0.7499999999999997780, 1.000000000000000000 ),
 .UNSPECIFIED. ) ;
#75568 = EDGE_CURVE ( 'NONE', #3563, #24877, #30644, .T. ) ;
#75569 = CARTESIAN_POINT ( 'NONE',  ( -4.416454581009999991, 1498.348563960429829, 236.0667878369980031 ) ) ;
#75570 = CARTESIAN_POINT ( 'NONE',  ( -21.66372438889999685, 1410.866044241829968, 216.3363889088479937 ) ) ;
#75571 = ORIENTED_EDGE ( 'NONE', *, *, #20753, .F. ) ;
#75572 = CARTESIAN_POINT ( 'NONE',  ( 44.51450203682119877, 1449.929878811980188, 268.5455458174560022 ) ) ;
#75573 = CARTESIAN_POINT ( 'NONE',  ( -11.12430337309289818, 1391.913060387059886, 206.3375259381840294 ) ) ;
#75574 = CARTESIAN_POINT ( 'NONE',  ( -16.94980721129255841, 1421.957272272979026, 226.8340596599985872 ) ) ;
#75575 =( BOUNDED_SURFACE ( )  B_SPLINE_SURFACE ( 3, 2, ( 
 ( #52322, #94849, #103222 ),
 ( #18125, #86445, #86996 ),
 ( #9735, #93179, #61290 ),
 ( #43901, #16448, #59057 ),
 ( #110540, #44461, #33827 ),
 ( #68019, #102128, #25407 ),
 ( #52868, #10284, #34390 ),
 ( #59600, #93716, #16993 ),
 ( #51193, #85323, #102663 ),
 ( #8618, #68565, #60158 ) ),
 .UNSPECIFIED., .F., .F., .T. ) 
 B_SPLINE_SURFACE_WITH_KNOTS ( ( 4, 2, 2, 2, 4 ),
 ( 3, 3 ),
 ( 0.000000000000000000, 0.3926990816987241395, 0.7853981633974482790, 1.178097245096172418, 1.570796326794896558 ),
 ( 0.000000000000000000, 1.000000000000000000 ),
 .UNSPECIFIED. ) 
 GEOMETRIC_REPRESENTATION_ITEM ( )  RATIONAL_B_SPLINE_SURFACE ( (
 ( 1.000000000000000000, 0.7763623250684315025, 1.000000000000000000),
 ( 1.000000000000000000, 0.7763684247040171238, 1.000000000000000000),
 ( 1.000000000000000000, 0.7746454561790633297, 1.000000000000000000),
 ( 1.000000000000000000, 0.7679730451979892569, 1.000000000000000000),
 ( 1.000000000000000000, 0.7630177051949805778, 1.000000000000000000),
 ( 1.000000000000000000, 0.7504512394525143515, 1.000000000000000000),
 ( 1.000000000000000000, 0.7428408967930927309, 1.000000000000000000),
 ( 1.000000000000000000, 0.7259222650906490548, 1.000000000000000000),
 ( 1.000000000000000000, 0.7166207884822589635, 1.000000000000000000),
 ( 1.000000000000000000, 0.7071067811865853203, 1.000000000000000000) ) ) 
 REPRESENTATION_ITEM ( '' )  SURFACE ( )  );
#75576 = CARTESIAN_POINT ( 'NONE',  ( 6.936398355645000180, 1516.667393516340098, 205.0850970932970085 ) ) ;
#75577 = ORIENTED_EDGE ( 'NONE', *, *, #29783, .T. ) ;
#75578 = CARTESIAN_POINT ( 'NONE',  ( 18.93123594888506389, 1457.623381184288746, 226.8509991318317986 ) ) ;
#75579 = CARTESIAN_POINT ( 'NONE',  ( 0.8500299760647389569, 1445.209765166890065, 199.0867373374109945 ) ) ;
#75580 = LINE ( 'NONE', #16713, #94457 ) ;
#75581 = ORIENTED_EDGE ( 'NONE', *, *, #14485, .F. ) ;
#75582 = CARTESIAN_POINT ( 'NONE',  ( 2.500000000000000000, 1448.210448407430022, 182.3842139046979867 ) ) ;
#75583 = CARTESIAN_POINT ( 'NONE',  ( 26.65315064050000160, 1451.818441385129745, 135.6605374257979975 ) ) ;
#75584 = CARTESIAN_POINT ( 'NONE',  ( -4.804127539825289617, 1508.551704408389924, 212.5477707811770074 ) ) ;
#75585 = CARTESIAN_POINT ( 'NONE',  ( 8.400707445830571274, 1503.837797309470034, 218.7125449626740021 ) ) ;
#75586 = CARTESIAN_POINT ( 'NONE',  ( 7.595989987639999441, 1421.918083777009997, 195.7234947746989917 ) ) ;
#75587 = EDGE_CURVE ( 'NONE', #91119, #92844, #41487, .T. ) ;
#75588 = CARTESIAN_POINT ( 'NONE',  ( -3.187940576023601924, 1370.279959858722350, 207.3802660875432480 ) ) ;
#75589 = CARTESIAN_POINT ( 'NONE',  ( -5.202919524220000369, 1495.777348644990070, 199.0561099548990001 ) ) ;
#75590 = CARTESIAN_POINT ( 'NONE',  ( 2.975652649659970006, 1409.016972467610003, 187.2097493808250306 ) ) ;
#75592 = CARTESIAN_POINT ( 'NONE',  ( 27.01382310970000233, 1451.969724731730139, 134.9184576876980088 ) ) ;
#75591 = CARTESIAN_POINT ( 'NONE',  ( 1.649770437750000207, 1417.467804857230021, 234.2977195291979911 ) ) ;
#75593 = CARTESIAN_POINT ( 'NONE',  ( 10.69099011935269949, 1423.897063905130153, 206.6970677081539804 ) ) ;
#75594 = B_SPLINE_CURVE_WITH_KNOTS ( 'NONE', 3,
 ( #84975, #46336, #105113, #62603 ),
 .UNSPECIFIED., .F., .F.,
 ( 4, 4 ),
 ( 0.000000000000000000, 1.000000000000000000 ),
 .UNSPECIFIED. ) ;
#75595 = CARTESIAN_POINT ( 'NONE',  ( -10.42949413029999839, 1379.124834216069985, 215.7630140696190040 ) ) ;
#75596 = ADVANCED_FACE ( 'NONE', ( #107161 ), #27650, .F. ) ;
#75597 = CARTESIAN_POINT ( 'NONE',  ( 2.431412526649999961, 1428.647745098929818, 149.4227846719979880 ) ) ;
#75598 = VERTEX_POINT ( 'NONE', #99848 ) ;
#75599 = CARTESIAN_POINT ( 'NONE',  ( 12.73136601901799914, 1416.225364278609959, 221.9752797600760061 ) ) ;
#75600 = CARTESIAN_POINT ( 'NONE',  ( 11.79676934137780187, 1432.336587679680179, 150.5395560521619984 ) ) ;
#75601 = DIRECTION ( 'NONE',  ( -3.552713678800501718E-15, 0.000000000000000000, -1.000000000000000000 ) ) ;
#75602 = CARTESIAN_POINT ( 'NONE',  ( -14.28029416299999887, 1390.367276380369958, 209.8449221693030040 ) ) ;
#75603 = CARTESIAN_POINT ( 'NONE',  ( 9.407086540023099630, 1428.119775475241568, 137.0999999980979567 ) ) ;
#75604 = CARTESIAN_POINT ( 'NONE',  ( 12.08651861739819999, 1426.128252729390169, 202.8034848243579802 ) ) ;
#75605 = CARTESIAN_POINT ( 'NONE',  ( -10.98588173227549980, 1462.620677329530054, 207.9438354903729760 ) ) ;
#75606 = CARTESIAN_POINT ( 'NONE',  ( -31.32742178079999462, 1444.517716081189974, 255.3819207742980097 ) ) ;
#75607 = CARTESIAN_POINT ( 'NONE',  ( -8.981694392507570512, 1384.175213772349935, 218.6078250012760122 ) ) ;
#75608 = CARTESIAN_POINT ( 'NONE',  ( 11.79248762149999941, 1433.694417784170128, 150.8231452198980094 ) ) ;
#75609 = FACE_OUTER_BOUND ( 'NONE', #8829, .T. ) ;
#75610 = CARTESIAN_POINT ( 'NONE',  ( -11.03823282802460071, 1462.321972888460095, 209.2524123285700171 ) ) ;
#75611 = DIRECTION ( 'NONE',  ( -0.8862055364699944482, 0.4630717415824551764, 0.01429367964246674658 ) ) ;
#75612 = CARTESIAN_POINT ( 'NONE',  ( 11.86347265473209944, 1425.940497895709996, 201.1513796338190048 ) ) ;
#75613 = CARTESIAN_POINT ( 'NONE',  ( 8.832652841333949567, 1464.232421199639930, 213.8219978802969763 ) ) ;
#75614 = CARTESIAN_POINT ( 'NONE',  ( -19.62297883809999988, 1486.467287247530066, 189.8658461344980140 ) ) ;
#75615 = CARTESIAN_POINT ( 'NONE',  ( 11.34243525793542595, 1398.249318583079003, 215.4825434740161541 ) ) ;
#75616 = CARTESIAN_POINT ( 'NONE',  ( -16.75996197530000131, 1409.498331158530164, 224.9264968051979849 ) ) ;
#75617 = FACE_OUTER_BOUND ( 'NONE', #83525, .T. ) ;
#75618 = CARTESIAN_POINT ( 'NONE',  ( 12.59650095789967494, 1416.818673810193104, 223.3990019334950716 ) ) ;
#75619 = CARTESIAN_POINT ( 'NONE',  ( -16.98925717958650239, 1409.671016636710192, 192.8613407240889899 ) ) ;
#75620 = CARTESIAN_POINT ( 'NONE',  ( 1.466212339980000001, 1515.204044912790096, 204.7960436283990191 ) ) ;
#75621 = CARTESIAN_POINT ( 'NONE',  ( 12.67165775215690005, 1426.886500604199910, 205.4076336300960008 ) ) ;
#75622 = CARTESIAN_POINT ( 'NONE',  ( -14.38096573875979978, 1422.143734374870064, 196.2925565939719945 ) ) ;
#75623 = CARTESIAN_POINT ( 'NONE',  ( -3.923552080019999444, 1416.217772598529791, 227.2437918289980132 ) ) ;
#75624 = CARTESIAN_POINT ( 'NONE',  ( -19.16657957493040243, 1419.018181932309972, 207.3808575570400023 ) ) ;
#75625 = CARTESIAN_POINT ( 'NONE',  ( 0.1707805864721430034, 1479.871249927690087, 182.0999213800499774 ) ) ;
#75627 = ORIENTED_EDGE ( 'NONE', *, *, #52162, .T. ) ;
#75626 = CARTESIAN_POINT ( 'NONE',  ( 31.23437356469435144, 1518.913060387330006, 195.3468678195113739 ) ) ;
#75628 = CARTESIAN_POINT ( 'NONE',  ( 1.679554717346656512, 1526.335487865669393, 178.4817626271500899 ) ) ;
#75629 = CARTESIAN_POINT ( 'NONE',  ( 0.4885701619419999808, 1464.413060387330006, 188.4720591257980118 ) ) ;
#75630 = CARTESIAN_POINT ( 'NONE',  ( 13.19837685220000090, 1434.900414701970021, 149.9808420451980169 ) ) ;
#75631 = CARTESIAN_POINT ( 'NONE',  ( -41.66177311457460064, 1443.657316188219966, 134.0999999982009854 ) ) ;
#75632 = CARTESIAN_POINT ( 'NONE',  ( -109.7183341539999901, 1384.893508909079856, 297.0862237871589855 ) ) ;
#75633 = VERTEX_POINT ( 'NONE', #15822 ) ;
#75634 = CARTESIAN_POINT ( 'NONE',  ( -16.97880994393915799, 1525.055427061254477, 181.2503854651100710 ) ) ;
#75635 = FACE_OUTER_BOUND ( 'NONE', #65381, .T. ) ;
#75636 = CARTESIAN_POINT ( 'NONE',  ( -103.6849498593194454, 1379.968036174091139, 305.2864844434715224 ) ) ;
#75637 = CARTESIAN_POINT ( 'NONE',  ( -16.69343462643249509, 1526.373507135059526, 183.7014874209610866 ) ) ;
#75638 = CARTESIAN_POINT ( 'NONE',  ( -7.199110364057590417, 1435.605555164340103, 215.2453670761979936 ) ) ;
#75639 = DIRECTION ( 'NONE',  ( -1.986099751379994994E-13, 1.179495926710000177E-14, 1.000000000000000000 ) ) ;
#75640 = DIRECTION ( 'NONE',  ( 0.000000000000000000, 0.000000000000000000, -1.000000000000000000 ) ) ;
#75641 = CARTESIAN_POINT ( 'NONE',  ( -14.09844076420000114, 1379.806461617270088, 211.4199521846090022 ) ) ;
#75642 = CARTESIAN_POINT ( 'NONE',  ( 3.913694301390000518, 1434.228895445299941, 184.9284356229979949 ) ) ;
#75643 = CARTESIAN_POINT ( 'NONE',  ( -59.16917651648999055, 1385.057337441720165, 242.2145958383559901 ) ) ;
#75644 = CARTESIAN_POINT ( 'NONE',  ( -11.31284123697730060, 1391.913060387289988, 211.6673135973910291 ) ) ;
#75645 = CARTESIAN_POINT ( 'NONE',  ( 12.30985188076150116, 1427.199944344410142, 207.2898684024129921 ) ) ;
#75646 = ORIENTED_EDGE ( 'NONE', *, *, #66990, .F. ) ;
#75647 = CARTESIAN_POINT ( 'NONE',  ( -30.94580702080000023, 1450.971962479829926, 136.2591019887980224 ) ) ;
#75648 = CARTESIAN_POINT ( 'NONE',  ( -15.72592697610619972, 1409.716376149900043, 226.1430192477070023 ) ) ;
#75650 = VERTEX_POINT ( 'NONE', #39959 ) ;
#75649 = CARTESIAN_POINT ( 'NONE',  ( -1.679554717346650072, 1526.335487865669393, 239.7619292962459383 ) ) ;
#75651 = CARTESIAN_POINT ( 'NONE',  ( 2.122693458210000106, 1474.244506326290093, 219.5571033596989992 ) ) ;
#75652 = CARTESIAN_POINT ( 'NONE',  ( -17.74610122149952574, 1410.896492951278333, 225.1977723225998886 ) ) ;
#75653 = CARTESIAN_POINT ( 'NONE',  ( -109.1319690089999881, 1384.726207818360081, 311.2603020862590029 ) ) ;
#75654 = CARTESIAN_POINT ( 'NONE',  ( -5.387811863060000483, 1496.648312753189884, 199.2595355468089906 ) ) ;
#75655 = CARTESIAN_POINT ( 'NONE',  ( 41.99750770990659277, 1442.862246457818856, 269.6474897767589027 ) ) ;
#75656 = DIRECTION ( 'NONE',  ( 0.000000000000000000, 1.000000000000000000, 0.000000000000000000 ) ) ;
#75657 = CARTESIAN_POINT ( 'NONE',  ( 18.99772002587713970, 1437.736752343170338, 213.2567656554087705 ) ) ;
#75658 = CARTESIAN_POINT ( 'NONE',  ( 2.500000000000000000, 1436.879499737369997, 182.8948590198639863 ) ) ;
#75659 = CARTESIAN_POINT ( 'NONE',  ( -96.21470915085019726, 1331.448250124730066, 304.2218459572590064 ) ) ;
#75660 = CARTESIAN_POINT ( 'NONE',  ( 8.099819236969999281, 1497.713060387329961, 229.6744222972979799 ) ) ;
#75661 = CARTESIAN_POINT ( 'NONE',  ( -1.030872721199999953, 1455.330695093189888, 198.6237620522990142 ) ) ;
#75662 = CARTESIAN_POINT ( 'NONE',  ( -5.012317106364999830, 1517.020727862619879, 206.2534121335969814 ) ) ;
#75663 = CARTESIAN_POINT ( 'NONE',  ( 2.500000000320000026, 1447.619163115829906, 168.9991029863980145 ) ) ;
#75664 = VERTEX_POINT ( 'NONE', #75774 ) ;
#75665 = CARTESIAN_POINT ( 'NONE',  ( 14.90597039080000030, 1485.461822778330088, 224.8639988762980124 ) ) ;
#75666 = FACE_OUTER_BOUND ( 'NONE', #20427, .T. ) ;
#75668 = VERTEX_POINT ( 'NONE', #58426 ) ;
#75667 = CARTESIAN_POINT ( 'NONE',  ( -68.62877234682019889, 1379.747624006590058, 280.2303598637119535 ) ) ;
#75669 = CARTESIAN_POINT ( 'NONE',  ( -7.827642019093867809, 1383.090619493809072, 218.8065417710187432 ) ) ;
#75670 = VERTEX_POINT ( 'NONE', #100416 ) ;
#75671 = DIRECTION ( 'NONE',  ( 9.341989762165448955E-47, -1.000000000000000000, 1.836970198721029688E-16 ) ) ;
#75672 = CARTESIAN_POINT ( 'NONE',  ( -24.18568768169999927, 1430.355574618330138, 205.7586331603280030 ) ) ;
#75674 = CARTESIAN_POINT ( 'NONE',  ( 16.11026621011109938, 1409.500970208199988, 192.7569509766140072 ) ) ;
#75673 = CARTESIAN_POINT ( 'NONE',  ( -11.71631912920000040, 1426.708822453530047, 142.6848033031979810 ) ) ;
#75675 = CARTESIAN_POINT ( 'NONE',  ( 5.013274961385000061, 1517.068517094990057, 211.4089302402969963 ) ) ;
#75676 = CARTESIAN_POINT ( 'NONE',  ( 40.71506559347059806, 1443.618839491749895, 137.1015882309970095 ) ) ;
#75677 = EDGE_CURVE ( 'NONE', #32377, #49931, #94701, .T. ) ;
#75678 = CARTESIAN_POINT ( 'NONE',  ( -6.814833847790001009, 1407.100405669529891, 264.8986903022980073 ) ) ;
#75679 = CARTESIAN_POINT ( 'NONE',  ( -2.953034986745780355, 1509.089592128550066, 179.4428969035240016 ) ) ;
#75681 = EDGE_CURVE ( 'NONE', #93538, #18777, #5382, .T. ) ;
#75680 = CARTESIAN_POINT ( 'NONE',  ( 12.58697395272539943, 1501.023083793659907, 210.9163362933149983 ) ) ;
#75682 = ITEM_DEFINED_TRANSFORMATION ( 'NONE', 'NONE', #52208,  #21632 ) ;
#75683 = CARTESIAN_POINT ( 'NONE',  ( 4.940370962924140130, 1508.551704408389924, 212.0905280059049858 ) ) ;
#75684 = CARTESIAN_POINT ( 'NONE',  ( -36.32303967410180690, 1437.564594092069910, 136.5418270925559909 ) ) ;
#75685 = ORIENTED_EDGE ( 'NONE', *, *, #23261, .F. ) ;
#75686 = CARTESIAN_POINT ( 'NONE',  ( -13.67844991905460006, 1504.250345474479900, 227.6838247662160200 ) ) ;
#75687 = CYLINDRICAL_SURFACE ( 'NONE', #15456, 2.000000000000003109 ) ;
#75688 = VERTEX_POINT ( 'NONE', #35984 ) ;
#75689 = ORIENTED_EDGE ( 'NONE', *, *, #7705, .T. ) ;
#75690 = CARTESIAN_POINT ( 'NONE',  ( -29.76000164536801762, 1509.996124611334608, 209.6549034325891796 ) ) ;
#75691 = CARTESIAN_POINT ( 'NONE',  ( 10.31264293309589952, 1453.306623136699955, 211.6178708374930011 ) ) ;
#75692 = CARTESIAN_POINT ( 'NONE',  ( -7.015915899421429458, 1508.242408774839987, 219.9931816339760076 ) ) ;
#75693 = CARTESIAN_POINT ( 'NONE',  ( -13.58041482308779990, 1508.551704408389924, 210.3416170982540052 ) ) ;
#75694 = DIRECTION ( 'NONE',  ( 0.000000000000000000, 0.000000000000000000, -1.000000000000000000 ) ) ;
#75695 = CARTESIAN_POINT ( 'NONE',  ( -40.70526293792549666, 1444.199265999389809, 137.0833899199729728 ) ) ;
#75696 = ADVANCED_FACE ( 'NONE', ( #18051 ), #62577, .T. ) ;
#75697 = FACE_OUTER_BOUND ( 'NONE', #97824, .T. ) ;
#75698 = CARTESIAN_POINT ( 'NONE',  ( 29.30029655192931770, 1525.907212628473872, 221.3719603026171114 ) ) ;
#75699 = CARTESIAN_POINT ( 'NONE',  ( 38.70145357755679782, 1443.501467202841695, 136.9791754767358611 ) ) ;
#75700 = CARTESIAN_POINT ( 'NONE',  ( -71.50733119889839884, 1384.746684647190023, 268.9689952328979530 ) ) ;
#75701 = ORIENTED_EDGE ( 'NONE', *, *, #78179, .F. ) ;
#75702 = CARTESIAN_POINT ( 'NONE',  ( -3.261007169695000041, 1516.596789218710001, 201.7991362452670216 ) ) ;
#75703 = CARTESIAN_POINT ( 'NONE',  ( -3.261652325025000021, 1516.939580991450157, 209.1351299096569960 ) ) ;
#75704 = VERTEX_POINT ( 'NONE', #9118 ) ;
#75705 = CARTESIAN_POINT ( 'NONE',  ( 11.77190271057030202, 1427.168883215420010, 146.5473278980630027 ) ) ;
#75706 = CARTESIAN_POINT ( 'NONE',  ( 2.937948913181351873, 1512.266332053888846, 217.0095423517265090 ) ) ;
#75707 = VERTEX_POINT ( 'NONE', #76881 ) ;
#75708 = CARTESIAN_POINT ( 'NONE',  ( -13.56343219680000090, 1416.311719779230089, 221.8446948800979897 ) ) ;
#75709 = CARTESIAN_POINT ( 'NONE',  ( -11.04095478537250052, 1432.346658662259870, 151.7150578551980118 ) ) ;
#75710 = CARTESIAN_POINT ( 'NONE',  ( -6.593958911874039153, 1433.916835198372837, 214.5366901220844511 ) ) ;
#75711 =( BOUNDED_CURVE ( )  B_SPLINE_CURVE ( 3, ( #13030, #106027, #39358, #73532 ),
 .UNSPECIFIED., .F., .F. ) 
 B_SPLINE_CURVE_WITH_KNOTS ( ( 4, 4 ),
 ( 1.013003765281151880, 2.128589034411239922 ),
 .UNSPECIFIED. ) 
 CURVE ( )  GEOMETRIC_REPRESENTATION_ITEM ( )  RATIONAL_B_SPLINE_CURVE ( ( 1.000000000000000000, 0.8989503786704379218, 0.8989503786704379218, 1.000000000000000000 ) ) 
 REPRESENTATION_ITEM ( '' )  );
#75712 = CARTESIAN_POINT ( 'NONE',  ( 24.16126765782752983, 1411.115443491750057, 209.3031085556986568 ) ) ;
#75713 = CARTESIAN_POINT ( 'NONE',  ( -12.60572195280000152, 1419.902368950130040, 222.2409655462980140 ) ) ;
#75714 = CARTESIAN_POINT ( 'NONE',  ( 11.00530662964919948, 1470.220588418350189, 206.9530455906469797 ) ) ;
#75715 = CARTESIAN_POINT ( 'NONE',  ( -9.853806547159999596, 1472.519282585889869, 204.9780994919989894 ) ) ;
#75716 = CARTESIAN_POINT ( 'NONE',  ( -11.71397076299980000, 1489.483175994190105, 212.5377881273170146 ) ) ;
#75717 = CARTESIAN_POINT ( 'NONE',  ( -60.07536325030000057, 1379.722864260740153, 261.7802271240589675 ) ) ;
#75718 = CARTESIAN_POINT ( 'NONE',  ( 23.38056391995960226, 1429.882408728640030, 206.2064200242359959 ) ) ;
#75720 = CARTESIAN_POINT ( 'NONE',  ( 3.587095331290290012, 1466.405175726029938, 198.6593342341859909 ) ) ;
#75719 = CARTESIAN_POINT ( 'NONE',  ( -20.79406209140000072, 1505.269740423389976, 209.4146929180660095 ) ) ;
#75721 = DIRECTION ( 'NONE',  ( 2.664535259100376091E-15, 0.000000000000000000, -1.000000000000000000 ) ) ;
#75722 = EDGE_CURVE ( 'NONE', #39623, #65697, #17782, .T. ) ;
#75723 = CARTESIAN_POINT ( 'NONE',  ( -4.616272334694999202, 1517.030858226499959, 216.4568033268070053 ) ) ;
#75724 = ORIENTED_EDGE ( 'NONE', *, *, #46851, .F. ) ;
#75725 = CARTESIAN_POINT ( 'NONE',  ( -1.313821539278499539, 1486.248793315761759, 181.8009333484911565 ) ) ;
#75726 = CARTESIAN_POINT ( 'NONE',  ( -21.62164173379369814, 1519.551704408389924, 210.2163513719069954 ) ) ;
#75727 = CARTESIAN_POINT ( 'NONE',  ( 4.621267883935000320, 1516.830644417779922, 214.1213023606370029 ) ) ;
#75728 = CARTESIAN_POINT ( 'NONE',  ( -2.905385431959103482, 1484.613154424542927, 183.2707264708236892 ) ) ;
#75729 = EDGE_CURVE ( 'NONE', #28004, #67358, #41361, .T. ) ;
#75730 = CARTESIAN_POINT ( 'NONE',  ( -2.319252365495519719, 1483.729198182639948, 198.7017601680090024 ) ) ;
#75732 = VERTEX_POINT ( 'NONE', #51681 ) ;
#75731 = CARTESIAN_POINT ( 'NONE',  ( -11.67852220755739800, 1501.333649510869918, 211.3056319267720085 ) ) ;
#75733 = CARTESIAN_POINT ( 'NONE',  ( -7.966197656679999461, 1384.914723845990011, 199.4893138218189961 ) ) ;
#75734 = CARTESIAN_POINT ( 'NONE',  ( -1.567668168089999980, 1508.358814145789893, 220.7516519924990064 ) ) ;
#75735 = CARTESIAN_POINT ( 'NONE',  ( -11.73152282100000043, 1429.503122515530094, 150.1532985455980054 ) ) ;
#75736 = CARTESIAN_POINT ( 'NONE',  ( 19.03555911386669663, 1456.921423106470002, 225.4803602023239932 ) ) ;
#75737 = CARTESIAN_POINT ( 'NONE',  ( -5.711199616050000039, 1441.581233931670113, 184.9882973716979961 ) ) ;
#75738 = CARTESIAN_POINT ( 'NONE',  ( -113.4000000000000057, 1306.483669372790018, 304.2218459572590064 ) ) ;
#75739 = CARTESIAN_POINT ( 'NONE',  ( 16.66936639845630097, 1518.913060387330006, 180.4828114240739296 ) ) ;
#75740 = CARTESIAN_POINT ( 'NONE',  ( 0.2707604742883649718, 1473.796951665749930, 188.2801592720749966 ) ) ;
#75742 = CARTESIAN_POINT ( 'NONE',  ( -20.67632449137469663, 1505.206979486720002, 209.5612231824529772 ) ) ;
#75741 = CARTESIAN_POINT ( 'NONE',  ( -20.86338484379999869, 1482.728658250230183, 225.9420377470979986 ) ) ;
#75743 = DIRECTION ( 'NONE',  ( -0.7067702477489239410, 0.03085653766399039377, -0.7067698995998028533 ) ) ;
#75744 = VERTEX_POINT ( 'NONE', #97536 ) ;
#75745 = CARTESIAN_POINT ( 'NONE',  ( -3.267291643295000103, 1516.842852731759876, 205.6749038603869906 ) ) ;
#75746 = CARTESIAN_POINT ( 'NONE',  ( 6.105441334590000046, 1407.073549914729938, 269.6382019816980460 ) ) ;
#75747 = CARTESIAN_POINT ( 'NONE',  ( -32.23393008293637507, 1523.462669333491931, 216.8400319009761006 ) ) ;
#75748 = CARTESIAN_POINT ( 'NONE',  ( 19.03615913129999981, 1430.304308985630087, 193.6166698355980031 ) ) ;
#75749 = CARTESIAN_POINT ( 'NONE',  ( 19.90509729610057121, 1426.429786633350204, 221.4441842125065705 ) ) ;
#75750 = CARTESIAN_POINT ( 'NONE',  ( -10.06053593028460647, 1390.279853981375481, 216.3031875838134681 ) ) ;
#75751 = CARTESIAN_POINT ( 'NONE',  ( -1.497109119499999919, 1451.179563906029898, 183.7882761563980125 ) ) ;
#75752 = DIRECTION ( 'NONE',  ( 1.755985294532464991E-16, -1.000000000000000000, 1.338183447452830017E-16 ) ) ;
#75753 = CARTESIAN_POINT ( 'NONE',  ( -15.94926467029999984, 1417.442432002970236, 205.6519267168989984 ) ) ;
#75754 = CARTESIAN_POINT ( 'NONE',  ( -13.98755486559999817, 1445.075814781340114, 188.4942211249980062 ) ) ;
#75755 = CARTESIAN_POINT ( 'NONE',  ( -17.70665509759999878, 1431.113060387329824, 216.0622255360179906 ) ) ;
#75756 = CARTESIAN_POINT ( 'NONE',  ( -8.637984804879090817, 1437.135132880460105, 209.2914201311819795 ) ) ;
#75757 = CARTESIAN_POINT ( 'NONE',  ( -7.661470012249999684, 1498.708137977089791, 218.7331922414889789 ) ) ;
#75758 = CARTESIAN_POINT ( 'NONE',  ( 1.456387282373979852, 1499.454921913780026, 181.4473683478569797 ) ) ;
#75759 = CARTESIAN_POINT ( 'NONE',  ( -18.41412373400000035, 1436.828957585569924, 209.1218459616979999 ) ) ;
#75760 = CARTESIAN_POINT ( 'NONE',  ( 11.37049604718461460, 1425.640868497123847, 139.1352433683615288 ) ) ;
#75761 = CARTESIAN_POINT ( 'NONE',  ( 20.87480701074298750, 1525.712835404586031, 234.0672321669388509 ) ) ;
#75762 = CARTESIAN_POINT ( 'NONE',  ( -7.085242296889999736, 1475.668883530029916, 267.5158693932980327 ) ) ;
#75763 = CARTESIAN_POINT ( 'NONE',  ( 1.363639811660000145, 1415.765555525229956, 232.8698637559979829 ) ) ;
#75764 = CARTESIAN_POINT ( 'NONE',  ( 2.632747685671115168, 1375.413060387289988, 210.5601225775116063 ) ) ;
#75765 = CARTESIAN_POINT ( 'NONE',  ( 17.99974041169339856, 1410.897141673580109, 222.9863982244630165 ) ) ;
#75766 = CARTESIAN_POINT ( 'NONE',  ( -48.61829462142750202, 1384.746706768770082, 258.8939480861469633 ) ) ;
#75767 = CARTESIAN_POINT ( 'NONE',  ( -106.5910199462759920, 1391.913060387289988, 302.7980903714330339 ) ) ;
#75768 = CARTESIAN_POINT ( 'NONE',  ( 11.39648212921470005, 1415.089996090470095, 222.7196566067729862 ) ) ;
#75769 = CARTESIAN_POINT ( 'NONE',  ( -106.4840262270000011, 1379.607751643809934, 300.2526974370589983 ) ) ;
#75770 = CARTESIAN_POINT ( 'NONE',  ( -16.49514809540558247, 1525.343727714918259, 237.0302647634398170 ) ) ;
#75771 = CARTESIAN_POINT ( 'NONE',  ( -2.370970874524632510, 1427.002265528473799, 137.0999999980979851 ) ) ;
#75772 = CARTESIAN_POINT ( 'NONE',  ( -20.52142497200000193, 1409.629684344930183, 201.2216482221679712 ) ) ;
#75773 = CARTESIAN_POINT ( 'NONE',  ( -12.10295352893632703, 1377.835289027229692, 206.7956396381484012 ) ) ;
#75774 = CARTESIAN_POINT ( 'NONE',  ( 22.86388141461030088, 1452.114636054890070, 134.1000000004160029 ) ) ;
#75775 = CARTESIAN_POINT ( 'NONE',  ( 2.812944321919999856E-11, 1407.650947899530138, 270.1377426963979929 ) ) ;
#75776 = CARTESIAN_POINT ( 'NONE',  ( 5.649719750514999639, 1514.243099272629934, 201.4728115316369781 ) ) ;
#75777 = CARTESIAN_POINT ( 'NONE',  ( -17.60265120761850000, 1440.931801637090075, 218.9608602370630024 ) ) ;
#75778 = CARTESIAN_POINT ( 'NONE',  ( 17.62880125161999345, 1524.547395018738143, 180.6298994264734858 ) ) ;
#75779 = CARTESIAN_POINT ( 'NONE',  ( -16.61337445554759995, 1463.629612650639956, 220.4655171656389996 ) ) ;
#75781 = CARTESIAN_POINT ( 'NONE',  ( -14.76985295356500139, 1513.863307887919973, 194.1477772255670118 ) ) ;
#75780 = CARTESIAN_POINT ( 'NONE',  ( 11.71755446250000077, 1426.708321543429975, 142.7746014835979906 ) ) ;
#75782 = CARTESIAN_POINT ( 'NONE',  ( 11.69707250263080134, 1426.722100592200150, 141.3107068769770081 ) ) ;
#75783 = CARTESIAN_POINT ( 'NONE',  ( -15.80104652479535865, 1409.464839237975184, 225.2834576049114617 ) ) ;
#75784 = CARTESIAN_POINT ( 'NONE',  ( -124.7066708633999923, 1371.894749952190068, 298.0449835127589608 ) ) ;
#75785 = CARTESIAN_POINT ( 'NONE',  ( 10.34950188612880062, 1451.639534178259964, 207.2650128704659949 ) ) ;
#75786 = CIRCLE ( 'NONE', #22110, 1.999999999999999556 ) ;
#75787 = DIRECTION ( 'NONE',  ( -0.000000000000000000, -1.000000000000000000, -0.000000000000000000 ) ) ;
#75788 = CARTESIAN_POINT ( 'NONE',  ( -4.037378294184999383, 1516.688761843659904, 202.5730239910470232 ) ) ;
#75789 = DIRECTION ( 'NONE',  ( 0.9993908270190955401, -0.03489949670250328678, 0.000000000000000000 ) ) ;
#75790 = CARTESIAN_POINT ( 'NONE',  ( -7.235185706049999332, 1427.271387135730038, 145.8323558008980001 ) ) ;
#75791 = CARTESIAN_POINT ( 'NONE',  ( 16.89844952793499999, 1513.192861445620110, 196.0568336347670026 ) ) ;
#75792 = FACE_BOUND ( 'NONE', #58355, .T. ) ;
#75793 = CARTESIAN_POINT ( 'NONE',  ( -39.44686632430000373, 1376.826872897580188, 228.9534929901590203 ) ) ;
#75794 = CARTESIAN_POINT ( 'NONE',  ( 20.36359139708810062, 1509.286488361670081, 229.5241780718589837 ) ) ;
#75795 = CIRCLE ( 'NONE', #79397, 1.999999999999998224 ) ;
#75797 = ORIENTED_EDGE ( 'NONE', *, *, #98706, .T. ) ;
#75796 = CARTESIAN_POINT ( 'NONE',  ( -43.20831771794370013, 1379.668237090550065, 233.4372218537739911 ) ) ;
#75798 = VERTEX_POINT ( 'NONE', #79102 ) ;
#75799 = CARTESIAN_POINT ( 'NONE',  ( 12.03364418142640169, 1433.763248732019974, 149.8196365535399934 ) ) ;
#75800 = CARTESIAN_POINT ( 'NONE',  ( -5.378824549970000035, 1397.157102389529882, 221.2434471751980141 ) ) ;
#75801 = EDGE_LOOP ( 'NONE', ( #94, #48061, #22903 ) ) ;
#75802 = CARTESIAN_POINT ( 'NONE',  ( -105.7049770469999999, 1379.426018556420104, 306.8995712054589831 ) ) ;
#75803 = DIRECTION ( 'NONE',  ( -3.237679667471999896E-17, -1.000000000000000000, -6.999474336859099157E-17 ) ) ;
#75804 = LINE ( 'NONE', #7487, #6950 ) ;
#75806 = CARTESIAN_POINT ( 'NONE',  ( 17.63676453250000264, 1421.690910225529933, 226.2934404118979899 ) ) ;
#75805 = FACE_OUTER_BOUND ( 'NONE', #31341, .T. ) ;
#75807 = CARTESIAN_POINT ( 'NONE',  ( 4.752926588879999414, 1507.807331693730021, 235.7611666444980187 ) ) ;
#75808 = B_SPLINE_CURVE_WITH_KNOTS ( 'NONE', 3,
 ( #73445, #12957, #72352, #48803 ),
 .UNSPECIFIED., .F., .F.,
 ( 4, 4 ),
 ( 0.000000000000000000, 1.000000000000000000 ),
 .UNSPECIFIED. ) ;
#75809 = CARTESIAN_POINT ( 'NONE',  ( 1.435641954649999885, 1429.773781293429920, 184.4573210536979957 ) ) ;
#75810 = CARTESIAN_POINT ( 'NONE',  ( -0.3443454749849999552, 1415.932840167130053, 191.2798017309980025 ) ) ;
#75811 = CARTESIAN_POINT ( 'NONE',  ( 2.345547646620000037, 1419.146311973829825, 204.4639097625889974 ) ) ;
#75812 = B_SPLINE_SURFACE_WITH_KNOTS ( 'NONE', 5, 4, ( 
 ( #8158, #110631, #101108, #8709, #49641 ),
 ( #66458, #109538, #23850, #34478, #41771 ),
 ( #67551, #83778, #7615, #110081, #41229 ),
 ( #50199, #351, #58042, #17082, #68653 ),
 ( #93273, #32812, #33358, #14903, #92179 ),
 ( #101653, #24940, #25503, #51277, #16536 ) ),
 .UNSPECIFIED., .F., .F., .F.,
 ( 6, 6 ),
 ( 5, 5 ),
 ( 0.000000000000000000, 111.1101480259999903 ),
 ( 25.81581217359999769, 39.03307591160000101 ),
 .UNSPECIFIED. ) ;
#75813 = CARTESIAN_POINT ( 'NONE',  ( 3.716253841760000398, 1442.231740553789905, 214.0742819844890050 ) ) ;
#75814 = CARTESIAN_POINT ( 'NONE',  ( 1.477202341570000188, 1415.048591094029916, 191.4945646901979899 ) ) ;
#75815 = CARTESIAN_POINT ( 'NONE',  ( 11.76498060490000164, 1431.988698125490146, 150.8030710463980029 ) ) ;
#75816 = CARTESIAN_POINT ( 'NONE',  ( 8.664447096804998694, 1512.053281741910041, 202.5614213353869957 ) ) ;
#75817 = EDGE_LOOP ( 'NONE', ( #78394, #97723, #37525, #15889 ) ) ;
#75818 = CARTESIAN_POINT ( 'NONE',  ( 13.21130589195640148, 1435.383535301609982, 150.2969612372090182 ) ) ;
#75819 = B_SPLINE_CURVE_WITH_KNOTS ( 'NONE', 5,
 ( #87207, #63152, #108275, #97252, #46339, #37916, #63688, #10499, #2127 ),
 .UNSPECIFIED., .F., .F.,
 ( 6, 3, 6 ),
 ( 0.000000000000000000, 0.6923720093109234641, 1.000000000000000000 ),
 .UNSPECIFIED. ) ;
#75820 = EDGE_LOOP ( 'NONE', ( #1063, #17702, #71020, #16009 ) ) ;
#75821 = EDGE_LOOP ( 'NONE', ( #91303, #51534, #88509, #50073 ) ) ;
#75822 = CARTESIAN_POINT ( 'NONE',  ( 13.07404856258703418, 1444.822502266877109, 169.4100179250317524 ) ) ;
#75823 = CARTESIAN_POINT ( 'NONE',  ( -9.455441787850000779, 1462.981412785230077, 234.6731641070979890 ) ) ;
#75824 = DIRECTION ( 'NONE',  ( 0.9455185755993177343, 0.000000000000000000, -0.3255681544571540909 ) ) ;
#75825 = CARTESIAN_POINT ( 'NONE',  ( -7.716878941104999612, 1516.833976295079992, 216.4517711926369827 ) ) ;
#75826 = CARTESIAN_POINT ( 'NONE',  ( -7.894477417095063565, 1512.053565093132875, 212.1161737988796858 ) ) ;
#75827 = B_SPLINE_SURFACE_WITH_KNOTS ( 'NONE', 5, 5, ( 
 ( #94477, #96716, #62029, #96149, #27291, #60922, #95598, #44105, #52510, #86639, #2675, #105108 ),
 ( #36800, #78805, #61472, #17750, #19986, #35137, #95051, #36246, #103426, #68768, #18867, #53064 ),
 ( #87201, #10493, #44664, #51952, #43551, #69318, #78242, #86094, #1555, #2120, #45779, #70434 ),
 ( #77698, #18319, #35687, #69878, #103993, #104552, #27848, #19427, #11052, #53629, #87771, #70992 ),
 ( #45223, #28399, #62599, #54180, #88308, #11600, #79914, #34583, #102871, #81004, #4311, #38438 ),
 ( #56911, #65325, #106205, #30598, #72614, #106745, #30032, #90495, #82095, #89407, #28957, #64226 ),
 ( #64786, #4836, #81534, #98349, #91044, #21622, #98896, #31140, #37354, #80463, #20522, #12695 ),
 ( #89947, #105674, #5396, #46333, #47412, #55827, #99435, #13222, #38983, #55277, #3776, #46876 ),
 ( #39554, #73728, #88857, #29487, #22713, #73160, #97794, #107305, #22163, #56363, #54729, #13770 ),
 ( #3227, #47954, #14332, #12141, #107851, #48522, #37909, #71553, #63146, #63683, #97247, #72091 ),
 ( #21071, #75909, #66976, #7595, #68089, #41750, #59673, #31690, #33893, #110061, #33336, #75377 ),
 ( #92156, #100549, #23829, #16517, #42304, #65872, #84838, #15975, #109516, #99992, #102201, #83208 ),
 ( #84304, #40649, #5952, #101087, #32792, #7049, #24385, #58569, #92698, #108408, #91605, #49073 ),
 ( #23284, #58021, #50176, #93783, #67531, #50707, #57480, #74279, #74820, #14882, #15428, #6497 ),
 ( #108966, #59130, #101631, #24920, #8138, #32253, #93252, #76457, #110611, #66433, #25481, #17060 ) ),
 .UNSPECIFIED., .F., .F., .F.,
 ( 6, 3, 3, 3, 6 ),
 ( 6, 3, 3, 6 ),
 ( 1.933760562350000045, 17.84603210599999912, 29.17820978809999843, 40.51038747020000130, 63.41552668279999949 ),
 ( 84.36360869960000741, 126.5454130579999941, 147.6363152340000227, 168.7272174100000086 ),
 .UNSPECIFIED. ) ;
#75828 = ORIENTED_EDGE ( 'NONE', *, *, #10386, .T. ) ;
#75829 = CARTESIAN_POINT ( 'NONE',  ( -15.46700379407589843, 1461.188231737419756, 228.6959062608830209 ) ) ;
#75830 = CARTESIAN_POINT ( 'NONE',  ( 3.500000000000000000, 1422.625370988529994, 168.5578661042980286 ) ) ;
#75831 = CARTESIAN_POINT ( 'NONE',  ( -28.76039927569999932, 1375.228231664269970, 215.0392276715589901 ) ) ;
#75832 = EDGE_CURVE ( 'NONE', #5115, #89576, #58096, .T. ) ;
#75833 = ORIENTED_EDGE ( 'NONE', *, *, #91235, .F. ) ;
#75834 = CARTESIAN_POINT ( 'NONE',  ( -4.623788007495000407, 1516.947419719950176, 205.6726967363569827 ) ) ;
#75835 = ORIENTED_EDGE ( 'NONE', *, *, #70025, .T. ) ;
#75836 = CARTESIAN_POINT ( 'NONE',  ( -105.3710641919550000, 1378.843319234500086, 304.5215261602800183 ) ) ;
#75837 = CARTESIAN_POINT ( 'NONE',  ( -18.70459389479999857, 1509.566239199129996, 231.7064163551980016 ) ) ;
#75838 = EDGE_CURVE ( 'NONE', #92224, #62492, #14281, .T. ) ;
#75839 = CARTESIAN_POINT ( 'NONE',  ( -5.839839396159999474, 1410.494359662829993, 187.1215865486979908 ) ) ;
#75840 = CARTESIAN_POINT ( 'NONE',  ( 7.719525595194999923, 1513.939092156100060, 216.2221105575569879 ) ) ;
#75842 = EDGE_LOOP ( 'NONE', ( #108153, #48802, #41548, #61801, #66936 ) ) ;
#75841 = CARTESIAN_POINT ( 'NONE',  ( 0.3622025831177250188, 1416.825783990419950, 227.1772706819449752 ) ) ;
#75843 = CARTESIAN_POINT ( 'NONE',  ( 20.55965903059999889, 1427.339473409130051, 220.5198651377980070 ) ) ;
#75844 = CARTESIAN_POINT ( 'NONE',  ( -15.13199540178550073, 1508.551704408389924, 210.3648847345600075 ) ) ;
#75845 = CARTESIAN_POINT ( 'NONE',  ( -109.9987472809999929, 1384.304072719160104, 311.2333125242590199 ) ) ;
#75846 = CARTESIAN_POINT ( 'NONE',  ( -173.8335085727399871, 1526.382868172863937, 100.8557906292094373 ) ) ;
#75847 = CARTESIAN_POINT ( 'NONE',  ( 2.877113070465000089, 1516.697242742309982, 214.1184881303969973 ) ) ;
#75848 = CARTESIAN_POINT ( 'NONE',  ( 22.71938917269999791, 1409.706427035829847, 209.1785880919549925 ) ) ;
#75849 = CARTESIAN_POINT ( 'NONE',  ( -20.70499093180000116, 1508.886810853430006, 189.6386861211979920 ) ) ;
#75850 = CARTESIAN_POINT ( 'NONE',  ( 6.120119194504639815, 1508.729257029040127, 216.5649251008960050 ) ) ;
#75851 = CARTESIAN_POINT ( 'NONE',  ( 6.563595869685000750, 1517.154223579619838, 211.4114704024570131 ) ) ;
#75852 = CARTESIAN_POINT ( 'NONE',  ( -21.44521871417750702, 1525.343710797494396, 233.4338460867892877 ) ) ;
#75853 = CARTESIAN_POINT ( 'NONE',  ( -20.86254339170000094, 1504.682062816289999, 214.2159060785090219 ) ) ;
#75854 = CARTESIAN_POINT ( 'NONE',  ( 1.232505279462991599, 1409.632634667178309, 232.4911126170792386 ) ) ;
#75856 = ORIENTED_EDGE ( 'NONE', *, *, #40020, .T. ) ;
#75855 = CARTESIAN_POINT ( 'NONE',  ( -60.19932042489999446, 1388.230348997210058, 279.3978214739589703 ) ) ;
#75857 = CARTESIAN_POINT ( 'NONE',  ( -51.53876818608200239, 1385.112767378740045, 264.8854167730279414 ) ) ;
#75858 = CARTESIAN_POINT ( 'NONE',  ( 6.248998597759999996, 1472.348800618430005, 259.9484879023979715 ) ) ;
#75859 = CARTESIAN_POINT ( 'NONE',  ( 11.78824854703250047, 1522.051704408389924, 211.4132493584619965 ) ) ;
#75860 = CARTESIAN_POINT ( 'NONE',  ( -1.122592899216370017E-16, 1388.079727053959914, 209.1218459616989946 ) ) ;
#75861 = DIRECTION ( 'NONE',  ( 0.000000000000000000, 0.000000000000000000, 1.000000000000000000 ) ) ;
#75862 = CARTESIAN_POINT ( 'NONE',  ( -4.932889665030000259, 1462.240114355689911, 204.2595497230389867 ) ) ;
#75863 = CARTESIAN_POINT ( 'NONE',  ( 1.082466572113199854, 1452.866867491690073, 183.3918909070579844 ) ) ;
#75864 = CIRCLE ( 'NONE', #27584, 0.9999999999999135136 ) ;
#75866 = CARTESIAN_POINT ( 'NONE',  ( -8.580993339069999948, 1384.885542790459795, 218.6696210660190047 ) ) ;
#75865 = CARTESIAN_POINT ( 'NONE',  ( -7.717505791104999346, 1516.857914730730045, 216.8393517232070167 ) ) ;
#75867 = CARTESIAN_POINT ( 'NONE',  ( -9.568540505426021525, 1448.523985602899984, 209.1776060292260127 ) ) ;
#75868 = CARTESIAN_POINT ( 'NONE',  ( -106.6282499509799919, 1381.613467129139963, 309.5665933865749935 ) ) ;
#75869 = ORIENTED_EDGE ( 'NONE', *, *, #74939, .F. ) ;
#75870 = CARTESIAN_POINT ( 'NONE',  ( -3.455378015385000001, 1516.627618683580067, 202.1863880069169852 ) ) ;
#75871 = FACE_OUTER_BOUND ( 'NONE', #93283, .T. ) ;
#75872 = AXIS2_PLACEMENT_3D ( 'NONE', #5505, #67090, #6055 ) ;
#75873 = CARTESIAN_POINT ( 'NONE',  ( 12.64331018290000053, 1422.763132344930227, 223.6605244860979838 ) ) ;
#75874 =( BOUNDED_SURFACE ( )  B_SPLINE_SURFACE ( 3, 2, ( 
 ( #21509, #47295, #20965 ),
 ( #64117, #48413, #71984 ),
 ( #90940, #90377, #107195 ),
 ( #81419, #63040, #12035 ) ),
 .UNSPECIFIED., .F., .F., .F. ) 
 B_SPLINE_SURFACE_WITH_KNOTS ( ( 4, 4 ),
 ( 3, 3 ),
 ( 0.000000000000000000, 0.0002960034161023842973 ),
 ( 0.000000000000000000, 1.000000000000000000 ),
 .UNSPECIFIED. ) 
 GEOMETRIC_REPRESENTATION_ITEM ( )  RATIONAL_B_SPLINE_SURFACE ( (
 ( 1.000000000000000000, 0.8072480644198088973, 1.000000000000000000),
 ( 1.000000000000000000, 0.8072480346917575433, 1.000000000000000000),
 ( 1.000000000000000000, 0.8071723757218559614, 1.000000000000000000),
 ( 1.000000000000000000, 0.8070209408749943192, 1.000000000000000000) ) ) 
 REPRESENTATION_ITEM ( '' )  SURFACE ( )  );
#75875 = CARTESIAN_POINT ( 'NONE',  ( 1.999999980934999977, 1517.051704408389924, 195.7913026028670060 ) ) ;
#75876 = DIRECTION ( 'NONE',  ( 0.000000000000000000, 1.000000000000000000, 0.000000000000000000 ) ) ;
#75877 = CARTESIAN_POINT ( 'NONE',  ( 4.647692645760000296, 1467.200465493689990, 217.9234193686490073 ) ) ;
#75878 = CARTESIAN_POINT ( 'NONE',  ( -17.16388877745089303, 1523.678648413191695, 179.6262614458747464 ) ) ;
#75879 = CARTESIAN_POINT ( 'NONE',  ( 27.59657656778820112, 1436.356223077960067, 136.7068084802659769 ) ) ;
#75880 = CARTESIAN_POINT ( 'NONE',  ( 39.68989170827939716, 1446.546521785269988, 136.7137753855650146 ) ) ;
#75881 = CARTESIAN_POINT ( 'NONE',  ( 19.72497240319906453, 1506.501081259675175, 218.9625358929377228 ) ) ;
#75882 = CARTESIAN_POINT ( 'NONE',  ( -31.92678845819044753, 1465.333974304449157, 269.3172746343190056 ) ) ;
#75883 = CARTESIAN_POINT ( 'NONE',  ( -109.0477392060000028, 1386.067204197109959, 297.2757566815589598 ) ) ;
#75884 = CARTESIAN_POINT ( 'NONE',  ( 13.71041708839999984, 1507.516673751029884, 185.7221359422979958 ) ) ;
#75885 = CARTESIAN_POINT ( 'NONE',  ( -21.48648064083822362, 1524.477587234266139, 184.1567740173552465 ) ) ;
#75886 = CARTESIAN_POINT ( 'NONE',  ( -38.72028640208406358, 1452.776172727556059, 269.5884039666330523 ) ) ;
#75887 = ORIENTED_EDGE ( 'NONE', *, *, #98052, .F. ) ;
#75888 = CARTESIAN_POINT ( 'NONE',  ( -25.74682230153359797, 1470.140385610140129, 210.8607376181039683 ) ) ;
#75889 = CARTESIAN_POINT ( 'NONE',  ( 8.899872388108134302, 1506.575640307498816, 188.8910645225604128 ) ) ;
#75890 = CARTESIAN_POINT ( 'NONE',  ( -4.556911026691660815, 1508.729442836390035, 212.9448241954719947 ) ) ;
#75891 = CARTESIAN_POINT ( 'NONE',  ( 7.878537825433329367, 1517.151704408390060, 200.0586249522280013 ) ) ;
#75892 = CARTESIAN_POINT ( 'NONE',  ( 11.60004869885203327, 1427.574042486475491, 134.2792576386086694 ) ) ;
#75893 = CARTESIAN_POINT ( 'NONE',  ( 19.47367602328466774, 1455.619968770807645, 226.0154353848046469 ) ) ;
#75894 = CARTESIAN_POINT ( 'NONE',  ( -9.982373020641928107, 1439.278825435209910, 208.9079553162600007 ) ) ;
#75895 = CARTESIAN_POINT ( 'NONE',  ( -3.983717799079939503, 1515.551844914359890, 211.4517850765819844 ) ) ;
#75896 = CARTESIAN_POINT ( 'NONE',  ( -10.29038504730294079, 1418.125687189650080, 229.8187361617479496 ) ) ;
#75897 = CARTESIAN_POINT ( 'NONE',  ( -6.735029543969123900, 1451.432364504263887, 153.2907587394053337 ) ) ;
#75898 = CARTESIAN_POINT ( 'NONE',  ( 3.829620113920000346, 1515.551704408389924, 211.4519800804890224 ) ) ;
#75899 = CARTESIAN_POINT ( 'NONE',  ( 25.67235157149999836, 1436.336280272470049, 137.0204247850980153 ) ) ;
#75900 = CARTESIAN_POINT ( 'NONE',  ( -12.66129559865252041, 1442.799074774669862, 169.4635015124096071 ) ) ;
#75901 = VERTEX_POINT ( 'NONE', #12419 ) ;
#75902 = CARTESIAN_POINT ( 'NONE',  ( 0.2892576526144139959, 1415.943166310999914, 191.0435026498350055 ) ) ;
#75903 = CARTESIAN_POINT ( 'NONE',  ( 21.33887654814517632, 1508.922069170062969, 226.3421127776584285 ) ) ;
#75904 = ORIENTED_EDGE ( 'NONE', *, *, #99903, .T. ) ;
#75905 = ORIENTED_EDGE ( 'NONE', *, *, #54202, .F. ) ;
#75906 = CARTESIAN_POINT ( 'NONE',  ( 12.53380665967529950, 1445.052233242549846, 186.0874955919830143 ) ) ;
#75907 = CARTESIAN_POINT ( 'NONE',  ( 4.623921183531392920, 1516.955031447278543, 203.1162470316040185 ) ) ;
#75909 = CARTESIAN_POINT ( 'NONE',  ( -4.375233889810000498, 1463.532726167829878, 231.7907868280979926 ) ) ;
#75908 = CARTESIAN_POINT ( 'NONE',  ( 3.001031723810000162, 1456.247125019289797, 219.3218834261989798 ) ) ;
#75910 = CARTESIAN_POINT ( 'NONE',  ( -8.051936654369999502, 1448.101386734190100, 213.6171964053189924 ) ) ;
#75911 = CARTESIAN_POINT ( 'NONE',  ( 4.228620053163889558, 1425.167187284519969, 185.3096231440469808 ) ) ;
#75912 = CARTESIAN_POINT ( 'NONE',  ( -12.30069474339200042, 1378.346207744910089, 209.9425806866760240 ) ) ;
#75913 = CARTESIAN_POINT ( 'NONE',  ( -2.542765869541859569, 1420.835077523395967, 185.4948760842592606 ) ) ;
#75914 = CARTESIAN_POINT ( 'NONE',  ( 7.005078520870000602, 1424.882473908839984, 213.2032269817289887 ) ) ;
#75915 = CARTESIAN_POINT ( 'NONE',  ( -14.66856476219100891, 1429.940063103053717, 222.0536632632462215 ) ) ;
#75916 = FACE_BOUND ( 'NONE', #88426, .T. ) ;
#75917 = CARTESIAN_POINT ( 'NONE',  ( 1.111971660999999889, 1450.991721771130187, 182.4208345951979879 ) ) ;
#75918 = CARTESIAN_POINT ( 'NONE',  ( 8.505021145809154248, 1364.171015757792247, 210.6218459617142003 ) ) ;
#75919 = FACE_OUTER_BOUND ( 'NONE', #8150, .T. ) ;
#75921 = ORIENTED_EDGE ( 'NONE', *, *, #105133, .F. ) ;
#75920 = CARTESIAN_POINT ( 'NONE',  ( -2.708169622750910029E-09, 1414.562637300989763, 245.8823571257100014 ) ) ;
#75922 = ORIENTED_EDGE ( 'NONE', *, *, #11350, .T. ) ;
#75923 = CARTESIAN_POINT ( 'NONE',  ( -11.80278639884820002, 1428.367824666609977, 148.3230517217830027 ) ) ;
#75924 = CARTESIAN_POINT ( 'NONE',  ( 7.535878249002015750, 1510.580107397280244, 203.3037915669708013 ) ) ;
#75925 = CARTESIAN_POINT ( 'NONE',  ( -4.301461581549999913, 1474.025770959829970, 270.1336327149980434 ) ) ;
#75926 = CARTESIAN_POINT ( 'NONE',  ( -110.0628941928870006, 1384.909579410989863, 296.9513031325649877 ) ) ;
#75927 = CARTESIAN_POINT ( 'NONE',  ( -103.2058326176597376, 1331.448250124730066, 321.4071368064087437 ) ) ;
#75928 = CARTESIAN_POINT ( 'NONE',  ( 1.689251544526354731, 1526.344110814221267, 239.7716210576236904 ) ) ;
#75929 = CARTESIAN_POINT ( 'NONE',  ( -7.964281638630000160, 1384.840201205250196, 199.4899964382389896 ) ) ;
#75930 = DIRECTION ( 'NONE',  ( 0.000000000000000000, -1.000000000000000000, 0.000000000000000000 ) ) ;
#75931 = CARTESIAN_POINT ( 'NONE',  ( 38.63560632403650175, 1444.097728697520097, 137.1726987354860228 ) ) ;
#75932 = CARTESIAN_POINT ( 'NONE',  ( 7.445922712503920238, 1367.935115748522094, 210.6218459616991936 ) ) ;
#75933 = CARTESIAN_POINT ( 'NONE',  ( -9.103497831145899610, 1449.500276181969866, 210.3008157486750065 ) ) ;
#75934 = CARTESIAN_POINT ( 'NONE',  ( -20.41013681796389889, 1410.032071447750013, 269.3516173646369793 ) ) ;
#75935 = CARTESIAN_POINT ( 'NONE',  ( -13.39296744828000030, 1434.924871481009859, 148.8778569621510144 ) ) ;
#75936 = ORIENTED_EDGE ( 'NONE', *, *, #11837, .F. ) ;
#75937 = CARTESIAN_POINT ( 'NONE',  ( 2.038646110889675178, 1525.960063244516959, 241.1857569150893994 ) ) ;
#75938 = B_SPLINE_SURFACE_WITH_KNOTS ( 'NONE', 4, 5, ( 
 ( #48708, #58746, #33512, #90677, #82831, #23475 ),
 ( #6123, #57668, #75010, #109160, #100723, #24006 ),
 ( #92329, #68826, #27342, #52566, #44163, #86699 ),
 ( #9993, #77214, #52009, #26228, #78300, #2181 ),
 ( #34087, #94534, #18371, #1614, #110794, #35751 ) ),
 .UNSPECIFIED., .F., .F., .F.,
 ( 5, 5 ),
 ( 6, 6 ),
 ( 7.049146647299999735, 7.791777982190000174 ),
 ( 0.000000000000000000, 2.000000000000000000 ),
 .UNSPECIFIED. ) ;
#75939 = VECTOR ( 'NONE', #107370, 1000.000000000000000 ) ;
#75940 = ORIENTED_EDGE ( 'NONE', *, *, #65076, .T. ) ;
#75941 = ORIENTED_EDGE ( 'NONE', *, *, #6990, .T. ) ;
#75942 = CARTESIAN_POINT ( 'NONE',  ( 4.827146942024284293, 1422.311623617143596, 184.2770325824816666 ) ) ;
#75943 = CARTESIAN_POINT ( 'NONE',  ( -10.32735784461773498, 1512.913060387330006, 184.1749888460368538 ) ) ;
#75944 = AXIS2_PLACEMENT_3D ( 'NONE', #62966, #45591, #89217 ) ;
#75945 = CARTESIAN_POINT ( 'NONE',  ( -1.119717754394999876, 1517.038650117239968, 212.5846815975970117 ) ) ;
#75946 = CARTESIAN_POINT ( 'NONE',  ( -18.93280221739999902, 1485.490082012730227, 189.5191571945979945 ) ) ;
#75947 = AXIS2_PLACEMENT_3D ( 'NONE', #38960, #73138, #107280 ) ;
#75948 = CARTESIAN_POINT ( 'NONE',  ( -17.38692480600779788, 1507.629789030409938, 229.8496573937590028 ) ) ;
#75949 = B_SPLINE_SURFACE_WITH_KNOTS ( 'NONE', 5, 1, ( 
 ( #33036, #31387 ),
 ( #49862, #22970 ),
 ( #32506, #75622 ),
 ( #57727, #84547 ),
 ( #66676, #92385 ),
 ( #100255, #100781 ),
 ( #39238, #91299 ),
 ( #24072, #14582 ),
 ( #40340, #74521 ),
 ( #108652, #58264 ),
 ( #83996, #7296 ),
 ( #101322, #31939 ),
 ( #24612, #66133 ),
 ( #23535, #58807 ),
 ( #92947, #73413 ),
 ( #107549, #30836 ),
 ( #94046, #68334 ),
 ( #1672, #15 ),
 ( #95714, #102989 ),
 ( #61581, #33577 ),
 ( #95166, #86760 ),
 ( #18422, #77813 ),
 ( #67769, #34696 ),
 ( #9494, #86203 ),
 ( #77272, #35252 ),
 ( #110301, #101882 ),
 ( #1122, #51507 ),
 ( #60476, #16759 ),
 ( #59377, #69437 ),
 ( #25173, #570 ),
 ( #85639, #52070 ),
 ( #18979, #61042 ),
 ( #68888, #10048 ),
 ( #102441, #93489 ),
 ( #8382, #52622 ),
 ( #94594, #50963 ),
 ( #25727, #53176 ),
 ( #42550, #44221 ),
 ( #42005, #34149 ),
 ( #7837, #76154 ),
 ( #85090, #17872 ),
 ( #76702, #69996 ),
 ( #78364, #8939 ),
 ( #59928, #17312 ),
 ( #35813, #43113 ),
 ( #26287, #103552 ),
 ( #26855, #43661 ),
 ( #104110, #27398 ),
 ( #21728, #80571 ),
 ( #29600, #63786 ),
 ( #63252, #88958 ) ),
 .UNSPECIFIED., .F., .F., .F.,
 ( 6, 3, 3, 3, 3, 3, 3, 3, 3, 3, 3, 3, 3, 3, 3, 3, 6 ),
 ( 2, 2 ),
 ( 0.000000000000000000, 28.69702819429999963, 61.04778752440000034, 93.62768910810000023, 123.7336603250000024, 156.1762685979999787, 187.3272846180000215, 220.4669312460000015, 237.3878297990000021, 254.2938300590000154, 289.2398204710000300, 325.3030936050000150, 360.8626869010000178, 395.8828220460000011, 432.6128460950000090, 468.8934854820000169, 502.1482307969999965 ),
 ( -3.370352201716179583E-07, 2.001701706146989945 ),
 .UNSPECIFIED. ) ;
#75950 = ORIENTED_EDGE ( 'NONE', *, *, #90698, .F. ) ;
#75951 = CARTESIAN_POINT ( 'NONE',  ( -28.77730029287999969, 1509.917985857419808, 212.2396942430650029 ) ) ;
#75952 = CARTESIAN_POINT ( 'NONE',  ( -7.719392420504999741, 1516.929962200689943, 202.5670673984569703 ) ) ;
#75953 = CARTESIAN_POINT ( 'NONE',  ( -29.71730757640000320, 1509.987350256529908, 208.1891636974079915 ) ) ;
#75954 = B_SPLINE_SURFACE_WITH_KNOTS ( 'NONE', 5, 5, ( 
 ( #100539, #48512, #99983, #103146, #31131, #109507 ),
 ( #22704, #101077, #66967, #23274, #108956, #58011 ),
 ( #82651, #85810, #82084, #92147, #99426, #75368 ),
 ( #9108, #66424, #65314, #56902, #32783, #57471 ),
 ( #32243, #5387, #83199, #24376, #23819, #91035 ),
 ( #5943, #83743, #40088, #40639, #108398, #74811 ) ),
 .UNSPECIFIED., .F., .F., .F.,
 ( 6, 6 ),
 ( 6, 6 ),
 ( 8.936092213160000242, 11.91340804030000022 ),
 ( 0.000000000000000000, 1.442075847869999983 ),
 .UNSPECIFIED. ) ;
#75955 = CARTESIAN_POINT ( 'NONE',  ( 2.370970874524634286, 1427.002265528474027, 134.0999999980980135 ) ) ;
#75956 = CARTESIAN_POINT ( 'NONE',  ( -44.14995057972470249, 1384.596438297579880, 217.3237505064830088 ) ) ;
#75957 = CARTESIAN_POINT ( 'NONE',  ( -2.599869711270000217, 1407.016598365429900, 196.2843278663980016 ) ) ;
#75958 = CARTESIAN_POINT ( 'NONE',  ( -12.14658859679999914, 1409.337228609230124, 227.1535549678980317 ) ) ;
#75960 = VERTEX_POINT ( 'NONE', #37629 ) ;
#75959 = CARTESIAN_POINT ( 'NONE',  ( 30.01999388067563146, 1525.848198008145346, 197.1136717113790553 ) ) ;
#75961 = CARTESIAN_POINT ( 'NONE',  ( -27.47792036623960144, 1488.737008339370050, 209.1940319314329884 ) ) ;
#75962 = CARTESIAN_POINT ( 'NONE',  ( 26.39526639180000345, 1469.246565959629834, 210.4302785482780109 ) ) ;
#75963 = CARTESIAN_POINT ( 'NONE',  ( -16.16124070225407294, 1379.595261704359018, 212.2433978542155444 ) ) ;
#75964 = CARTESIAN_POINT ( 'NONE',  ( 10.45057174002269917, 1460.060802511540032, 206.0227405347829972 ) ) ;
#75965 = CARTESIAN_POINT ( 'NONE',  ( -24.09633375880000017, 1435.413152144519927, 137.5044708534980202 ) ) ;
#75966 = CARTESIAN_POINT ( 'NONE',  ( -24.32956343839999747, 1442.099522796889914, 211.7759529297080121 ) ) ;
#75967 = CARTESIAN_POINT ( 'NONE',  ( -6.933616859135000254, 1516.548716157039962, 211.4141532006069895 ) ) ;
#75968 = CARTESIAN_POINT ( 'NONE',  ( -68.31895350100000996, 1379.747064260159959, 279.0929441650590093 ) ) ;
#75969 = CARTESIAN_POINT ( 'NONE',  ( -0.01304300961527469875, 1452.999749643619907, 183.2385070609109903 ) ) ;
#75970 = CARTESIAN_POINT ( 'NONE',  ( -14.54088437389999910, 1410.754219534529966, 226.7644051071980016 ) ) ;
#75971 = CARTESIAN_POINT ( 'NONE',  ( 3.397541313661426976, 1440.732790238158714, 156.8344482731262133 ) ) ;
#75972 = CARTESIAN_POINT ( 'NONE',  ( -5.786847777804999815, 1517.104497701820037, 208.3841784293060186 ) ) ;
#75973 = VERTEX_POINT ( 'NONE', #19143 ) ;
#75974 = DIRECTION ( 'NONE',  ( 0.8771707529346988164, 0.03063147765598519048, -0.4792005663316608599 ) ) ;
#75975 = CARTESIAN_POINT ( 'NONE',  ( -11.37631282269999922, 1471.001977454990083, 208.1230460654030026 ) ) ;
#75976 = CARTESIAN_POINT ( 'NONE',  ( -1.381610875089999979E-15, 1384.913060387289988, 218.6218459572590120 ) ) ;
#75977 = ORIENTED_EDGE ( 'NONE', *, *, #20324, .T. ) ;
#75978 = CARTESIAN_POINT ( 'NONE',  ( -18.86688640473621703, 1512.187213306747481, 180.7825021045441076 ) ) ;
#75979 = CARTESIAN_POINT ( 'NONE',  ( 12.82065956846409804, 1434.792185812719936, 149.9145850215789721 ) ) ;
#75980 = CARTESIAN_POINT ( 'NONE',  ( -4.086192991946269615, 1440.407209789042327, 185.3182923436035026 ) ) ;
#75981 = AXIS2_PLACEMENT_3D ( 'NONE', #66622, #24559, #110240 ) ;
#75982 = CARTESIAN_POINT ( 'NONE',  ( -4.284542764180000241, 1413.032915330810056, 207.8185126793489985 ) ) ;
#75983 = CARTESIAN_POINT ( 'NONE',  ( 11.80119706069999985, 1415.163755984229965, 222.4114065333980079 ) ) ;
#75984 = CARTESIAN_POINT ( 'NONE',  ( 4.037057355369999101, 1486.123908481589979, 199.1211976137989836 ) ) ;
#75985 = CARTESIAN_POINT ( 'NONE',  ( -18.13594796521936559, 1507.809373629487709, 187.1116949291995013 ) ) ;
#75986 = DIRECTION ( 'NONE',  ( 0.000000000000000000, 1.000000000000000000, 0.000000000000000000 ) ) ;
#75987 = ADVANCED_FACE ( 'NONE', ( #104284 ), #19591, .F. ) ;
#75989 = CARTESIAN_POINT ( 'NONE',  ( 39.14754387628220655, 1437.687579064466945, 135.1140641504456426 ) ) ;
#75988 = CARTESIAN_POINT ( 'NONE',  ( -3.449149233875000053, 1516.947419719950176, 213.7456339395970133 ) ) ;
#75990 = CARTESIAN_POINT ( 'NONE',  ( 20.67559640589999859, 1509.531575910530137, 188.3714930344980019 ) ) ;
#75991 = CARTESIAN_POINT ( 'NONE',  ( 7.330554133425000174, 1516.857992118400034, 216.4511490482170188 ) ) ;
#75992 = ORIENTED_EDGE ( 'NONE', *, *, #97271, .F. ) ;
#75993 = CARTESIAN_POINT ( 'NONE',  ( -12.78667974309999877, 1416.822694190629818, 195.3262915446979946 ) ) ;
#75994 = CARTESIAN_POINT ( 'NONE',  ( -16.79954545500000052, 1420.446322000240116, 203.4828821667790066 ) ) ;
#75995 = CARTESIAN_POINT ( 'NONE',  ( -17.60942431520539841, 1508.551704408389924, 211.7095227962340118 ) ) ;
#75996 = DIRECTION ( 'NONE',  ( 0.000000000000000000, 1.000000000000000000, 0.000000000000000000 ) ) ;
#75998 = B_SPLINE_CURVE_WITH_KNOTS ( 'NONE', 5,
 ( #28015, #37523, #55443, #64397, #53810, #106377 ),
 .UNSPECIFIED., .F., .F.,
 ( 6, 6 ),
 ( 297.6813684100000046, 302.5784080160000258 ),
 .UNSPECIFIED. ) ;
#75997 = DIRECTION ( 'NONE',  ( 0.000000000000000000, 1.000000000000000000, 0.000000000000000000 ) ) ;
#75999 = CARTESIAN_POINT ( 'NONE',  ( 17.69507376911758101, 1519.551704408389924, 202.0148427141579361 ) ) ;
#76000 = CARTESIAN_POINT ( 'NONE',  ( -4.145978979534980458E-15, 1375.413060387289988, 209.1218459572589836 ) ) ;
#76001 = CARTESIAN_POINT ( 'NONE',  ( -6.821413868843755779, 1508.365261329358646, 219.8335085021152224 ) ) ;
#76002 = DIRECTION ( 'NONE',  ( 0.9455185755993178454, 0.000000000000000000, -0.3255681544571537578 ) ) ;
#76003 = CARTESIAN_POINT ( 'NONE',  ( 18.14860257456183845, 1425.108924779807012, 224.7878952339535488 ) ) ;
#76004 = CARTESIAN_POINT ( 'NONE',  ( -9.771922359260001301, 1440.444625599219989, 148.8200729295979841 ) ) ;
#76005 = CARTESIAN_POINT ( 'NONE',  ( 37.77835552715119860, 1440.913060384539904, 255.9250353463820034 ) ) ;
#76007 = CARTESIAN_POINT ( 'NONE',  ( -16.06428792994629973, 1414.913060387329779, 209.3174441339999987 ) ) ;
#76006 = CARTESIAN_POINT ( 'NONE',  ( -13.10445383010389975, 1418.121923837399891, 200.6546514748530115 ) ) ;
#76008 = CARTESIAN_POINT ( 'NONE',  ( -2.253566441613126910E-10, 1426.918876941764893, 137.0999999980980135 ) ) ;
#76009 = ORIENTED_EDGE ( 'NONE', *, *, #23098, .F. ) ;
#76010 = ORIENTED_EDGE ( 'NONE', *, *, #27478, .T. ) ;
#76011 = CARTESIAN_POINT ( 'NONE',  ( 28.44698416550310327, 1526.373507135059072, 219.8751933407330341 ) ) ;
#76012 = CARTESIAN_POINT ( 'NONE',  ( -4.144683537393576422, 1507.117986068643631, 231.4540176283237543 ) ) ;
#76013 = CARTESIAN_POINT ( 'NONE',  ( -24.38138866919999970, 1442.062446048410038, 212.1316646185979948 ) ) ;
#76014 = CARTESIAN_POINT ( 'NONE',  ( 0.5133626083067620582, 1410.311097044259895, 185.0719925509139898 ) ) ;
#76015 = DIRECTION ( 'NONE',  ( 0.000000000000000000, 0.000000000000000000, -1.000000000000000000 ) ) ;
#76016 = CARTESIAN_POINT ( 'NONE',  ( 27.60404634758340947, 1509.989021275989899, 220.8700857203302519 ) ) ;
#76017 = CARTESIAN_POINT ( 'NONE',  ( -1.840383241931389913, 1487.831799196779912, 219.8181463656999881 ) ) ;
#76019 = EDGE_CURVE ( 'NONE', #99467, #107075, #91335, .T. ) ;
#76018 = CARTESIAN_POINT ( 'NONE',  ( -4.324092172210000307, 1515.269353063089966, 208.7601266040480255 ) ) ;
#76020 = CARTESIAN_POINT ( 'NONE',  ( -71.04079330152269733, 1383.784253855209954, 295.9543559495810428 ) ) ;
#76021 = EDGE_CURVE ( 'NONE', #8596, #4497, #64647, .T. ) ;
#76022 = CIRCLE ( 'NONE', #20609, 1.000000000000000000 ) ;
#76023 = ADVANCED_FACE ( 'NONE', ( #57763 ), #44695, .F. ) ;
#76024 = CARTESIAN_POINT ( 'NONE',  ( 10.67630109080000089, 1452.395781299630244, 151.6471186536979872 ) ) ;
#76025 = CARTESIAN_POINT ( 'NONE',  ( 4.780307568339999591, 1467.625956517089890, 217.8721402715589761 ) ) ;
#76026 = CARTESIAN_POINT ( 'NONE',  ( 11.10832711078520063, 1491.515140723940021, 210.2565573149119871 ) ) ;
#76027 = ADVANCED_FACE ( 'NONE', ( #40374 ), #23153, .F. ) ;
#76029 = ORIENTED_EDGE ( 'NONE', *, *, #6253, .F. ) ;
#76028 = CARTESIAN_POINT ( 'NONE',  ( -2.695638927469999668, 1457.674280517889883, 219.0325817157390134 ) ) ;
#76030 = CARTESIAN_POINT ( 'NONE',  ( -1.438892182569999845, 1452.191226611430011, 183.8587016213980121 ) ) ;
#76031 = B_SPLINE_SURFACE_WITH_KNOTS ( 'NONE', 2, 5, ( 
 ( #85511, #60913, #103984, #8807, #44654, #59796 ),
 ( #77148, #86630, #1000, #103416, #26722, #18310 ),
 ( #452, #69867, #9924, #44095, #35678, #61463 ) ),
 .UNSPECIFIED., .F., .F., .F.,
 ( 3, 3 ),
 ( 6, 6 ),
 ( 1.399803019509999968, 2.016961153540000051 ),
 ( 0.000000000000000000, 1.000000000000000000 ),
 .UNSPECIFIED. ) ;
#76032 = CARTESIAN_POINT ( 'NONE',  ( -33.74298654390000252, 1380.921279986640229, 228.6690588220590143 ) ) ;
#76033 = EDGE_CURVE ( 'NONE', #50772, #65089, #16585, .T. ) ;
#76034 = CARTESIAN_POINT ( 'NONE',  ( 8.120708804965499183, 1436.294995401849974, 206.2774205879739782 ) ) ;
#76035 = VERTEX_POINT ( 'NONE', #8976 ) ;
#76036 = ORIENTED_EDGE ( 'NONE', *, *, #7436, .T. ) ;
#76037 = B_SPLINE_CURVE_WITH_KNOTS ( 'NONE', 5,
 ( #28315, #79833, #55194, #46795, #96064, #104461 ),
 .UNSPECIFIED., .F., .F.,
 ( 6, 6 ),
 ( -2.000000000000000000, 0.000000000000000000 ),
 .UNSPECIFIED. ) ;
#76038 = EDGE_CURVE ( 'NONE', #22289, #16677, #32122, .T. ) ;
#76039 = CARTESIAN_POINT ( 'NONE',  ( 13.88129723608619948, 1507.515551148199847, 232.8168547917639728 ) ) ;
#76040 = CARTESIAN_POINT ( 'NONE',  ( -8.200764929360001787, 1500.840159096690059, 209.4951459900700286 ) ) ;
#76041 = CARTESIAN_POINT ( 'NONE',  ( 39.82865069103799982, 1441.236877534039877, 136.8517713851130111 ) ) ;
#76043 = DIRECTION ( 'NONE',  ( -0.000000000000000000, -1.000000000000000000, -0.000000000000000000 ) ) ;
#76042 = CARTESIAN_POINT ( 'NONE',  ( -11.81135191919999983, 1436.410413307749877, 147.6956600043980075 ) ) ;
#76044 = CARTESIAN_POINT ( 'NONE',  ( 11.77666586973660046, 1479.544451823169993, 209.3554088579860206 ) ) ;
#76045 = CARTESIAN_POINT ( 'NONE',  ( -104.2862556689999991, 1379.876065007149919, 302.9147207968590578 ) ) ;
#76046 = CARTESIAN_POINT ( 'NONE',  ( -113.4000000000000057, 1306.413060387289988, 304.2218459572590064 ) ) ;
#76047 = CYLINDRICAL_SURFACE ( 'NONE', #91032, 2.458500000000005237 ) ;
#76048 = LINE ( 'NONE', #82785, #56766 ) ;
#76049 = FACE_OUTER_BOUND ( 'NONE', #86107, .T. ) ;
#76050 = CARTESIAN_POINT ( 'NONE',  ( 3.378643529439999682, 1409.031045219230009, 187.3370713307979827 ) ) ;
#76051 = CARTESIAN_POINT ( 'NONE',  ( 2.968366584736970015, 1486.970885391709999, 197.5475828882330234 ) ) ;
#76052 = CARTESIAN_POINT ( 'NONE',  ( 7.040216406195790810, 1434.373471180939987, 203.9688476978490144 ) ) ;
#76053 = CARTESIAN_POINT ( 'NONE',  ( -3.137828956056770480, 1440.800072403580089, 158.1453491124979962 ) ) ;
#76054 = DIRECTION ( 'NONE',  ( 0.000000000000000000, 0.000000000000000000, -1.000000000000000000 ) ) ;
#76055 = ORIENTED_EDGE ( 'NONE', *, *, #34423, .T. ) ;
#76056 = VECTOR ( 'NONE', #56463, 1000.000000000000000 ) ;
#76057 = CARTESIAN_POINT ( 'NONE',  ( -18.28539703770000102, 1466.456797679889860, 217.8105514170289894 ) ) ;
#76059 = ADVANCED_FACE ( 'NONE', ( #85127 ), #1157, .F. ) ;
#76058 = CARTESIAN_POINT ( 'NONE',  ( -1.633469776390000128, 1432.353341358199941, 150.3624711946980028 ) ) ;
#76060 = DIRECTION ( 'NONE',  ( 0.000000000000000000, -1.836970198721029688E-16, -1.000000000000000000 ) ) ;
#76061 = DIRECTION ( 'NONE',  ( 0.9455185755993178454, 0.000000000000000000, -0.3255681544571537578 ) ) ;
#76062 = CARTESIAN_POINT ( 'NONE',  ( 15.16669330050000042, 1430.147119278929949, 190.8796077056979925 ) ) ;
#76063 = CARTESIAN_POINT ( 'NONE',  ( -1.718598421969799969E-10, 1470.598202367599924, 255.5842205547500043 ) ) ;
#76064 = CARTESIAN_POINT ( 'NONE',  ( -2.632747685671116944, 1389.413060387289988, 207.6835693458863830 ) ) ;
#76065 = CARTESIAN_POINT ( 'NONE',  ( -0.9297777941500000587, 1416.254459046630018, 227.9489298555980099 ) ) ;
#76066 = CARTESIAN_POINT ( 'NONE',  ( -23.75590350410000440, 1435.760101040910058, 211.5282110633580146 ) ) ;
#76067 = CARTESIAN_POINT ( 'NONE',  ( -3.269259737370000085, 1476.740802117289832, 199.2818558395189825 ) ) ;
#76068 = CARTESIAN_POINT ( 'NONE',  ( -107.7932546339999931, 1388.509443340949929, 309.9252778232590231 ) ) ;
#76069 = ADVANCED_FACE ( 'NONE', ( #94078 ), #68747, .T. ) ;
#76070 = VECTOR ( 'NONE', #93164, 1000.000000000000000 ) ;
#76071 = CARTESIAN_POINT ( 'NONE',  ( -0.4936889915673177698, 1485.614862604095151, 181.8905814463562365 ) ) ;
#76072 = CARTESIAN_POINT ( 'NONE',  ( -7.173827098650000345, 1361.757975858899954, 207.6218459616989946 ) ) ;
#76073 = CARTESIAN_POINT ( 'NONE',  ( -46.14792574297130301, 1439.829534759850048, 266.9721075858579979 ) ) ;
#76074 = CARTESIAN_POINT ( 'NONE',  ( 13.83038607890710203, 1509.255194850690032, 234.1910450026739738 ) ) ;
#76075 = CARTESIAN_POINT ( 'NONE',  ( -8.180909276350000425, 1424.652263318880159, 208.1606179922690103 ) ) ;
#76076 = EDGE_CURVE ( 'NONE', #37425, #104484, #47383, .T. ) ;
#76077 = CARTESIAN_POINT ( 'NONE',  ( 2.480427254505000345, 1516.872851364150165, 208.3639601402670110 ) ) ;
#76078 = CARTESIAN_POINT ( 'NONE',  ( -14.33548952289999967, 1390.363893295419984, 208.3507362592630159 ) ) ;
#76079 = B_SPLINE_SURFACE_WITH_KNOTS ( 'NONE', 5, 5, ( 
 ( #5580, #108585, #108022, #31319, #109153, #32437, #57661, #65502, #31871 ),
 ( #23998, #58194, #67707, #34081, #101816, #52557, #50359, #43598, #78291 ),
 ( #60408, #94526, #50895, #8318, #35742, #68818, #110232, #17800, #60972 ),
 ( #69929, #43050, #77207, #33506, #35185, #34634, #104042, #76094, #68274 ),
 ( #52001, #27334, #95097, #102381, #86141, #9434, #85025, #42479, #61520 ),
 ( #25110, #77749, #18363, #102919, #95648, #509, #26219, #59314, #69370 ),
 ( #84485, #93426, #25663, #1058, #103479, #7772, #86691, #9985, #41938 ),
 ( #44155, #1605, #26784, #16695, #76636, #110788, #59856, #93980, #17246 ),
 ( #51439, #8866, #85569, #62077, #21115, #88355, #46927, #55320, #63727 ),
 ( #29540, #38488, #96203, #11644, #28448, #37956, #45271, #80511, #97837 ),
 ( #63191, #19478, #89452, #72136, #97298, #62642, #3828, #3271, #2173 ),
 ( #54228, #37401, #71035, #36288, #78867, #70480, #79409, #12745, #96763 ),
 ( #71600, #105721, #12186, #106791, #72665, #30081, #104601, #20033, #45821 ),
 ( #44715, #29005, #53680, #27894, #81045, #87822, #11110, #2721, #53113 ),
 ( #46379, #4359, #36843, #64275, #79954, #88900, #20569, #105156, #54768 ),
 ( #106254, #18915, #87250, #10541, #73207, #14925, #91651, #5994, #48006 ),
 ( #82144, #55874, #107351, #49120, #30647, #92203, #66486, #83253, #6548 ),
 ( #108457, #31739, #49670, #39028, #40699, #73773, #64833, #89995, #100047 ),
 ( #21668, #100593, #15475, #74870, #13270, #7099, #90542, #23335, #22762 ),
 ( #39603, #4887, #47461, #98940, #5443, #58070, #31190, #57527, #82705 ),
 ( #109019, #75429, #41255, #109566, #22215, #65377, #99480, #65925, #81583 ) ),
 .UNSPECIFIED., .F., .F., .F.,
 ( 6, 3, 3, 3, 3, 3, 6 ),
 ( 6, 3, 6 ),
 ( 24.25933569942640133, 29.62372026779999956, 34.98808232409999874, 45.71680643680000600, 67.17425466199999562, 83.91850212199999248, 143.5761545054720045 ),
 ( -3.635447242111609987E-05, 1.000000000000000000, 2.000013395910110070 ),
 .UNSPECIFIED. ) ;
#76080 = CARTESIAN_POINT ( 'NONE',  ( -6.643844541757576216, 1470.948041183543182, 216.7502065885994682 ) ) ;
#76081 = CARTESIAN_POINT ( 'NONE',  ( 7.517250621253449339, 1425.897439506280080, 212.2678162509879769 ) ) ;
#76082 = EDGE_CURVE ( 'NONE', #64525, #68085, #109022, .T. ) ;
#76083 = CARTESIAN_POINT ( 'NONE',  ( -26.38863270286480045, 1451.975261639769997, 135.2102608963000137 ) ) ;
#76084 = EDGE_LOOP ( 'NONE', ( #108656, #2798 ) ) ;
#76085 = CARTESIAN_POINT ( 'NONE',  ( 26.67762293060000189, 1439.176105477569990, 225.6805344121979999 ) ) ;
#76087 = CARTESIAN_POINT ( 'NONE',  ( 14.96370694810000046, 1488.812149333129810, 194.0324691636979821 ) ) ;
#76086 = CARTESIAN_POINT ( 'NONE',  ( -10.93570548119130059, 1492.910398145819954, 207.3716705518500021 ) ) ;
#76088 = CARTESIAN_POINT ( 'NONE',  ( 14.45771159804956874, 1416.835807151514246, 196.8517380151662053 ) ) ;
#76089 = CARTESIAN_POINT ( 'NONE',  ( -3.061551880244241186, 1475.979329965256511, 199.2479746720524076 ) ) ;
#76090 = CARTESIAN_POINT ( 'NONE',  ( -12.61160394886860026, 1379.083170910369972, 208.5076010362149930 ) ) ;
#76091 = CARTESIAN_POINT ( 'NONE',  ( -23.21186549893350204, 1452.102484182780017, 138.3455140363329861 ) ) ;
#76092 = LINE ( 'NONE', #42477, #4255 ) ;
#76093 = ORIENTED_EDGE ( 'NONE', *, *, #82208, .F. ) ;
#76094 = CARTESIAN_POINT ( 'NONE',  ( -1.793964770197490122, 1410.263195636249975, 269.6152129905299830 ) ) ;
#76095 = CARTESIAN_POINT ( 'NONE',  ( -0.05321753368360000042, 1509.045416894829941, 239.1217103925980041 ) ) ;
#76096 = CARTESIAN_POINT ( 'NONE',  ( -7.260305637304787396, 1509.032998980356524, 215.6421396095613545 ) ) ;
#76097 = VERTEX_POINT ( 'NONE', #1709 ) ;
#76098 = ORIENTED_EDGE ( 'NONE', *, *, #110273, .T. ) ;
#76099 = CARTESIAN_POINT ( 'NONE',  ( -22.81975492585869958, 1409.709889425679876, 209.1761138208090074 ) ) ;
#76100 = ORIENTED_EDGE ( 'NONE', *, *, #45994, .T. ) ;
#76101 = CARTESIAN_POINT ( 'NONE',  ( -109.9849286017959997, 1384.913355884089924, 311.4561078401599730 ) ) ;
#76102 = CARTESIAN_POINT ( 'NONE',  ( -45.67175128301336429, 1440.701170895977839, 266.1885892358925503 ) ) ;
#76103 = CARTESIAN_POINT ( 'NONE',  ( -16.98033619447083353, 1436.324910093480185, 148.2366724938339928 ) ) ;
#76104 = CARTESIAN_POINT ( 'NONE',  ( 3.788406704206539910, 1508.728291632010041, 213.4250813669160038 ) ) ;
#76105 = CARTESIAN_POINT ( 'NONE',  ( 35.68833539314010039, 1463.121747042800052, 268.5374238623429619 ) ) ;
#76106 = CIRCLE ( 'NONE', #36708, 2.000000000000001776 ) ;
#76107 = CARTESIAN_POINT ( 'NONE',  ( -4.534001460666400085, 1508.610336687640029, 204.8848403547060002 ) ) ;
#76108 = CARTESIAN_POINT ( 'NONE',  ( -17.14314410641370046, 1422.256345865689354, 226.7315907088579650 ) ) ;
#76109 = CARTESIAN_POINT ( 'NONE',  ( -1.714334285315000095, 1516.699825673279975, 205.0952314524469955 ) ) ;
#76110 = VERTEX_POINT ( 'NONE', #11207 ) ;
#76111 = CARTESIAN_POINT ( 'NONE',  ( -11.59421085610000013, 1433.816539371060117, 151.1950375012979748 ) ) ;
#76112 = CARTESIAN_POINT ( 'NONE',  ( 15.29028524431559966, 1512.571279492550048, 195.8110339931610042 ) ) ;
#76113 = CARTESIAN_POINT ( 'NONE',  ( 22.64490784369999687, 1409.703832166029997, 208.7208416667509994 ) ) ;
#76114 = ORIENTED_EDGE ( 'NONE', *, *, #24699, .F. ) ;
#76115 = CARTESIAN_POINT ( 'NONE',  ( -11.83501748325819847, 1481.582715289189991, 210.0201637637719898 ) ) ;
#76116 = CARTESIAN_POINT ( 'NONE',  ( 1.248319867352440049, 1432.832940376729994, 200.7627304351539976 ) ) ;
#76117 = CARTESIAN_POINT ( 'NONE',  ( -3.246944597254960208, 1508.551704408389924, 213.9909153047919972 ) ) ;
#76118 = CARTESIAN_POINT ( 'NONE',  ( -3.078458326440000281, 1391.041439170870035, 208.7217714433539868 ) ) ;
#76119 = CARTESIAN_POINT ( 'NONE',  ( 8.175629841830000188, 1421.338625457219905, 196.0692449803989916 ) ) ;
#76120 = CARTESIAN_POINT ( 'NONE',  ( -0.9950319637076819879, 1432.231308707049948, 218.5764185903129828 ) ) ;
#76121 = CARTESIAN_POINT ( 'NONE',  ( 10.22475231824599895, 1479.684064890109994, 205.9930891779119975 ) ) ;
#76122 = CARTESIAN_POINT ( 'NONE',  ( 1.483224784644179950, 1408.964855738119923, 186.7893816159290168 ) ) ;
#76123 = CARTESIAN_POINT ( 'NONE',  ( 1.004776255440000154, 1416.277075963729885, 233.2712822367979868 ) ) ;
#76124 = FACE_OUTER_BOUND ( 'NONE', #52157, .T. ) ;
#76125 = ADVANCED_FACE ( 'NONE', ( #37495 ), #51759, .F. ) ;
#76126 = CARTESIAN_POINT ( 'NONE',  ( -13.14956782490000009, 1379.692368811980032, 212.8542620991189835 ) ) ;
#76127 = CARTESIAN_POINT ( 'NONE',  ( 2.311632204762886111, 1525.506926151471362, 241.8052033139069010 ) ) ;
#76128 = ORIENTED_EDGE ( 'NONE', *, *, #100780, .T. ) ;
#76129 = CARTESIAN_POINT ( 'NONE',  ( 12.44185449472429994, 1415.426561690370136, 221.4308737802959968 ) ) ;
#76130 = CARTESIAN_POINT ( 'NONE',  ( 11.00562616383409953, 1432.347154498319924, 151.7431425785430292 ) ) ;
#76131 = CARTESIAN_POINT ( 'NONE',  ( -10.82927499412819650, 1508.551704408370824, 209.2608739639107682 ) ) ;
#76132 = AXIS2_PLACEMENT_3D ( 'NONE', #102750, #7611, #9819 ) ;
#76133 = CARTESIAN_POINT ( 'NONE',  ( -13.37265018080000090, 1390.548598904210166, 209.7987839237050309 ) ) ;
#76134 = CARTESIAN_POINT ( 'NONE',  ( 9.748898013885689551, 1427.681173174970127, 211.1332189737210001 ) ) ;
#76135 = CARTESIAN_POINT ( 'NONE',  ( 12.33008173652610040, 1426.296687997340086, 202.7608368823210299 ) ) ;
#76136 = CARTESIAN_POINT ( 'NONE',  ( 1.335254395760000046, 1430.413233478789834, 217.4945813416789804 ) ) ;
#76137 = CARTESIAN_POINT ( 'NONE',  ( -32.79207798990000100, 1453.265480485330045, 262.6648722463980334 ) ) ;
#76138 = EDGE_CURVE ( 'NONE', #48402, #51877, #60768, .T. ) ;
#76139 = LINE ( 'NONE', #34130, #7391 ) ;
#76140 = CARTESIAN_POINT ( 'NONE',  ( 11.26095182839999964, 1433.846396481040074, 151.5570170780979993 ) ) ;
#76141 = CARTESIAN_POINT ( 'NONE',  ( 21.34957048960000137, 1448.971257410079943, 234.3916895488980003 ) ) ;
#76142 = CARTESIAN_POINT ( 'NONE',  ( -10.57973492554160089, 1462.173887409690224, 209.2258057589959890 ) ) ;
#76143 = CARTESIAN_POINT ( 'NONE',  ( -29.74444329484511940, 1526.348417187221685, 201.0223654199412806 ) ) ;
#76144 = CARTESIAN_POINT ( 'NONE',  ( 8.790767757275109062, 1424.094608705360088, 196.7971378858789819 ) ) ;
#76145 = CARTESIAN_POINT ( 'NONE',  ( 6.263504934518880241, 1465.252758315099982, 218.2608339057509852 ) ) ;
#76146 = CARTESIAN_POINT ( 'NONE',  ( -10.56986511919999927, 1482.340628623390103, 205.9074532915990119 ) ) ;
#76147 = CARTESIAN_POINT ( 'NONE',  ( 0.8265242352189998698, 1408.941923249630008, 231.1644247498980178 ) ) ;
#76148 = DIRECTION ( 'NONE',  ( 0.02091224828123190022, 0.9990482215818557998, 0.03827961371219716635 ) ) ;
#76149 = CARTESIAN_POINT ( 'NONE',  ( -8.097026068654489706, 1425.580256812905645, 208.3196847037820021 ) ) ;
#76150 = CARTESIAN_POINT ( 'NONE',  ( 26.44407582984479532, 1436.722936376503412, 136.8187510453977325 ) ) ;
#76151 = CARTESIAN_POINT ( 'NONE',  ( -15.41379235132240133, 1383.858177494749953, 219.3473563989259958 ) ) ;
#76152 = CARTESIAN_POINT ( 'NONE',  ( -0.4260839224734190300, 1523.429859730332510, 173.4147438076392405 ) ) ;
#76153 = EDGE_CURVE ( 'NONE', #39456, #911, #48109, .T. ) ;
#76154 = CARTESIAN_POINT ( 'NONE',  ( -17.84103558406399870, 1489.004100625149931, 195.1797355196500234 ) ) ;
#76155 = CARTESIAN_POINT ( 'NONE',  ( 1.134357970594999987, 1516.744381837270112, 213.1504571913470159 ) ) ;
#76156 = CARTESIAN_POINT ( 'NONE',  ( -22.20130412889999860, 1417.681004048810109, 209.9662649635100138 ) ) ;
#76157 = CARTESIAN_POINT ( 'NONE',  ( 0.2052462343486599894, 1460.027118118999852, 182.9519127876829998 ) ) ;
#76159 = VERTEX_POINT ( 'NONE', #73865 ) ;
#76158 = CARTESIAN_POINT ( 'NONE',  ( 0.000000000000000000, 1512.187213306747481, 209.1218459616979999 ) ) ;
#76160 = CARTESIAN_POINT ( 'NONE',  ( -28.38894342380001490, 1444.994950788470987, 176.3316754166978910 ) ) ;
#76161 = ADVANCED_FACE ( 'NONE', ( #107993 ), #808, .T. ) ;
#76162 = CARTESIAN_POINT ( 'NONE',  ( -18.22821675530000007, 1443.229620277490085, 204.5519556382290034 ) ) ;
#76163 = CYLINDRICAL_SURFACE ( 'NONE', #12117, 2.000000000000003553 ) ;
#76164 = CARTESIAN_POINT ( 'NONE',  ( -39.89055406580479968, 1448.739173191730060, 134.0999999981559938 ) ) ;
#76165 = CARTESIAN_POINT ( 'NONE',  ( -110.0629075430000086, 1384.909055395449968, 296.9513015316589986 ) ) ;
#76166 = VERTEX_POINT ( 'NONE', #43019 ) ;
#76167 = CARTESIAN_POINT ( 'NONE',  ( -5.607667144112319590, 1391.799625134960024, 203.2661880012859967 ) ) ;
#76168 = CARTESIAN_POINT ( 'NONE',  ( 2.472529913803013013, 1523.678648413191695, 175.3762130535718313 ) ) ;
#76169 = CARTESIAN_POINT ( 'NONE',  ( 8.849375732825370378, 1449.202560831883147, 206.6011072519091272 ) ) ;
#76170 = DIRECTION ( 'NONE',  ( -0.6736849260863841948, 0.000000000000000000, 0.7390186874254148774 ) ) ;
#76172 = ADVANCED_FACE ( 'NONE', ( #83898 ), #41359, .F. ) ;
#76171 = CARTESIAN_POINT ( 'NONE',  ( -3.117088932150390068, 1432.832834640699957, 217.3706902353420105 ) ) ;
#76173 = CARTESIAN_POINT ( 'NONE',  ( -14.54584372631119926, 1473.797026299110030, 194.1930890860980128 ) ) ;
#76174 = CARTESIAN_POINT ( 'NONE',  ( 22.91749086919999812, 1507.625766668030110, 210.6365783057379701 ) ) ;
#76175 = CARTESIAN_POINT ( 'NONE',  ( 7.204667672338278983, 1409.164652926410099, 222.2401956198280004 ) ) ;
#76176 = CARTESIAN_POINT ( 'NONE',  ( -11.03495751070000175, 1391.553749705140035, 203.9031261639289880 ) ) ;
#76177 = CARTESIAN_POINT ( 'NONE',  ( -84.62390092619399695, 1385.174868275669951, 288.3880241305470236 ) ) ;
#76178 = CARTESIAN_POINT ( 'NONE',  ( -10.51241594247230005, 1391.913060387289988, 213.5546871049940023 ) ) ;
#76179 = CARTESIAN_POINT ( 'NONE',  ( 10.70122832801980017, 1423.012206936599796, 207.4581769705870329 ) ) ;
#76180 = ORIENTED_EDGE ( 'NONE', *, *, #39174, .T. ) ;
#76181 = CARTESIAN_POINT ( 'NONE',  ( -32.67729508290000240, 1450.483548884780021, 136.2818069901979925 ) ) ;
#76182 = EDGE_CURVE ( 'NONE', #51642, #27006, #9822, .T. ) ;
#76183 = DIRECTION ( 'NONE',  ( 0.000000000000000000, -1.000000000000000000, 0.000000000000000000 ) ) ;
#76184 = AXIS2_PLACEMENT_3D ( 'NONE', #95788, #87962, #77346 ) ;
#76186 = ORIENTED_EDGE ( 'NONE', *, *, #29537, .T. ) ;
#76185 = CARTESIAN_POINT ( 'NONE',  ( -1.436439550961307932, 1526.373507135059526, 239.4995027077839325 ) ) ;
#76187 = CARTESIAN_POINT ( 'NONE',  ( 1.864351022469999730, 1473.433313301389944, 219.1822183682990044 ) ) ;
#76188 = CIRCLE ( 'NONE', #60063, 2.000000000000001776 ) ;
#76189 = CARTESIAN_POINT ( 'NONE',  ( -16.66231036550682987, 1523.604703353109699, 237.7554842931448036 ) ) ;
#76190 = CARTESIAN_POINT ( 'NONE',  ( -7.834163150019012534, 1364.423415641956353, 208.3718459617061285 ) ) ;
#76191 = CARTESIAN_POINT ( 'NONE',  ( -9.041914599929999241, 1494.936448903489918, 202.3768923597089895 ) ) ;
#76192 = CARTESIAN_POINT ( 'NONE',  ( -14.08142637225379978, 1379.709117121690042, 211.5303641152310092 ) ) ;
#76193 = CARTESIAN_POINT ( 'NONE',  ( 3.034964868304999897, 1517.051704408389924, 200.9398869892670234 ) ) ;
#76194 = CARTESIAN_POINT ( 'NONE',  ( 16.16623905053635823, 1432.037924341066628, 218.4554949826395500 ) ) ;
#76195 = CARTESIAN_POINT ( 'NONE',  ( 7302.760118613915438, 5181.793945261120825, 11064.62217173819772 ) ) ;
#76196 = CARTESIAN_POINT ( 'NONE',  ( 9.167612539120000292, 1450.047499010689990, 204.0226639485589999 ) ) ;
#76197 = CARTESIAN_POINT ( 'NONE',  ( -21.59687142900000012, 1507.523380033690046, 209.4572543540780032 ) ) ;
#76198 = CARTESIAN_POINT ( 'NONE',  ( 7.713339349770000020, 1475.513060387329915, 228.7257818846979944 ) ) ;
#76199 = EDGE_CURVE ( 'NONE', #59685, #108309, #76807, .T. ) ;
#76200 = CARTESIAN_POINT ( 'NONE',  ( -1.202320767300000037, 1456.214200931789946, 199.5726487006490117 ) ) ;
#76201 = CARTESIAN_POINT ( 'NONE',  ( -5.011678876155000850, 1516.989560013210166, 205.8658785457569991 ) ) ;
#76202 = CARTESIAN_POINT ( 'NONE',  ( 3.148243353760000307, 1447.343022348850127, 154.4222316864979803 ) ) ;
#76203 = ADVANCED_FACE ( 'NONE', ( #109663 ), #94650, .T. ) ;
#76204 = CARTESIAN_POINT ( 'NONE',  ( 1.546867746950000067, 1416.839692131129823, 190.2222509470979901 ) ) ;
#76205 = CARTESIAN_POINT ( 'NONE',  ( 19.85510561680000308, 1471.391771582229921, 270.0615508828979614 ) ) ;
#76207 = ORIENTED_EDGE ( 'NONE', *, *, #44750, .T. ) ;
#76206 = CARTESIAN_POINT ( 'NONE',  ( -68.70087839430000543, 1379.747840857399979, 280.2882393206589882 ) ) ;
#76208 = AXIS2_PLACEMENT_3D ( 'NONE', #75431, #110111, #8737 ) ;
#76209 = CARTESIAN_POINT ( 'NONE',  ( -8.013767138614300123, 1382.608589018177554, 218.6364342332414026 ) ) ;
#76210 = VERTEX_POINT ( 'NONE', #45799 ) ;
#76211 = CARTESIAN_POINT ( 'NONE',  ( -16.57651866747404057, 1513.029502680755968, 221.0948183014304789 ) ) ;
#76212 = CARTESIAN_POINT ( 'NONE',  ( -25.41997721759999962, 1449.801887509380094, 207.2020760266680099 ) ) ;
#76214 = CARTESIAN_POINT ( 'NONE',  ( 16.42397614938620265, 1410.721834178540121, 191.6524092019909915 ) ) ;
#76213 = CARTESIAN_POINT ( 'NONE',  ( -11.44610352279480203, 1425.985488001439990, 130.8067335706190022 ) ) ;
#76215 = CARTESIAN_POINT ( 'NONE',  ( -2.282622950494999969, 1516.861367446839949, 211.4218295478370067 ) ) ;
#76216 =( BOUNDED_CURVE ( )  B_SPLINE_CURVE ( 3, ( #61145, #9041, #44318, #26955 ),
 .UNSPECIFIED., .F., .T. ) 
 B_SPLINE_CURVE_WITH_KNOTS ( ( 4, 4 ),
 ( 2.436781329611979352, 3.141592653589793116 ),
 .UNSPECIFIED. ) 
 CURVE ( )  GEOMETRIC_REPRESENTATION_ITEM ( )  RATIONAL_B_SPLINE_CURVE ( ( 1.000000000000000000, 0.9590300661663082593, 0.9590300661663082593, 1.000000000000000000 ) ) 
 REPRESENTATION_ITEM ( '' )  );
#76217 = CARTESIAN_POINT ( 'NONE',  ( 29.01787501698136396, 1510.037283517486912, 201.5082493885905421 ) ) ;
#76218 = CARTESIAN_POINT ( 'NONE',  ( 1.424296475967616660, 1450.671211070973186, 181.6313727864856560 ) ) ;
#76219 = B_SPLINE_CURVE_WITH_KNOTS ( 'NONE', 3,
 ( #87123, #10413, #66363, #73652, #13145, #14263 ),
 .UNSPECIFIED., .F., .F.,
 ( 4, 2, 4 ),
 ( 0.000000000000000000, 0.5000000000000000000, 1.000000000000000000 ),
 .UNSPECIFIED. ) ;
#76220 =( NAMED_UNIT ( * ) PLANE_ANGLE_UNIT ( ) SI_UNIT ( $, .RADIAN. ) );
#76221 = CARTESIAN_POINT ( 'NONE',  ( -13.38006552295539997, 1379.538105693709895, 208.4172449948689803 ) ) ;
#76222 = CARTESIAN_POINT ( 'NONE',  ( 12.67146871665720020, 1500.791398092430200, 210.0979814907519767 ) ) ;
#76223 = CARTESIAN_POINT ( 'NONE',  ( 3.818684287277759992, 1508.551704408389924, 213.7264380181929937 ) ) ;
#76224 = CARTESIAN_POINT ( 'NONE',  ( -39.53412538496939987, 1440.582317794330038, 136.7849119739890114 ) ) ;
#76225 = ORIENTED_EDGE ( 'NONE', *, *, #43449, .T. ) ;
#76226 = CARTESIAN_POINT ( 'NONE',  ( 12.64873006253779941, 1397.980667074559733, 213.9846389742999975 ) ) ;
#76227 = CARTESIAN_POINT ( 'NONE',  ( -16.66936639845670243, 1518.913060387330006, 180.4828114240741854 ) ) ;
#76228 = ORIENTED_EDGE ( 'NONE', *, *, #22164, .F. ) ;
#76229 = ORIENTED_EDGE ( 'NONE', *, *, #87858, .T. ) ;
#76230 = B_SPLINE_CURVE_WITH_KNOTS ( 'NONE', 3,
 ( #69947, #60991, #104619, #43619, #44737, #36862 ),
 .UNSPECIFIED., .F., .F.,
 ( 4, 2, 4 ),
 ( -0.08571269188183310017, -0.04143665797639420334, -1.438549643295594649E-08 ),
 .UNSPECIFIED. ) ;
#76231 = CARTESIAN_POINT ( 'NONE',  ( -29.64937900391915093, 1509.975914221921357, 210.4712216346827915 ) ) ;
#76232 = FACE_OUTER_BOUND ( 'NONE', #11936, .T. ) ;
#76233 = CARTESIAN_POINT ( 'NONE',  ( -14.15085831685690110, 1380.030482968580145, 211.0724251982179851 ) ) ;
#76234 = CARTESIAN_POINT ( 'NONE',  ( -12.26971806897292261, 1417.403025294029476, 199.8085102575429062 ) ) ;
#76235 = FACE_OUTER_BOUND ( 'NONE', #63568, .T. ) ;
#76236 = CARTESIAN_POINT ( 'NONE',  ( -6.487838854381950071, 1454.049012225269962, 202.3499870543650161 ) ) ;
#76237 = CARTESIAN_POINT ( 'NONE',  ( 33.91369117179520032, 1435.681798755330192, 134.4205480820800176 ) ) ;
#76238 = CARTESIAN_POINT ( 'NONE',  ( -0.4403324739431219714, 1517.051704035390003, 216.6089087266339845 ) ) ;
#76239 = CARTESIAN_POINT ( 'NONE',  ( -1.742717375088950107E-15, 1375.426148861440197, 209.1218459572589836 ) ) ;
#76240 = CARTESIAN_POINT ( 'NONE',  ( -10.07717734240000063, 1391.913060387289988, 214.9705334440889715 ) ) ;
#76241 = CARTESIAN_POINT ( 'NONE',  ( -87.22158348405449146, 1384.827375891360134, 290.6397261970639647 ) ) ;
#76242 = VERTEX_POINT ( 'NONE', #20544 ) ;
#76243 = CARTESIAN_POINT ( 'NONE',  ( 1.709384572955000126, 1517.224900789629828, 201.7820965968870155 ) ) ;
#76244 = CARTESIAN_POINT ( 'NONE',  ( 1.709766494024999917, 1516.959716008189844, 209.1091877442879934 ) ) ;
#76245 = ORIENTED_EDGE ( 'NONE', *, *, #308, .T. ) ;
#76246 = CARTESIAN_POINT ( 'NONE',  ( 11.08206323080000111, 1414.913528139129994, 222.2042284754980130 ) ) ;
#76247 = CARTESIAN_POINT ( 'NONE',  ( 3.385873918483515155, 1511.683950138257387, 217.1255238520139415 ) ) ;
#76248 = VERTEX_POINT ( 'NONE', #95070 ) ;
#76249 = CARTESIAN_POINT ( 'NONE',  ( -13.88473851270000026, 1415.296882296330068, 220.8066774238980088 ) ) ;
#76250 = CARTESIAN_POINT ( 'NONE',  ( 6.708192185693589771, 1429.353568409279887, 215.8261836254480102 ) ) ;
#76251 = CARTESIAN_POINT ( 'NONE',  ( -17.15734414464520086, 1420.193758488640015, 204.4307800783660127 ) ) ;
#76252 = CARTESIAN_POINT ( 'NONE',  ( -9.639755125763619148, 1461.269863503290026, 208.0610523092789776 ) ) ;
#76253 = DIRECTION ( 'NONE',  ( 1.755985294532469921E-16, -1.000000000000000000, 1.338183447452831989E-16 ) ) ;
#76254 = CARTESIAN_POINT ( 'NONE',  ( -7.720339733105665125, 1446.701196261682981, 154.1134164384996268 ) ) ;
#76255 = CARTESIAN_POINT ( 'NONE',  ( -9.574683806340001269, 1473.399577885589906, 205.3280175804189867 ) ) ;
#76256 = CARTESIAN_POINT ( 'NONE',  ( 18.02257621027576917, 1526.382868172863937, 182.8951942368371988 ) ) ;
#76257 = CARTESIAN_POINT ( 'NONE',  ( -54.44115314580000131, 1379.700200843730045, 248.9289766756589870 ) ) ;
#76258 = CARTESIAN_POINT ( 'NONE',  ( -15.73134880039999928, 1485.117178942230112, 224.0171761809980069 ) ) ;
#76260 = DIRECTION ( 'NONE',  ( 5.980589973904019347E-17, -1.000000000000000000, 1.736889445713099699E-16 ) ) ;
#76259 = CARTESIAN_POINT ( 'NONE',  ( -5.099055259868809920, 1496.765404324240080, 199.0959566236750220 ) ) ;
#76261 = CARTESIAN_POINT ( 'NONE',  ( 15.13342375178309851, 1507.606285622089899, 226.3974328904010065 ) ) ;
#76262 = ADVANCED_FACE ( 'NONE', ( #104013 ), #54748, .F. ) ;
#76263 = B_SPLINE_CURVE_WITH_KNOTS ( 'NONE', 5,
 ( #89238, #46711, #29873, #64061, #4682, #64614 ),
 .UNSPECIFIED., .F., .F.,
 ( 6, 6 ),
 ( 266.2319129360000147, 276.0458535200000370 ),
 .UNSPECIFIED. ) ;
#76264 = CARTESIAN_POINT ( 'NONE',  ( -2.499956565898610261, 1419.670774135810007, 129.2260277615939970 ) ) ;
#76265 = ORIENTED_EDGE ( 'NONE', *, *, #20160, .T. ) ;
#76266 = CARTESIAN_POINT ( 'NONE',  ( -1.290830522935544789, 1486.252651503785501, 181.7990903393099700 ) ) ;
#76267 = CARTESIAN_POINT ( 'NONE',  ( -21.51496489921823851, 1524.872178180562969, 234.5520185365066652 ) ) ;
#76268 = CARTESIAN_POINT ( 'NONE',  ( 1.712644716155000024, 1516.636036526019780, 214.1174694231270053 ) ) ;
#76269 = CARTESIAN_POINT ( 'NONE',  ( -2.991115354478053767, 1485.673002022499531, 182.6499386298461616 ) ) ;
#76270 = CARTESIAN_POINT ( 'NONE',  ( -14.53003990559999892, 1415.677402202029953, 213.1288439181290073 ) ) ;
#76272 = VERTEX_POINT ( 'NONE', #9955 ) ;
#76271 = CARTESIAN_POINT ( 'NONE',  ( 4.556911006048280477, 1508.729442775010057, 212.9448352109289999 ) ) ;
#76273 = CARTESIAN_POINT ( 'NONE',  ( 0.5620975284769998970, 1416.851343898729965, 190.4751211474980153 ) ) ;
#76275 = B_SPLINE_CURVE_WITH_KNOTS ( 'NONE', 3,
 ( #12758, #19491, #37966, #21679, #105170, #2733, #53694, #81057, #62654, #38501, #96776, #55886, #46390, #72678, #97850 ),
 .UNSPECIFIED., .F., .F.,
 ( 4, 2, 2, 1, 1, 1, 2, 2, 4 ),
 ( 0.000000000000000000, 0.2500000000000007216, 0.3750000000000014433, 0.4375000000000032196, 0.4687500000000054401, 0.4843750000000056066, 0.4921875000000097145, 0.5000000000000137668, 1.000000000000000000 ),
 .UNSPECIFIED. ) ;
#76274 = CARTESIAN_POINT ( 'NONE',  ( -1.569490127089999909, 1507.974949271890182, 221.0030736986989837 ) ) ;
#76276 = ADVANCED_FACE ( 'NONE', ( #70452 ), #104572, .F. ) ;
#76277 = CARTESIAN_POINT ( 'NONE',  ( -10.92384068729999846, 1429.091921970129988, 151.0140743380979984 ) ) ;
#76278 = CARTESIAN_POINT ( 'NONE',  ( 19.55988977460000200, 1474.636381753090063, 214.0184790771390055 ) ) ;
#76279 = CARTESIAN_POINT ( 'NONE',  ( -7.624682118549999998, 1442.078355704660225, 184.2071361224980137 ) ) ;
#76280 = CARTESIAN_POINT ( 'NONE',  ( -28.15442856212169787, 1509.896234822020006, 200.8410265843269826 ) ) ;
#76281 = DIRECTION ( 'NONE',  ( 1.000000000000000000, 0.000000000000000000, 0.000000000000000000 ) ) ;
#76282 = CARTESIAN_POINT ( 'NONE',  ( 0.2660838379469560033, 1443.814632406239980, 189.5938922378529981 ) ) ;
#76284 = CARTESIAN_POINT ( 'NONE',  ( -10.55795760898930169, 1481.591005463860029, 207.1796093610390130 ) ) ;
#76283 = CARTESIAN_POINT ( 'NONE',  ( -20.54580208550000009, 1495.372389045430054, 227.4306167334980273 ) ) ;
#76285 = CARTESIAN_POINT ( 'NONE',  ( -16.96961820828100187, 1460.580780704285871, 228.2620474942170006 ) ) ;
#76286 = ORIENTED_EDGE ( 'NONE', *, *, #84896, .F. ) ;
#76287 = CARTESIAN_POINT ( 'NONE',  ( -5.786527600464999033, 1517.025653221279981, 205.6708125431369751 ) ) ;
#76288 = CARTESIAN_POINT ( 'NONE',  ( 36.03851880410000064, 1418.520028046229982, 267.9355420903980303 ) ) ;
#76289 = CARTESIAN_POINT ( 'NONE',  ( 1.875671004969999833, 1456.514200624189925, 219.5762891113990065 ) ) ;
#76290 = CARTESIAN_POINT ( 'NONE',  ( 18.99729322769999840, 1449.733786570959865, 191.9831398968979954 ) ) ;
#76291 = AXIS2_PLACEMENT_3D ( 'NONE', #67275, #40388, #75120 ) ;
#76292 = CARTESIAN_POINT ( 'NONE',  ( -0.02088553982763170086, 1508.565558233520051, 237.9144398107179939 ) ) ;
#76293 = CARTESIAN_POINT ( 'NONE',  ( -9.255471102502529135, 1389.295763922535798, 217.3525502945869903 ) ) ;
#76294 = CARTESIAN_POINT ( 'NONE',  ( -32.38114538885245963, 1523.604703353109699, 216.1203639561433647 ) ) ;
#76295 = CARTESIAN_POINT ( 'NONE',  ( 15.26419385149999997, 1460.025905744229931, 232.1043486749979934 ) ) ;
#76296 = CARTESIAN_POINT ( 'NONE',  ( -15.20766188370000194, 1415.439842373489910, 206.5207236011790144 ) ) ;
#76297 = CARTESIAN_POINT ( 'NONE',  ( -13.65702322080000108, 1443.964959164910169, 187.8161327681980026 ) ) ;
#76298 = EDGE_CURVE ( 'NONE', #28737, #26609, #59871, .T. ) ;
#76299 = CARTESIAN_POINT ( 'NONE',  ( -22.44565107540000071, 1519.913060387329779, 213.3775353178480145 ) ) ;
#76300 = CARTESIAN_POINT ( 'NONE',  ( -8.607248916523710491, 1436.893216450120008, 209.7353648425139738 ) ) ;
#76301 = CARTESIAN_POINT ( 'NONE',  ( 0.9912867144625557847, 1407.655978792028236, 270.1376065696978799 ) ) ;
#76302 = EDGE_CURVE ( 'NONE', #101078, #75505, #25059, .T. ) ;
#76303 = CARTESIAN_POINT ( 'NONE',  ( -2.725379146709999922, 1470.857295113890132, 189.2740040492990090 ) ) ;
#76304 = CARTESIAN_POINT ( 'NONE',  ( -19.62446893450000118, 1440.913060387330006, 214.3676144200779845 ) ) ;
#76306 = EDGE_CURVE ( 'NONE', #40681, #13824, #71582, .T. ) ;
#76305 = CARTESIAN_POINT ( 'NONE',  ( -10.93665447375030020, 1508.551709316179995, 207.6442539328949977 ) ) ;
#76307 = DIRECTION ( 'NONE',  ( 1.000000000000000000, 0.000000000000000000, 0.000000000000000000 ) ) ;
#76308 = CARTESIAN_POINT ( 'NONE',  ( -9.770742656079999477, 1474.306579240830160, 269.6204776596980537 ) ) ;
#76309 = CARTESIAN_POINT ( 'NONE',  ( -30.60461244942494119, 1523.621879633029039, 196.4204177336144426 ) ) ;
#76310 = CARTESIAN_POINT ( 'NONE',  ( -14.78979538456069243, 1514.562512395940075, 192.8671644546608661 ) ) ;
#76311 = CARTESIAN_POINT ( 'NONE',  ( 17.93928201133349987, 1417.697889326150062, 223.6392055776269956 ) ) ;
#76312 = CARTESIAN_POINT ( 'NONE',  ( -44.65204099977980690, 1384.765860786410030, 250.8497032329840124 ) ) ;
#76313 = DIRECTION ( 'NONE',  ( 0.03489949670247723124, 0.9993908270190966503, -2.775557561563011889E-14 ) ) ;
#76314 = CARTESIAN_POINT ( 'NONE',  ( 11.93592535262039966, 1415.651572961180136, 223.2534673748540115 ) ) ;
#76315 = B_SPLINE_CURVE_WITH_KNOTS ( 'NONE', 5,
 ( #89854, #47857, #4209, #5299, #39457, #20978 ),
 .UNSPECIFIED., .F., .F.,
 ( 6, 6 ),
 ( -2.000000000000000000, 0.000000000000000000 ),
 .UNSPECIFIED. ) ;
#76316 = ADVANCED_FACE ( 'NONE', ( #2696 ), #96174, .T. ) ;
#76317 = CARTESIAN_POINT ( 'NONE',  ( 21.84020450222056908, 1512.187213306747481, 234.9798068779740277 ) ) ;
#76318 = CARTESIAN_POINT ( 'NONE',  ( -5.534100668969379910, 1464.371862158079921, 199.5915835189479992 ) ) ;
#76319 = CARTESIAN_POINT ( 'NONE',  ( 31.23437356469435144, 1512.187213306747481, 195.3468678195113739 ) ) ;
#76320 = CARTESIAN_POINT ( 'NONE',  ( -22.12837256650000128, 1409.685800185430026, 205.2451141150779677 ) ) ;
#76321 = CARTESIAN_POINT ( 'NONE',  ( -8.586603470991246212, 1382.365454073439651, 200.1294793584183935 ) ) ;
#76322 = CARTESIAN_POINT ( 'NONE',  ( 4.856733042310000137, 1485.951405104490050, 218.7380990343689859 ) ) ;
#76323 = CARTESIAN_POINT ( 'NONE',  ( 10.49503676954149967, 1479.901654632730242, 207.2485989259390067 ) ) ;
#76324 = CARTESIAN_POINT ( 'NONE',  ( 1.639582970820000041, 1434.541746329560056, 150.4377894671980016 ) ) ;
#76325 = CARTESIAN_POINT ( 'NONE',  ( 20.42700490659999701, 1433.617019421789792, 214.5837023497890073 ) ) ;
#76326 = CARTESIAN_POINT ( 'NONE',  ( 17.26793975759715138, 1525.730671948510235, 181.5864082646643851 ) ) ;
#76327 = CARTESIAN_POINT ( 'NONE',  ( -2.472529913803023227, 1523.678648413191695, 175.3762130535718597 ) ) ;
#76329 = CARTESIAN_POINT ( 'NONE',  ( -2.487935012184434136, 1508.551704408389924, 204.2892291574235628 ) ) ;
#76328 = CARTESIAN_POINT ( 'NONE',  ( -21.62710251429999886, 1409.668295441930013, 211.5114173564280122 ) ) ;
#76330 = CARTESIAN_POINT ( 'NONE',  ( 11.72797607332480041, 1426.701692393189887, 143.5212822355949811 ) ) ;
#76331 = DIRECTION ( 'NONE',  ( 0.000000000000000000, 0.000000000000000000, -1.000000000000000000 ) ) ;
#76332 = CARTESIAN_POINT ( 'NONE',  ( -7.592573335200579976, 1517.051705360449887, 204.6351128173299969 ) ) ;
#76333 = CARTESIAN_POINT ( 'NONE',  ( -16.66936639845609847, 1518.913060387330006, 237.7608804993221838 ) ) ;
#76334 = CARTESIAN_POINT ( 'NONE',  ( -2.500000000000000000, 1439.615672362369878, 128.3512065685980019 ) ) ;
#76335 = CARTESIAN_POINT ( 'NONE',  ( 6.939219482805000005, 1516.783701990830195, 203.3409846960470020 ) ) ;
#76336 = CYLINDRICAL_SURFACE ( 'NONE', #19690, 1.000000000000001110 ) ;
#76337 = CARTESIAN_POINT ( 'NONE',  ( -11.74015320060000001, 1428.979986575930070, 144.1938086916980239 ) ) ;
#76338 = CARTESIAN_POINT ( 'NONE',  ( 15.73511540573499801, 1514.703592237370003, 193.7861023190669982 ) ) ;
#76339 = FACE_BOUND ( 'NONE', #43065, .T. ) ;
#76340 = CARTESIAN_POINT ( 'NONE',  ( 1.874390728800000128, 1508.748819628430056, 237.3943831762979926 ) ) ;
#76341 = ADVANCED_FACE ( 'NONE', ( #79380 ), #26707, .F. ) ;
#76342 = CARTESIAN_POINT ( 'NONE',  ( 21.26194160363760233, 1509.381988423189796, 228.0863887365900098 ) ) ;
#76345 = VERTEX_POINT ( 'NONE', #81557 ) ;
#76344 = CARTESIAN_POINT ( 'NONE',  ( -48.05471153476000268, 1379.681133392060019, 241.5169778073720011 ) ) ;
#76343 = AXIS2_PLACEMENT_3D ( 'NONE', #88042, #721, #43814 ) ;
#76346 = ORIENTED_EDGE ( 'NONE', *, *, #98178, .T. ) ;
#76347 = CARTESIAN_POINT ( 'NONE',  ( 11.45376624174839897, 1434.341927546149918, 151.4236503405790017 ) ) ;
#76348 = CARTESIAN_POINT ( 'NONE',  ( -12.72899733799999922, 1397.389012456630098, 211.4694218863679964 ) ) ;
#76349 = EDGE_LOOP ( 'NONE', ( #60413, #82128, #36583, #80208 ) ) ;
#76350 = CARTESIAN_POINT ( 'NONE',  ( -107.0802177269999902, 1378.913060387289988, 307.3184745608590447 ) ) ;
#76351 = CARTESIAN_POINT ( 'NONE',  ( -109.6575798300000031, 1384.922737831749828, 311.3230295302589639 ) ) ;
#76352 = CARTESIAN_POINT ( 'NONE',  ( 3.465081665767860031, 1515.493283046529996, 205.2090687340129875 ) ) ;
#76355 = ADVANCED_FACE ( 'NONE', ( #21093 ), #73748, .T. ) ;
#76354 = CARTESIAN_POINT ( 'NONE',  ( -14.13384278227159818, 1509.281245845819967, 183.3826977356570183 ) ) ;
#76353 = CARTESIAN_POINT ( 'NONE',  ( 16.06955848517850072, 1424.062620710240026, 191.1090677130400195 ) ) ;
#76356 = CARTESIAN_POINT ( 'NONE',  ( 17.31741470348719858, 1498.111796630450044, 230.4563530528860156 ) ) ;
#76357 = CARTESIAN_POINT ( 'NONE',  ( 1.530673255310000203, 1429.773503041730009, 184.4796783900980301 ) ) ;
#76358 = CARTESIAN_POINT ( 'NONE',  ( -2.676551809669999837, 1415.087818611729972, 192.3610496020979781 ) ) ;
#76359 = CARTESIAN_POINT ( 'NONE',  ( 42.54900162989899570, 1440.913053717579942, 270.0692078703979746 ) ) ;
#76360 = CARTESIAN_POINT ( 'NONE',  ( 0.9175745326867349450, 1395.945102796070159, 198.1514473720520186 ) ) ;
#76361 = CARTESIAN_POINT ( 'NONE',  ( 0.1681681984989999989, 1420.473120458229914, 179.3023655596979893 ) ) ;
#76362 = CARTESIAN_POINT ( 'NONE',  ( 11.86318670040000001, 1432.127862331690039, 150.3942814104979959 ) ) ;
#76363 = CARTESIAN_POINT ( 'NONE',  ( 7.922128340844998284, 1512.637906871309724, 202.2771797188770222 ) ) ;
#76364 = ORIENTED_EDGE ( 'NONE', *, *, #16601, .F. ) ;
#76365 = CARTESIAN_POINT ( 'NONE',  ( 13.52173958309080071, 1435.750944454330011, 150.3327472168750205 ) ) ;
#76366 = EDGE_LOOP ( 'NONE', ( #19342, #110754, #421, #3961 ) ) ;
#76367 = VERTEX_POINT ( 'NONE', #81024 ) ;
#76368 = CARTESIAN_POINT ( 'NONE',  ( 13.21106958178233270, 1444.696289312639465, 169.3897206396751756 ) ) ;
#76369 = CARTESIAN_POINT ( 'NONE',  ( -9.313356613159999853, 1463.019685538429940, 234.3550464167980181 ) ) ;
#76370 = CARTESIAN_POINT ( 'NONE',  ( -8.168076443215248617, 1407.240959200780026, 219.8347814960359869 ) ) ;
#76371 = CIRCLE ( 'NONE', #37036, 9.000000000000007105 ) ;
#76372 = CARTESIAN_POINT ( 'NONE',  ( -1.126138146715000010, 1517.208444099459939, 216.8485306577670144 ) ) ;
#76373 = CARTESIAN_POINT ( 'NONE',  ( -7.889127765447542906, 1512.111483631436613, 212.0902013560271655 ) ) ;
#76374 = CARTESIAN_POINT ( 'NONE',  ( 11.19986414605820002, 1422.142818617800003, 210.4362617274329921 ) ) ;
#76375 = CARTESIAN_POINT ( 'NONE',  ( 2.500000000000000000, 1448.210397838020072, 167.6163145387380098 ) ) ;
#76376 = CARTESIAN_POINT ( 'NONE',  ( -26.65670438309999923, 1379.321141781539836, 211.2412313610489889 ) ) ;
#76377 = ORIENTED_EDGE ( 'NONE', *, *, #11122, .F. ) ;
#76378 = CARTESIAN_POINT ( 'NONE',  ( -4.624736897314999595, 1516.994127245590107, 206.2540423059970180 ) ) ;
#76379 = ORIENTED_EDGE ( 'NONE', *, *, #79257, .F. ) ;
#76380 = DIRECTION ( 'NONE',  ( -1.836970198721029688E-16, -1.000000000000000000, 0.000000000000000000 ) ) ;
#76381 = CARTESIAN_POINT ( 'NONE',  ( -18.63864992400000276, 1509.044553702130088, 230.2784244607980213 ) ) ;
#76382 = CARTESIAN_POINT ( 'NONE',  ( -6.931887347990000059, 1409.155127227530102, 188.8914258914980167 ) ) ;
#76383 = CARTESIAN_POINT ( 'NONE',  ( 7.636446028244999518, 1514.050458741990042, 215.1082210740069911 ) ) ;
#76385 = EDGE_LOOP ( 'NONE', ( #104025, #99946, #34160, #92767 ) ) ;
#76384 = CARTESIAN_POINT ( 'NONE',  ( -2.206960501559600107, 1422.422356592760025, 192.6328859643259932 ) ) ;
#76386 = CARTESIAN_POINT ( 'NONE',  ( 23.70375358549999945, 1434.825524415949985, 215.3081005562079895 ) ) ;
#76387 = CARTESIAN_POINT ( 'NONE',  ( 11.86716023049999968, 1432.353341358199941, 147.6509521729980179 ) ) ;
#76388 = CARTESIAN_POINT ( 'NONE',  ( -9.184850993605149917E-16, 1374.913060387289988, 209.1218459616989946 ) ) ;
#76389 = DIRECTION ( 'NONE',  ( 0.000000000000000000, 1.000000000000000000, 0.000000000000000000 ) ) ;
#76390 = CIRCLE ( 'NONE', #96055, 1.999999999999999556 ) ;
#76391 = CARTESIAN_POINT ( 'NONE',  ( -4.610938249504999753, 1516.815231249920089, 213.1623732742069990 ) ) ;
#76392 = CARTESIAN_POINT ( 'NONE',  ( 2.281297470570000208, 1468.629604151690046, 216.0053196740190060 ) ) ;
#76393 = CARTESIAN_POINT ( 'NONE',  ( 24.02347886858969872, 1410.714002848892278, 209.6150515799677976 ) ) ;
#76394 = CARTESIAN_POINT ( 'NONE',  ( 7.512716704728560124, 1509.034509440879901, 215.2632436668019977 ) ) ;
#76395 = CARTESIAN_POINT ( 'NONE',  ( -2.282622950494999969, 1516.861367446839949, 211.4218295478370067 ) ) ;
#76396 = CARTESIAN_POINT ( 'NONE',  ( -21.77174004986084555, 1524.860077346004800, 233.5882226505204642 ) ) ;
#76397 = CARTESIAN_POINT ( 'NONE',  ( 13.86092958890000126, 1410.765486798930169, 191.1266625105979813 ) ) ;
#76398 = CARTESIAN_POINT ( 'NONE',  ( 2.461132262735347798, 1421.750034555250522, 139.1420193590112717 ) ) ;
#76400 = ORIENTED_EDGE ( 'NONE', *, *, #60562, .T. ) ;
#76399 = CARTESIAN_POINT ( 'NONE',  ( -46.12437349460000036, 1389.616683096550105, 246.0195738906589895 ) ) ;
#76401 = CARTESIAN_POINT ( 'NONE',  ( -69.10652963092418588, 1385.027354731980040, 294.0433430371250552 ) ) ;
#76402 = CARTESIAN_POINT ( 'NONE',  ( 1.052045010949999979E-09, 1470.400767512030143, 255.2684314988979963 ) ) ;
#76403 = CARTESIAN_POINT ( 'NONE',  ( -4.234272664024971711, 1370.421201462527506, 209.6675854122346152 ) ) ;
#76404 = CARTESIAN_POINT ( 'NONE',  ( 0.3248848659079795476, 1494.310064355425538, 220.2531037086061758 ) ) ;
#76405 = CARTESIAN_POINT ( 'NONE',  ( -3.777475378889999735, 1462.602678821090194, 203.1963512104490235 ) ) ;
#76406 = CARTESIAN_POINT ( 'NONE',  ( 0.4160887415541561496, 1444.416418669234645, 218.0718905750308352 ) ) ;
#76407 = AXIS2_PLACEMENT_3D ( 'NONE', #106986, #64466, #98582 ) ;
#76409 = CARTESIAN_POINT ( 'NONE',  ( 16.96418136024609780, 1409.508820805990126, 222.1821933189740150 ) ) ;
#76408 = CARTESIAN_POINT ( 'NONE',  ( 7.868158389100000427, 1422.937290482379922, 214.1570520181289794 ) ) ;
#76410 = CARTESIAN_POINT ( 'NONE',  ( -10.36656297781870073, 1447.925473656809800, 209.2996031035340252 ) ) ;
#76412 = B_SPLINE_CURVE_WITH_KNOTS ( 'NONE', 5,
 ( #11671, #1635, #104069, #18945, #87849, #71063, #105185, #10573, #20061, #88381, #45847, #536, #68844, #102948, #60437 ),
 .UNSPECIFIED., .F., .F.,
 ( 6, 3, 3, 3, 6 ),
 ( 0.000000000000000000, 0.3446931986191029695, 0.5658372174535590826, 0.8241082499738381362, 1.000000000000000000 ),
 .UNSPECIFIED. ) ;
#76411 = CARTESIAN_POINT ( 'NONE',  ( -108.9087294810559996, 1383.070058043159861, 310.9164552416630158 ) ) ;
#76413 = ORIENTED_EDGE ( 'NONE', *, *, #101536, .F. ) ;
#76414 = CARTESIAN_POINT ( 'NONE',  ( 2.870951667784999994, 1517.111322026010157, 202.5592101095969895 ) ) ;
#76415 = CARTESIAN_POINT ( 'NONE',  ( -13.27214107118760111, 1508.445510704319986, 216.9337900148879896 ) ) ;
#76416 = CARTESIAN_POINT ( 'NONE',  ( 14.80435908759999997, 1474.026124292930035, 223.3946435410979916 ) ) ;
#76417 = CIRCLE ( 'NONE', #6637, 2.028272653252106927 ) ;
#76418 = CARTESIAN_POINT ( 'NONE',  ( -1.541238598094009972E-13, 1515.051704408389924, 212.9514660752490158 ) ) ;
#76419 = CARTESIAN_POINT ( 'NONE',  ( -33.28034951413127374, 1522.644714754858796, 217.4407153818779079 ) ) ;
#76420 = CYLINDRICAL_SURFACE ( 'NONE', #75325, 33.13701971169416538 ) ;
#76421 = CARTESIAN_POINT ( 'NONE',  ( 25.99184421905080811, 1450.775692673193362, 136.7467824686237918 ) ) ;
#76422 = CARTESIAN_POINT ( 'NONE',  ( 15.49277546151340879, 1420.928748437756440, 227.7039097393026452 ) ) ;
#76423 = CARTESIAN_POINT ( 'NONE',  ( 32.02224580989319946, 1436.511321034889988, 136.5688601130949849 ) ) ;
#76424 = SPHERICAL_SURFACE ( 'NONE', #18092, 2.000000000000000000 ) ;
#76425 = DIRECTION ( 'NONE',  ( 0.7414773880254760252, -0.000000000000000000, 0.6709778558543624261 ) ) ;
#76426 = CARTESIAN_POINT ( 'NONE',  ( -2.532955078589999687, 1430.062185629989926, 201.0558263785989652 ) ) ;
#76427 = EDGE_CURVE ( 'NONE', #52452, #72871, #91625, .T. ) ;
#76428 = CARTESIAN_POINT ( 'NONE',  ( 14.69816566019999904, 1509.426331642330069, 184.0211180668979978 ) ) ;
#76429 = CARTESIAN_POINT ( 'NONE',  ( -21.26060865160879843, 1525.055402519452628, 184.3612730374274520 ) ) ;
#76430 = CARTESIAN_POINT ( 'NONE',  ( -6.852639342928195099, 1447.389009270719498, 215.1469147219418403 ) ) ;
#76431 = VERTEX_POINT ( 'NONE', #39004 ) ;
#76432 = DIRECTION ( 'NONE',  ( 0.000000000000000000, 0.000000000000000000, 1.000000000000000000 ) ) ;
#76433 = CARTESIAN_POINT ( 'NONE',  ( -35.99825504957585309, 1419.870133879962850, 269.2276119577702502 ) ) ;
#76434 = CARTESIAN_POINT ( 'NONE',  ( -4.492644285160710460, 1508.880967439349888, 212.9248381652639921 ) ) ;
#76435 = CARTESIAN_POINT ( 'NONE',  ( 15.97551097353819927, 1477.212431653470048, 189.0465089897220139 ) ) ;
#76436 = CARTESIAN_POINT ( 'NONE',  ( -2.710264235259999877E-09, 1476.076643212929866, 267.5371647992980115 ) ) ;
#76438 = AXIS2_PLACEMENT_3D ( 'NONE', #91983, #49449, #40478 ) ;
#76437 = CARTESIAN_POINT ( 'NONE',  ( 11.50779367390000019, 1502.003025289490097, 210.7563750071790025 ) ) ;
#76439 = CARTESIAN_POINT ( 'NONE',  ( -28.29412264859999837, 1508.657108475729956, 208.9834593761570147 ) ) ;
#76440 = CARTESIAN_POINT ( 'NONE',  ( 8.758614224470001375, 1427.348506402559906, 211.4846174044990050 ) ) ;
#76441 = CARTESIAN_POINT ( 'NONE',  ( 16.62351968733444352, 1524.082582765195411, 180.5404605103855999 ) ) ;
#76442 = DIRECTION ( 'NONE',  ( 0.000000000000000000, 1.000000000000000000, 0.000000000000000000 ) ) ;
#76444 = ADVANCED_FACE ( 'NONE', ( #89426 ), #73181, .T. ) ;
#76443 = CARTESIAN_POINT ( 'NONE',  ( -6.982994490885238825, 1451.423926582423519, 153.2281128498337637 ) ) ;
#76445 = CARTESIAN_POINT ( 'NONE',  ( -18.16418870590820234, 1416.835419214280137, 209.0763567938479923 ) ) ;
#76446 = CARTESIAN_POINT ( 'NONE',  ( 25.87190634410000101, 1436.506016957939892, 136.9687052083980063 ) ) ;
#76447 = CARTESIAN_POINT ( 'NONE',  ( -7.872426330613159884, 1396.187971572860079, 201.3681491859670132 ) ) ;
#76448 = ORIENTED_EDGE ( 'NONE', *, *, #93835, .F. ) ;
#76449 = CARTESIAN_POINT ( 'NONE',  ( -0.05448001189851819914, 1416.221314539589912, 191.0976842799670123 ) ) ;
#76450 = CARTESIAN_POINT ( 'NONE',  ( 21.18003081007569932, 1508.593876612841086, 226.2067732376109177 ) ) ;
#76451 = EDGE_CURVE ( 'NONE', #16403, #105885, #86037, .T. ) ;
#76452 = EDGE_LOOP ( 'NONE', ( #86279, #103633 ) ) ;
#76453 = ORIENTED_EDGE ( 'NONE', *, *, #92607, .F. ) ;
#76454 = CARTESIAN_POINT ( 'NONE',  ( -11.33871459559999906, 1500.797327991989960, 210.5565315030190163 ) ) ;
#76455 = CARTESIAN_POINT ( 'NONE',  ( -15.01426432124087285, 1416.094347576616428, 205.4938507932126868 ) ) ;
#76457 = CARTESIAN_POINT ( 'NONE',  ( -22.42801321349999810, 1448.695731516339947, 212.0101260109479995 ) ) ;
#76456 = DIRECTION ( 'NONE',  ( -0.3090169943749515036, 0.000000000000000000, -0.9510565162951521989 ) ) ;
#76458 = CARTESIAN_POINT ( 'NONE',  ( -2.861397284679999764, 1445.646508516890208, 217.6990959301490136 ) ) ;
#76459 = CARTESIAN_POINT ( 'NONE',  ( -11.87550762409999905, 1433.043840478560242, 149.9802072585979715 ) ) ;
#76460 = CARTESIAN_POINT ( 'NONE',  ( -14.31906343784990021, 1380.323795378649947, 209.9058136714729983 ) ) ;
#76461 = AXIS2_PLACEMENT_3D ( 'NONE', #61436, #60316, #19383 ) ;
#76462 = CARTESIAN_POINT ( 'NONE',  ( -2.749484708945287181, 1420.045225311068180, 186.0761315375977176 ) ) ;
#76463 = CARTESIAN_POINT ( 'NONE',  ( 7.910841848800000520, 1423.398885000399787, 212.8692358303489982 ) ) ;
#76464 = CARTESIAN_POINT ( 'NONE',  ( -24.42787553970000047, 1439.418188418060026, 210.9954768190879975 ) ) ;
#76466 = CARTESIAN_POINT ( 'NONE',  ( -3.320856779727160202, 1454.266511067670081, 199.1807039058840019 ) ) ;
#76465 = B_SPLINE_CURVE_WITH_KNOTS ( 'NONE', 3,
 ( #627, #86817, #86260, #103619, #102498, #10109, #77327, #44281, #67833, #34207, #103046, #25787, #17374, #26344, #42066, #101943, #78425, #9549, #60541, #25232, #51572, #59435, #76, #1180, #52132, #34758, #43719, #35311, #85154, #85706, #94662, #9001, #43174, #76217, #69497, #42613, #110362, #68946, #26917, #61107, #93546, #17934, #95222, #16819, #18484, #51020, #76766, #68391, #76016, #67092, #59241, #49184, #109086, #74937, #101751, #15534, #31255, #57589, #65996, #92263, #7704, #91713 ),
 .UNSPECIFIED., .F., .F.,
 ( 4, 2, 2, 2, 2, 2, 1, 1, 1, 1, 1, 2, 2, 2, 2, 2, 2, 2, 1, 1, 1, 2, 2, 2, 2, 2, 2, 1, 1, 1, 1, 2, 2, 2, 2, 2, 4 ),
 ( 0.000000000000000000, 0.06250000000010860757, 0.1250000000002172151, 0.1875000000003258227, 0.2187500000003799461, 0.2343750000004068135, 0.2421875000004203027, 0.2460937500004272693, 0.2480468750004305167, 0.2490234375004321821, 0.2495117187504330147, 0.2497558593754329592, 0.2500000000004328760, 0.3125000000004529155, 0.3750000000004730105, 0.4375000000004930500, 0.4687500000005025980, 0.4843750000005078160, 0.4921875000005098144, 0.4960937500005103695, 0.4980468750005100365, 0.4990234375005098699, 0.5000000000005097034, 0.6250000000003840261, 0.6875000000003212985, 0.7187500000002903233, 0.7343750000002747802, 0.7421875000002672307, 0.7460937500002634559, 0.7480468750002610134, 0.7490234375002594591, 0.7495117187502580158, 0.7500000000002566836, 0.8125000000001925127, 0.8750000000001283418, 0.9375000000000642819, 1.000000000000000000 ),
 .UNSPECIFIED. ) ;
#76467 = CARTESIAN_POINT ( 'NONE',  ( 2.146415212520000004, 1450.119370040659760, 182.3300074786979792 ) ) ;
#76468 = CARTESIAN_POINT ( 'NONE',  ( 7.340269731178259427, 1361.836778001474158, 210.6218459616987957 ) ) ;
#76469 = CARTESIAN_POINT ( 'NONE',  ( -30.16373308232411787, 1510.076423030737942, 210.1342399186210628 ) ) ;
#76471 = ORIENTED_EDGE ( 'NONE', *, *, #67080, .F. ) ;
#76470 = CARTESIAN_POINT ( 'NONE',  ( -2.797080001758770053E-09, 1414.990986343060058, 244.4381637399740157 ) ) ;
#76472 = ORIENTED_EDGE ( 'NONE', *, *, #18796, .T. ) ;
#76473 = CARTESIAN_POINT ( 'NONE',  ( -11.83258938619150058, 1430.066262795869989, 149.4976403726300305 ) ) ;
#76474 = CARTESIAN_POINT ( 'NONE',  ( -21.58852250170129849, 1507.326192596420015, 209.4237101338769946 ) ) ;
#76475 = CARTESIAN_POINT ( 'NONE',  ( -104.3512419375300055, 1378.528619065190014, 309.1652050167789980 ) ) ;
#76476 = CARTESIAN_POINT ( 'NONE',  ( -110.0628895161599985, 1384.915043845459877, 296.9512959549039692 ) ) ;
#76478 = EDGE_CURVE ( 'NONE', #63483, #81290, #87687, .T. ) ;
#76477 = CARTESIAN_POINT ( 'NONE',  ( -103.9363405334473356, 1366.350733876288359, 309.3918666868620448 ) ) ;
#76479 = CARTESIAN_POINT ( 'NONE',  ( 1.191524307911317804, 1526.382868172864164, 239.2353018730791518 ) ) ;
#76480 = DIRECTION ( 'NONE',  ( -0.6736849260863841948, 0.000000000000000000, 0.7390186874254148774 ) ) ;
#76481 = CARTESIAN_POINT ( 'NONE',  ( -17.42808535260000014, 1431.113060387329824, 201.5089395310880036 ) ) ;
#76482 = CARTESIAN_POINT ( 'NONE',  ( 8.988338641399998608, 1366.896325247149889, 207.6218459616989946 ) ) ;
#76483 = CARTESIAN_POINT ( 'NONE',  ( -10.25042859964420039, 1447.425305017889968, 210.5414048152140083 ) ) ;
#76484 = CARTESIAN_POINT ( 'NONE',  ( -10.63393819740299939, 1406.766374306999978, 267.1884441437949818 ) ) ;
#76485 = CARTESIAN_POINT ( 'NONE',  ( -14.32024519749940161, 1436.001929727169909, 149.9627363249020107 ) ) ;
#76486 = ORIENTED_EDGE ( 'NONE', *, *, #43179, .F. ) ;
#76487 = CARTESIAN_POINT ( 'NONE',  ( 2.143764089412641738, 1525.848198008145346, 241.3832866758193632 ) ) ;
#76488 = CARTESIAN_POINT ( 'NONE',  ( 13.24110963769999927, 1443.105933592210022, 187.8974491670979887 ) ) ;
#76489 = ORIENTED_EDGE ( 'NONE', *, *, #36038, .F. ) ;
#76490 = VECTOR ( 'NONE', #48920, 1000.000000000000000 ) ;
#76491 = ORIENTED_EDGE ( 'NONE', *, *, #63978, .F. ) ;
#76492 = CYLINDRICAL_SURFACE ( 'NONE', #109194, 1.000000000000003553 ) ;
#76493 = DIRECTION ( 'NONE',  ( -0.7071067657658171024, -0.01693754150844739917, 0.7069039124915460492 ) ) ;
#76494 = CARTESIAN_POINT ( 'NONE',  ( 6.946748518954999341, 1516.983995446890049, 214.1250666973070054 ) ) ;
#76495 = CARTESIAN_POINT ( 'NONE',  ( 5.121512540634999944, 1511.279956263560052, 217.0557608965669658 ) ) ;
#76496 = CIRCLE ( 'NONE', #12152, 2.000000000000000000 ) ;
#76497 = CARTESIAN_POINT ( 'NONE',  ( -17.02086975159189919, 1479.748893642479970, 228.8538236634169891 ) ) ;
#76498 = ORIENTED_EDGE ( 'NONE', *, *, #48415, .F. ) ;
#76499 = FACE_OUTER_BOUND ( 'NONE', #12136, .T. ) ;
#76500 = COLOUR_RGB ( '', 0.09019608, 0.27058824, 0.51372549) ;
#76501 = CARTESIAN_POINT ( 'NONE',  ( 7.325541787135000149, 1516.710692850270107, 204.1167749238070144 ) ) ;
#76502 = CARTESIAN_POINT ( 'NONE',  ( -27.26565262369999942, 1508.025370090229899, 204.2545478268079933 ) ) ;
#76503 = CARTESIAN_POINT ( 'NONE',  ( -1.523967229539999746, 1477.816987455330036, 230.7230646392980020 ) ) ;
#76504 = CARTESIAN_POINT ( 'NONE',  ( -29.89848049817870290, 1384.555929490659992, 205.5315682105770065 ) ) ;
#76505 = CARTESIAN_POINT ( 'NONE',  ( -2.589228330169999648, 1407.329175972530265, 196.2821412641980316 ) ) ;
#76507 = VERTEX_POINT ( 'NONE', #64808 ) ;
#76506 = CARTESIAN_POINT ( 'NONE',  ( -10.96015512746500065, 1512.830284628050094, 193.2119433744669834 ) ) ;
#76508 = CARTESIAN_POINT ( 'NONE',  ( -25.47454973720070370, 1449.924923776209880, 210.2506139651870001 ) ) ;
#76509 = CARTESIAN_POINT ( 'NONE',  ( 26.53588231950000065, 1469.248395150029864, 209.7046586876050185 ) ) ;
#76510 = CARTESIAN_POINT ( 'NONE',  ( -11.83466398015730725, 1521.951704408389787, 228.0588040460849015 ) ) ;
#76511 = CARTESIAN_POINT ( 'NONE',  ( -10.37387122812170048, 1479.853456459100244, 210.7819233421560057 ) ) ;
#76512 = CARTESIAN_POINT ( 'NONE',  ( -24.74905961449999836, 1435.859003228780239, 137.6504519889980145 ) ) ;
#76513 = CIRCLE ( 'NONE', #28245, 4079.102317997178943 ) ;
#76514 = CARTESIAN_POINT ( 'NONE',  ( -4.995623491025000362, 1516.636036526019780, 210.8344906863870278 ) ) ;
#76515 = CARTESIAN_POINT ( 'NONE',  ( -68.14024846860000650, 1379.746849200649876, 278.7967730264589932 ) ) ;
#76516 = CARTESIAN_POINT ( 'NONE',  ( -14.95253593330000008, 1415.584822001330167, 226.8728895648979744 ) ) ;
#76517 = CARTESIAN_POINT ( 'NONE',  ( -29.55269881708354873, 1525.821544997590991, 221.1141083160998448 ) ) ;
#76518 =( BOUNDED_CURVE ( )  B_SPLINE_CURVE ( 3, ( #95010, #62553, #96673, #95559 ),
 .UNSPECIFIED., .F., .F. ) 
 B_SPLINE_CURVE_WITH_KNOTS ( ( 4, 4 ),
 ( 4.177898496273999562, 5.246908467225170014 ),
 .UNSPECIFIED. ) 
 CURVE ( )  GEOMETRIC_REPRESENTATION_ITEM ( )  RATIONAL_B_SPLINE_CURVE ( ( 1.000000000000000000, 0.9070139350561767788, 0.9070139350561767788, 1.000000000000000000 ) ) 
 REPRESENTATION_ITEM ( '' )  );
#76519 = CARTESIAN_POINT ( 'NONE',  ( 4.028611221114998919, 1516.744381837270112, 207.9874879615069858 ) ) ;
#76520 = ORIENTED_EDGE ( 'NONE', *, *, #2344, .T. ) ;
#76521 = CARTESIAN_POINT ( 'NONE',  ( -2.587453686403140107, 1451.957470480449956, 184.6860871491240061 ) ) ;
#76522 = CARTESIAN_POINT ( 'NONE',  ( -12.81728032640000059, 1415.366301205729997, 228.1481425647979790 ) ) ;
#76523 = FACE_OUTER_BOUND ( 'NONE', #81673, .T. ) ;
#76524 = VERTEX_POINT ( 'NONE', #107872 ) ;
#76525 = DIRECTION ( 'NONE',  ( 0.6677681214262592979, -0.7443693545591762994, 0.000000000000000000 ) ) ;
#76526 = CARTESIAN_POINT ( 'NONE',  ( -8.633016166312110329, 1493.573642282540050, 200.3527115318569827 ) ) ;
#76527 = CARTESIAN_POINT ( 'NONE',  ( 12.75105367887320007, 1435.273936497249906, 150.5906040834139787 ) ) ;
#76528 = CARTESIAN_POINT ( 'NONE',  ( -4.119144758445948185, 1441.439880715936170, 184.2549068806088712 ) ) ;
#76529 = CARTESIAN_POINT ( 'NONE',  ( -17.26522478369999902, 1417.948008348349958, 205.1437062577190034 ) ) ;
#76530 = CARTESIAN_POINT ( 'NONE',  ( -2.157536728406358684, 1378.913060387289988, 210.3005136483567981 ) ) ;
#76531 = CARTESIAN_POINT ( 'NONE',  ( 5.537689631040000116, 1487.530061922989944, 199.3434706563589884 ) ) ;
#76532 = DIRECTION ( 'NONE',  ( -0.000000000000000000, -1.000000000000000000, -0.000000000000000000 ) ) ;
#76533 = CARTESIAN_POINT ( 'NONE',  ( 4.221427320000399774, 1441.605329825029912, 168.6675303822389935 ) ) ;
#76534 = CONICAL_SURFACE ( 'NONE', #64033, 23.69926344187880929, 1.195358426993359036 ) ;
#76536 = FACE_OUTER_BOUND ( 'NONE', #9722, .T. ) ;
#76535 = CARTESIAN_POINT ( 'NONE',  ( -1.121950782074999875, 1517.123342927159911, 214.1352753262870010 ) ) ;
#76537 = CARTESIAN_POINT ( 'NONE',  ( -8.859979363206980096, 1384.988067842360124, 218.6842175230869714 ) ) ;
#76538 = CARTESIAN_POINT ( 'NONE',  ( -3.453544863754999472, 1517.106845464700200, 216.4586906126469898 ) ) ;
#76539 = ORIENTED_EDGE ( 'NONE', *, *, #14782, .F. ) ;
#76540 = CARTESIAN_POINT ( 'NONE',  ( -12.45642918560000112, 1416.822692809430009, 194.7673859448979954 ) ) ;
#76541 = CARTESIAN_POINT ( 'NONE',  ( -2.480175250669919951, 1429.207669930499833, 200.0830571243679969 ) ) ;
#76542 = ORIENTED_EDGE ( 'NONE', *, *, #71827, .F. ) ;
#76543 = CARTESIAN_POINT ( 'NONE',  ( 1.308044573769999941, 1420.880219163630045, 182.9927263326979983 ) ) ;
#76544 = CARTESIAN_POINT ( 'NONE',  ( -113.4000000000000057, 1381.413060387289988, 304.2218459572590064 ) ) ;
#76545 = CARTESIAN_POINT ( 'NONE',  ( 3.143084115766277886, 1525.137906803777241, 176.7009701364783893 ) ) ;
#76546 = CARTESIAN_POINT ( 'NONE',  ( -7.544890056106759779, 1384.926148859619843, 219.0875905756669795 ) ) ;
#76547 = CARTESIAN_POINT ( 'NONE',  ( -11.36767047984990064, 1471.003751822059940, 208.1245920186299827 ) ) ;
#76548 = CARTESIAN_POINT ( 'NONE',  ( -4.166056713077788132, 1508.165813601425270, 220.6324487379284562 ) ) ;
#76549 = CARTESIAN_POINT ( 'NONE',  ( 17.21543977323896613, 1422.420158212175465, 226.7018114670726447 ) ) ;
#76550 = CARTESIAN_POINT ( 'NONE',  ( 18.11449771340117820, 1507.710592339239383, 230.4427339259977998 ) ) ;
#76551 = CARTESIAN_POINT ( 'NONE',  ( 8.983202878996561225, 1460.605128901860098, 205.0537694474210184 ) ) ;
#76552 = CARTESIAN_POINT ( 'NONE',  ( -2.493947715939999643, 1442.756953654919926, 150.6345094620980092 ) ) ;
#76553 = CARTESIAN_POINT ( 'NONE',  ( 45.41371203904640197, 1440.913060377029979, 265.9156451615399988 ) ) ;
#76555 = CARTESIAN_POINT ( 'NONE',  ( 2.283436972078669822E-15, 1391.413060387289988, 209.1218459572589836 ) ) ;
#76554 = CARTESIAN_POINT ( 'NONE',  ( -6.433661733563849516, 1419.885808465230184, 194.8545971097019844 ) ) ;
#76556 = CARTESIAN_POINT ( 'NONE',  ( 2.686147501205266686, 1526.329757971589288, 241.8500438829907182 ) ) ;
#76557 = VERTEX_POINT ( 'NONE', #22188 ) ;
#76558 = ORIENTED_EDGE ( 'NONE', *, *, #47228, .F. ) ;
#76559 = CARTESIAN_POINT ( 'NONE',  ( -5.512326787969999309, 1497.963565169690128, 220.3136703888989985 ) ) ;
#76560 = AXIS2_PLACEMENT_3D ( 'NONE', #89227, #12523, #46701 ) ;
#76561 = CARTESIAN_POINT ( 'NONE',  ( -10.26697147908009811, 1506.473665945047060, 228.6001773789730862 ) ) ;
#76562 = CARTESIAN_POINT ( 'NONE',  ( -27.78452750869999832, 1508.000976251930069, 210.4681927209580010 ) ) ;
#76563 = CARTESIAN_POINT ( 'NONE',  ( 8.873274052869998485, 1425.079924521729936, 195.6592732233990262 ) ) ;
#76564 = VECTOR ( 'NONE', #27972, 1000.000000000000227 ) ;
#76565 = CARTESIAN_POINT ( 'NONE',  ( -3.897008745070269509, 1426.015660802909224, 186.0506595318446728 ) ) ;
#76566 = CARTESIAN_POINT ( 'NONE',  ( 10.50320544853759941, 1422.350872714849856, 211.5057683799360007 ) ) ;
#76567 = AXIS2_PLACEMENT_3D ( 'NONE', #49869, #7844, #17880 ) ;
#76568 = CARTESIAN_POINT ( 'NONE',  ( -4.635490668534062664, 1377.970142912541405, 204.0379736860714956 ) ) ;
#76569 = CARTESIAN_POINT ( 'NONE',  ( 13.31050689230000117, 1414.983771850430003, 197.8499836737979933 ) ) ;
#76571 = ADVANCED_FACE ( 'NONE', ( #40116 ), #103606, .F. ) ;
#76570 = CARTESIAN_POINT ( 'NONE',  ( -61.79250326028719797, 1383.794347301399966, 283.5912797454389533 ) ) ;
#76572 = AXIS2_PLACEMENT_3D ( 'NONE', #69531, #18515, #78456 ) ;
#76573 = CARTESIAN_POINT ( 'NONE',  ( 16.43064545349999861, 1451.907610170929729, 148.9104844442979925 ) ) ;
#76574 = CARTESIAN_POINT ( 'NONE',  ( -27.36889314738404977, 1509.257027982647969, 212.0753268043458775 ) ) ;
#76575 = CARTESIAN_POINT ( 'NONE',  ( 11.12768290801760074, 1491.440051377930104, 209.9868098767680067 ) ) ;
#76577 = ORIENTED_EDGE ( 'NONE', *, *, #93250, .F. ) ;
#76576 = CARTESIAN_POINT ( 'NONE',  ( 23.71809045669999705, 1508.481479934130220, 195.1786701157980133 ) ) ;
#76578 = VECTOR ( 'NONE', #61095, 1000.000000000000000 ) ;
#76579 = CARTESIAN_POINT ( 'NONE',  ( 32.40058737600813998, 1524.130440953581001, 216.9356993550890707 ) ) ;
#76580 = CARTESIAN_POINT ( 'NONE',  ( -52.43938806090000071, 1381.597557294350281, 231.3376853649589862 ) ) ;
#76581 = CARTESIAN_POINT ( 'NONE',  ( 0.7162863658319988946, 1429.709265593189912, 217.4063670190490143 ) ) ;
#76582 = EDGE_CURVE ( 'NONE', #2790, #43895, #35266, .T. ) ;
#76583 = ORIENTED_EDGE ( 'NONE', *, *, #91241, .F. ) ;
#76584 = ORIENTED_EDGE ( 'NONE', *, *, #53184, .F. ) ;
#76585 = CARTESIAN_POINT ( 'NONE',  ( -22.08622291482314282, 1518.913060387330006, 233.8253038720786776 ) ) ;
#76586 = CARTESIAN_POINT ( 'NONE',  ( -113.4000000000000057, 1381.413060387289988, 304.2218459572590064 ) ) ;
#76587 = CARTESIAN_POINT ( 'NONE',  ( 38.97238355074230043, 1439.678263993750079, 136.6980159596599833 ) ) ;
#76589 = DIRECTION ( 'NONE',  ( 0.000000000000000000, 0.000000000000000000, 1.000000000000000000 ) ) ;
#76588 = CARTESIAN_POINT ( 'NONE',  ( -8.301987938657498844, 1519.551704408389924, 185.0111222839169898 ) ) ;
#76590 = CARTESIAN_POINT ( 'NONE',  ( 11.56134810898769949, 1480.201629797219994, 211.4332244987409979 ) ) ;
#76591 = CARTESIAN_POINT ( 'NONE',  ( -108.0946408660000060, 1381.519821111719921, 298.2388064062590729 ) ) ;
#76592 = CARTESIAN_POINT ( 'NONE',  ( -21.53981368633734661, 1523.542365884046603, 234.3096115065273750 ) ) ;
#76593 = CARTESIAN_POINT ( 'NONE',  ( -11.56020812217769489, 1434.913448849900533, 151.4031740279024802 ) ) ;
#76594 = CARTESIAN_POINT ( 'NONE',  ( -16.08708462094059755, 1508.551704408389924, 213.7294159091019878 ) ) ;
#76595 = CIRCLE ( 'NONE', #21169, 7.016581249619902039 ) ;
#76596 = CARTESIAN_POINT ( 'NONE',  ( 4.970581720019999317, 1409.086636925830135, 187.4197542652979962 ) ) ;
#76597 = CARTESIAN_POINT ( 'NONE',  ( 2.819396220834549993, 1486.922886763410133, 197.5136065300459904 ) ) ;
#76598 = CARTESIAN_POINT ( 'NONE',  ( 5.628941412700790181, 1434.147628282120195, 202.5779479739449869 ) ) ;
#76599 = CARTESIAN_POINT ( 'NONE',  ( -3.697587031422459702, 1440.988254563350210, 157.0261807637750167 ) ) ;
#76600 = CARTESIAN_POINT ( 'NONE',  ( -21.40326933649999575, 1452.165641750530085, 142.6046343431980006 ) ) ;
#76601 = CARTESIAN_POINT ( 'NONE',  ( 0.9755134735189999740, 1466.582224391130012, 235.3782024704980245 ) ) ;
#76602 = ORIENTED_EDGE ( 'NONE', *, *, #54960, .T. ) ;
#76603 = CARTESIAN_POINT ( 'NONE',  ( 22.16303642491469716, 1474.378995651259856, 210.0398025965960187 ) ) ;
#76604 = DIRECTION ( 'NONE',  ( 0.9455185755993178454, 0.000000000000000000, -0.3255681544571537578 ) ) ;
#76605 = CARTESIAN_POINT ( 'NONE',  ( 3.066583199566000534E-32, 1507.508085020990166, 209.1218459616989946 ) ) ;
#76606 = DIRECTION ( 'NONE',  ( -1.407418274235000032E-17, -1.000000000000000000, 2.576261870300899651E-17 ) ) ;
#76607 = CARTESIAN_POINT ( 'NONE',  ( -5.657316317590000310, 1475.078194850989803, 204.3863535599990087 ) ) ;
#76608 = B_SPLINE_CURVE_WITH_KNOTS ( 'NONE', 3,
 ( #8222, #42388, #67615, #100630, #23376, #83291, #75995, #40187, #25569, #108497, #84929, #68181, #83841, #31782, #101728, #100096, #102288, #16600, #6589, #14966, #91689, #41840 ),
 .UNSPECIFIED., .F., .F.,
 ( 4, 3, 3, 3, 3, 3, 3, 4 ),
 ( -9.467922507749999994, -8.528615746326670077, -7.393658045039350313, -7.008072864428970483, -6.043576188583889675, -5.200792916686279632, -4.480935144650000090, -4.388980137787560132 ),
 .UNSPECIFIED. ) ;
#76609 = CARTESIAN_POINT ( 'NONE',  ( -2.295465748574410035E-11, 1470.383016079100116, 255.0304770405179511 ) ) ;
#76610 = CARTESIAN_POINT ( 'NONE',  ( 0.6219649428874711727, 1515.589553501007686, 213.1416252726859852 ) ) ;
#76611 = CARTESIAN_POINT ( 'NONE',  ( -1.552659050370000182, 1415.628674276829770, 227.5866819053980237 ) ) ;
#76612 = CARTESIAN_POINT ( 'NONE',  ( -3.037920316420000155, 1417.285933716130103, 233.5158617220979806 ) ) ;
#76613 = CARTESIAN_POINT ( 'NONE',  ( -2.194372809809999936, 1475.747898641790016, 198.6287671099989893 ) ) ;
#76614 = CARTESIAN_POINT ( 'NONE',  ( -106.5011323819999944, 1389.176690760049951, 308.8516233391590049 ) ) ;
#76615 = CARTESIAN_POINT ( 'NONE',  ( -0.3887204637380738403, 1485.756074821177890, 181.8627589278759729 ) ) ;
#76616 = CARTESIAN_POINT ( 'NONE',  ( 4.670493445319249481, 1358.850376296546983, 209.6218459617033432 ) ) ;
#76617 = CARTESIAN_POINT ( 'NONE',  ( -45.91620460975560292, 1438.463282072589891, 268.4996293049820224 ) ) ;
#76618 = CARTESIAN_POINT ( 'NONE',  ( 13.85848044686079916, 1509.281222645870002, 234.2549437311519966 ) ) ;
#76619 = CARTESIAN_POINT ( 'NONE',  ( -7.634073948139999288, 1426.135584679400154, 206.2171369772389653 ) ) ;
#76620 = ORIENTED_EDGE ( 'NONE', *, *, #109531, .F. ) ;
#76621 = CARTESIAN_POINT ( 'NONE',  ( 7.326072144144999854, 1516.714320817460020, 208.3685457967989976 ) ) ;
#76622 = CARTESIAN_POINT ( 'NONE',  ( -5.429844217520000349, 1436.698278606120084, 154.7014901950980175 ) ) ;
#76623 = CARTESIAN_POINT ( 'NONE',  ( -7.032901808474493421, 1471.052634343683849, 216.4002283616353566 ) ) ;
#76624 = CARTESIAN_POINT ( 'NONE',  ( 7.530331464701590427, 1425.809918452410102, 212.2263711254659881 ) ) ;
#76625 = CARTESIAN_POINT ( 'NONE',  ( -25.77240273999639797, 1452.013063856540157, 135.1833753210919724 ) ) ;
#76626 = VERTEX_POINT ( 'NONE', #1870 ) ;
#76627 = CARTESIAN_POINT ( 'NONE',  ( 18.32607164059999860, 1423.244042729530065, 231.9815855802980025 ) ) ;
#76629 = CARTESIAN_POINT ( 'NONE',  ( 14.54643167989999952, 1470.812340170230073, 194.6419432318980114 ) ) ;
#76628 = CARTESIAN_POINT ( 'NONE',  ( -10.94188635223400041, 1492.630926138539962, 207.2829489295590122 ) ) ;
#76630 = CARTESIAN_POINT ( 'NONE',  ( -6.281421547999999966, 1461.340667028890039, 207.5740607322589995 ) ) ;
#76631 = CARTESIAN_POINT ( 'NONE',  ( -4.138543392800874798, 1515.492058412108918, 207.2788837464903509 ) ) ;
#76632 = CARTESIAN_POINT ( 'NONE',  ( 7.223461847829999449, 1425.153791230060051, 192.5261047659990084 ) ) ;
#76633 = CARTESIAN_POINT ( 'NONE',  ( 3.873898975603070394, 1468.026799752889929, 218.3319420452740189 ) ) ;
#76634 = DIRECTION ( 'NONE',  ( 0.8090169943749507819, -0.000000000000000000, 0.5877852522924685852 ) ) ;
#76635 = ORIENTED_EDGE ( 'NONE', *, *, #40496, .F. ) ;
#76636 = CARTESIAN_POINT ( 'NONE',  ( -6.685506928249539627, 1409.565136544780216, 270.3700927272910235 ) ) ;
#76637 = CARTESIAN_POINT ( 'NONE',  ( 8.813846681050000242, 1418.026211838229756, 230.6754341397980284 ) ) ;
#76638 = CARTESIAN_POINT ( 'NONE',  ( 8.222217444529830388, 1435.932500431779999, 206.6299244032960019 ) ) ;
#76639 = ORIENTED_EDGE ( 'NONE', *, *, #106228, .T. ) ;
#76640 = VERTEX_POINT ( 'NONE', #77453 ) ;
#76641 = CARTESIAN_POINT ( 'NONE',  ( -23.50732105891940193, 1410.149254099409973, 209.9394804832799935 ) ) ;
#76642 = B_SPLINE_CURVE_WITH_KNOTS ( 'NONE', 3,
 ( #58621, #35057, #8188, #32839, #52436, #67032 ),
 .UNSPECIFIED., .F., .F.,
 ( 4, 2, 4 ),
 ( 0.000000000000000000, 0.5000000000000000000, 1.000000000000000000 ),
 .UNSPECIFIED. ) ;
#76643 = CARTESIAN_POINT ( 'NONE',  ( -11.00421634129999937, 1481.586355903290041, 208.5478235484490028 ) ) ;
#76644 = CARTESIAN_POINT ( 'NONE',  ( -102.6425412143000102, 1375.179104070690073, 310.0986724762790345 ) ) ;
#76645 = FACE_OUTER_BOUND ( 'NONE', #44613, .T. ) ;
#76646 = TOROIDAL_SURFACE ( 'NONE', #22990, 2.000000000000000000, 1.000000000000000000 ) ;
#76647 = CARTESIAN_POINT ( 'NONE',  ( -20.57476409830681874, 1436.447616954657860, 144.8090829293095680 ) ) ;
#76648 = CARTESIAN_POINT ( 'NONE',  ( 4.678985465398590726, 1508.551704408389924, 213.1800342119370271 ) ) ;
#76649 = EDGE_CURVE ( 'NONE', #40367, #32267, #583, .T. ) ;
#76650 = CARTESIAN_POINT ( 'NONE',  ( 35.58359713094720433, 1463.005569991589709, 268.8138335405850512 ) ) ;
#76651 = EDGE_CURVE ( 'NONE', #56028, #13558, #84639, .T. ) ;
#76652 = CARTESIAN_POINT ( 'NONE',  ( -4.426491236972309729, 1508.728286123109910, 204.9619822988670137 ) ) ;
#76653 = CARTESIAN_POINT ( 'NONE',  ( -5.842412022809999605, 1427.301855271020258, 202.1826430572290008 ) ) ;
#76654 = CARTESIAN_POINT ( 'NONE',  ( -6.949265684145000677, 1517.089216728169959, 205.6689289091970068 ) ) ;
#76655 = ORIENTED_EDGE ( 'NONE', *, *, #40020, .F. ) ;
#76656 = CARTESIAN_POINT ( 'NONE',  ( 18.22805055419890152, 1459.311389626190021, 227.8763770136359881 ) ) ;
#76657 = CARTESIAN_POINT ( 'NONE',  ( 1.501528787941759813, 1445.491189390299951, 199.1508277339860058 ) ) ;
#76658 = LINE ( 'NONE', #93444, #15792 ) ;
#76659 = EDGE_LOOP ( 'NONE', ( #93704, #71697, #13998, #62356, #89847 ) ) ;
#76660 = CARTESIAN_POINT ( 'NONE',  ( 2.500000005550000015, 1448.575512279979876, 182.8814919026980021 ) ) ;
#76661 = EDGE_CURVE ( 'NONE', #12048, #93687, #39221, .T. ) ;
#76662 = CARTESIAN_POINT ( 'NONE',  ( 27.02609346130070023, 1451.901655341519927, 135.4159119962619968 ) ) ;
#76663 = EDGE_CURVE ( 'NONE', #70222, #60117, #106076, .T. ) ;
#76664 = CARTESIAN_POINT ( 'NONE',  ( -2.968682043993700059, 1508.551704408389924, 214.0622169246639714 ) ) ;
#76665 = CARTESIAN_POINT ( 'NONE',  ( -9.787614191920001261, 1388.284344778709965, 200.9830834995690054 ) ) ;
#76666 = CARTESIAN_POINT ( 'NONE',  ( 7.431286581940000247, 1422.782057261100135, 195.6224716579989718 ) ) ;
#76667 = CARTESIAN_POINT ( 'NONE',  ( -3.114972218757349864, 1433.209950781340012, 218.1554066274329955 ) ) ;
#76668 = CARTESIAN_POINT ( 'NONE',  ( 27.23063139319997816, 1443.913060387329097, 161.8596747266978753 ) ) ;
#76669 = CARTESIAN_POINT ( 'NONE',  ( 4.180008225707200431, 1409.059029491030060, 187.6061561084030131 ) ) ;
#76671 = DIRECTION ( 'NONE',  ( 0.8775825618903710934, -0.000000000000000000, 0.4794255386042062250 ) ) ;
#76670 = CARTESIAN_POINT ( 'NONE',  ( 2.446918720040000217, 1417.581962241529936, 234.9465420055979905 ) ) ;
#76672 = CARTESIAN_POINT ( 'NONE',  ( -29.99620953741480278, 1524.382868172863937, 219.7462484079463252 ) ) ;
#76673 = CARTESIAN_POINT ( 'NONE',  ( -12.13826128220000022, 1378.628687927729970, 212.1996395817189978 ) ) ;
#76674 = CARTESIAN_POINT ( 'NONE',  ( 15.29896286170615305, 1422.370102515510780, 230.0239554351165907 ) ) ;
#76675 = ORIENTED_EDGE ( 'NONE', *, *, #28297, .F. ) ;
#76676 = CARTESIAN_POINT ( 'NONE',  ( -32.23393008313284724, 1523.382868172864164, 201.4036600223109588 ) ) ;
#76677 = CARTESIAN_POINT ( 'NONE',  ( 11.86607448679350085, 1432.335963006760039, 150.0622438253739972 ) ) ;
#76678 = CARTESIAN_POINT ( 'NONE',  ( 32.31945039880172033, 1524.082740465118377, 202.1440840643585943 ) ) ;
#76679 = CARTESIAN_POINT ( 'NONE',  ( -11.74761972249999964, 1388.317445593919956, 202.1816773684589919 ) ) ;
#76680 = CARTESIAN_POINT ( 'NONE',  ( 9.440304233305520043, 1422.746543296229902, 211.8015284199159964 ) ) ;
#76681 = EDGE_CURVE ( 'NONE', #65089, #74815, #100710, .T. ) ;
#76682 = DIRECTION ( 'NONE',  ( -1.000000000000000000, 0.000000000000000000, 0.000000000000000000 ) ) ;
#76683 = CARTESIAN_POINT ( 'NONE',  ( 1.245016291430000033, 1431.187216657390081, 218.1259619513589882 ) ) ;
#76684 = CARTESIAN_POINT ( 'NONE',  ( -42.15865170690000241, 1450.809155637750109, 271.1218459616979999 ) ) ;
#76685 = CARTESIAN_POINT ( 'NONE',  ( -8.859238207665629972, 1384.780024425459942, 218.6827953414510262 ) ) ;
#76686 = CARTESIAN_POINT ( 'NONE',  ( 11.49921796000000107, 1433.639916894349881, 151.2944310539980108 ) ) ;
#76687 = CARTESIAN_POINT ( 'NONE',  ( 23.42675388089999799, 1443.575607730780121, 234.3916895488980003 ) ) ;
#76688 = CARTESIAN_POINT ( 'NONE',  ( -9.655872537241959819, 1460.619437666070098, 208.6456940018040029 ) ) ;
#76689 = ADVANCED_FACE ( 'NONE', ( #108702 ), #99733, .T. ) ;
#76690 = CARTESIAN_POINT ( 'NONE',  ( 0.5992832621693802153, 1467.074120444730170, 235.5491957431187586 ) ) ;
#76691 = CARTESIAN_POINT ( 'NONE',  ( -1.842962215417937033, 1515.551704407335137, 213.1059277167897505 ) ) ;
#76692 = CARTESIAN_POINT ( 'NONE',  ( -14.49383181622579997, 1422.099016211560183, 229.4564907068830166 ) ) ;
#76693 = CARTESIAN_POINT ( 'NONE',  ( 12.86122366611430046, 1416.830086716310007, 221.8629622564060071 ) ) ;
#76694 = PLANE ( 'NONE',  #23425 ) ;
#76695 = CARTESIAN_POINT ( 'NONE',  ( -25.85060555058009868, 1509.854941346010037, 193.0608776564500317 ) ) ;
#76696 = CARTESIAN_POINT ( 'NONE',  ( -8.105593519943804282, 1425.120261978882354, 209.5236776171163910 ) ) ;
#76697 = FACE_OUTER_BOUND ( 'NONE', #28035, .T. ) ;
#76698 = CARTESIAN_POINT ( 'NONE',  ( -41.66768200349253704, 1443.241368483788392, 135.6286826123361777 ) ) ;
#76699 = B_SPLINE_CURVE_WITH_KNOTS ( 'NONE', 5,
 ( #7944, #91953, #109325, #42113, #101992, #40996 ),
 .UNSPECIFIED., .F., .F.,
 ( 6, 6 ),
 ( 0.000000000000000000, 1.000000000000000000 ),
 .UNSPECIFIED. ) ;
#76700 = CARTESIAN_POINT ( 'NONE',  ( -16.27387329549090111, 1383.857350287579948, 219.5485982243399974 ) ) ;
#76701 = CARTESIAN_POINT ( 'NONE',  ( -11.04413905111285565, 1433.699474062253785, 151.7296044286115944 ) ) ;
#76702 = CARTESIAN_POINT ( 'NONE',  ( 9.992001597533901602, 1491.422526970020044, 188.4943246393440006 ) ) ;
#76703 = CARTESIAN_POINT ( 'NONE',  ( -4.610938249504999753, 1516.815231249920089, 213.1623732742069990 ) ) ;
#76704 = CARTESIAN_POINT ( 'NONE',  ( -16.16672696929999731, 1420.120271228960064, 210.5293282507990114 ) ) ;
#76705 = CARTESIAN_POINT ( 'NONE',  ( 0.1715556276115110246, 1479.416462729990144, 182.1194568275189738 ) ) ;
#76707 = VERTEX_POINT ( 'NONE', #100302 ) ;
#76706 = CARTESIAN_POINT ( 'NONE',  ( -7.491155460717596526, 1414.913060387329779, 194.4095434935337039 ) ) ;
#76708 = CARTESIAN_POINT ( 'NONE',  ( 1.436439550961320810, 1526.373507135059526, 178.7441892156120389 ) ) ;
#76709 = AXIS2_PLACEMENT_3D ( 'NONE', #73046, #44688, #55712 ) ;
#76710 = CARTESIAN_POINT ( 'NONE',  ( -5.389719915088219793, 1440.971386074470047, 154.8246291213590098 ) ) ;
#76711 = LINE ( 'NONE', #68896, #46135 ) ;
#76712 = EDGE_CURVE ( 'NONE', #75505, #46627, #53739, .T. ) ;
#76713 = CARTESIAN_POINT ( 'NONE',  ( -39.34220581718710008, 1449.349331648840234, 134.0999999980729740 ) ) ;
#76714 = CARTESIAN_POINT ( 'NONE',  ( -109.8951077769999927, 1384.900382187740206, 297.0284516700590416 ) ) ;
#76715 = VERTEX_POINT ( 'NONE', #49911 ) ;
#76716 = B_SPLINE_SURFACE_WITH_KNOTS ( 'NONE', 5, 5, ( 
 ( #70993, #9389, #11053, #79363, #27292, #102872 ),
 ( #44108, #60923, #45224, #79915, #77701, #103427 ),
 ( #61473, #96151, #86095, #105110, #62601, #2677 ),
 ( #95600, #43552, #36247, #96717, #11602, #18320 ),
 ( #19987, #10494, #34585, #68771, #18868, #44666 ),
 ( #94478, #17751, #51954, #2121, #26735, #95052 ),
 ( #52511, #86641, #78243, #1556, #39555, #21623 ),
 ( #29489, #107306, #30033, #5397, #73729, #3778 ),
 ( #28958, #38440, #55278, #99436, #106206, #89949 ) ),
 .UNSPECIFIED., .F., .F., .F.,
 ( 6, 3, 6 ),
 ( 6, 6 ),
 ( 10.57355459961640065, 12.71109754730000141, 14.84862610992340137 ),
 ( -0.0004205665836232139773, 2.000000000000000000 ),
 .UNSPECIFIED. ) ;
#76717 = CARTESIAN_POINT ( 'NONE',  ( -5.519031869189769068, 1391.701565166340060, 203.3041584978760170 ) ) ;
#76718 = CARTESIAN_POINT ( 'NONE',  ( 2.622430729442960740, 1523.621879633028811, 176.0901726876731459 ) ) ;
#76719 = CARTESIAN_POINT ( 'NONE',  ( -16.30669498860000033, 1415.087745006229852, 214.1831677707580184 ) ) ;
#76720 = CARTESIAN_POINT ( 'NONE',  ( -5.932239102140000497, 1391.913060387289988, 215.1144410137189880 ) ) ;
#76721 = CARTESIAN_POINT ( 'NONE',  ( -7.485129992997699766, 1435.765762796630042, 215.5585987123639882 ) ) ;
#76722 = CARTESIAN_POINT ( 'NONE',  ( -14.03642065347150236, 1457.296397347949778, 194.7061520102889745 ) ) ;
#76723 = CARTESIAN_POINT ( 'NONE',  ( -28.25086642335310216, 1508.135711581739997, 208.8579954535609886 ) ) ;
#76724 = CARTESIAN_POINT ( 'NONE',  ( -9.833393186232889605, 1517.051704408389924, 212.5077547680540135 ) ) ;
#76725 = CARTESIAN_POINT ( 'NONE',  ( -11.68975942279999991, 1391.913060387289988, 209.2396716380060013 ) ) ;
#76726 = CARTESIAN_POINT ( 'NONE',  ( -77.91803962745299827, 1385.149028708040078, 280.1724417302780239 ) ) ;
#76727 = CARTESIAN_POINT ( 'NONE',  ( 13.15726445491959851, 1416.851343895820037, 196.3340833728059920 ) ) ;
#76728 = CARTESIAN_POINT ( 'NONE',  ( 10.15095921180179950, 1426.119696681420010, 208.5876670455920134 ) ) ;
#76729 = ORIENTED_EDGE ( 'NONE', *, *, #32467, .T. ) ;
#76730 = AXIS2_PLACEMENT_3D ( 'NONE', #32481, #31914, #94023 ) ;
#76731 = CARTESIAN_POINT ( 'NONE',  ( -32.69005726390000177, 1451.771678911430172, 135.1859641189979868 ) ) ;
#76732 = B_SPLINE_CURVE_WITH_KNOTS ( 'NONE', 5,
 ( #92815, #58681, #94454, #34011, #77679, #86075 ),
 .UNSPECIFIED., .F., .F.,
 ( 6, 6 ),
 ( -93.45893461050000894, -23.20786975740000457 ),
 .UNSPECIFIED. ) ;
#76733 = CARTESIAN_POINT ( 'NONE',  ( 16.90742463042001376, 1442.831169986190844, 162.4348201727408991 ) ) ;
#76735 = ORIENTED_EDGE ( 'NONE', *, *, #53067, .T. ) ;
#76734 = CARTESIAN_POINT ( 'NONE',  ( 15.20279577643499991, 1514.921193718960012, 194.6261569368670337 ) ) ;
#76736 = CARTESIAN_POINT ( 'NONE',  ( 1.762362329279999917, 1472.996463562990130, 219.1807010226990258 ) ) ;
#76737 = AXIS2_PLACEMENT_3D ( 'NONE', #107575, #30861, #105946 ) ;
#76738 = CARTESIAN_POINT ( 'NONE',  ( 26.80001153169999739, 1509.848937414829834, 219.2969692978980163 ) ) ;
#76739 = CARTESIAN_POINT ( 'NONE',  ( -8.537163784377359121, 1364.215151872246452, 210.6218459617142003 ) ) ;
#76740 = CARTESIAN_POINT ( 'NONE',  ( -6.949448346310000524, 1495.994811745590141, 200.2534193484290199 ) ) ;
#76741 = CARTESIAN_POINT ( 'NONE',  ( 40.12840166341722181, 1450.023108907809046, 269.6125932357766146 ) ) ;
#76742 = CARTESIAN_POINT ( 'NONE',  ( 13.04207810306199988, 1409.368499790489750, 192.3005055522939983 ) ) ;
#76743 = CARTESIAN_POINT ( 'NONE',  ( 5.492330840890000232, 1396.104856806630096, 219.0480561951579830 ) ) ;
#76744 = CARTESIAN_POINT ( 'NONE',  ( 1.797565579259999824, 1415.903556500329842, 232.4419632410979943 ) ) ;
#76745 = CARTESIAN_POINT ( 'NONE',  ( 5.845440260250000186, 1447.515577236790023, 201.5716352439589798 ) ) ;
#76746 = CARTESIAN_POINT ( 'NONE',  ( -22.14848735670008395, 1507.850285361328133, 225.9298081188978813 ) ) ;
#76747 = CARTESIAN_POINT ( 'NONE',  ( -9.860907387307680239, 1368.605983359357424, 208.3718459617010978 ) ) ;
#76748 = CARTESIAN_POINT ( 'NONE',  ( -3.264929865090000050, 1455.156803674389948, 200.1463034570790001 ) ) ;
#76749 = ADVANCED_FACE ( 'NONE', ( #75666 ), #61627, .F. ) ;
#76750 = CARTESIAN_POINT ( 'NONE',  ( -6.562635860634999929, 1517.111322026010157, 206.2508942643169974 ) ) ;
#76751 = AXIS2_PLACEMENT_3D ( 'NONE', #51474, #18396, #103518 ) ;
#76753 = ADVANCED_FACE ( 'NONE', ( #34196 ), #80444, .F. ) ;
#76752 = CARTESIAN_POINT ( 'NONE',  ( 3.692944191490000083, 1446.771171062450094, 157.7765864143980252 ) ) ;
#76754 = B_SPLINE_SURFACE_WITH_KNOTS ( 'NONE', 5, 5, ( 
 ( #48857, #23621, #49392, #65649, #32586, #15201, #83520, #84077, #67855 ),
 ( #110384, #99765, #57805, #91929, #24152, #49939, #108176, #5738, #84622 ),
 ( #39880, #23055, #82982, #74047, #58342, #33119, #31468, #66761, #82440 ),
 ( #109842, #100862, #57264, #6273, #91391, #7918, #109300, #67307, #40423 ),
 ( #42088, #14669, #74599, #101403, #92467, #24695, #108735, #6814, #76237 ),
 ( #32026, #58891, #93024, #16296, #15738, #7375, #90826, #41539, #66215 ) ),
 .UNSPECIFIED., .F., .F., .F.,
 ( 6, 6 ),
 ( 6, 3, 6 ),
 ( 40.37450813634060154, 42.94666622520000487 ),
 ( 0.000000000000000000, 8.028376882759999944, 16.05675376549999811 ),
 .UNSPECIFIED. ) ;
#76755 = CARTESIAN_POINT ( 'NONE',  ( -2.500000000000000000, 1432.496417326090068, 157.4993228830980172 ) ) ;
#76756 = CARTESIAN_POINT ( 'NONE',  ( -0.8447098492589989460, 1496.888790194590001, 197.4916273440990153 ) ) ;
#76758 = VERTEX_POINT ( 'NONE', #18472 ) ;
#76757 = CARTESIAN_POINT ( 'NONE',  ( 1.474632190929999975, 1495.646359947390010, 220.9745027109989906 ) ) ;
#76759 = CARTESIAN_POINT ( 'NONE',  ( -18.64672481365220236, 1416.851343896850040, 208.5597484336410048 ) ) ;
#76760 = VERTEX_POINT ( 'NONE', #85694 ) ;
#76761 = CARTESIAN_POINT ( 'NONE',  ( 4.363122647529283249, 1409.354802298928007, 137.0999999980979851 ) ) ;
#76762 = CARTESIAN_POINT ( 'NONE',  ( -23.54254250629999845, 1430.351957812429873, 203.7587613919580178 ) ) ;
#76764 = CARTESIAN_POINT ( 'NONE',  ( 17.06148083016629968, 1410.141651639420161, 192.3522963160290260 ) ) ;
#76763 = CARTESIAN_POINT ( 'NONE',  ( -11.30526943965280040, 1426.459633991370083, 113.0055148446249973 ) ) ;
#76765 = CARTESIAN_POINT ( 'NONE',  ( 3.269184908365000197, 1516.940296199220029, 211.4060453336370244 ) ) ;
#76766 = CARTESIAN_POINT ( 'NONE',  ( 27.81444809721715927, 1509.996208870221835, 220.3660356682784141 ) ) ;
#76767 = CARTESIAN_POINT ( 'NONE',  ( 1.327771434284243934, 1450.718180199849940, 181.5841407004881773 ) ) ;
#76768 = FILL_AREA_STYLE ('',( #8442 ) ) ;
#76769 = CARTESIAN_POINT ( 'NONE',  ( 16.68893861061719974, 1509.501544872269960, 233.4110457454409868 ) ) ;
#76770 = CARTESIAN_POINT ( 'NONE',  ( 15.08870150073219207, 1461.900455706623006, 229.9510696313039091 ) ) ;
#76771 = CARTESIAN_POINT ( 'NONE',  ( -4.992905592350000532, 1391.642135889690053, 214.6650328897389954 ) ) ;
#76772 = CARTESIAN_POINT ( 'NONE',  ( -11.21638122688047368, 1413.913060387330006, 208.4170904300009397 ) ) ;
#76773 = ORIENTED_EDGE ( 'NONE', *, *, #25335, .F. ) ;
#76774 = CARTESIAN_POINT ( 'NONE',  ( 7.810568386166560018, 1396.185811445500121, 217.7799683602849825 ) ) ;
#76775 = CARTESIAN_POINT ( 'NONE',  ( 9.321518847882098058, 1461.563338749869899, 206.3986575956980118 ) ) ;
#76776 = CARTESIAN_POINT ( 'NONE',  ( -18.24693087420000381, 1457.532738398730089, 228.9631694535979989 ) ) ;
#76777 = ORIENTED_EDGE ( 'NONE', *, *, #19379, .T. ) ;
#76778 = ORIENTED_EDGE ( 'NONE', *, *, #49993, .F. ) ;
#76779 = CARTESIAN_POINT ( 'NONE',  ( -0.4039940643739989845, 1432.524637096890046, 203.3438492792190004 ) ) ;
#76780 = DIRECTION ( 'NONE',  ( -0.6081597637245996779, 0.7938146520356244018, 0.000000000000000000 ) ) ;
#76781 = CARTESIAN_POINT ( 'NONE',  ( -21.62164173326539895, 1521.951704408389787, 210.2163513712909833 ) ) ;
#76782 = CARTESIAN_POINT ( 'NONE',  ( -12.62024803869436340, 1417.247709474677322, 200.2862650437438674 ) ) ;
#76783 = ADVANCED_FACE ( 'NONE', ( #110350 ), #69687, .T. ) ;
#76784 = CARTESIAN_POINT ( 'NONE',  ( 4.290508133339999475, 1515.379316001789903, 209.4884471522930198 ) ) ;
#76785 = VECTOR ( 'NONE', #21823, 1000.000000000000114 ) ;
#76786 = CARTESIAN_POINT ( 'NONE',  ( 0.4794255386045085388, 1547.913060387330006, 209.9994285235883922 ) ) ;
#76787 = CARTESIAN_POINT ( 'NONE',  ( 26.86204993032690069, 1508.007394616730153, 206.2315948942269870 ) ) ;
#76788 = CARTESIAN_POINT ( 'NONE',  ( 3.783303485079999806, 1421.764240203399822, 183.6423304018649958 ) ) ;
#76789 = ADVANCED_FACE ( 'NONE', ( #97411 ), #72239, .F. ) ;
#76790 = CARTESIAN_POINT ( 'NONE',  ( 9.201685189691980682, 1450.874596308319951, 209.9835013892320035 ) ) ;
#76791 = CARTESIAN_POINT ( 'NONE',  ( -12.03143819960000016, 1391.727509755350184, 211.6223019673990109 ) ) ;
#76792 = CARTESIAN_POINT ( 'NONE',  ( -91.93393826891069409, 1384.846171626159958, 293.6354712203719828 ) ) ;
#76793 = EDGE_LOOP ( 'NONE', ( #24551, #5312, #2703, #36790 ) ) ;
#76794 = CARTESIAN_POINT ( 'NONE',  ( 7.326795523374999952, 1516.760434454289907, 203.3416138547669902 ) ) ;
#76795 = CARTESIAN_POINT ( 'NONE',  ( -5.011551406145000165, 1517.080322339569875, 208.3849417611969841 ) ) ;
#76796 = ORIENTED_EDGE ( 'NONE', *, *, #106350, .F. ) ;
#76798 = EDGE_CURVE ( 'NONE', #99771, #65489, #14359, .T. ) ;
#76797 = CARTESIAN_POINT ( 'NONE',  ( 11.78922831828120010, 1427.761296424969942, 147.5992861727949901 ) ) ;
#76799 = VECTOR ( 'NONE', #50440, 1000.000000000000000 ) ;
#76800 = CARTESIAN_POINT ( 'NONE',  ( 20.51182933999999847, 1507.864840975229981, 228.4145674124980303 ) ) ;
#76801 = ORIENTED_EDGE ( 'NONE', *, *, #67205, .T. ) ;
#76802 = CARTESIAN_POINT ( 'NONE',  ( -13.57674101270000122, 1415.245980409529921, 221.0231452625980069 ) ) ;
#76803 = CARTESIAN_POINT ( 'NONE',  ( -17.11746647137171706, 1443.086052842848176, 162.7559337440806644 ) ) ;
#76804 = DIRECTION ( 'NONE',  ( -0.000000000000000000, -1.000000000000000000, -0.000000000000000000 ) ) ;
#76805 = CARTESIAN_POINT ( 'NONE',  ( -10.15849568003170056, 1462.015375114950075, 208.6822598999149818 ) ) ;
#76806 = CARTESIAN_POINT ( 'NONE',  ( -6.719886790419999478, 1423.239095099330143, 186.8024023444980060 ) ) ;
#76807 = CIRCLE ( 'NONE', #41068, 11.71219856409999949 ) ;
#76808 = DIRECTION ( 'NONE',  ( -0.000000000000000000, -1.000000000000000000, -0.000000000000000000 ) ) ;
#76809 = CARTESIAN_POINT ( 'NONE',  ( -9.636570100870001099, 1473.857455401490142, 205.4329981810490153 ) ) ;
#76810 = FACE_OUTER_BOUND ( 'NONE', #2670, .T. ) ;
#76811 = CARTESIAN_POINT ( 'NONE',  ( -51.95708025780000128, 1379.690182529579943, 243.6310195730590067 ) ) ;
#76812 = CARTESIAN_POINT ( 'NONE',  ( 22.73961117905130180, 1415.546519254560053, 206.2005574400780006 ) ) ;
#76813 = EDGE_CURVE ( 'NONE', #59275, #101745, #66035, .T. ) ;
#76815 = CARTESIAN_POINT ( 'NONE',  ( 5.092807830394789903, 1466.926502071939922, 199.2585311702579816 ) ) ;
#76814 = DIRECTION ( 'NONE',  ( 9.404037925578970303E-16, -1.000000000000000000, 2.220446049250000002E-16 ) ) ;
#76816 = CARTESIAN_POINT ( 'NONE',  ( -4.654161102448804321, 1423.691786733173558, 184.4582529657765235 ) ) ;
#76817 = CARTESIAN_POINT ( 'NONE',  ( -5.800581839631719916, 1423.415691768110037, 91.00909034883800075 ) ) ;
#76818 = ORIENTED_EDGE ( 'NONE', *, *, #41280, .F. ) ;
#76819 = AXIS2_PLACEMENT_3D ( 'NONE', #78760, #2076, #52470 ) ;
#76820 = ADVANCED_FACE ( 'NONE', ( #12849 ), #29109, .F. ) ;
#76821 = CARTESIAN_POINT ( 'NONE',  ( 18.30039643192660037, 1424.506794127079957, 223.6085225123430007 ) ) ;
#76822 = CARTESIAN_POINT ( 'NONE',  ( 1.931477262906880821, 1516.530173527225770, 216.8307695177551295 ) ) ;
#76823 = CARTESIAN_POINT ( 'NONE',  ( -2.904196725509198718, 1484.572852589933518, 183.2790564706236580 ) ) ;
#76824 = CARTESIAN_POINT ( 'NONE',  ( 5.895408526091680201, 1407.650947103020144, 270.1377427648220078 ) ) ;
#76825 = EDGE_CURVE ( 'NONE', #105791, #37255, #18006, .T. ) ;
#76827 = VERTEX_POINT ( 'NONE', #71144 ) ;
#76826 = CARTESIAN_POINT ( 'NONE',  ( 0.8481724230196159287, 1515.120541028469916, 204.7938570022450051 ) ) ;
#76828 = CARTESIAN_POINT ( 'NONE',  ( 1.520093416789999985, 1489.468502498129965, 187.0056096891980246 ) ) ;
#76829 = B_SPLINE_CURVE_WITH_KNOTS ( 'NONE', 3,
 ( #10988, #85457, #35075, #17687, #19361, #68703, #52453, #102808, #27234, #44041, #77637, #26103, #110675, #8755, #77096, #69818, #60293, #26664, #406, #44598, #78181, #70374, #103362, #34523, #94411, #9332, #60865, #51893, #86030, #35622, #94990, #53005, #18257, #87138, #9874, #10429, #104489, #45162, #106149, #106686, #37846, #80947, #64169, #29977, #105049, #72034, #11543, #96654, #55216, #89344, #12640, #22103, #21564, #13159, #46275, #47346, #36738, #64726, #80402, #3716, #12081, #4247, #19922, #81474, #4777, #98287, #79302, #29427, #54122, #46818, #73104, #55774, #54672, #45718, #38381, #97742, #72556, #89889, #63626, #21013, #38924, #63090, #70933, #107243, #71489, #30535, #2613, #98842, #56302, #90433, #28338, #62531, #88250, #79855, #3166, #37298, #105610, #28895, #97188, #20462, #88799, #65268, #23777, #57964, #92097, #101579, #101032, #92643, #14829, #15917, #5337, #33284, #49016, #83153, #91552, #99378, #22653, #48467, #39497, #73669, #99933, #6447, #56857, #15376, #41698, #109464, #23227, #14276, #6989, #66378, #49565, #83694, #40593, #74764, #32743, #107800, #50116, #41143, #75322, #31085, #100496, #66923, #24330, #108903, #32193, #108353, #58513, #84245, #90988, #7543, #75857, #82605, #5895, #57427, #110007, #67474, #24867, #65815, #40041, #74224, #59070, #13711, #47897, #82033, #31634, #54403, #3440, #2895, #19657, #276, #70661, #84787, #33841, #25974, #60173, #87998, #102141, #85903, #50656, #105890, #8085, #88535, #93727, #37572, #8631, #96937, #9210, #42254, #43370, #17005, #93193, #45990, #51769, #102678, #11284, #85334, #77518, #68031, #62823, #62252, #71208, #2350, #59614, #42806, #94291, #36464, #104777, #76401, #17569, #28063, #25419, #20204, #105328, #11819, #96378, #51205, #76966, #53860, #45449, #34402, #110555, #68575, #79590, #37014, #28621, #80121, #71772, #29169, #16462, #90716, #72295, #21833, #47086, #99105, #82326, #48187, #12355, #56031, #29713, #3992, #73384, #30811, #40315, #39776, #31361, #64448, #65545, #54941, #82868, #98564, #90157, #30255, #38116, #106427, #98011, #89069, #46545, #38661, #80679, #63897, #57148, #91275, #5624, #72837, #21282, #56582, #5061, #22382, #14001, #13438, #47628, #73935, #55491, #99654, #108066, #107520, #89616, #39207, #12907, #14555, #81756, #64988, #81211, #22944, #48744, #4526, #6161, #74498, #106970, #108627, #63359, #97475, #20745, #50940, #83970, #6713, #66653, #59354, #23510, #8911, #91817 ),
 .UNSPECIFIED., .F., .F.,
 ( 4, 3, 3, 3, 3, 3, 3, 3, 3, 3, 3, 3, 3, 3, 3, 3, 3, 3, 3, 3, 3, 3, 3, 3, 3, 3, 3, 3, 3, 3, 3, 3, 3, 3, 3, 3, 3, 3, 3, 3, 3, 3, 3, 3, 3, 3, 3, 3, 3, 3, 3, 3, 3, 3, 3, 3, 3, 3, 3, 3, 3, 3, 3, 3, 3, 3, 3, 3, 3, 3, 3, 3, 3, 3, 3, 3, 3, 3, 3, 3, 3, 3, 3, 3, 3, 3, 3, 3, 3, 3, 3, 3, 3, 3, 3, 3, 3, 3, 3, 3, 4 ),
 ( 9.527080348409999289, 10.85173027196099937, 12.00624473378430146, 13.10086034166340063, 14.14961175496640067, 15.14877182358010010, 15.39383910896309970, 16.42944771861520081, 17.50948676729140274, 18.64816147367130128, 19.92972531175479745, 21.39309245868300025, 23.20366259091170136, 24.59245591388290109, 25.84110766704660023, 26.97705335283380279, 27.58084801734310076, 28.68944630574549848, 29.82656121067200061, 30.99685979729480323, 32.20647895571269714, 33.49104441228929829, 34.83666280905310231, 36.25746581317260109, 37.80012760393510263, 39.36589684718460092, 40.85204067702190400, 41.39509552342049403, 43.75295810538389674, 46.16562766740489110, 48.42936579919658868, 50.56808164685719476, 52.48310125732749043, 54.31967719734500122, 56.09294667343839080, 57.81364711399808698, 59.48968560173540254, 61.10873929825010009, 62.70029911509010390, 64.25293939849369451, 65.53909258048099673, 67.16844705198229803, 68.87663427951409290, 70.69318331658230647, 72.67675589585680029, 75.06336699077600372, 77.83965603350679885, 79.89839901332899785, 81.75326913944610396, 83.48794843525729448, 85.13855407467239900, 86.69737124088230473, 88.21590074822410088, 89.68095808219059961, 90.91108773633949625, 92.82794843041369859, 94.79388189049979019, 96.79267130114249085, 98.79623022816639377, 100.7738431079329899, 102.7044857337120050, 104.5710202628480090, 106.3668334849150057, 108.1169125231769925, 109.8255655786209957, 111.4968565625370047, 113.1177619320860117, 114.7136499496349984, 116.2730054179010040, 117.6367619667960014, 119.0754927998699912, 120.5565149085459922, 122.0751441691740098, 123.5870575414840005, 125.0706667163910026, 126.5142087427740165, 127.9148134135910198, 129.2561388162960441, 130.5667318641620227, 131.8367184849859939, 132.4493970707720223, 133.5475295398549918, 134.6463778432060394, 135.7455120869569782, 136.8793330144310403, 137.9772763609580011, 139.0740946830690064, 140.1694335882050098, 141.2629533371109858, 142.3532320226559875, 143.4413191182189848, 144.5259477239419823, 144.8160795067510094, 146.5546788388820119, 148.3790043525229976, 150.2749373096100101, 152.1509483487260184, 153.9553471829370039, 155.6832911718549894, 157.3186866423189940, 157.6516401924140212 ),
 .UNSPECIFIED. ) ;
#76830 = CARTESIAN_POINT ( 'NONE',  ( 0.6547232732189989246, 1508.551704408389924, 219.9513850608990140 ) ) ;
#76831 = CARTESIAN_POINT ( 'NONE',  ( -10.85481319969999880, 1425.430217766629994, 147.2777488329979860 ) ) ;
#76832 = DIRECTION ( 'NONE',  ( 0.000000000000000000, 1.000000000000000000, 0.000000000000000000 ) ) ;
#76833 = CARTESIAN_POINT ( 'NONE',  ( 3.035844568486590234, 1446.218552265309881, 199.4665232611309875 ) ) ;
#76834 = ADVANCED_FACE ( 'NONE', ( #70592 ), #89435, .T. ) ;
#76835 = DIRECTION ( 'NONE',  ( -5.980589973904019347E-17, 1.000000000000000000, -1.736889445713099699E-16 ) ) ;
#76836 = CARTESIAN_POINT ( 'NONE',  ( 8.165488601299999871, 1502.104785131989956, 208.0160615438289824 ) ) ;
#76837 = EDGE_CURVE ( 'NONE', #20553, #38713, #83450, .T. ) ;
#76838 = CARTESIAN_POINT ( 'NONE',  ( 5.826988351930000753, 1410.392867642730153, 231.1209932769980071 ) ) ;
#76840 = CARTESIAN_POINT ( 'NONE',  ( -11.40823118469380049, 1481.949762775670024, 208.3180590605030034 ) ) ;
#76839 = CARTESIAN_POINT ( 'NONE',  ( -19.67423585419999910, 1495.375718038329978, 228.6692629309980020 ) ) ;
#76841 = CARTESIAN_POINT ( 'NONE',  ( -16.13435506578399981, 1459.076926233949962, 230.3615790949820052 ) ) ;
#76842 = CIRCLE ( 'NONE', #39353, 3.750000000000000000 ) ;
#76843 = VERTEX_POINT ( 'NONE', #28001 ) ;
#76844 = CARTESIAN_POINT ( 'NONE',  ( -6.562635860634999929, 1517.111322026010157, 206.2508942643169974 ) ) ;
#76845 = CARTESIAN_POINT ( 'NONE',  ( 31.74787428599999828, 1415.252022282229973, 268.0541964391980514 ) ) ;
#76846 = B_SPLINE_CURVE_WITH_KNOTS ( 'NONE', 3,
 ( #85199, #41565, #16322, #32608 ),
 .UNSPECIFIED., .F., .F.,
 ( 4, 4 ),
 ( 0.000000000000000000, 0.03289823588023810252 ),
 .UNSPECIFIED. ) ;
#76847 = CARTESIAN_POINT ( 'NONE',  ( 7.141639577908946102, 1508.551704408428805, 214.6352815282469635 ) ) ;
#76848 = EDGE_CURVE ( 'NONE', #30026, #47770, #5426, .T. ) ;
#76849 = CARTESIAN_POINT ( 'NONE',  ( 21.79136847569999702, 1469.153666633229932, 195.1686735108980031 ) ) ;
#76850 = CARTESIAN_POINT ( 'NONE',  ( 0.3821805048270000005, 1506.433683729329914, 231.1012307613979999 ) ) ;
#76851 = CARTESIAN_POINT ( 'NONE',  ( -8.949046086683678070, 1388.869870210199451, 217.7000893693110868 ) ) ;
#76852 = CARTESIAN_POINT ( 'NONE',  ( -1.321099038869999909, 1450.950434108429818, 183.2266072565980153 ) ) ;
#76853 = LINE ( 'NONE', #58951, #103351 ) ;
#76854 = CARTESIAN_POINT ( 'NONE',  ( -15.62861107659999860, 1418.244676480490170, 203.0179540571090229 ) ) ;
#76855 = AXIS2_PLACEMENT_3D ( 'NONE', #53050, #2107, #62586 ) ;
#76856 = CARTESIAN_POINT ( 'NONE',  ( -13.20913601900000067, 1444.817643627899997, 187.1579182788979949 ) ) ;
#76857 = CARTESIAN_POINT ( 'NONE',  ( -2.692717788947200486, 1485.501216450119955, 197.5304516791929927 ) ) ;
#76858 = CARTESIAN_POINT ( 'NONE',  ( -16.64746823025755518, 1419.609048024772392, 209.0357172696779458 ) ) ;
#76859 = CARTESIAN_POINT ( 'NONE',  ( 20.94370973160000204, 1411.258104562529979, 270.0430967323979417 ) ) ;
#76860 = ORIENTED_EDGE ( 'NONE', *, *, #26231, .T. ) ;
#76861 = CARTESIAN_POINT ( 'NONE',  ( 2.124170329769999643, 1471.509589720390068, 189.1723552809990281 ) ) ;
#76862 = CARTESIAN_POINT ( 'NONE',  ( -13.20657463812640131, 1409.374244136060270, 216.1033536567719864 ) ) ;
#76863 = B_SPLINE_SURFACE_WITH_KNOTS ( 'NONE', 5, 1, ( 
 ( #21443, #46702 ),
 ( #6323, #5222 ),
 ( #32074, #40472 ),
 ( #48347, #99813 ),
 ( #97634, #72990 ),
 ( #80832, #74647 ) ),
 .UNSPECIFIED., .F., .F., .F.,
 ( 6, 6 ),
 ( 2, 2 ),
 ( 0.000000000000000000, 3.671445137310000106 ),
 ( 0.000000000000000000, 14.00000000000000000 ),
 .UNSPECIFIED. ) ;
#76864 = CARTESIAN_POINT ( 'NONE',  ( -11.65521739879129903, 1507.535655379640275, 207.9035470749859940 ) ) ;
#76865 = CARTESIAN_POINT ( 'NONE',  ( -23.72448802369999754, 1471.157921940630104, 268.2433403273980161 ) ) ;
#76866 = CARTESIAN_POINT ( 'NONE',  ( -7.464251903891183204, 1516.685766403216121, 209.9631294702575701 ) ) ;
#76867 = CARTESIAN_POINT ( 'NONE',  ( -10.94176001355937977, 1391.017588921819652, 214.8528320132766112 ) ) ;
#76868 = CARTESIAN_POINT ( 'NONE',  ( -24.33598933562576150, 1444.630201432154536, 211.2345754049932509 ) ) ;
#76869 = CARTESIAN_POINT ( 'NONE',  ( -74.53996386105208671, 1384.650779838590097, 299.6395783774970027 ) ) ;
#76870 = CARTESIAN_POINT ( 'NONE',  ( -20.28996348272639949, 1384.951249660460007, 201.7330533080949806 ) ) ;
#76871 = CARTESIAN_POINT ( 'NONE',  ( 11.94034776663059993, 1415.658863692289970, 223.2578065737770032 ) ) ;
#76872 = EDGE_CURVE ( 'NONE', #5037, #2310, #102099, .T. ) ;
#76873 = B_SPLINE_SURFACE_WITH_KNOTS ( 'NONE', 5, 5, ( 
 ( #95181, #68903, #17888, #43677, #18437, #35268, #43128, #52087, #110317 ),
 ( #69452, #103570, #94060, #30, #77829, #70012, #86774, #50978, #10063 ),
 ( #34712, #42021, #59392, #44236, #85107, #78380, #104126, #27413, #16775 ),
 ( #61596, #95729, #18993, #76719, #25189, #51522, #8396, #33591, #101896 ),
 ( #42566, #68349, #25742, #17328, #85656, #8955, #71114, #72210, #45353 ),
 ( #36369, #105238, #96848, #62156, #87333, #2256, #62726, #4439, #29082 ) ),
 .UNSPECIFIED., .F., .F., .F.,
 ( 6, 6 ),
 ( 6, 3, 6 ),
 ( 25.26539605949999867, 42.22154059670000237 ),
 ( 0.000000000000000000, 1.000000000000000000, 2.000000000000000000 ),
 .UNSPECIFIED. ) ;
#76874 = CARTESIAN_POINT ( 'NONE',  ( -107.9702631740000101, 1378.913060387289988, 299.5275268469590060 ) ) ;
#76875 = CARTESIAN_POINT ( 'NONE',  ( -19.02270174366844913, 1526.382868172864164, 185.3889643600148815 ) ) ;
#76876 = DIRECTION ( 'NONE',  ( -1.000000000000000000, 0.000000000000000000, 0.000000000000000000 ) ) ;
#76877 = CARTESIAN_POINT ( 'NONE',  ( -22.44875270440000392, 1409.696988105930131, 206.2467493338480153 ) ) ;
#76878 = EDGE_CURVE ( 'NONE', #76557, #104116, #62698, .T. ) ;
#76879 =( BOUNDED_SURFACE ( )  B_SPLINE_SURFACE ( 3, 2, ( 
 ( #65265, #99375, #30533 ),
 ( #38922, #22649, #73102 ),
 ( #107241, #88797, #64724 ),
 ( #56299, #90429, #13708 ),
 ( #11541, #79853, #37296 ),
 ( #49562, #66920, #74761 ),
 ( #32190, #56854, #32740 ),
 ( #41695, #6986, #76398 ) ),
 .UNSPECIFIED., .F., .F., .T. ) 
 B_SPLINE_SURFACE_WITH_KNOTS ( ( 4, 2, 2, 4 ),
 ( 3, 3 ),
 ( 0.000000000000000000, 0.004949390070308980552, 0.007424085105463470828, 0.009898780140617961104 ),
 ( 0.000000000000000000, 1.000000000000000000 ),
 .UNSPECIFIED. ) 
 GEOMETRIC_REPRESENTATION_ITEM ( )  RATIONAL_B_SPLINE_SURFACE ( (
 ( 1.000000000000000000, 0.7008166191799920508, 1.000000000000000000),
 ( 1.000000000000000000, 0.6998717291170757360, 1.000000000000000000),
 ( 1.000000000000000000, 0.6996362392812857101, 1.000000000000000000),
 ( 1.000000000000000000, 0.6996543790199832857, 1.000000000000000000),
 ( 1.000000000000000000, 0.6997206315696691270, 1.000000000000000000),
 ( 1.000000000000000000, 0.6997875685659131761, 1.000000000000000000),
 ( 1.000000000000000000, 0.6997874683881916136, 1.000000000000000000),
 ( 1.000000000000000000, 0.6996393069086717098, 1.000000000000000000) ) ) 
 REPRESENTATION_ITEM ( '' )  SURFACE ( )  );
#76880 = CARTESIAN_POINT ( 'NONE',  ( 17.84636975430000305, 1416.824060884929850, 206.2620219508280286 ) ) ;
#76881 = CARTESIAN_POINT ( 'NONE',  ( -10.47043688597563182, 1517.051704408389924, 221.2386401010601844 ) ) ;
#76882 = VECTOR ( 'NONE', #86408, 1000.000000000000000 ) ;
#76883 = CARTESIAN_POINT ( 'NONE',  ( 10.60758307464649874, 1480.113492495000173, 207.9930903275029834 ) ) ;
#76884 = B_SPLINE_SURFACE_WITH_KNOTS ( 'NONE', 5, 5, ( 
 ( #79076, #18023, #95306, #77948, #36499, #94743, #1254, #103699, #70695 ),
 ( #96969, #62282, #88028, #45481, #2928, #20233, #37044, #9088, #77402 ),
 ( #706, #22410, #39805, #72326, #12389, #37600, #98595, #99133, #30287 ),
 ( #73416, #54976, #107552, #11851, #72863, #73965, #3473, #106456, #22975 ),
 ( #39241, #63926, #80152, #90748, #46574, #56612, #80709, #30839, #71803 ),
 ( #4018, #65015, #81786, #105922, #38144, #14027, #82357, #99682, #29202 ),
 ( #106998, #108096, #63391, #29739, #88567, #48218, #5657, #98041, #97506 ),
 ( #21315, #31390, #55518, #65571, #20775, #46024, #89101, #90185, #89646 ),
 ( #4555, #5088, #12932, #47113, #81239, #38688, #64479, #21859, #56058 ),
 ( #13468, #47659, #23538, #8386, #58810, #50967, #32509, #66679, #14585 ),
 ( #75075, #101325, #57730, #16764, #59382, #85095, #84552, #91849, #91302 ),
 ( #16222, #92950, #24615, #100784, #100258, #67229, #15126, #24077, #68339 ) ),
 .UNSPECIFIED., .F., .F., .F.,
 ( 6, 3, 3, 6 ),
 ( 6, 3, 6 ),
 ( 15.94786254319999941, 27.90018821209999800, 46.89625937809999812, 68.39792989049999505 ),
 ( 0.000000000000000000, 1.000000000000000000, 2.000000005329749975 ),
 .UNSPECIFIED. ) ;
#76885 = CARTESIAN_POINT ( 'NONE',  ( 2.471608048749999842, 1438.194204504490017, 150.4833623973980252 ) ) ;
#76886 = CARTESIAN_POINT ( 'NONE',  ( -17.66148164096410156, 1440.150380355800053, 218.7822556169580253 ) ) ;
#76887 = CARTESIAN_POINT ( 'NONE',  ( 17.72020223055846699, 1524.201670966335769, 180.4880726372848017 ) ) ;
#76888 = CARTESIAN_POINT ( 'NONE',  ( -3.535390505542900019, 1507.776748193199865, 180.9473287765760006 ) ) ;
#76890 = CARTESIAN_POINT ( 'NONE',  ( -10.36756237719999874, 1382.682511944280122, 200.8304498154890041 ) ) ;
#76889 = FACE_OUTER_BOUND ( 'NONE', #11239, .T. ) ;
#76891 = CARTESIAN_POINT ( 'NONE',  ( 11.70201856712229826, 1426.718767056610204, 141.6641753760530094 ) ) ;
#76892 = CARTESIAN_POINT ( 'NONE',  ( 9.696539317786241341, 1436.240278671050191, 210.7713209817480049 ) ) ;
#76893 = AXIS2_PLACEMENT_3D ( 'NONE', #77176, #110204, #35155 ) ;
#76894 = CARTESIAN_POINT ( 'NONE',  ( -122.7580815721600089, 1314.643966242390206, 299.1095026942290360 ) ) ;
#76895 = CARTESIAN_POINT ( 'NONE',  ( 5.529292985537660243, 1447.580617647699910, 200.5261424873660019 ) ) ;
#76896 = DIRECTION ( 'NONE',  ( -0.07512831052118132402, 0.9801898970463382987, -0.1832580221614370231 ) ) ;
#76897 = EDGE_CURVE ( 'NONE', #103079, #72815, #88343, .T. ) ;
#76898 = CARTESIAN_POINT ( 'NONE',  ( 7.714371502985000184, 1516.738222552470233, 203.3422428319769892 ) ) ;
#76899 = CARTESIAN_POINT ( 'NONE',  ( -4.215652631204428680, 1398.038844839439435, 221.4193366157311118 ) ) ;
#76900 = CARTESIAN_POINT ( 'NONE',  ( 0.000000000000000000, 1514.413060387330006, 209.1218459616979999 ) ) ;
#76901 = FACE_OUTER_BOUND ( 'NONE', #95116, .T. ) ;
#76902 = CARTESIAN_POINT ( 'NONE',  ( -17.60543171180000144, 1410.868334040629861, 194.0670716385980086 ) ) ;
#76903 = AXIS2_PLACEMENT_3D ( 'NONE', #28401, #69319, #88309 ) ;
#76904 = CARTESIAN_POINT ( 'NONE',  ( 7.365750702793119942, 1505.956296822819922, 218.2324441051819974 ) ) ;
#76906 = ORIENTED_EDGE ( 'NONE', *, *, #100700, .F. ) ;
#76905 = CARTESIAN_POINT ( 'NONE',  ( -31.28542702328589797, 1379.632103487770109, 219.4205719633520175 ) ) ;
#76907 = VERTEX_POINT ( 'NONE', #20022 ) ;
#76908 = CARTESIAN_POINT ( 'NONE',  ( 12.04588369443019857, 1433.807560102029811, 150.0158760707519718 ) ) ;
#76909 = CARTESIAN_POINT ( 'NONE',  ( 21.92026280708336827, 1524.524650307258071, 184.5694803541689453 ) ) ;
#76910 = ORIENTED_EDGE ( 'NONE', *, *, #104050, .T. ) ;
#76911 = CARTESIAN_POINT ( 'NONE',  ( -0.0002573390537614959981, 1396.305641767069801, 221.3136691980663784 ) ) ;
#76912 = DIRECTION ( 'NONE',  ( 0.4090087482554189968, 4.257102464871849587E-15, -0.9125304618754023211 ) ) ;
#76913 = CARTESIAN_POINT ( 'NONE',  ( -4.487249775048080203, 1509.038615934839981, 211.6097811040130239 ) ) ;
#76915 = CARTESIAN_POINT ( 'NONE',  ( 9.534219445089998857, 1428.030197386430018, 144.1938086916980239 ) ) ;
#76914 = CARTESIAN_POINT ( 'NONE',  ( 16.09580795758349936, 1424.963234393459970, 191.0812631129040255 ) ) ;
#76916 = CARTESIAN_POINT ( 'NONE',  ( 18.87825204697160331, 1498.114858794700240, 229.4168632574339881 ) ) ;
#76917 = EDGE_CURVE ( 'NONE', #59045, #6757, #66203, .T. ) ;
#76918 = CARTESIAN_POINT ( 'NONE',  ( 0.2362929480300000051, 1488.177340598630053, 181.7177447157979771 ) ) ;
#76919 = CARTESIAN_POINT ( 'NONE',  ( -0.3551208789749999983, 1416.218047894730262, 191.1510192753979993 ) ) ;
#76920 = CARTESIAN_POINT ( 'NONE',  ( -24.52161429607329879, 1444.774474201280100, 210.9829639010650055 ) ) ;
#76921 = CARTESIAN_POINT ( 'NONE',  ( 5.293700147766140063, 1396.097920486130079, 199.4374042141640189 ) ) ;
#76922 = CARTESIAN_POINT ( 'NONE',  ( 35.32500643191499279, 1435.854286985769932, 134.0999999975889807 ) ) ;
#76923 = CARTESIAN_POINT ( 'NONE',  ( 11.57048490630000082, 1431.876862801990001, 151.1817391485979840 ) ) ;
#76924 = CARTESIAN_POINT ( 'NONE',  ( 8.061256550655000908, 1512.677556571450168, 202.2106555494169982 ) ) ;
#76925 = ORIENTED_EDGE ( 'NONE', *, *, #18286, .F. ) ;
#76926 = CARTESIAN_POINT ( 'NONE',  ( 14.13185208260100012, 1435.965080345399883, 150.0649179125809951 ) ) ;
#76927 = ADVANCED_FACE ( 'NONE', ( #2160 ), #52668, .F. ) ;
#76928 = ORIENTED_EDGE ( 'NONE', *, *, #56286, .F. ) ;
#76929 = ORIENTED_EDGE ( 'NONE', *, *, #41147, .F. ) ;
#76930 = CARTESIAN_POINT ( 'NONE',  ( 13.14582496903311259, 1444.761283730599416, 169.3990323816187527 ) ) ;
#76931 = CARTESIAN_POINT ( 'NONE',  ( -4.469061828439999218, 1464.606722983030295, 237.1332388458979779 ) ) ;
#76932 = AXIS2_PLACEMENT_3D ( 'NONE', #52341, #27669, #61309 ) ;
#76933 = CARTESIAN_POINT ( 'NONE',  ( 25.78167222729700114, 1509.813387082529971, 195.1140727163279962 ) ) ;
#76934 = CARTESIAN_POINT ( 'NONE',  ( -19.67539872490000263, 1467.567198463789964, 206.2061548292190025 ) ) ;
#76935 = CARTESIAN_POINT ( 'NONE',  ( 11.40789371488579995, 1422.073302846210026, 210.0656248370559922 ) ) ;
#76936 = CARTESIAN_POINT ( 'NONE',  ( -37.25828949241959265, 1379.646493637162166, 220.1838309194394583 ) ) ;
#76937 = FACE_OUTER_BOUND ( 'NONE', #26380, .T. ) ;
#76938 = ORIENTED_EDGE ( 'NONE', *, *, #95259, .T. ) ;
#76939 = CARTESIAN_POINT ( 'NONE',  ( 2.864326087304999824, 1516.826109302209943, 206.6287721023469999 ) ) ;
#76940 = ORIENTED_EDGE ( 'NONE', *, *, #87682, .T. ) ;
#76941 = CARTESIAN_POINT ( 'NONE',  ( -103.8863835612550020, 1379.884582398730117, 304.0035884679699620 ) ) ;
#76942 = AXIS2_PLACEMENT_3D ( 'NONE', #1297, #80756, #53366 ) ;
#76943 = CARTESIAN_POINT ( 'NONE',  ( -19.06981053970000062, 1509.578992845429866, 231.5773580161979908 ) ) ;
#76944 = EDGE_CURVE ( 'NONE', #20905, #14138, #21956, .T. ) ;
#76945 = EDGE_LOOP ( 'NONE', ( #70153, #16079, #16639, #24573 ) ) ;
#76946 = CARTESIAN_POINT ( 'NONE',  ( -13.01091002569999944, 1409.534180062029918, 190.3248903057979931 ) ) ;
#76947 = CARTESIAN_POINT ( 'NONE',  ( 6.946514176795000495, 1512.024017243149956, 216.2067250139469934 ) ) ;
#76949 = ORIENTED_EDGE ( 'NONE', *, *, #14854, .F. ) ;
#76948 = CARTESIAN_POINT ( 'NONE',  ( 1.370146406885849988, 1423.265678981450037, 192.5490732762039841 ) ) ;
#76950 = CARTESIAN_POINT ( 'NONE',  ( 24.55105544570000120, 1439.606887532569999, 213.0196149167179840 ) ) ;
#76951 = CARTESIAN_POINT ( 'NONE',  ( -18.26458976723020200, 1508.551704408389924, 210.4136963709630095 ) ) ;
#76952 = CARTESIAN_POINT ( 'NONE',  ( -13.77266209894789917, 1522.051704408389924, 217.0393652727940150 ) ) ;
#76953 = FACE_OUTER_BOUND ( 'NONE', #97021, .T. ) ;
#76954 = ADVANCED_FACE ( 'NONE', ( #102242 ), #63495, .T. ) ;
#76955 = CARTESIAN_POINT ( 'NONE',  ( 29.40443212115394189, 1511.187213306747708, 222.0897836382243042 ) ) ;
#76956 = CARTESIAN_POINT ( 'NONE',  ( 1.131796810615000037, 1516.659138130710289, 214.8948242487770131 ) ) ;
#76957 = EDGE_CURVE ( 'NONE', #72801, #47896, #17860, .T. ) ;
#76958 = CARTESIAN_POINT ( 'NONE',  ( -2.930595334879239733, 1428.959675587809897, 200.2235252233409994 ) ) ;
#76959 = CARTESIAN_POINT ( 'NONE',  ( -20.61444355170000264, 1508.354544900629890, 190.2376287260979950 ) ) ;
#76960 = CARTESIAN_POINT ( 'NONE',  ( 5.513200264406510342, 1508.884117426920056, 216.6305509554049991 ) ) ;
#76961 = CARTESIAN_POINT ( 'NONE',  ( -6.546039433425000276, 1516.565291103010168, 211.4147861392469849 ) ) ;
#76962 = CARTESIAN_POINT ( 'NONE',  ( 14.66466848360000164, 1409.425161895129804, 192.9600527036979827 ) ) ;
#76963 = CARTESIAN_POINT ( 'NONE',  ( 30.57819355944784689, 1525.253996226933623, 221.5701614757928439 ) ) ;
#76965 = ORIENTED_EDGE ( 'NONE', *, *, #60452, .F. ) ;
#76964 = CARTESIAN_POINT ( 'NONE',  ( -66.16583944359999236, 1390.700906735469971, 276.1376312171590257 ) ) ;
#76966 = CARTESIAN_POINT ( 'NONE',  ( -72.47380510957108868, 1385.015833470149801, 297.6916867413240197 ) ) ;
#76967 = CIRCLE ( 'NONE', #7251, 1.999999999997927436 ) ;
#76968 = CARTESIAN_POINT ( 'NONE',  ( 11.55308038760000144, 1469.479404942429937, 255.2309336889980216 ) ) ;
#76969 = CARTESIAN_POINT ( 'NONE',  ( 1.897589185483037122, 1452.532807482775752, 183.5787857509751859 ) ) ;
#76970 = CARTESIAN_POINT ( 'NONE',  ( -28.17578495147160211, 1509.896980478850082, 217.3377154775169799 ) ) ;
#76971 = CARTESIAN_POINT ( 'NONE',  ( -2.549355810456779725, 1507.417392930419965, 236.9597321781060089 ) ) ;
#76972 = CIRCLE ( 'NONE', #28694, 30.10786454236638576 ) ;
#76973 = ADVANCED_FACE ( 'NONE', ( #20982 ), #46485, .T. ) ;
#76974 = CARTESIAN_POINT ( 'NONE',  ( -23.99136450790000197, 1445.147507561969860, 213.3355241665780113 ) ) ;
#76975 = B_SPLINE_CURVE_WITH_KNOTS ( 'NONE', 3,
 ( #19711, #53914, #88049, #11334 ),
 .UNSPECIFIED., .F., .F.,
 ( 4, 4 ),
 ( 0.000000000000000000, 1.000000000000000000 ),
 .UNSPECIFIED. ) ;
#76977 = CARTESIAN_POINT ( 'NONE',  ( 17.76902723066159950, 1410.077149175569957, 222.7945870334489769 ) ) ;
#76976 = CARTESIAN_POINT ( 'NONE',  ( -11.60004869885203682, 1411.254281879943164, 137.0999999980979851 ) ) ;
#76978 = DIRECTION ( 'NONE',  ( 1.000000000000000000, 0.000000000000000000, 0.000000000000000000 ) ) ;
#76979 = ORIENTED_EDGE ( 'NONE', *, *, #21887, .T. ) ;
#76980 = CARTESIAN_POINT ( 'NONE',  ( 2.869693458934999608, 1517.070197312179971, 203.3343689375869872 ) ) ;
#76981 = CARTESIAN_POINT ( 'NONE',  ( 0.2163172094670000045, 1405.717036350329863, 267.8540247887980286 ) ) ;
#76982 = EDGE_CURVE ( 'NONE', #81986, #8168, #39393, .T. ) ;
#76983 = CIRCLE ( 'NONE', #9022, 1.000000000000000888 ) ;
#76984 = CARTESIAN_POINT ( 'NONE',  ( 28.63451943380000131, 1509.912999839629947, 206.7172238586179844 ) ) ;
#76985 = CARTESIAN_POINT ( 'NONE',  ( 24.57126113369999842, 1440.930743420699855, 213.1726824911179961 ) ) ;
#76987 = B_SPLINE_CURVE_WITH_KNOTS ( 'NONE', 3,
 ( #7020, #69156, #101607, #59099, #101061, #24358, #33309, #59644, #15947, #85934, #60765, #15404, #302 ),
 .UNSPECIFIED., .F., .F.,
 ( 4, 3, 3, 3, 4 ),
 ( -3.420209351472869752, -3.144711398279999681, -1.710104561635330089, -1.461849369231190021, 0.000000000000000000 ),
 .UNSPECIFIED. ) ;
#76986 = CARTESIAN_POINT ( 'NONE',  ( -19.63722818134010240, 1521.951704408389787, 200.0074286634620364 ) ) ;
#76988 = CARTESIAN_POINT ( 'NONE',  ( 3.172884302710000437, 1467.373997971989866, 218.6974001167089909 ) ) ;
#76989 = CARTESIAN_POINT ( 'NONE',  ( -20.99310762600000047, 1509.712614273529880, 187.9175820947980071 ) ) ;
#76990 = CARTESIAN_POINT ( 'NONE',  ( 29.16087826349600221, 1436.844756045629993, 136.7088000707439903 ) ) ;
#76991 = CARTESIAN_POINT ( 'NONE',  ( 34.97887668886630053, 1450.312591923280024, 136.2298315295870168 ) ) ;
#76992 = CARTESIAN_POINT ( 'NONE',  ( 3.207026754074329869E-15, 1467.715966850440054, 261.8343058931689598 ) ) ;
#76993 = CARTESIAN_POINT ( 'NONE',  ( -2.188303739500000233, 1431.240665291890082, 201.0188168257489849 ) ) ;
#76994 = CARTESIAN_POINT ( 'NONE',  ( 8.878917281270000572, 1509.223119011030121, 181.5151191445980032 ) ) ;
#76995 = CARTESIAN_POINT ( 'NONE',  ( 10.58112656791359996, 1481.600201880140048, 209.5141384132439839 ) ) ;
#76996 = CARTESIAN_POINT ( 'NONE',  ( -21.50863349123644142, 1524.374142163903798, 184.1251891552226994 ) ) ;
#76997 = CARTESIAN_POINT ( 'NONE',  ( -38.88868005081535273, 1452.484090863069014, 269.5912342720579318 ) ) ;
#76998 = ORIENTED_EDGE ( 'NONE', *, *, #51201, .F. ) ;
#76999 = CARTESIAN_POINT ( 'NONE',  ( -18.93537658700000037, 1413.766156166430164, 268.3665355202980436 ) ) ;
#77000 = B_SPLINE_CURVE_WITH_KNOTS ( 'NONE', 3,
 ( #40078, #75358, #82069, #40629, #109498, #49053 ),
 .UNSPECIFIED., .F., .F.,
 ( 4, 2, 4 ),
 ( 0.000000000000000000, 0.5000000000000000000, 1.000000000000000000 ),
 .UNSPECIFIED. ) ;
#77001 = CARTESIAN_POINT ( 'NONE',  ( 4.777537831619650177, 1455.786797201459876, 218.6089316382710024 ) ) ;
#77002 = CARTESIAN_POINT ( 'NONE',  ( -671.9628848459639130, -8383.748406600810995, -1657.040904779356197 ) ) ;
#77003 = CARTESIAN_POINT ( 'NONE',  ( 26.79414481833639883, 1435.433178084320161, 135.2874577367330176 ) ) ;
#77004 = VECTOR ( 'NONE', #61163, 1000.000000000000000 ) ;
#77005 = CARTESIAN_POINT ( 'NONE',  ( -0.3883820753600000231, 1416.446510123330199, 233.6943695348979873 ) ) ;
#77007 = CARTESIAN_POINT ( 'NONE',  ( 31.40702543711169881, 1523.611961620354123, 196.3340613265677916 ) ) ;
#77006 = CARTESIAN_POINT ( 'NONE',  ( 11.58814563159999977, 1501.742621387089912, 209.9262120703820074 ) ) ;
#77008 = CARTESIAN_POINT ( 'NONE',  ( -13.07100154019126315, 1444.825073959231759, 186.3867726210717137 ) ) ;
#77009 = B_SPLINE_SURFACE_WITH_KNOTS ( 'NONE', 5, 1, ( 
 ( #12137, #62024 ),
 ( #55272, #80459 ),
 ( #96712, #45219 ),
 ( #30028, #28953 ),
 ( #79357, #97790 ),
 ( #88853, #12691 ) ),
 .UNSPECIFIED., .F., .F., .F.,
 ( 6, 6 ),
 ( 2, 2 ),
 ( 0.000000000000000000, 3.930294876060000053 ),
 ( 0.000000000000000000, 14.00000000000000000 ),
 .UNSPECIFIED. ) ;
#77010 = CARTESIAN_POINT ( 'NONE',  ( 7.481288447059999847, 1426.924569037480069, 212.2063472014090166 ) ) ;
#77011 = CARTESIAN_POINT ( 'NONE',  ( -8.325276424809809228, 1512.905891558365056, 216.5259404424210743 ) ) ;
#77012 = FACE_OUTER_BOUND ( 'NONE', #4246, .T. ) ;
#77013 = CARTESIAN_POINT ( 'NONE',  ( 32.86802468386284914, 1512.187213306747481, 201.0396662540042030 ) ) ;
#77014 = FACE_OUTER_BOUND ( 'NONE', #95742, .T. ) ;
#77015 = CARTESIAN_POINT ( 'NONE',  ( 25.63655495179999733, 1436.189972215739999, 136.9580440781980144 ) ) ;
#77016 = CARTESIAN_POINT ( 'NONE',  ( -10.88335057715240062, 1396.293115364239839, 207.0876604851810043 ) ) ;
#77017 = ORIENTED_EDGE ( 'NONE', *, *, #63675, .T. ) ;
#77018 = CIRCLE ( 'NONE', #46576, 1.000000000000000888 ) ;
#77019 = CARTESIAN_POINT ( 'NONE',  ( -17.21692188389469891, 1410.879836749619926, 226.0201596333920122 ) ) ;
#77020 = CARTESIAN_POINT ( 'NONE',  ( 12.00000000000000000, 1443.913060387330006, 147.5878346084980137 ) ) ;
#77021 = VERTEX_POINT ( 'NONE', #56266 ) ;
#77022 = ORIENTED_EDGE ( 'NONE', *, *, #13091, .F. ) ;
#77023 = CARTESIAN_POINT ( 'NONE',  ( -11.77155278529999904, 1501.635673497090011, 210.8734570959489929 ) ) ;
#77024 = CYLINDRICAL_SURFACE ( 'NONE', #6331, 1.999999999999994005 ) ;
#77026 = CARTESIAN_POINT ( 'NONE',  ( 0.06756312569560819770, 1456.974508360119898, 219.7477876681689963 ) ) ;
#77025 = DIRECTION ( 'NONE',  ( 0.9510565162951523099, 0.000000000000000000, -0.3090169943749515591 ) ) ;
#77027 = CARTESIAN_POINT ( 'NONE',  ( 22.68528333430000288, 1409.869697741029995, 212.6986685081479891 ) ) ;
#77028 = CARTESIAN_POINT ( 'NONE',  ( 9.682511080499990541, 1436.279831232390052, 210.8541354582289955 ) ) ;
#77029 = CARTESIAN_POINT ( 'NONE',  ( -7.512750246095000861, 1509.038615934159907, 203.6084103740969908 ) ) ;
#77030 = CARTESIAN_POINT ( 'NONE',  ( -2.792392588003326903, 1526.382868172863937, 241.3440112565233164 ) ) ;
#77031 = CARTESIAN_POINT ( 'NONE',  ( -9.771923492860000948, 1448.872168905890021, 190.8346797514990101 ) ) ;
#77032 = FACE_BOUND ( 'NONE', #95499, .T. ) ;
#77033 = CARTESIAN_POINT ( 'NONE',  ( -101.5621914980000042, 1376.194720364869909, 306.3892953801590124 ) ) ;
#77034 = CARTESIAN_POINT ( 'NONE',  ( 8.602227872912603601, 1365.853205000053777, 207.6218459616988241 ) ) ;
#77036 = ORIENTED_EDGE ( 'NONE', *, *, #84290, .F. ) ;
#77035 = CARTESIAN_POINT ( 'NONE',  ( -2.528665822673169918E-09, 1414.285713195190056, 246.7922399721219904 ) ) ;
#77037 = ORIENTED_EDGE ( 'NONE', *, *, #93831, .F. ) ;
#77038 = CARTESIAN_POINT ( 'NONE',  ( -11.82137633359979922, 1429.378842759500003, 149.1280831305220147 ) ) ;
#77039 = CARTESIAN_POINT ( 'NONE',  ( 7.407689794035296593, 1511.025938460391671, 202.7787461935695035 ) ) ;
#77040 = CARTESIAN_POINT ( 'NONE',  ( -2.303611226680000179, 1473.224731274329770, 270.4285322737979982 ) ) ;
#77041 = CARTESIAN_POINT ( 'NONE',  ( -110.0629084955440078, 1384.909053975289908, 296.9513011978259556 ) ) ;
#77042 = CARTESIAN_POINT ( 'NONE',  ( -124.0634771228999966, 1314.643966242390206, 304.2218459572590064 ) ) ;
#77043 = CIRCLE ( 'NONE', #68108, 2.500000000000002220 ) ;
#77044 = B_SPLINE_CURVE_WITH_KNOTS ( 'NONE', 3,
 ( #55984, #5009, #39156, #72787, #106914, #106373, #64941, #90663, #54888, #64393, #73888, #63303, #80627, #21228, #82274 ),
 .UNSPECIFIED., .F., .F.,
 ( 4, 2, 2, 1, 1, 1, 2, 2, 4 ),
 ( 0.000000000000000000, 0.2499999999999962252, 0.3749999999999940048, 0.4374999999999953926, 0.4687499999999934497, 0.4843749999999965583, 0.4921874999999956146, 0.4999999999999946709, 1.000000000000000000 ),
 .UNSPECIFIED. ) ;
#77045 = CARTESIAN_POINT ( 'NONE',  ( 1.191524307911315805, 1526.382868172864164, 239.2353018730791518 ) ) ;
#77046 = CARTESIAN_POINT ( 'NONE',  ( 14.43914856551324100, 1435.431933939060400, 149.5787995519261528 ) ) ;
#77047 = FACE_OUTER_BOUND ( 'NONE', #82773, .T. ) ;
#77048 = SURFACE_STYLE_FILL_AREA ( #69771 ) ;
#77049 = CARTESIAN_POINT ( 'NONE',  ( -22.72903601768109993, 1507.336004462989877, 208.4180099543350195 ) ) ;
#77050 = CARTESIAN_POINT ( 'NONE',  ( 6.995010115480782886, 1370.198628283411608, 208.3718459617010978 ) ) ;
#77051 = CARTESIAN_POINT ( 'NONE',  ( 9.888001510779538705, 1409.198532364260018, 197.8619322872570194 ) ) ;
#77052 = CARTESIAN_POINT ( 'NONE',  ( -15.53680187063869944, 1407.737570638100124, 268.3823695302049828 ) ) ;
#77053 = CARTESIAN_POINT ( 'NONE',  ( -14.33596079271969970, 1436.258147809659931, 150.0352455327449945 ) ) ;
#77054 = ORIENTED_EDGE ( 'NONE', *, *, #68125, .F. ) ;
#77055 = DIRECTION ( 'NONE',  ( 1.000000000000000000, 0.000000000000000000, 0.000000000000000000 ) ) ;
#77056 = CARTESIAN_POINT ( 'NONE',  ( 13.42771486050000007, 1443.428666381239964, 188.1474344706980162 ) ) ;
#77057 = EDGE_LOOP ( 'NONE', ( #43310, #108588, #12484 ) ) ;
#77058 = VERTEX_POINT ( 'NONE', #13673 ) ;
#77059 = CARTESIAN_POINT ( 'NONE',  ( -22.06116865633574164, 1506.527232288060532, 209.1639464567564346 ) ) ;
#77060 = CARTESIAN_POINT ( 'NONE',  ( -21.76695791008670611, 1524.152349020271004, 183.4045362816220290 ) ) ;
#77061 = CARTESIAN_POINT ( 'NONE',  ( 7.722536764694999611, 1517.050041317280147, 213.7387458049869906 ) ) ;
#77062 = CARTESIAN_POINT ( 'NONE',  ( -16.06248428700000375, 1485.484064211630084, 187.6661218516980227 ) ) ;
#77063 = CARTESIAN_POINT ( 'NONE',  ( 8.742163716520650412E-12, 1408.913060387359792, 224.1216835645979870 ) ) ;
#77064 = VERTEX_POINT ( 'NONE', #47863 ) ;
#77065 = CARTESIAN_POINT ( 'NONE',  ( -109.5441724480000119, 1375.366238318880050, 302.0293835567589440 ) ) ;
#77066 = AXIS2_PLACEMENT_3D ( 'NONE', #76952, #262, #94847 ) ;
#77067 = CARTESIAN_POINT ( 'NONE',  ( -2.500000000000000000, 1419.365678191629968, 145.1702635125890311 ) ) ;
#77068 = CARTESIAN_POINT ( 'NONE',  ( -5.784008673325000238, 1516.911981270829983, 204.1205073037870079 ) ) ;
#77069 = ADVANCED_FACE ( 'NONE', ( #81997 ), #1724, .T. ) ;
#77070 = CARTESIAN_POINT ( 'NONE',  ( -27.58156214539999951, 1508.605065867730218, 205.3521991578080019 ) ) ;
#77071 = EDGE_CURVE ( 'NONE', #78702, #46347, #7309, .T. ) ;
#77072 = CARTESIAN_POINT ( 'NONE',  ( -2.182463115098289386, 1517.051704408389696, 216.8444262845050616 ) ) ;
#77073 = CARTESIAN_POINT ( 'NONE',  ( -30.61151124082590158, 1384.557641573209821, 205.9241274443010070 ) ) ;
#77074 = CARTESIAN_POINT ( 'NONE',  ( -5.683186617470000535, 1409.111521637029909, 195.5271251408980220 ) ) ;
#77075 = AXIS2_PLACEMENT_3D ( 'NONE', #88837, #11582, #71534 ) ;
#77076 = DIRECTION ( 'NONE',  ( 0.000000000000000000, 1.000000000000000000, 0.000000000000000000 ) ) ;
#77078 = VERTEX_POINT ( 'NONE', #8601 ) ;
#77077 = CARTESIAN_POINT ( 'NONE',  ( -38.39760561535049987, 1443.174109818610077, 137.1306153789020073 ) ) ;
#77079 = CARTESIAN_POINT ( 'NONE',  ( -28.25140912874190136, 1508.152706103189757, 208.8568142479740004 ) ) ;
#77080 = CARTESIAN_POINT ( 'NONE',  ( 27.14725374240000022, 1488.689090776530065, 210.8864821603579855 ) ) ;
#77081 = CARTESIAN_POINT ( 'NONE',  ( -57.29365481403381466, 1379.717584333650848, 260.4218402486304171 ) ) ;
#77082 = CARTESIAN_POINT ( 'NONE',  ( 19.75967613925110200, 1467.111012934069777, 224.7767255004650053 ) ) ;
#77083 = CARTESIAN_POINT ( 'NONE',  ( -13.17868479539550108, 1436.069128864759932, 150.6624180133409823 ) ) ;
#77084 = VECTOR ( 'NONE', #103399, 1000.000000000000114 ) ;
#77085 = CARTESIAN_POINT ( 'NONE',  ( 1.136004274065000041, 1516.815173273089840, 211.9874827793370287 ) ) ;
#77086 = CARTESIAN_POINT ( 'NONE',  ( -68.54084681569999304, 1379.747861287210071, 279.6492226308589579 ) ) ;
#77087 = EDGE_CURVE ( 'NONE', #92786, #62492, #93013, .T. ) ;
#77088 = CARTESIAN_POINT ( 'NONE',  ( -15.28683124289999995, 1417.995325491429867, 226.9473089156979881 ) ) ;
#77089 = CARTESIAN_POINT ( 'NONE',  ( 6.686050678956539706, 1483.907811585419950, 213.3532383466159956 ) ) ;
#77090 = CARTESIAN_POINT ( 'NONE',  ( 2.284053471355000031, 1516.854133554269993, 207.9850318982369970 ) ) ;
#77091 = ORIENTED_EDGE ( 'NONE', *, *, #44061, .T. ) ;
#77092 = DIRECTION ( 'NONE',  ( -1.000000000000000000, 0.000000000000000000, -0.000000000000000000 ) ) ;
#77093 = CARTESIAN_POINT ( 'NONE',  ( 3.023156474270449756, 1440.625623375490250, 157.2242885116500020 ) ) ;
#77094 = CARTESIAN_POINT ( 'NONE',  ( -49.59345295620000371, 1385.124330617979922, 260.9076469794590025 ) ) ;
#77095 = ORIENTED_EDGE ( 'NONE', *, *, #30943, .F. ) ;
#77097 = AXIS2_PLACEMENT_3D ( 'NONE', #298, #42831, #845 ) ;
#77096 = CARTESIAN_POINT ( 'NONE',  ( -13.28712287618670018, 1385.300651250900046, 219.1026202486000045 ) ) ;
#77099 = ORIENTED_EDGE ( 'NONE', *, *, #76712, .T. ) ;
#77098 = CARTESIAN_POINT ( 'NONE',  ( -9.468502320038240327, 1493.161931906950031, 201.2760261155009971 ) ) ;
#77100 = CARTESIAN_POINT ( 'NONE',  ( 12.48554310994400041, 1434.717551771250101, 150.3686571217509993 ) ) ;
#77101 = CARTESIAN_POINT ( 'NONE',  ( 7.681229707928440398, 1459.296350014880090, 232.9086509542260046 ) ) ;
#77102 = CARTESIAN_POINT ( 'NONE',  ( -24.44688238734340047, 1509.532643014110135, 223.1734339750240110 ) ) ;
#77103 = LINE ( 'NONE', #411, #102727 ) ;
#77104 = DIRECTION ( 'NONE',  ( -0.9455185755993178454, 0.000000000000000000, 0.3255681544571537578 ) ) ;
#77105 = FACE_OUTER_BOUND ( 'NONE', #99988, .T. ) ;
#77107 = CARTESIAN_POINT ( 'NONE',  ( 14.31611368511230076, 1440.103953689049831, 195.6162067410979830 ) ) ;
#77106 = CARTESIAN_POINT ( 'NONE',  ( 0.01306000193830150063, 1516.939762005280045, 213.7404293621069939 ) ) ;
#77108 = CARTESIAN_POINT ( 'NONE',  ( 19.86721287640000000, 1507.838653413830116, 189.0155849983980261 ) ) ;
#77109 = CARTESIAN_POINT ( 'NONE',  ( 18.80339027203730140, 1425.953307585449693, 225.0197318394450008 ) ) ;
#77110 = VERTEX_POINT ( 'NONE', #79702 ) ;
#77111 = CARTESIAN_POINT ( 'NONE',  ( -12.73048917230000043, 1416.839648759230158, 195.1127161226980036 ) ) ;
#77112 = EDGE_CURVE ( 'NONE', #106272, #26067, #87446, .T. ) ;
#77113 = CARTESIAN_POINT ( 'NONE',  ( -17.09580434209999922, 1420.284596455289829, 203.6963249145289865 ) ) ;
#77114 = ORIENTED_EDGE ( 'NONE', *, *, #40376, .F. ) ;
#77115 = AXIS2_PLACEMENT_3D ( 'NONE', #2749, #27923, #44183 ) ;
#77116 = CARTESIAN_POINT ( 'NONE',  ( 6.813366145865759727, 1488.144601911519885, 204.7706368192809805 ) ) ;
#77117 = DIRECTION ( 'NONE',  ( -1.836970198721029688E-16, -1.000000000000000000, -1.314768175368352060E-31 ) ) ;
#77118 = ADVANCED_FACE ( 'NONE', ( #45561 ), #29470, .T. ) ;
#77119 = CARTESIAN_POINT ( 'NONE',  ( 3.177670542995198133, 1525.042412244750722, 176.6379763401895673 ) ) ;
#77120 = CARTESIAN_POINT ( 'NONE',  ( -9816.840209716168829, 50.13405481564039690, 1424.308828391800034 ) ) ;
#77121 = CARTESIAN_POINT ( 'NONE',  ( -1.984413551915469975, 1517.151704408390060, 219.3307686695569885 ) ) ;
#77122 = CARTESIAN_POINT ( 'NONE',  ( -2.659206587534440835, 1508.055408576787386, 220.9016337176575178 ) ) ;
#77123 = CARTESIAN_POINT ( 'NONE',  ( 17.79796669920695962, 1423.568134027953874, 226.0479527846472934 ) ) ;
#77124 = CARTESIAN_POINT ( 'NONE',  ( 10.79528402730720060, 1489.628194868570063, 207.4012257063180016 ) ) ;
#77125 = CARTESIAN_POINT ( 'NONE',  ( -3.286480964850000408, 1456.341185808290220, 218.0120306903490075 ) ) ;
#77126 = CARTESIAN_POINT ( 'NONE',  ( 17.27558691658489920, 1507.606285602530079, 193.9884222186300065 ) ) ;
#77127 = CARTESIAN_POINT ( 'NONE',  ( 26.51885050974659919, 1446.534126665770145, 137.5835070401340090 ) ) ;
#77129 = CARTESIAN_POINT ( 'NONE',  ( 4.327152622306750018, 1515.152479455989806, 208.7968194348430018 ) ) ;
#77128 = CARTESIAN_POINT ( 'NONE',  ( -11.81062501566809964, 1419.674596867499986, 197.5957448953309950 ) ) ;
#77130 = CARTESIAN_POINT ( 'NONE',  ( 7.112123000905755887, 1509.032357807246399, 202.3798014945801640 ) ) ;
#77131 = VERTEX_POINT ( 'NONE', #7233 ) ;
#77132 = CARTESIAN_POINT ( 'NONE',  ( 1.546943247107299912, 1416.828039266790029, 190.2227890105679933 ) ) ;
#77133 = CARTESIAN_POINT ( 'NONE',  ( 25.16773666439999957, 1469.174723959130233, 206.4821696811979734 ) ) ;
#77134 = DIRECTION ( 'NONE',  ( 0.2054769195713318786, 0.000000000000000000, -0.9786619618251628516 ) ) ;
#77135 = CARTESIAN_POINT ( 'NONE',  ( -24.39471867520000004, 1441.818671411180048, 212.1017248715180017 ) ) ;
#77136 = CARTESIAN_POINT ( 'NONE',  ( 9.754839755262800338, 1410.624863008607917, 188.5069135823247848 ) ) ;
#77137 = CARTESIAN_POINT ( 'NONE',  ( -3.841995486307249852, 1426.014736440487241, 186.0323716116992614 ) ) ;
#77138 = CARTESIAN_POINT ( 'NONE',  ( 29.16136750932905741, 1526.143142182216252, 220.6593063690870622 ) ) ;
#77139 = FACE_OUTER_BOUND ( 'NONE', #17527, .T. ) ;
#77140 = CARTESIAN_POINT ( 'NONE',  ( 3.217389378496539720, 1424.184544469090042, 188.9579904087769933 ) ) ;
#77141 = CARTESIAN_POINT ( 'NONE',  ( -74.26730215954620462, 1383.781415895790133, 299.1588454321730524 ) ) ;
#77142 = FACE_OUTER_BOUND ( 'NONE', #107400, .T. ) ;
#77143 = CARTESIAN_POINT ( 'NONE',  ( -27.73009598743778170, 1509.592383908645388, 212.1188701747986158 ) ) ;
#77145 = VECTOR ( 'NONE', #92764, 1000.000000000000000 ) ;
#77144 = DIRECTION ( 'NONE',  ( 0.9858563016923833633, 0.000000000000000000, 0.1675928173085483863 ) ) ;
#77147 = EDGE_LOOP ( 'NONE', ( #43890, #20072, #26003, #17340 ) ) ;
#77146 = CARTESIAN_POINT ( 'NONE',  ( 10.42932300190150130, 1451.825531649119966, 207.6750499181110001 ) ) ;
#77148 = CARTESIAN_POINT ( 'NONE',  ( -1.555730441549999954, 1414.913528139930122, 226.2389583330979974 ) ) ;
#77149 = CARTESIAN_POINT ( 'NONE',  ( -53.30655931660000135, 1379.972319575679876, 259.1995162978590201 ) ) ;
#77150 = CARTESIAN_POINT ( 'NONE',  ( -16.88043746970000214, 1409.502538253129842, 223.8714129622979954 ) ) ;
#77151 = VERTEX_POINT ( 'NONE', #74459 ) ;
#77152 = ORIENTED_EDGE ( 'NONE', *, *, #38617, .T. ) ;
#77153 = CARTESIAN_POINT ( 'NONE',  ( 20.02269696830319745, 1509.646906251600058, 231.0594384784430133 ) ) ;
#77154 = CARTESIAN_POINT ( 'NONE',  ( -5.714377949607280627, 1458.767755790989895, 212.7178556816730008 ) ) ;
#77155 = CARTESIAN_POINT ( 'NONE',  ( 39.52630824909760321, 1440.563701659530125, 136.7829907804839991 ) ) ;
#77157 = CARTESIAN_POINT ( 'NONE',  ( 1.804213551060599885, 1410.351307734219972, 232.1928989352460064 ) ) ;
#77156 = CARTESIAN_POINT ( 'NONE',  ( 18.34422345790000008, 1416.813004075630033, 209.3831160866600101 ) ) ;
#77158 = B_SPLINE_CURVE_WITH_KNOTS ( 'NONE', 3,
 ( #19131, #71256, #97521, #19703, #96984, #70707 ),
 .UNSPECIFIED., .F., .F.,
 ( 4, 2, 4 ),
 ( -0.08456724678697399855, -0.04349631223698429555, -3.514124158332521120E-09 ),
 .UNSPECIFIED. ) ;
#77159 = CARTESIAN_POINT ( 'NONE',  ( -18.53418666356940037, 1507.620785846770104, 229.7143111648900060 ) ) ;
#77160 = CARTESIAN_POINT ( 'NONE',  ( -109.5839456589999941, 1383.369684524640206, 297.2159463091589942 ) ) ;
#77161 = AXIS2_PLACEMENT_3D ( 'NONE', #74123, #108253, #66288 ) ;
#77162 = CARTESIAN_POINT ( 'NONE',  ( -12.74251030676457219, 1435.892414221138324, 150.8545518745174263 ) ) ;
#77163 = CARTESIAN_POINT ( 'NONE',  ( -19.87223104929999806, 1484.291808912129909, 191.2808552885979907 ) ) ;
#77164 = CARTESIAN_POINT ( 'NONE',  ( 2.296480925049999566, 1409.498280224829841, 185.7306842272979850 ) ) ;
#77165 = CARTESIAN_POINT ( 'NONE',  ( -1.080437161831740100, 1485.854186192430234, 197.2704867795639814 ) ) ;
#77166 = CARTESIAN_POINT ( 'NONE',  ( -6.218421316459999737, 1442.637438626040193, 154.8383831912979929 ) ) ;
#77167 = CARTESIAN_POINT ( 'NONE',  ( 9.273216669420000002, 1438.130896514020151, 153.0611339723980109 ) ) ;
#77168 = CARTESIAN_POINT ( 'NONE',  ( -2.500000000000000000, 1438.975676423110144, 156.0980984760799970 ) ) ;
#77169 = CARTESIAN_POINT ( 'NONE',  ( 32.86802468386292020, 1523.481610426287716, 217.2040256693915410 ) ) ;
#77170 = CARTESIAN_POINT ( 'NONE',  ( 1.793053373890000080, 1464.825772794629984, 236.8167814476979913 ) ) ;
#77171 = ORIENTED_EDGE ( 'NONE', *, *, #28567, .T. ) ;
#77172 = CARTESIAN_POINT ( 'NONE',  ( 22.23389067522870022, 1475.761154642579868, 209.7977657726480061 ) ) ;
#77173 = CARTESIAN_POINT ( 'NONE',  ( -39.85331664670000151, 1454.050829305929938, 270.3388278179979807 ) ) ;
#77174 = CARTESIAN_POINT ( 'NONE',  ( -23.71336536504703574, 1436.266214628221860, 212.4341823126743520 ) ) ;
#77175 = DIRECTION ( 'NONE',  ( -1.000000000000000000, 0.000000000000000000, 0.000000000000000000 ) ) ;
#77176 = CARTESIAN_POINT ( 'NONE',  ( 0.000000000000000000, 1511.163060387329779, 209.1218459616979999 ) ) ;
#77177 = AXIS2_PLACEMENT_3D ( 'NONE', #16635, #50302, #57048 ) ;
#77178 = CARTESIAN_POINT ( 'NONE',  ( -5.234639134658570038E-09, 1472.084393564380207, 259.1903821046649909 ) ) ;
#77179 = CARTESIAN_POINT ( 'NONE',  ( -19.94885833576309864, 1486.773834316860075, 191.0002569412860112 ) ) ;
#77180 = CARTESIAN_POINT ( 'NONE',  ( -1.309033247469999717, 1415.245980412430072, 227.1689405978980290 ) ) ;
#77181 = CARTESIAN_POINT ( 'NONE',  ( -9.915983682350001160, 1418.249051007830076, 230.0631123014979664 ) ) ;
#77182 = CARTESIAN_POINT ( 'NONE',  ( -1.749524734880000043, 1475.561370704890123, 198.2000993585989761 ) ) ;
#77183 = CARTESIAN_POINT ( 'NONE',  ( -108.0994041090000053, 1388.972225179880070, 310.0915140952590150 ) ) ;
#77184 = CARTESIAN_POINT ( 'NONE',  ( -7.591975382166549657, 1510.802068165409992, 214.6174606883600120 ) ) ;
#77185 = CARTESIAN_POINT ( 'NONE',  ( -4.745098151931287589, 1360.923919868593885, 210.6218459616991936 ) ) ;
#77186 = CARTESIAN_POINT ( 'NONE',  ( -46.08525396504009564, 1437.664701401070261, 267.5961899802729818 ) ) ;
#77187 = CARTESIAN_POINT ( 'NONE',  ( -33.93019615848960768, 1501.977400791986611, 197.6607374646001176 ) ) ;
#77188 = CARTESIAN_POINT ( 'NONE',  ( -5.303285988883490454, 1442.879254652209966, 200.5943008362860098 ) ) ;
#77189 = ORIENTED_EDGE ( 'NONE', *, *, #38464, .F. ) ;
#77190 = CARTESIAN_POINT ( 'NONE',  ( 4.625789976465000564, 1517.104192383289956, 210.2432295619669844 ) ) ;
#77191 = CARTESIAN_POINT ( 'NONE',  ( -5.423613671689999194, 1436.253592826889872, 154.6924146223979903 ) ) ;
#77192 = CARTESIAN_POINT ( 'NONE',  ( 19.26235814462797080, 1456.284170134162196, 224.9177539954318945 ) ) ;
#77193 = CARTESIAN_POINT ( 'NONE',  ( 7.532490811327241076, 1425.518623867940050, 212.1875454003960044 ) ) ;
#77194 = AXIS2_PLACEMENT_3D ( 'NONE', #97191, #31088, #54675 ) ;
#77195 = CARTESIAN_POINT ( 'NONE',  ( -25.57130305119999747, 1451.861998525429954, 136.0021594398979801 ) ) ;
#77196 = ORIENTED_EDGE ( 'NONE', *, *, #107194, .T. ) ;
#77197 = CARTESIAN_POINT ( 'NONE',  ( 22.58669161350000110, 1429.440852403829922, 225.6931608660979975 ) ) ;
#77199 = CARTESIAN_POINT ( 'NONE',  ( -15.16689671995240118, 1513.426431440490205, 223.4767850746570161 ) ) ;
#77198 = CARTESIAN_POINT ( 'NONE',  ( -3.302453616664800418, 1524.523992613103019, 176.3738900077313758 ) ) ;
#77200 =( BOUNDED_SURFACE ( )  B_SPLINE_SURFACE ( 3, 2, ( 
 ( #101245, #24544, #86682 ),
 ( #7763, #68809, #16147 ),
 ( #35177, #50351, #86134 ),
 ( #33498, #102911, #103470 ),
 ( #110781, #8309, #25100 ),
 ( #85015, #95090, #69360 ),
 ( #34072, #68265, #26777 ),
 ( #59846, #43041, #75546 ),
 ( #8858, #109682, #9427 ),
 ( #77198, #17793, #501 ),
 ( #26210, #60399, #51993 ),
 ( #43591, #77739, #53670 ),
 ( #71594, #105714, #79401 ),
 ( #44706, #96756, #27327 ) ),
 .UNSPECIFIED., .F., .F., .F. ) 
 B_SPLINE_SURFACE_WITH_KNOTS ( ( 4, 2, 2, 2, 2, 2, 4 ),
 ( 3, 3 ),
 ( 3.503057219300664826E-16, 0.0009443072508239316355, 0.001416460876235722246, 0.001888614501647512857, 0.002360768127059303251, 0.002832921752471094078, 0.003777229003294675300 ),
 ( 0.000000000000000000, 1.000000000000000000 ),
 .UNSPECIFIED. ) 
 GEOMETRIC_REPRESENTATION_ITEM ( )  RATIONAL_B_SPLINE_SURFACE ( (
 ( 1.000000000000000000, 0.9376006582765973318, 1.000000000000000000),
 ( 1.000000000000000000, 0.9283977714730347053, 1.000000000000000000),
 ( 1.000000000000000000, 0.9189750060488452998, 1.000000000000000000),
 ( 1.000000000000000000, 0.9042792056123225564, 1.000000000000000000),
 ( 1.000000000000000000, 0.8992469033844563420, 1.000000000000000000),
 ( 1.000000000000000000, 0.8891280264680836432, 1.000000000000000000),
 ( 1.000000000000000000, 0.8840337471678507697, 1.000000000000000000),
 ( 1.000000000000000000, 0.8736395124160363235, 1.000000000000000000),
 ( 1.000000000000000000, 0.8683406746552264632, 1.000000000000000000),
 ( 1.000000000000000000, 0.8573361860708257343, 1.000000000000000000),
 ( 1.000000000000000000, 0.8516508399493437631, 1.000000000000000000),
 ( 1.000000000000000000, 0.8340914917071454715, 1.000000000000000000),
 ( 1.000000000000000000, 0.8215597275857998705, 1.000000000000000000),
 ( 1.000000000000000000, 0.8070209408750025348, 1.000000000000000000) ) ) 
 REPRESENTATION_ITEM ( '' )  SURFACE ( )  );
#77201 = CARTESIAN_POINT ( 'NONE',  ( -0.4074389651556699632, 1487.893877509609638, 219.9700315476485457 ) ) ;
#77202 = CARTESIAN_POINT ( 'NONE',  ( -19.27620331059999970, 1429.330891638030153, 211.8895311099979892 ) ) ;
#77203 = CARTESIAN_POINT ( 'NONE',  ( 7.890413475299999924, 1422.993678601120109, 213.8680409669790095 ) ) ;
#77204 = CARTESIAN_POINT ( 'NONE',  ( -0.9496117000910009320, 1455.546544636789804, 215.7787860308390009 ) ) ;
#77205 = DIRECTION ( 'NONE',  ( 1.755985294532464991E-16, -1.000000000000000000, 1.338183447452830017E-16 ) ) ;
#77206 = EDGE_LOOP ( 'NONE', ( #27725, #36425, #5275, #23754 ) ) ;
#77207 = CARTESIAN_POINT ( 'NONE',  ( -1.857564137763940026, 1408.260413705610063, 270.3921255040010010 ) ) ;
#77208 = CARTESIAN_POINT ( 'NONE',  ( 6.289830419486070134, 1417.554321210839817, 231.5395384113830062 ) ) ;
#77209 = CARTESIAN_POINT ( 'NONE',  ( -5.775165567126295585, 1509.036904579127395, 216.6345513647860344 ) ) ;
#77211 = ORIENTED_EDGE ( 'NONE', *, *, #1647, .T. ) ;
#77210 = FACE_OUTER_BOUND ( 'NONE', #91597, .T. ) ;
#77212 = VERTEX_POINT ( 'NONE', #83373 ) ;
#77213 = CARTESIAN_POINT ( 'NONE',  ( -23.79955979311329983, 1410.855393305810139, 210.1471472738759871 ) ) ;
#77214 = CARTESIAN_POINT ( 'NONE',  ( -4.117509958049999419, 1423.942521120929996, 184.8346656465980118 ) ) ;
#77215 = CARTESIAN_POINT ( 'NONE',  ( -12.84239665067440050, 1435.935719077439899, 150.8114796122480072 ) ) ;
#77216 = CARTESIAN_POINT ( 'NONE',  ( -9.393138309199999370, 1428.175987565129844, 133.6118001900980232 ) ) ;
#77217 = PRESENTATION_LAYER_ASSIGNMENT (  '', '', ( #53993 ) ) ;
#77218 = CARTESIAN_POINT ( 'NONE',  ( -20.72930395482273980, 1436.452857176349426, 144.6331020082059524 ) ) ;
#77219 = CARTESIAN_POINT ( 'NONE',  ( -22.76855102469999892, 1420.825742769929775, 213.4933674877779879 ) ) ;
#77220 = EDGE_CURVE ( 'NONE', #108859, #25949, #76972, .T. ) ;
#77221 = CARTESIAN_POINT ( 'NONE',  ( 39.21901426951580305, 1459.467597158179842, 268.4332945158389521 ) ) ;
#77222 = CARTESIAN_POINT ( 'NONE',  ( -11.65026559816559981, 1391.913060387150153, 208.7216013930580232 ) ) ;
#77223 = CARTESIAN_POINT ( 'NONE',  ( -31.12456774391156600, 1525.960063244517187, 217.0912716842400698 ) ) ;
#77224 = CARTESIAN_POINT ( 'NONE',  ( 6.546951682585000043, 1516.606339319019980, 206.2472570094369928 ) ) ;
#77225 = ORIENTED_EDGE ( 'NONE', *, *, #79903, .T. ) ;
#77226 = CARTESIAN_POINT ( 'NONE',  ( 18.37403822010337606, 1459.029453797243377, 227.7512596423872537 ) ) ;
#77227 = CARTESIAN_POINT ( 'NONE',  ( -0.3874239798002959700, 1444.710807817890100, 199.0717356154370066 ) ) ;
#77228 = CYLINDRICAL_SURFACE ( 'NONE', #13971, 1.999999999999999556 ) ;
#77229 = EDGE_LOOP ( 'NONE', ( #54490, #68123, #54802, #55214 ) ) ;
#77230 = CARTESIAN_POINT ( 'NONE',  ( 4.038582018629999659, 1515.598601288590089, 209.1218459616989946 ) ) ;
#77232 = EDGE_CURVE ( 'NONE', #37845, #64533, #56706, .T. ) ;
#77231 = CARTESIAN_POINT ( 'NONE',  ( 25.64531625424840300, 1451.299216082280054, 136.7230207455749849 ) ) ;
#77233 = CARTESIAN_POINT ( 'NONE',  ( -3.301717782203759999, 1508.551704408389924, 213.9725500436610162 ) ) ;
#77234 = CARTESIAN_POINT ( 'NONE',  ( -4.167839424791409599E-16, 1389.896721459789887, 214.6127231082590185 ) ) ;
#77235 = CARTESIAN_POINT ( 'NONE',  ( 8.003593684729999325, 1421.506473294969965, 195.9720126397990043 ) ) ;
#77236 = CARTESIAN_POINT ( 'NONE',  ( 18.19540490880000050, 1409.548457928130119, 195.8472809290980194 ) ) ;
#77237 = CARTESIAN_POINT ( 'NONE',  ( 13.51610093809999924, 1443.913060387330006, 169.3501091259980171 ) ) ;
#77238 = CARTESIAN_POINT ( 'NONE',  ( -32.02808312589908013, 1511.187213306747708, 220.9649204700466782 ) ) ;
#77240 = CARTESIAN_POINT ( 'NONE',  ( -18.87276086228866134, 1424.762499899002478, 224.4369045893865859 ) ) ;
#77239 = CARTESIAN_POINT ( 'NONE',  ( 1.161811177069999923, 1415.656198137530055, 233.0499152497979765 ) ) ;
#77241 = CARTESIAN_POINT ( 'NONE',  ( 1.245434630070580084, 1451.852414238919891, 183.2837320638540177 ) ) ;
#77242 = CIRCLE ( 'NONE', #86176, 1.999999999999967359 ) ;
#77243 = CARTESIAN_POINT ( 'NONE',  ( -0.2698014165509999840, 1467.673031231229743, 229.6951974530979896 ) ) ;
#77244 = CARTESIAN_POINT ( 'NONE',  ( -8.039279795659998840, 1382.384107263689884, 218.6139994057390084 ) ) ;
#77245 = CARTESIAN_POINT ( 'NONE',  ( 16.62685400382315137, 1423.339598140291173, 229.2113107412401121 ) ) ;
#77246 = ORIENTED_EDGE ( 'NONE', *, *, #83786, .F. ) ;
#77247 = CARTESIAN_POINT ( 'NONE',  ( 10.86245182430920053, 1414.913060387399810, 221.4373602865120176 ) ) ;
#77248 = CYLINDRICAL_SURFACE ( 'NONE', #101729, 8.000000000000000000 ) ;
#77249 = CARTESIAN_POINT ( 'NONE',  ( 19.65496168979899849, 1477.254282174050104, 226.3273697325350042 ) ) ;
#77250 = CARTESIAN_POINT ( 'NONE',  ( -13.44625623449999985, 1389.878228146560105, 205.4975164690590077 ) ) ;
#77251 = CARTESIAN_POINT ( 'NONE',  ( 9.722118187324769067, 1428.114093149220025, 212.2006445887890038 ) ) ;
#77252 = CARTESIAN_POINT ( 'NONE',  ( -35.49482433925479796, 1450.187122272009901, 136.2332348560269679 ) ) ;
#77253 = CARTESIAN_POINT ( 'NONE',  ( -11.02639390884469961, 1462.494802824179942, 208.5122157637580074 ) ) ;
#77254 = VECTOR ( 'NONE', #41013, 1000.000000000000114 ) ;
#77255 = CARTESIAN_POINT ( 'NONE',  ( -6.832964021560000489, 1472.413060387330006, 271.1218459616979999 ) ) ;
#77256 = CARTESIAN_POINT ( 'NONE',  ( -21.72816396132508387, 1509.385241977931855, 191.5789249730982817 ) ) ;
#77257 = CARTESIAN_POINT ( 'NONE',  ( 11.07785633880000020, 1433.780515129440118, 151.7038518673980150 ) ) ;
#77258 = CARTESIAN_POINT ( 'NONE',  ( 20.74408968300000211, 1445.748654444839985, 224.8635562271979893 ) ) ;
#77259 = CARTESIAN_POINT ( 'NONE',  ( -10.15934713503659914, 1461.826274973950149, 209.4099054465810070 ) ) ;
#77260 = CARTESIAN_POINT ( 'NONE',  ( 18.26072392659999721, 1430.705547050490168, 200.8927042014090034 ) ) ;
#77261 = CARTESIAN_POINT ( 'NONE',  ( 11.10393296898399917, 1422.031618569310012, 201.8322731501689873 ) ) ;
#77262 = CARTESIAN_POINT ( 'NONE',  ( 4.577373674521229674, 1466.377811852470131, 218.3518963470609719 ) ) ;
#77263 = CARTESIAN_POINT ( 'NONE',  ( 22.65292971370000075, 1409.704085498430004, 208.9051947466459751 ) ) ;
#77264 = CARTESIAN_POINT ( 'NONE',  ( 11.57393272574848098, 1398.256210180372136, 215.0439578202975497 ) ) ;
#77265 = CARTESIAN_POINT ( 'NONE',  ( -21.51266965019000210, 1509.664297269830058, 231.4111640300060060 ) ) ;
#77266 = CIRCLE ( 'NONE', #9398, 15.41143114519999990 ) ;
#77267 = CARTESIAN_POINT ( 'NONE',  ( 23.22702228879999709, 1430.350733257130059, 215.3285367829879817 ) ) ;
#77268 = CARTESIAN_POINT ( 'NONE',  ( 1.847634001515719993, 1478.089546411300262, 198.8590795898780073 ) ) ;
#77269 = CARTESIAN_POINT ( 'NONE',  ( 25.55657149410041029, 1436.634586687895762, 137.2252252342358076 ) ) ;
#77270 = CARTESIAN_POINT ( 'NONE',  ( -1.070047859720000050, 1515.100834970490041, 204.7933409809490115 ) ) ;
#77271 = CARTESIAN_POINT ( 'NONE',  ( 18.88069888589999934, 1519.913060387329779, 221.9840912428979891 ) ) ;
#77272 = CARTESIAN_POINT ( 'NONE',  ( -18.32377787238529976, 1464.077817495989848, 217.4721512438379989 ) ) ;
#77273 = CARTESIAN_POINT ( 'NONE',  ( -1.120543735785000106, 1517.073005577650065, 213.1661658574570026 ) ) ;
#77275 = AXIS2_PLACEMENT_3D ( 'NONE', #34049, #41905, #76061 ) ;
#77274 = CARTESIAN_POINT ( 'NONE',  ( -17.92363191590630223, 1419.539427151339851, 207.5409190893379900 ) ) ;
#77276 = CARTESIAN_POINT ( 'NONE',  ( -2.330134126718832466, 1515.372048949687496, 204.8601094097913062 ) ) ;
#77278 = VERTEX_POINT ( 'NONE', #109692 ) ;
#77277 = CARTESIAN_POINT ( 'NONE',  ( 3.007039907259999811, 1441.535623192690082, 218.1727213951389786 ) ) ;
#77279 = DIRECTION ( 'NONE',  ( -1.000000000000000000, 0.000000000000000000, 0.000000000000000000 ) ) ;
#77280 = CARTESIAN_POINT ( 'NONE',  ( -17.22592475669603473, 1444.324653571829685, 162.9227486557985003 ) ) ;
#77281 = CARTESIAN_POINT ( 'NONE',  ( 13.19839718189999900, 1434.900414472690045, 149.8854151423980170 ) ) ;
#77282 = CARTESIAN_POINT ( 'NONE',  ( -37.48372878019959842, 1450.753171827299866, 134.0999999986339901 ) ) ;
#77283 = CARTESIAN_POINT ( 'NONE',  ( 0.000000000000000000, 1512.413060387330006, 209.1218459616979999 ) ) ;
#77284 = ORIENTED_EDGE ( 'NONE', *, *, #38349, .F. ) ;
#77285 = CARTESIAN_POINT ( 'NONE',  ( -38.64250925225250199, 1443.812098351759914, 137.1879208927209959 ) ) ;
#77286 = CARTESIAN_POINT ( 'NONE',  ( -12.80774525297199951, 1390.891660332020138, 210.6890168614469871 ) ) ;
#77287 = CARTESIAN_POINT ( 'NONE',  ( 7.034933902804894501, 1447.215032318710655, 203.3807619420004471 ) ) ;
#77288 = CARTESIAN_POINT ( 'NONE',  ( 5.058911271898960393, 1501.257153743159961, 229.8391433438629861 ) ) ;
#77289 = CARTESIAN_POINT ( 'NONE',  ( -4.221863112604749446, 1432.192955440190190, 216.4616610906159906 ) ) ;
#77290 = CARTESIAN_POINT ( 'NONE',  ( -107.9736457860882268, 1380.698907176378498, 309.9509774194930856 ) ) ;
#77291 = CARTESIAN_POINT ( 'NONE',  ( -17.06449333799999835, 1423.205374796969863, 209.2384713359739976 ) ) ;
#77292 = CARTESIAN_POINT ( 'NONE',  ( -17.99954540876850118, 1410.904693920620048, 195.2564682659330231 ) ) ;
#77293 = CARTESIAN_POINT ( 'NONE',  ( -11.42119214989999954, 1391.324142034819943, 204.4961053831890183 ) ) ;
#77294 = CARTESIAN_POINT ( 'NONE',  ( -67.67823920127010240, 1385.100504050170002, 260.9636858420549856 ) ) ;
#77295 = CARTESIAN_POINT ( 'NONE',  ( -17.34479452230000263, 1421.466062287029899, 191.6560375100980025 ) ) ;
#77296 = CARTESIAN_POINT ( 'NONE',  ( 11.41385934714260131, 1427.071059820410028, 208.0189296849380014 ) ) ;
#77297 = ORIENTED_EDGE ( 'NONE', *, *, #84652, .F. ) ;
#77298 = CARTESIAN_POINT ( 'NONE',  ( 19.64599270300000100, 1476.662575758389949, 214.0395835971089866 ) ) ;
#77300 = VERTEX_POINT ( 'NONE', #40274 ) ;
#77299 = DIRECTION ( 'NONE',  ( -0.8386695113602927742, -0.4884709562387165027, 0.2408932868012759743 ) ) ;
#77301 = CARTESIAN_POINT ( 'NONE',  ( 5.204738269408170304, 1467.429567479219941, 217.6200523410610117 ) ) ;
#77302 = VERTEX_POINT ( 'NONE', #32968 ) ;
#77303 = CARTESIAN_POINT ( 'NONE',  ( 18.95676294599999778, 1454.627617991990064, 205.4346706876590076 ) ) ;
#77304 = CARTESIAN_POINT ( 'NONE',  ( -9.505471540889999460, 1363.500209798499782, 207.6218459616989946 ) ) ;
#77305 = CARTESIAN_POINT ( 'NONE',  ( -13.77266209894789917, 1517.151704408390060, 217.0393652727940150 ) ) ;
#77306 = CARTESIAN_POINT ( 'NONE',  ( -4.468129194875738897, 1440.960114343879923, 155.7399638150290002 ) ) ;
#77307 = CARTESIAN_POINT ( 'NONE',  ( -22.52609270459879909, 1509.699688878229836, 190.3921826462719764 ) ) ;
#77308 = CARTESIAN_POINT ( 'NONE',  ( 16.50752364097115432, 1432.498724059854794, 217.9353314166346536 ) ) ;
#77309 = CARTESIAN_POINT ( 'NONE',  ( 2.324664979250000041, 1417.769420424829832, 234.1229704360980008 ) ) ;
#77310 = CARTESIAN_POINT ( 'NONE',  ( 4.195509702449999878, 1446.137837910890084, 200.9285957949090005 ) ) ;
#77311 = CARTESIAN_POINT ( 'NONE',  ( -0.4794255386042055589, 1405.913060387330006, 208.2442633998076076 ) ) ;
#77312 = CARTESIAN_POINT ( 'NONE',  ( -8.232155009519999567, 1367.485244382299925, 207.6218459616989946 ) ) ;
#77313 = CARTESIAN_POINT ( 'NONE',  ( -30.45769963430608129, 1526.208281990539263, 217.1507671409966349 ) ) ;
#77314 = CARTESIAN_POINT ( 'NONE',  ( -4.043366258305000294, 1516.951766529250108, 206.2549880390970145 ) ) ;
#77315 = CARTESIAN_POINT ( 'NONE',  ( 3.143430471549999883, 1447.188766879889954, 156.1110924090980063 ) ) ;
#77316 = LINE ( 'NONE', #60527, #78047 ) ;
#77317 = CARTESIAN_POINT ( 'NONE',  ( -2.982626223070000027, 1495.726940333489893, 197.1455590585989910 ) ) ;
#77319 = ORIENTED_EDGE ( 'NONE', *, *, #45529, .T. ) ;
#77318 = CARTESIAN_POINT ( 'NONE',  ( 0.07386333743999859425, 1495.692473857890036, 220.7224845649989788 ) ) ;
#77320 = DIRECTION ( 'NONE',  ( 0.000000000000000000, -1.000000000000000000, 0.000000000000000000 ) ) ;
#77321 = VERTEX_POINT ( 'NONE', #82284 ) ;
#77322 = CARTESIAN_POINT ( 'NONE',  ( -16.60142423921517718, 1513.050501378448644, 221.1601934794027784 ) ) ;
#77323 = CARTESIAN_POINT ( 'NONE',  ( -24.81840806659999998, 1430.361839728229825, 208.2500735500409803 ) ) ;
#77325 = CARTESIAN_POINT ( 'NONE',  ( 16.90311995223630248, 1409.749624152390197, 192.7847012683340040 ) ) ;
#77324 = CARTESIAN_POINT ( 'NONE',  ( -11.32017911025210033, 1426.032081424100170, 121.9038151518229967 ) ) ;
#77326 = CARTESIAN_POINT ( 'NONE',  ( -1.118353254094999860, 1516.977201124959947, 211.6155430111569729 ) ) ;
#77327 = CARTESIAN_POINT ( 'NONE',  ( 13.83427921383815296, 1509.519097606679679, 182.4629909201055113 ) ) ;
#77328 = FACE_OUTER_BOUND ( 'NONE', #86147, .T. ) ;
#77329 = CARTESIAN_POINT ( 'NONE',  ( -41.56051825480000161, 1440.913060433189912, 261.5689736827979459 ) ) ;
#77330 = CARTESIAN_POINT ( 'NONE',  ( 14.12038737319999804, 1509.406339941330089, 234.8413163218980060 ) ) ;
#77331 = CARTESIAN_POINT ( 'NONE',  ( 17.83610898133235523, 1459.676779477080800, 228.1619011578495702 ) ) ;
#77332 = APPLICATION_PROTOCOL_DEFINITION ( 'draft international standard', 'automotive_design', 1998, #39875 ) ;
#77333 = CARTESIAN_POINT ( 'NONE',  ( -5.156155033729999282, 1391.908488887390149, 214.6091172688990127 ) ) ;
#77334 = CARTESIAN_POINT ( 'NONE',  ( -34.23216826509359834, 1437.030530471749898, 136.5523443324769914 ) ) ;
#77335 = ORIENTED_EDGE ( 'NONE', *, *, #101724, .F. ) ;
#77336 = CARTESIAN_POINT ( 'NONE',  ( 7.347645689298669680, 1396.698419829339855, 197.9933311278070107 ) ) ;
#77337 = CARTESIAN_POINT ( 'NONE',  ( -19.72124761859999964, 1465.041912645589946, 210.1751448674889673 ) ) ;
#77338 = CARTESIAN_POINT ( 'NONE',  ( -16.17568645049999887, 1459.146939831430018, 230.7169136887979732 ) ) ;
#77339 = VERTEX_POINT ( 'NONE', #5582 ) ;
#77340 = EDGE_LOOP ( 'NONE', ( #16162, #10138, #37654, #52909 ) ) ;
#77341 = CARTESIAN_POINT ( 'NONE',  ( 9.146446762356999827, 1451.678219335869926, 210.6876116052179952 ) ) ;
#77342 = CARTESIAN_POINT ( 'NONE',  ( 5.662127998274639649E-15, 1428.868816406519954, 155.3340242552920074 ) ) ;
#77343 = DIRECTION ( 'NONE',  ( -0.03006000153037165917, -0.4884709562386974624, 0.8720622232497212689 ) ) ;
#77344 = CARTESIAN_POINT ( 'NONE',  ( -12.72547068037749973, 1417.199233372673916, 200.4382052065058417 ) ) ;
#77346 = DIRECTION ( 'NONE',  ( -0.2020450484956257953, -0.9583089390315990830, 0.2020439945916019109 ) ) ;
#77345 = AXIS2_PLACEMENT_3D ( 'NONE', #45868, #4408, #105769 ) ;
#77347 = CARTESIAN_POINT ( 'NONE',  ( -2.074664006059999899, 1461.195951710430109, 235.0034078370979955 ) ) ;
#77348 = CARTESIAN_POINT ( 'NONE',  ( 7.167019213074620865, 1508.551563895499839, 203.6086053948930044 ) ) ;
#77349 = CARTESIAN_POINT ( 'NONE',  ( 9.221327038241270202, 1450.741336465750237, 208.5540976675539753 ) ) ;
#77350 = CARTESIAN_POINT ( 'NONE',  ( -12.48995958559999941, 1501.883328862989856, 211.6213070104490157 ) ) ;
#77351 = CARTESIAN_POINT ( 'NONE',  ( -107.2131581586909874, 1384.895988242240037, 297.0540560109790249 ) ) ;
#77352 = VERTEX_POINT ( 'NONE', #57663 ) ;
#77353 = CARTESIAN_POINT ( 'NONE',  ( 4.613762356885000138, 1516.939574742129935, 203.3372076122869885 ) ) ;
#77354 = CARTESIAN_POINT ( 'NONE',  ( -2.873919040654999701, 1516.940252185109784, 209.1351185066319829 ) ) ;
#77355 = ORIENTED_EDGE ( 'NONE', *, *, #106261, .F. ) ;
#77356 = CARTESIAN_POINT ( 'NONE',  ( 10.79382126600000014, 1414.913060387329779, 222.1041115775979904 ) ) ;
#77357 = CARTESIAN_POINT ( 'NONE',  ( 3.605887597328768290, 1511.586661999378066, 217.1930125735252943 ) ) ;
#77358 = ORIENTED_EDGE ( 'NONE', *, *, #62048, .F. ) ;
#77359 = CARTESIAN_POINT ( 'NONE',  ( -1.464954376784709966, 1483.297409201249820, 182.5266383246559769 ) ) ;
#77360 = EDGE_CURVE ( 'NONE', #13046, #76760, #11296, .T. ) ;
#77361 = CARTESIAN_POINT ( 'NONE',  ( -11.79676896300389899, 1432.336587515399970, 150.5395565867330276 ) ) ;
#77362 = CARTESIAN_POINT ( 'NONE',  ( 3.014560028699999616, 1509.018331143230171, 237.6263297230979958 ) ) ;
#77363 = CARTESIAN_POINT ( 'NONE',  ( -8.728492600723082973, 1490.412091298440828, 215.7830027718222823 ) ) ;
#77364 = CARTESIAN_POINT ( 'NONE',  ( -5.092207154709999628, 1422.992073831329890, 184.8686965921980061 ) ) ;
#77365 = CARTESIAN_POINT ( 'NONE',  ( 6.470863363499999465, 1408.267973739730223, 270.2848116647979850 ) ) ;
#77366 = DIRECTION ( 'NONE',  ( -0.8775825618903725367, 0.000000000000000000, -0.4794255386042032829 ) ) ;
#77367 = CARTESIAN_POINT ( 'NONE',  ( -8.299659899499999938, 1474.751288659789907, 202.8760590113290050 ) ) ;
#77368 = CARTESIAN_POINT ( 'NONE',  ( 6.734164940669999488, 1492.669934513789940, 217.9607762184490127 ) ) ;
#77369 = CARTESIAN_POINT ( 'NONE',  ( -37.80579224959999607, 1379.643095642800063, 220.6117142568589884 ) ) ;
#77370 = CARTESIAN_POINT ( 'NONE',  ( -16.32008265250000179, 1485.103448096529974, 223.8634069782979736 ) ) ;
#77372 = DIRECTION ( 'NONE',  ( 0.03489949670244951035, -0.9993908270190976495, 0.000000000000000000 ) ) ;
#77371 = CARTESIAN_POINT ( 'NONE',  ( -3.753366994719999905, 1497.283149898290048, 198.4996119181990082 ) ) ;
#77373 = CARTESIAN_POINT ( 'NONE',  ( -4.996827698378051075, 1423.157233635628472, 184.7741671071053986 ) ) ;
#77374 = LINE ( 'NONE', #99924, #91448 ) ;
#77375 = CARTESIAN_POINT ( 'NONE',  ( -5.360123413344440202, 1422.242518929100015, 144.1648998030460120 ) ) ;
#77376 = VERTEX_POINT ( 'NONE', #32439 ) ;
#77377 = CARTESIAN_POINT ( 'NONE',  ( 28.54286204732486709, 1526.382868172863937, 198.4427524198199535 ) ) ;
#77378 = CARTESIAN_POINT ( 'NONE',  ( 33.36586802512172767, 1512.187213306747481, 201.9069332299488622 ) ) ;
#77379 = CARTESIAN_POINT ( 'NONE',  ( -2.953143827464752125, 1485.357549468870047, 182.9368206477720662 ) ) ;
#77380 = CARTESIAN_POINT ( 'NONE',  ( -14.68341694679999954, 1416.023439710309958, 213.8223955244490071 ) ) ;
#77382 = ORIENTED_EDGE ( 'NONE', *, *, #24147, .F. ) ;
#77381 = CARTESIAN_POINT ( 'NONE',  ( 0.2472019594487090133, 1515.155075545669888, 204.7947613204019888 ) ) ;
#77383 = CARTESIAN_POINT ( 'NONE',  ( 0.7397222398529998966, 1507.631725798030175, 186.3339393659980203 ) ) ;
#77384 = DIRECTION ( 'NONE',  ( -9.056288633775531119E-47, 1.000000000000000000, -1.836970198721029688E-16 ) ) ;
#77385 = CARTESIAN_POINT ( 'NONE',  ( -10.92055574760000169, 1428.871682173630006, 150.9007266609980320 ) ) ;
#77386 = CARTESIAN_POINT ( 'NONE',  ( 19.30758915063299952, 1456.939942660950010, 224.6494214983680138 ) ) ;
#77387 = DIRECTION ( 'NONE',  ( -1.000000000000000000, -2.249639673992789970E-32, -1.224646799147350002E-16 ) ) ;
#77388 = CARTESIAN_POINT ( 'NONE',  ( -2.579296836780000213, 1448.314969905590033, 190.1938323369989803 ) ) ;
#77389 = CARTESIAN_POINT ( 'NONE',  ( -109.1111611177930030, 1384.583257041720117, 311.2497810013429671 ) ) ;
#77390 = CARTESIAN_POINT ( 'NONE',  ( -15.69395960576500038, 1511.900571936589813, 221.5073600987669806 ) ) ;
#77391 = CARTESIAN_POINT ( 'NONE',  ( 3.424720300894999792, 1517.051704408389924, 200.5840233334270124 ) ) ;
#77392 = EDGE_CURVE ( 'NONE', #34085, #88970, #51325, .T. ) ;
#77394 = CARTESIAN_POINT ( 'NONE',  ( -10.32965322753309856, 1480.667151729589932, 206.9880687129259798 ) ) ;
#77393 = CARTESIAN_POINT ( 'NONE',  ( 0.4151546846821904668, 1524.726013923371283, 244.9330574173806383 ) ) ;
#77395 = CARTESIAN_POINT ( 'NONE',  ( -16.78521628583800052, 1460.263955658562054, 228.3353027301660063 ) ) ;
#77396 = CARTESIAN_POINT ( 'NONE',  ( -7.725990199955000470, 1517.181921232829836, 206.6366402828969910 ) ) ;
#77397 = CARTESIAN_POINT ( 'NONE',  ( 31.69002272450000035, 1415.319682416229853, 267.1138992859980021 ) ) ;
#77398 = CARTESIAN_POINT ( 'NONE',  ( 6.763640255447179445E-10, 1465.118916387369836, 238.1343321182859825 ) ) ;
#77399 = CARTESIAN_POINT ( 'NONE',  ( 22.21890555590000105, 1469.152603482329823, 196.0583803768979863 ) ) ;
#77400 = CARTESIAN_POINT ( 'NONE',  ( -0.2273306708084070205, 1508.146722782000097, 237.5484237907730005 ) ) ;
#77401 = CARTESIAN_POINT ( 'NONE',  ( -1.676216088789999947, 1450.511947750759873, 182.4451611760979972 ) ) ;
#77402 = CARTESIAN_POINT ( 'NONE',  ( -7.605711504302860249, 1407.218299713070110, 198.4634440487380118 ) ) ;
#77403 = CARTESIAN_POINT ( 'NONE',  ( -14.89294192899999913, 1417.697066551509806, 203.6067385514490127 ) ) ;
#77404 = CARTESIAN_POINT ( 'NONE',  ( -14.52606424000000018, 1443.052989431600054, 188.9151166515979980 ) ) ;
#77405 = DIRECTION ( 'NONE',  ( 1.000000000000000000, 0.000000000000000000, 0.000000000000000000 ) ) ;
#77406 = CARTESIAN_POINT ( 'NONE',  ( -8.589426147275000645, 1436.798469860880004, 209.9038450004319998 ) ) ;
#77407 = CARTESIAN_POINT ( 'NONE',  ( -7.395375191670000348, 1498.053836090689856, 218.0873371574190003 ) ) ;
#77408 = ORIENTED_EDGE ( 'NONE', *, *, #59298, .F. ) ;
#77409 = CARTESIAN_POINT ( 'NONE',  ( -2.689982596155000127, 1512.192993275409890, 201.4357459275669839 ) ) ;
#77410 = CARTESIAN_POINT ( 'NONE',  ( -14.83265502289820148, 1409.431028114330047, 210.8625800445090022 ) ) ;
#77411 = B_SPLINE_CURVE_WITH_KNOTS ( 'NONE', 3,
 ( #101762, #68215, #59798, #102320, #50304, #24502, #58692, #25606, #83325, #92825, #23948, #6620, #58145, #86632, #45771, #62021, #71546, #1002, #70426, #61465, #105667, #44657, #87194, #95591, #78798, #36239, #10486, #86087, #45215, #9927, #52503, #43544, #78235, #104545, #60347, #2113, #19979 ),
 .UNSPECIFIED., .F., .F.,
 ( 4, 3, 3, 3, 3, 3, 3, 3, 3, 3, 3, 3, 4 ),
 ( -1.999999730069600190, -1.888170853378660086, -1.719898845985929903, -1.549431836185619860, -1.377736129787159980, -1.204387122194009896, -1.030404623667469988, -0.8562074511777200136, -0.6822290056525619484, -0.5094606239557140093, -0.3379870002562179732, -0.1681008084855228901, -7.314383555279135862E-06 ),
 .UNSPECIFIED. ) ;
#77412 = CARTESIAN_POINT ( 'NONE',  ( -11.95044407570070000, 1508.551708580389914, 209.5547805494060185 ) ) ;
#77413 = CARTESIAN_POINT ( 'NONE',  ( 21.63731731441962935, 1524.599984580802129, 234.6744441581147953 ) ) ;
#77414 = CARTESIAN_POINT ( 'NONE',  ( -27.01637664349999923, 1469.366081882129947, 266.9349976846980326 ) ) ;
#77415 = CARTESIAN_POINT ( 'NONE',  ( 30.04349656869209895, 1524.760046179776054, 195.9289099819404214 ) ) ;
#77416 = CARTESIAN_POINT ( 'NONE',  ( 0.1634414413833199797, 1420.301959611109851, 183.5344649337699821 ) ) ;
#77417 = CARTESIAN_POINT ( 'NONE',  ( -25.23662982120000109, 1509.794342920329882, 222.8844980439979793 ) ) ;
#77418 = CARTESIAN_POINT ( 'NONE',  ( -81.43278738633540570, 1384.635623096480003, 304.7600304791900498 ) ) ;
#77419 = B_SPLINE_SURFACE_WITH_KNOTS ( 'NONE', 5, 1, ( 
 ( #47651, #73958 ),
 ( #5081, #65008 ),
 ( #48211, #82349 ),
 ( #31382, #57722 ),
 ( #6730, #65564 ),
 ( #22966, #99674 ) ),
 .UNSPECIFIED., .F., .F., .F.,
 ( 6, 6 ),
 ( 2, 2 ),
 ( 0.000000000000000000, 16.14237680569999966 ),
 ( 0.000000000000000000, 14.00000000000000000 ),
 .UNSPECIFIED. ) ;
#77420 = CARTESIAN_POINT ( 'NONE',  ( -26.92027982241999950, 1384.963071672040087, 204.0559658860740058 ) ) ;
#77421 = CARTESIAN_POINT ( 'NONE',  ( 9.786977751178733698, 1517.051704408389924, 226.9642986345448890 ) ) ;
#77422 = CARTESIAN_POINT ( 'NONE',  ( 11.86597105769770089, 1415.542389211310137, 223.1847760632660140 ) ) ;
#77423 = CARTESIAN_POINT ( 'NONE',  ( 2.487935142314050108, 1509.038615934839981, 213.6090957367470082 ) ) ;
#77424 = DIRECTION ( 'NONE',  ( 0.9455185755993178454, 0.000000000000000000, -0.3255681544571537578 ) ) ;
#77425 = CARTESIAN_POINT ( 'NONE',  ( -2.253566441613126910E-10, 1426.918876941764893, 137.0999999980980135 ) ) ;
#77426 = EDGE_CURVE ( 'NONE', #58087, #59861, #86144, .T. ) ;
#77427 = CARTESIAN_POINT ( 'NONE',  ( -23.37532479789999940, 1410.224545597529868, 206.6383130864379893 ) ) ;
#77428 = EDGE_CURVE ( 'NONE', #5861, #63089, #104045, .T. ) ;
#77429 = EDGE_CURVE ( 'NONE', #94174, #15766, #17778, .T. ) ;
#77430 = CARTESIAN_POINT ( 'NONE',  ( 17.83292642509999837, 1416.519106787730152, 206.2642702630979841 ) ) ;
#77431 = CARTESIAN_POINT ( 'NONE',  ( 4.533751981029999989, 1484.466359252490065, 219.6316280533989982 ) ) ;
#77432 = DIRECTION ( 'NONE',  ( 0.2054769195713296304, 0.000000000000000000, -0.9786619618251631847 ) ) ;
#77433 = EDGE_CURVE ( 'NONE', #9799, #75668, #33869, .T. ) ;
#77434 = CARTESIAN_POINT ( 'NONE',  ( 0.8348477807080000312, 1443.913060387330006, 150.8032249175980155 ) ) ;
#77435 = EDGE_CURVE ( 'NONE', #5162, #25680, #41151, .T. ) ;
#77436 = CARTESIAN_POINT ( 'NONE',  ( 11.65726901512490166, 1435.318858471669955, 225.6545570341099847 ) ) ;
#77437 = CARTESIAN_POINT ( 'NONE',  ( 16.97881484272545549, 1525.055402519452173, 181.2503677391246129 ) ) ;
#77438 = CARTESIAN_POINT ( 'NONE',  ( -5.586175246986850418, 1491.246062496780041, 185.8699218406250111 ) ) ;
#77440 = CARTESIAN_POINT ( 'NONE',  ( -9.263518881979999620, 1384.040644720069849, 200.0636813112390087 ) ) ;
#77439 = CARTESIAN_POINT ( 'NONE',  ( -21.33808675349999717, 1409.658202796229943, 210.9642962936580091 ) ) ;
#77441 = CARTESIAN_POINT ( 'NONE',  ( 11.69356494263769974, 1426.724475661050292, 141.0600989001800087 ) ) ;
#77442 = CARTESIAN_POINT ( 'NONE',  ( 9.749723431585490374, 1436.068361671160119, 210.4025069022860066 ) ) ;
#77443 = CARTESIAN_POINT ( 'NONE',  ( -15.06617558477470098, 1420.498972720419943, 211.7929360720449949 ) ) ;
#77444 = CARTESIAN_POINT ( 'NONE',  ( 5.079734284382990239, 1447.323964650199969, 200.2742450949660054 ) ) ;
#77445 = ADVANCED_FACE ( 'NONE', ( #41940 ), #28605, .T. ) ;
#77446 = CARTESIAN_POINT ( 'NONE',  ( 11.60004869885203682, 1428.983126981193436, 134.0999999980966777 ) ) ;
#77447 = CARTESIAN_POINT ( 'NONE',  ( 5.000083827734999709, 1516.858456333729919, 204.1129977322069919 ) ) ;
#77449 = CARTESIAN_POINT ( 'NONE',  ( 19.66678637246580053, 1519.551704408389924, 202.3500283489900085 ) ) ;
#77448 = B_SPLINE_CURVE_WITH_KNOTS ( 'NONE', 5,
 ( #68614, #16501, #58553, #51240, #15956, #26579 ),
 .UNSPECIFIED., .F., .F.,
 ( 6, 6 ),
 ( 0.000000000000000000, 1.000000000000000000 ),
 .UNSPECIFIED. ) ;
#77450 = FACE_BOUND ( 'NONE', #32621, .T. ) ;
#77451 = CARTESIAN_POINT ( 'NONE',  ( -18.84520706720000049, 1449.647908397599849, 193.3285045537979840 ) ) ;
#77452 =( NAMED_UNIT ( * ) PLANE_ANGLE_UNIT ( ) SI_UNIT ( $, .RADIAN. ) );
#77453 = CARTESIAN_POINT ( 'NONE',  ( -0.7790226144181949808, 1442.687261678630193, 200.2740145696140246 ) ) ;
#77455 = ORIENTED_EDGE ( 'NONE', *, *, #26199, .F. ) ;
#77454 = CARTESIAN_POINT ( 'NONE',  ( -62.63656304554481125, 1379.732098069620179, 270.6469071953959542 ) ) ;
#77456 = ORIENTED_EDGE ( 'NONE', *, *, #87774, .F. ) ;
#77457 = CARTESIAN_POINT ( 'NONE',  ( 11.94671513487030090, 1433.512659209229923, 149.9919407150609914 ) ) ;
#77458 = CARTESIAN_POINT ( 'NONE',  ( 20.68299398337628858, 1525.856065479229073, 184.2887586734088643 ) ) ;
#77459 = ORIENTED_EDGE ( 'NONE', *, *, #27407, .T. ) ;
#77460 = CARTESIAN_POINT ( 'NONE',  ( -106.5585968837300044, 1390.939245634569943, 300.3884029622149683 ) ) ;
#77461 = CARTESIAN_POINT ( 'NONE',  ( -10.36637489306960092, 1448.036064164660047, 209.0396054626149862 ) ) ;
#77462 = CARTESIAN_POINT ( 'NONE',  ( 2.956826570602010040, 1515.222544082249897, 204.7977243905010027 ) ) ;
#77464 = CARTESIAN_POINT ( 'NONE',  ( 4.496878417739999634, 1428.155750001629940, 101.8807690336980016 ) ) ;
#77463 = CARTESIAN_POINT ( 'NONE',  ( 16.05359747075639731, 1423.514842284070028, 191.1259792483479885 ) ) ;
#77465 = CARTESIAN_POINT ( 'NONE',  ( 10.89898159000000000, 1507.806799034729920, 234.1500837693980088 ) ) ;
#77466 = EDGE_CURVE ( 'NONE', #49508, #21931, #87228, .T. ) ;
#77467 = CARTESIAN_POINT ( 'NONE',  ( 1.347910446750000268, 1507.642032470829918, 181.0718040488980023 ) ) ;
#77468 = CARTESIAN_POINT ( 'NONE',  ( -2.824000289829999844, 1415.931784856029935, 191.4879063651980289 ) ) ;
#77469 = CARTESIAN_POINT ( 'NONE',  ( 13.13561839920526886, 1522.051704408389924, 209.9352119836111683 ) ) ;
#77470 = FILL_AREA_STYLE_COLOUR ( '', #109354 ) ;
#77471 = CARTESIAN_POINT ( 'NONE',  ( 5.012317068235000228, 1517.020727862619879, 211.9902797687369969 ) ) ;
#77472 = ADVANCED_FACE ( 'NONE', ( #43601 ), #1860, .T. ) ;
#77473 = CARTESIAN_POINT ( 'NONE',  ( 13.94822761382920184, 1415.393085341020196, 197.3723107886449952 ) ) ;
#77474 = CARTESIAN_POINT ( 'NONE',  ( 11.75433822149999941, 1431.172422370689901, 150.7091801069980193 ) ) ;
#77475 = CARTESIAN_POINT ( 'NONE',  ( 7.503873103355000573, 1512.035910181040208, 202.5568695388469962 ) ) ;
#77476 = ORIENTED_EDGE ( 'NONE', *, *, #81471, .F. ) ;
#77477 = CARTESIAN_POINT ( 'NONE',  ( 13.97106068711859983, 1435.306965887609977, 149.5915603287180033 ) ) ;
#77478 = CARTESIAN_POINT ( 'NONE',  ( -5.013264327984152224, 1375.413060387289988, 203.5257471471711312 ) ) ;
#77479 = ORIENTED_EDGE ( 'NONE', *, *, #60374, .T. ) ;
#77480 = ADVANCED_FACE ( 'NONE', ( #61523 ), #95577, .T. ) ;
#77481 = VERTEX_POINT ( 'NONE', #79412 ) ;
#77482 = CARTESIAN_POINT ( 'NONE',  ( 12.89600770202496882, 1444.937073510895061, 169.4370095252451733 ) ) ;
#77483 = CARTESIAN_POINT ( 'NONE',  ( -0.3222264186639999806, 1466.023156234830140, 235.8295837109980084 ) ) ;
#77484 = CARTESIAN_POINT ( 'NONE',  ( -12.75668250589355068, 1503.496714303483031, 208.6968331601771069 ) ) ;
#77485 = CARTESIAN_POINT ( 'NONE',  ( -6.554151464375000735, 1516.906641539930206, 216.4536580562070185 ) ) ;
#77486 = CARTESIAN_POINT ( 'NONE',  ( -8.302057905577099106, 1511.419855272942868, 213.4520019170473688 ) ) ;
#77487 = ADVANCED_FACE ( 'NONE', ( #72138 ), #63193, .T. ) ;
#77488 = CARTESIAN_POINT ( 'NONE',  ( -18.66998849382813219, 1445.113969046085003, 213.7790260993002107 ) ) ;
#77489 = CARTESIAN_POINT ( 'NONE',  ( -49.28295861101878472, 1379.685963475619246, 238.1969093270015776 ) ) ;
#77490 = DIRECTION ( 'NONE',  ( 0.000000000000000000, -6.123233995736769734E-17, -1.000000000000000000 ) ) ;
#77491 = EDGE_LOOP ( 'NONE', ( #110329, #88622, #78756, #34639, #78432 ) ) ;
#77492 = CARTESIAN_POINT ( 'NONE',  ( -6.949574985774999547, 1517.102359858469754, 205.8627441332170065 ) ) ;
#77493 = ORIENTED_EDGE ( 'NONE', *, *, #35497, .F. ) ;
#77494 = CARTESIAN_POINT ( 'NONE',  ( -105.3812835198930031, 1378.843491006310160, 304.0398711368210343 ) ) ;
#77495 = CARTESIAN_POINT ( 'NONE',  ( 2.409034624560000282, 1511.999350511789999, 206.7128113371389873 ) ) ;
#77496 = ORIENTED_EDGE ( 'NONE', *, *, #24172, .T. ) ;
#77497 = CARTESIAN_POINT ( 'NONE',  ( -7.050955535139999952, 1409.159285179630160, 188.4661246024980130 ) ) ;
#77498 = CARTESIAN_POINT ( 'NONE',  ( 8.118882928225001905, 1514.642928591849795, 215.6564664142569825 ) ) ;
#77500 = ORIENTED_EDGE ( 'NONE', *, *, #29200, .T. ) ;
#77499 = CARTESIAN_POINT ( 'NONE',  ( -7.052967567875161770, 1427.664849047028611, 137.0999999980979851 ) ) ;
#77501 = CARTESIAN_POINT ( 'NONE',  ( 24.45814044340000137, 1438.107944938759829, 212.7365612476880017 ) ) ;
#77502 = CARTESIAN_POINT ( 'NONE',  ( -16.94284628566209960, 1508.551704408389924, 210.3926682970049740 ) ) ;
#77503 = CARTESIAN_POINT ( 'NONE',  ( -12.02051106306990036, 1491.153688555679992, 206.6632162730240054 ) ) ;
#77504 = CARTESIAN_POINT ( 'NONE',  ( 9.959920982146540425, 1432.347050772769990, 152.5236881046529902 ) ) ;
#77505 = DIRECTION ( 'NONE',  ( -0.000000000000000000, -1.000000000000000000, -0.000000000000000000 ) ) ;
#77506 = CARTESIAN_POINT ( 'NONE',  ( -2.480813923114999930, 1517.051603658920158, 214.1347848340070072 ) ) ;
#77507 = B_SPLINE_CURVE_WITH_KNOTS ( 'NONE', 5,
 ( #86384, #10798, #86938, #19732, #88067, #45525 ),
 .UNSPECIFIED., .F., .F.,
 ( 6, 6 ),
 ( -2.000000000000000000, 0.000000000000000000 ),
 .UNSPECIFIED. ) ;
#77508 = CARTESIAN_POINT ( 'NONE',  ( -2.678371528919849975, 1429.099047671080143, 200.1418393138040130 ) ) ;
#77509 = EDGE_CURVE ( 'NONE', #5014, #39452, #88902, .T. ) ;
#77510 = CARTESIAN_POINT ( 'NONE',  ( -20.55810159319999997, 1507.794327612029974, 189.9655093376980233 ) ) ;
#77511 = CARTESIAN_POINT ( 'NONE',  ( 29.86461515634920971, 1525.960063244517187, 220.9690070206020494 ) ) ;
#77512 = CARTESIAN_POINT ( 'NONE',  ( -2.864326125434999870, 1516.826109302209943, 211.6149197999869784 ) ) ;
#77513 = EDGE_CURVE ( 'NONE', #31342, #28739, #73368, .T. ) ;
#77514 = CARTESIAN_POINT ( 'NONE',  ( 14.06841109650000021, 1410.335884455629866, 191.3015486027980216 ) ) ;
#77515 = CARTESIAN_POINT ( 'NONE',  ( -17.05332910918329148, 1486.127261448098807, 187.7340081784555537 ) ) ;
#77517 = ORIENTED_EDGE ( 'NONE', *, *, #30133, .F. ) ;
#77516 = CARTESIAN_POINT ( 'NONE',  ( -81.20151922889999696, 1386.553224299360181, 304.9219196665589493 ) ) ;
#77518 = CARTESIAN_POINT ( 'NONE',  ( -65.34101701133390350, 1385.041919093109982, 289.2241435049139682 ) ) ;
#77519 = CARTESIAN_POINT ( 'NONE',  ( 31.44037043649999674, 1456.450353286529889, 254.7811851438980284 ) ) ;
#77520 = CARTESIAN_POINT ( 'NONE',  ( 10.90828758974610047, 1490.545376044769910, 210.3161421217920122 ) ) ;
#77521 = CARTESIAN_POINT ( 'NONE',  ( 19.37182493330882593, 1526.345556099435726, 232.9230866865991629 ) ) ;
#77522 = CARTESIAN_POINT ( 'NONE',  ( -3.915418352780020150, 1508.947664731669875, 237.8621089956459969 ) ) ;
#77523 = CARTESIAN_POINT ( 'NONE',  ( -23.35577775049999971, 1449.058501480780251, 216.5496097239480093 ) ) ;
#77524 = ADVANCED_FACE ( 'NONE', ( #11647 ), #54231, .F. ) ;
#77526 = CARTESIAN_POINT ( 'NONE',  ( 17.10104755112020314, 1409.537284391650019, 222.2845644592789824 ) ) ;
#77525 = CARTESIAN_POINT ( 'NONE',  ( 11.76895983000000001, 1432.299379893459900, 150.8120316597980093 ) ) ;
#77527 = CARTESIAN_POINT ( 'NONE',  ( -9.203111897236890826, 1450.336789552200116, 208.5678280199140033 ) ) ;
#77528 = CARTESIAN_POINT ( 'NONE',  ( -108.2558473347470027, 1382.950532872079975, 310.7470917612149606 ) ) ;
#77529 = EDGE_LOOP ( 'NONE', ( #55371, #32853, #1594 ) ) ;
#77530 = CARTESIAN_POINT ( 'NONE',  ( -7.721907926364999675, 1517.026025493960105, 204.1173703575669833 ) ) ;
#77531 = CARTESIAN_POINT ( 'NONE',  ( -8.056653238513129978, 1508.431094367349942, 219.4233643241270215 ) ) ;
#77532 = CARTESIAN_POINT ( 'NONE',  ( 4.858360387713474893, 1508.551704413348716, 211.6097810847319920 ) ) ;
#77533 = CARTESIAN_POINT ( 'NONE',  ( 12.82226628359999943, 1419.802649937829983, 223.2233948557979772 ) ) ;
#77534 = CARTESIAN_POINT ( 'NONE',  ( 5.398680167209999325, 1433.945743868580166, 154.6429197126979886 ) ) ;
#77535 =( BOUNDED_CURVE ( )  B_SPLINE_CURVE ( 5, ( #98623, #55006, #29230, #73448, #37628, #98074 ),
 .UNSPECIFIED., .F., .T. ) 
 B_SPLINE_CURVE_WITH_KNOTS ( ( 6, 6 ),
 ( 0.000000000000000000, 1.000000000000000000 ),
 .UNSPECIFIED. ) 
 CURVE ( )  GEOMETRIC_REPRESENTATION_ITEM ( )  RATIONAL_B_SPLINE_CURVE ( ( 0.2685209231508545735, 0.2609802027898279753, 0.2554570136197181762, 0.2518190045398730481, 0.2499999999999668043, 0.2500000000000000000 ) ) 
 REPRESENTATION_ITEM ( '' )  );
#77536 = CARTESIAN_POINT ( 'NONE',  ( -28.11203376899999995, 1444.250560465929993, 137.5208087134980133 ) ) ;
#77537 = FACE_OUTER_BOUND ( 'NONE', #47427, .T. ) ;
#77538 = CARTESIAN_POINT ( 'NONE',  ( 27.34169902030170363, 1435.611507683570153, 136.1486617027460113 ) ) ;
#77539 = EDGE_CURVE ( 'NONE', #37235, #31591, #94784, .T. ) ;
#77540 = DIRECTION ( 'NONE',  ( 0.000000000000000000, -1.000000000000000000, 0.000000000000000000 ) ) ;
#77541 = CYLINDRICAL_SURFACE ( 'NONE', #77097, 0.9999999999999948930 ) ;
#77542 = CARTESIAN_POINT ( 'NONE',  ( -109.7887639940000071, 1385.331325759269930, 297.0716752156589564 ) ) ;
#77543 = CARTESIAN_POINT ( 'NONE',  ( 10.63508560284700089, 1480.849370521759965, 210.2894055373469939 ) ) ;
#77544 = CARTESIAN_POINT ( 'NONE',  ( 19.92151515271105566, 1526.208281990539490, 184.7237256173480944 ) ) ;
#77545 = CARTESIAN_POINT ( 'NONE',  ( -4.954768278013866656, 1446.481062136786022, 216.7370039512331914 ) ) ;
#77546 = EDGE_LOOP ( 'NONE', ( #72608, #81176, #32969, #107881 ) ) ;
#77548 = ADVANCED_FACE ( 'NONE', ( #37404 ), #9850, .T. ) ;
#77547 = CARTESIAN_POINT ( 'NONE',  ( -6.438546668759999925, 1410.951844103529993, 268.3665355202980436 ) ) ;
#77549 = CARTESIAN_POINT ( 'NONE',  ( 4.124008068921309444, 1455.961819920020162, 218.9107260925210028 ) ) ;
#77550 = TOROIDAL_SURFACE ( 'NONE', #41805, 30.13701971169416538, 3.000000000000000000 ) ;
#77551 = CARTESIAN_POINT ( 'NONE',  ( 0.9642394209830019713, 1486.365851861090050, 197.2124130950990093 ) ) ;
#77552 = CARTESIAN_POINT ( 'NONE',  ( -21.84020450222019250, 1523.382868172864164, 234.9798068779743403 ) ) ;
#77553 = CARTESIAN_POINT ( 'NONE',  ( -2.805498944269999911E-09, 1475.983410498229887, 267.2349610869979983 ) ) ;
#77555 = CARTESIAN_POINT ( 'NONE',  ( -17.22592475670000312, 1444.324653571829913, 162.9227486557980171 ) ) ;
#77554 = CARTESIAN_POINT ( 'NONE',  ( 11.87587340029999972, 1501.155101168290003, 209.4695087910589848 ) ) ;
#77556 = CARTESIAN_POINT ( 'NONE',  ( 19.19535387687943029, 1456.080104641030175, 225.8939609127118047 ) ) ;
#77557 = DIRECTION ( 'NONE',  ( -1.755985294532469921E-16, 1.000000000000000000, -1.338183447452831989E-16 ) ) ;
#77558 = CARTESIAN_POINT ( 'NONE',  ( -15.65684374876079943, 1384.875147521260033, 219.5768865249289945 ) ) ;
#77559 = CARTESIAN_POINT ( 'NONE',  ( 31.81407709660777527, 1501.977400791986611, 221.9534378623329758 ) ) ;
#77560 = CARTESIAN_POINT ( 'NONE',  ( -14.98234439516031813, 1451.152531978053503, 149.7337978842586779 ) ) ;
#77561 = CARTESIAN_POINT ( 'NONE',  ( -8.114589821750000098, 1483.072352354889972, 201.8754299783889792 ) ) ;
#77562 = CARTESIAN_POINT ( 'NONE',  ( 25.40170928279999885, 1435.672096233849970, 136.5747932110980116 ) ) ;
#77563 = ADVANCED_FACE ( 'NONE', ( #56969 ), #55476, .F. ) ;
#77564 = CARTESIAN_POINT ( 'NONE',  ( -7.287693820798589961, 1396.167552263480047, 200.8210620288550103 ) ) ;
#77565 = ORIENTED_EDGE ( 'NONE', *, *, #86306, .T. ) ;
#77566 = CARTESIAN_POINT ( 'NONE',  ( -16.24136799685820165, 1409.480169776980119, 225.1139067059710044 ) ) ;
#77567 = EDGE_CURVE ( 'NONE', #94550, #35126, #55876, .T. ) ;
#77568 = CARTESIAN_POINT ( 'NONE',  ( 3.035119290295853034, 1377.913060387289988, 207.4637527364374705 ) ) ;
#77569 = VERTEX_POINT ( 'NONE', #24851 ) ;
#77570 = ORIENTED_EDGE ( 'NONE', *, *, #34461, .T. ) ;
#77571 = CARTESIAN_POINT ( 'NONE',  ( 7.075014806132906564, 1516.558166122959847, 206.6310126780043674 ) ) ;
#77573 = CARTESIAN_POINT ( 'NONE',  ( 1.520272259658780101, 1456.597953077289958, 219.6336397091319839 ) ) ;
#77572 = CARTESIAN_POINT ( 'NONE',  ( 10.33654884809999963, 1425.426884123429772, 91.92460148769789896 ) ) ;
#77574 = CARTESIAN_POINT ( 'NONE',  ( -11.07712053549999887, 1433.090719799819908, 151.6979285180979957 ) ) ;
#77575 = CARTESIAN_POINT ( 'NONE',  ( -2.497425431713394151, 1421.160177316890895, 184.9476756208646293 ) ) ;
#77576 = CARTESIAN_POINT ( 'NONE',  ( 7.230170464569999567, 1423.528413094569942, 213.4846319112089930 ) ) ;
#77577 = CARTESIAN_POINT ( 'NONE',  ( -2.775555821850000271, 1468.867611631090085, 187.4507004057990116 ) ) ;
#77578 = CARTESIAN_POINT ( 'NONE',  ( 8.326542548460000859, 1507.918730797030094, 183.0016923208980018 ) ) ;
#77579 = CARTESIAN_POINT ( 'NONE',  ( 3.492106839979999933, 1450.387407648259796, 184.0776196846979929 ) ) ;
#77580 = CARTESIAN_POINT ( 'NONE',  ( 8.126636070261570310, 1364.911473247693039, 208.3718459617061285 ) ) ;
#77581 = EDGE_CURVE ( 'NONE', #9164, #92866, #93955, .T. ) ;
#77582 = EDGE_CURVE ( 'NONE', #10167, #31573, #78722, .T. ) ;
#77584 = VERTEX_POINT ( 'NONE', #50641 ) ;
#77583 = CARTESIAN_POINT ( 'NONE',  ( -9.617209101676776228, 1463.011625816246806, 234.9738961404823954 ) ) ;
#77585 = ORIENTED_EDGE ( 'NONE', *, *, #19298, .T. ) ;
#77586 = CARTESIAN_POINT ( 'NONE',  ( -41.49257713859999797, 1443.691015385260016, 136.5669737734980345 ) ) ;
#77587 = CARTESIAN_POINT ( 'NONE',  ( 7.519244400428443775, 1510.642476670986071, 203.1920689657892751 ) ) ;
#77588 = CARTESIAN_POINT ( 'NONE',  ( -0.9653266517330000296, 1472.614618005129842, 270.3713489653979991 ) ) ;
#77589 = CARTESIAN_POINT ( 'NONE',  ( 7.712506219943952246, 1500.328028434782254, 200.7279699965547763 ) ) ;
#77590 = CARTESIAN_POINT ( 'NONE',  ( -3.527564898500000101, 1486.518325717629978, 181.8541436997979872 ) ) ;
#77591 = CARTESIAN_POINT ( 'NONE',  ( -31.52384429374384567, 1525.730671948512054, 201.2079775281771390 ) ) ;
#77592 = CARTESIAN_POINT ( 'NONE',  ( -1.658825910028130179, 1475.382055513630121, 197.7986645737999822 ) ) ;
#77593 = CARTESIAN_POINT ( 'NONE',  ( 21.33808983710000007, 1409.658202903930032, 207.2794041873680158 ) ) ;
#77594 = CARTESIAN_POINT ( 'NONE',  ( -22.92687821287150030, 1507.614846683489986, 207.6532172876729874 ) ) ;
#77595 = CARTESIAN_POINT ( 'NONE',  ( 8.726849315049999944, 1367.111769039820047, 207.6218459616989946 ) ) ;
#77596 = CARTESIAN_POINT ( 'NONE',  ( 6.262051076867260591, 1407.785014201449940, 196.9935646766689956 ) ) ;
#77597 = CARTESIAN_POINT ( 'NONE',  ( -20.62979332817520017, 1409.412394061799887, 267.3561677121959974 ) ) ;
#77598 = CARTESIAN_POINT ( 'NONE',  ( -10.79382269979189957, 1414.913060387349788, 196.1395788316550011 ) ) ;
#77599 = EDGE_LOOP ( 'NONE', ( #56717, #34598, #103930 ) ) ;
#77600 = DIRECTION ( 'NONE',  ( 0.000000000000000000, 1.000000000000000000, 0.000000000000000000 ) ) ;
#77601 = CARTESIAN_POINT ( 'NONE',  ( 13.50895069809999960, 1444.844319576610133, 188.7199091778979891 ) ) ;
#77602 = EDGE_LOOP ( 'NONE', ( #13859, #27056, #82576, #7927 ) ) ;
#77603 = ORIENTED_EDGE ( 'NONE', *, *, #100368, .T. ) ;
#77604 = DIRECTION ( 'NONE',  ( 0.9510565162951478690, 0.000000000000000000, -0.3090169943749654369 ) ) ;
#77605 = CARTESIAN_POINT ( 'NONE',  ( 9.258247136799999666, 1363.198586359130104, 207.6218459616989946 ) ) ;
#77606 = EDGE_CURVE ( 'NONE', #12203, #96482, #44166, .T. ) ;
#77607 = CARTESIAN_POINT ( 'NONE',  ( 2.877744946244999991, 1516.723920667490120, 213.7309102736070088 ) ) ;
#77608 = CARTESIAN_POINT ( 'NONE',  ( -15.62157406900000112, 1485.483397133530161, 187.4151579208979967 ) ) ;
#77609 = VERTEX_POINT ( 'NONE', #76387 ) ;
#77610 = CARTESIAN_POINT ( 'NONE',  ( -105.7801839960000052, 1376.961008902830145, 301.4143074619590266 ) ) ;
#77611 = CARTESIAN_POINT ( 'NONE',  ( -106.1624399561229950, 1378.913060387289988, 302.5126857932060034 ) ) ;
#77612 = CARTESIAN_POINT ( 'NONE',  ( -5.007588685045000432, 1516.804776704140068, 203.3466091393569855 ) ) ;
#77613 = CARTESIAN_POINT ( 'NONE',  ( -26.37683023809999838, 1508.582706905729992, 201.5299876253779985 ) ) ;
#77614 = CARTESIAN_POINT ( 'NONE',  ( 3.687149994097108433E-15, 1518.913060387330006, 239.2297105040643714 ) ) ;
#77615 = CARTESIAN_POINT ( 'NONE',  ( -73.11479823269999656, 1385.127942832860072, 272.3424178700590232 ) ) ;
#77616 = CARTESIAN_POINT ( 'NONE',  ( -65.13305399213498958, 1384.705767306430062, 255.3553050933879831 ) ) ;
#77617 = CARTESIAN_POINT ( 'NONE',  ( -3.862688431370000064, 1407.379791273530145, 196.6061506809980131 ) ) ;
#77618 = CARTESIAN_POINT ( 'NONE',  ( -13.75903318429999977, 1409.893112517929922, 226.9379566688979821 ) ) ;
#77620 = ORIENTED_EDGE ( 'NONE', *, *, #35393, .F. ) ;
#77619 = CARTESIAN_POINT ( 'NONE',  ( -10.51245417620000033, 1447.347034548050033, 186.8435989827979711 ) ) ;
#77621 = CARTESIAN_POINT ( 'NONE',  ( -28.27963355899620268, 1508.150913702349953, 209.6131352202170035 ) ) ;
#77622 = CARTESIAN_POINT ( 'NONE',  ( 27.39969415949999743, 1508.129222249830036, 213.4901677084380083 ) ) ;
#77623 = AXIS2_PLACEMENT_3D ( 'NONE', #106381, #11241, #106921 ) ;
#77624 = CARTESIAN_POINT ( 'NONE',  ( 20.71370920478009836, 1497.619563572799962, 225.7436213016659963 ) ) ;
#77625 = CARTESIAN_POINT ( 'NONE',  ( -25.39307201429999949, 1435.891440879340053, 136.8929830188979793 ) ) ;
#77626 = CARTESIAN_POINT ( 'NONE',  ( 6.561995960394999550, 1517.083030555940013, 212.3803205491769859 ) ) ;
#77627 = CARTESIAN_POINT ( 'NONE',  ( -68.35177030640001306, 1379.747234628189972, 279.2299283338589930 ) ) ;
#77628 = AXIS2_PLACEMENT_3D ( 'NONE', #73783, #30656, #64841 ) ;
#77629 = CARTESIAN_POINT ( 'NONE',  ( -4.363122647530000009, 1432.413060387330006, 146.1721969590979882 ) ) ;
#77630 = CARTESIAN_POINT ( 'NONE',  ( -29.53441971554730472, 1525.651286436461760, 221.7311721888731881 ) ) ;
#77631 = CARTESIAN_POINT ( 'NONE',  ( -7.724874651314999952, 1517.139320148880188, 208.3815253650730028 ) ) ;
#77632 = VERTEX_POINT ( 'NONE', #15899 ) ;
#77633 = PLANE ( 'NONE',  #93817 ) ;
#77634 = CARTESIAN_POINT ( 'NONE',  ( -1.013019939329999897, 1412.845282977929855, 233.1607918147980172 ) ) ;
#77635 = CARTESIAN_POINT ( 'NONE',  ( -13.36456641330000039, 1385.300820372649923, 218.9430041755990146 ) ) ;
#77636 = ORIENTED_EDGE ( 'NONE', *, *, #39255, .F. ) ;
#77637 = CARTESIAN_POINT ( 'NONE',  ( -12.19044366360270004, 1385.304304086989987, 218.9500151190139832 ) ) ;
#77638 = CARTESIAN_POINT ( 'NONE',  ( -3.464428872329999631, 1429.082167021389978, 201.1863187793390182 ) ) ;
#77639 = CARTESIAN_POINT ( 'NONE',  ( 12.12303243055349888, 1434.792252859569999, 150.9027648073679870 ) ) ;
#77640 = B_SPLINE_SURFACE_WITH_KNOTS ( 'NONE', 5, 5, ( 
 ( #104838, #26030, #34459, #20811, #51258, #105393 ),
 ( #89136, #72357, #88057, #68635, #71837, #102736 ),
 ( #55009, #10786, #19145, #95884, #11885, #105955 ),
 ( #37631, #28125, #45514, #53352, #46610, #87497 ),
 ( #79105, #12422, #79655, #8687, #2960, #44957 ),
 ( #4051, #11342, #62317, #46057, #2412, #37077 ),
 ( #80742, #20264, #29233, #71280, #63422, #97539 ),
 ( #88602, #80190, #36529, #3507, #19720, #97001 ),
 ( #38177, #70725, #53922, #106488, #96442, #29774 ),
 ( #28686, #62891, #63962, #98077, #85391, #333 ),
 ( #42868, #61758, #77027, #65605, #99717, #109256 ),
 ( #22444, #100290, #12962, #40931, #56645, #90779 ),
 ( #107035, #72895, #56092, #47145, #81270, #107585 ),
 ( #30322, #15156, #81820, #5691, #99163, #5123 ),
 ( #4586, #66713, #23571, #64510, #14062, #108688 ),
 ( #23010, #73453, #21348, #48251, #98626, #57214 ),
 ( #14622, #108129, #38720, #21893, #65049, #82393 ),
 ( #57764, #91883, #90219, #32540, #13503, #39835 ),
 ( #6767, #47692, #31422, #39279, #82932, #91339 ),
 ( #30871, #73998, #48809, #6224, #40377, #89680 ),
 ( #74555, #31980, #49347, #66170, #83474, #75109 ) ),
 .UNSPECIFIED., .F., .F., .F.,
 ( 6, 3, 3, 3, 3, 3, 6 ),
 ( 6, 6 ),
 ( 41.21984250090000046, 43.22195389150000011, 43.93735686660000539, 45.64078810350000026, 47.34421934030000045, 50.75108181390000084, 60.28232112689999411 ),
 ( 0.000000000000000000, 1.469175964770000009 ),
 .UNSPECIFIED. ) ;
#77641 = CARTESIAN_POINT ( 'NONE',  ( 14.47037193060810090, 1459.302085855910036, 230.1578363246120205 ) ) ;
#77642 = DIRECTION ( 'NONE',  ( 0.5877852522924762457, 0.000000000000000000, 0.8090169943749451198 ) ) ;
#77643 = CARTESIAN_POINT ( 'NONE',  ( -2.113408855709999923, 1409.489867483530134, 186.5712290354979928 ) ) ;
#77644 = CARTESIAN_POINT ( 'NONE',  ( 1.599187595592249878, 1431.274712152729990, 218.4776966100959896 ) ) ;
#77645 = CARTESIAN_POINT ( 'NONE',  ( 4.230878294131939832, 1441.526452546219843, 164.7455269374289912 ) ) ;
#77647 = DIRECTION ( 'NONE',  ( -5.980589973904019347E-17, 1.000000000000000000, -1.736889445713099699E-16 ) ) ;
#77646 = CARTESIAN_POINT ( 'NONE',  ( 4.621267883935000320, 1516.830644417779922, 214.1213023606370029 ) ) ;
#77648 = CARTESIAN_POINT ( 'NONE',  ( 19.89462793710000099, 1508.347918119229917, 188.9544000135980184 ) ) ;
#77649 = CARTESIAN_POINT ( 'NONE',  ( -2.872208748294999836, 1517.145312756229941, 216.4596396827270155 ) ) ;
#77650 = VERTEX_POINT ( 'NONE', #50099 ) ;
#77651 = CARTESIAN_POINT ( 'NONE',  ( -11.29419939623580049, 1414.913057855109855, 197.0838916197120056 ) ) ;
#77652 = B_SPLINE_SURFACE_WITH_KNOTS ( 'NONE', 5, 5, ( 
 ( #30895, #11909, #4611, #46084, #105981, #72923, #98652, #21918, #56114, #47716, #45541, #81846 ),
 ( #37106, #71305, #62916, #97027, #23035, #33097, #24670, #14647, #57237, #84601, #40952, #14087 ),
 ( #16275, #108157, #24129, #50477, #108712, #67286, #23596, #66191, #101941, #57785, #83495, #48833 ),
 ( #48276, #75129, #56670, #65630, #15718, #82956, #82421, #99744, #39860, #5715, #32003, #74023 ),
 ( #58869, #15180, #100311, #74576, #66737, #92999, #91903, #31447, #49367, #84053, #6791, #6249 ),
 ( #109278, #32561, #100840, #101378, #7892, #91368, #42064, #58320, #92442, #40399, #76214, #49919 ),
 ( #7352, #41515, #90806, #75674, #109818, #110359, #33636, #67830, #52129, #51018, #10106, #51570 ),
 ( #8438, #43171, #69495, #36407, #77869, #95769, #42611, #26342, #1178, #73, #624, #34204 ),
 ( #68388, #1734, #35308, #43717, #27454, #25785, #103617, #86815, #60538, #85152, #78993, #87378 ),
 ( #52678, #94660, #103044, #17931, #35873, #104168, #34755, #76764, #86257, #102495, #44279, #26915 ),
 ( #9547, #2296, #61103, #78423, #53236, #59432, #59984, #94101, #68944, #95220, #18481, #16817 ),
 ( #70057, #61638, #10672, #19035, #44838, #77325, #17372, #70599, #25229, #93544, #85703, #8999 ) ),
 .UNSPECIFIED., .F., .F., .F.,
 ( 6, 3, 3, 6 ),
 ( 6, 3, 3, 6 ),
 ( 6.297091802710249375, 6.724583630079999708, 7.579194017749999901, 8.375326175313119847 ),
 ( -3.459696186616099858E-05, 0.3241439638239999588, 0.9724318914720000429, 1.438929940459749979 ),
 .UNSPECIFIED. ) ;
#77653 = DIRECTION ( 'NONE',  ( 0.000000000000000000, 0.7071067811865198172, -0.7071067811865753283 ) ) ;
#77654 = ORIENTED_EDGE ( 'NONE', *, *, #84206, .F. ) ;
#77655 = CARTESIAN_POINT ( 'NONE',  ( 2.648695236860000080, 1421.139663013429754, 184.4912115941980062 ) ) ;
#77656 = SURFACE_STYLE_USAGE ( .BOTH. , #17710 ) ;
#77657 = CARTESIAN_POINT ( 'NONE',  ( 0.000000000000000000, 1414.913060387329779, 209.1218459616979999 ) ) ;
#77658 = CARTESIAN_POINT ( 'NONE',  ( 3.039942922830000338, 1441.350710123290128, 218.5632362648489959 ) ) ;
#77659 = CARTESIAN_POINT ( 'NONE',  ( -29.85692059557563027, 1525.159177407156221, 196.1177194699280903 ) ) ;
#77660 = LINE ( 'NONE', #54142, #67512 ) ;
#77661 = EDGE_CURVE ( 'NONE', #365, #27217, #15578, .T. ) ;
#77662 = CARTESIAN_POINT ( 'NONE',  ( 18.41105348850000212, 1415.553739807329976, 210.1831042486080037 ) ) ;
#77663 = CARTESIAN_POINT ( 'NONE',  ( 13.88131303110161596, 1507.515608694632874, 232.8168500089977044 ) ) ;
#77664 = DIRECTION ( 'NONE',  ( 0.000000000000000000, 1.000000000000000000, 0.000000000000000000 ) ) ;
#77665 = CARTESIAN_POINT ( 'NONE',  ( -9277.894383878754525, -2339.359351152912041, 136.3368685514004710 ) ) ;
#77666 = CARTESIAN_POINT ( 'NONE',  ( 15.68557539840000103, 1410.853897593630109, 191.5168599455980143 ) ) ;
#77668 = CARTESIAN_POINT ( 'NONE',  ( -5.216843437400244810, 1391.913060387290216, 203.7324240256280916 ) ) ;
#77667 = CARTESIAN_POINT ( 'NONE',  ( -9.417893745694790653, 1420.662742013269963, 195.0156044709679861 ) ) ;
#77669 = FACE_OUTER_BOUND ( 'NONE', #64350, .T. ) ;
#77670 = ORIENTED_EDGE ( 'NONE', *, *, #29773, .F. ) ;
#77671 = CARTESIAN_POINT ( 'NONE',  ( 0.7038424768878800419, 1507.336011380059972, 186.3928043249479742 ) ) ;
#77672 = FACE_OUTER_BOUND ( 'NONE', #41180, .T. ) ;
#77673 = CARTESIAN_POINT ( 'NONE',  ( -27.77037812200000033, 1508.603156321929873, 210.5143981962980035 ) ) ;
#77674 = CARTESIAN_POINT ( 'NONE',  ( 3.744175762052851297, 1410.420533046074297, 185.9466301700599047 ) ) ;
#77675 = CARTESIAN_POINT ( 'NONE',  ( -3.569562092499118489, 1426.009408117103476, 185.9142566006702850 ) ) ;
#77676 = B_SPLINE_SURFACE_WITH_KNOTS ( 'NONE', 5, 5, ( 
 ( #41085, #30476, #5279, #39434, #108840, #22592 ),
 ( #107739, #22044, #75262, #31024, #83092, #23169 ),
 ( #91496, #31576, #65753, #107187, #65205, #99318 ),
 ( #73610, #109411, #39983, #64664, #99870, #98781 ),
 ( #6928, #32687, #56241, #56795, #90932, #74159 ),
 ( #57369, #108290, #81971, #32137, #14219, #66322 ),
 ( #48405, #5843, #14775, #15314, #82549, #23723 ),
 ( #48961, #6385, #40533, #74709, #90370, #100440 ),
 ( #13648, #57908, #92042, #49507, #47838, #83632 ),
 ( #2918, #30277, #4545, #54426, #37035, #47646 ),
 ( #106989, #38135, #5078, #80144, #38679, #39228 ),
 ( #11842, #81775, #64470, #63382, #94878, #89637 ),
 ( #88020, #98585, #88559, #21851, #71230, #46013 ),
 ( #98032, #56048, #90175, #72316, #11304, #55509 ),
 ( #72855, #3463, #29191, #73404, #106448, #13457 ),
 ( #107541, #63917, #30829, #71793, #29731, #19678 ),
 ( #53883, #105352, #105912, #12924, #37591, #21304 ),
 ( #45472, #47104, #12379, #79614, #89092, #80700 ),
 ( #28642, #97498, #62846, #96959, #20766, #20225 ),
 ( #54965, #46566, #81230, #4010, #108084, #57170 ),
 ( #92940, #83431, #49856, #91293, #39795, #92378 ),
 ( #40334, #31379, #14574, #108645, #31931, #16212 ),
 ( #74515, #67218, #15650, #24064, #91838, #50415 ),
 ( #66125, #82346, #109749, #83989, #22962, #5645 ),
 ( #75064, #75616, #6728, #84540, #48763, #7289 ),
 ( #41451, #49306, #7829, #90734, #82890, #40884 ),
 ( #22400, #101314, #100249, #109214, #57720, #42000 ) ),
 .UNSPECIFIED., .F., .F., .F.,
 ( 6, 3, 3, 3, 3, 3, 3, 3, 6 ),
 ( 6, 6 ),
 ( 50.96205257140000100, 60.48206970939999394, 63.97289610280000005, 65.71830929959999423, 66.59101589789999309, 67.46372249629999374, 67.82259044730000141, 68.73290467190000186, 70.00208684739999399 ),
 ( 0.000000000000000000, 1.468559632160000072 ),
 .UNSPECIFIED. ) ;
#77677 = CARTESIAN_POINT ( 'NONE',  ( 28.72841836130201543, 1526.333389947990099, 220.1290250959143862 ) ) ;
#77678 = CARTESIAN_POINT ( 'NONE',  ( -7.550503362009299835, 1510.480349264700180, 214.6730346447039892 ) ) ;
#77679 = CARTESIAN_POINT ( 'NONE',  ( -1.527346172629999943, 1467.905318097929921, 230.2847532987979946 ) ) ;
#77680 = CARTESIAN_POINT ( 'NONE',  ( 11.27337966920289958, 1433.557911275300057, 225.8166862488670006 ) ) ;
#77681 = CARTESIAN_POINT ( 'NONE',  ( -69.58852568934280214, 1383.785633056889992, 294.3347849598490029 ) ) ;
#77682 = CARTESIAN_POINT ( 'NONE',  ( -0.05914945545369999780, 1451.662743606630102, 154.0810024862979901 ) ) ;
#77683 = DIRECTION ( 'NONE',  ( 0.9942586961433764747, -0.000000000000000000, 0.1070030146457237041 ) ) ;
#77684 = CARTESIAN_POINT ( 'NONE',  ( -1.146118350564959920, 1516.628317670959859, 201.4103523897319974 ) ) ;
#77686 = ORIENTED_EDGE ( 'NONE', *, *, #14374, .F. ) ;
#77685 = CARTESIAN_POINT ( 'NONE',  ( 10.55224117611160217, 1452.267020623229882, 208.7256732491289881 ) ) ;
#77687 = DIRECTION ( 'NONE',  ( -0.8090169943749534465, -0.000000000000000000, -0.5877852522924650325 ) ) ;
#77688 = CARTESIAN_POINT ( 'NONE',  ( -82.19905968850000022, 1381.016078469080185, 303.3370635716590300 ) ) ;
#77689 = EDGE_CURVE ( 'NONE', #97374, #34577, #103201, .T. ) ;
#77690 = DIRECTION ( 'NONE',  ( -0.03206683765522939239, -0.9990097422274648586, 0.03084238734935479398 ) ) ;
#77691 = ORIENTED_EDGE ( 'NONE', *, *, #9807, .T. ) ;
#77692 = VERTEX_POINT ( 'NONE', #109448 ) ;
#77693 = CARTESIAN_POINT ( 'NONE',  ( 18.17240998359999793, 1509.561555716230032, 232.4487212659979889 ) ) ;
#77694 = B_SPLINE_CURVE_WITH_KNOTS ( 'NONE', 3,
 ( #82496, #48356, #4684, #90326, #73563, #5798, #106589, #65705, #89240, #107696, #80845, #56749, #30980, #99826, #47793, #12535, #38276, #90886, #38823, #29875 ),
 .UNSPECIFIED., .F., .F.,
 ( 4, 2, 2, 2, 1, 1, 1, 1, 2, 2, 2, 4 ),
 ( 0.000000000000000000, 0.2500000000009953149, 0.3750000000014879764, 0.4375000000017343904, 0.4687500000018708368, 0.4843750000019390045, 0.4921875000019731439, 0.4960937500019942381, 0.4980468750019917956, 0.5000000000019892976, 0.7500000000009947598, 1.000000000000000000 ),
 .UNSPECIFIED. ) ;
#77695 = CARTESIAN_POINT ( 'NONE',  ( 18.51436573157378618, 1511.187213306747708, 237.1421867457405881 ) ) ;
#77696 = CARTESIAN_POINT ( 'NONE',  ( 37.77063578043529901, 1438.437603869379700, 136.5939142087520111 ) ) ;
#77698 = CARTESIAN_POINT ( 'NONE',  ( 3.374205057650000136E-09, 1472.348783246430003, 259.9484461764980097 ) ) ;
#77697 = CARTESIAN_POINT ( 'NONE',  ( 10.92533434161652828, 1411.430006105364782, 269.3500472981405096 ) ) ;
#77699 = EDGE_CURVE ( 'NONE', #83466, #31153, #72776, .T. ) ;
#77700 = AXIS2_PLACEMENT_3D ( 'NONE', #3311, #104637, #103524 ) ;
#77701 = CARTESIAN_POINT ( 'NONE',  ( 9.377531398314840061, 1435.528482238679999, 208.6857172028140042 ) ) ;
#77702 = CARTESIAN_POINT ( 'NONE',  ( -107.8378136989999945, 1382.531835676999890, 297.9003899234589881 ) ) ;
#77703 = EDGE_CURVE ( 'NONE', #88887, #87290, #7100, .T. ) ;
#77704 = CARTESIAN_POINT ( 'NONE',  ( -12.79212758865954846, 1435.914429446145050, 150.8331423002523763 ) ) ;
#77705 = DIRECTION ( 'NONE',  ( -0.6736849260863839728, 0.000000000000000000, 0.7390186874254150995 ) ) ;
#77706 = CARTESIAN_POINT ( 'NONE',  ( 2.985074718659999959, 1409.521906423129849, 185.9264304420979954 ) ) ;
#77707 = CARTESIAN_POINT ( 'NONE',  ( 13.15671565689999944, 1428.802034784529951, 222.6511392629980151 ) ) ;
#77708 = CARTESIAN_POINT ( 'NONE',  ( -6.472929290989999807, 1440.851741214640015, 154.4738949224980047 ) ) ;
#77709 = CARTESIAN_POINT ( 'NONE',  ( 11.70596015200000117, 1435.783535252809997, 151.4055867023980113 ) ) ;
#77710 = CARTESIAN_POINT ( 'NONE',  ( -14.89996083112460035, 1421.394563697389913, 203.5315014676550049 ) ) ;
#77711 = AXIS2_PLACEMENT_3D ( 'NONE', #12824, #106339, #72217 ) ;
#77712 = EDGE_CURVE ( 'NONE', #104308, #74738, #28085, .T. ) ;
#77713 = CARTESIAN_POINT ( 'NONE',  ( -3.415166128929299827, 1451.477990676830132, 184.8447288809229860 ) ) ;
#77714 = CARTESIAN_POINT ( 'NONE',  ( 0.1613156720539999922, 1465.436708526229950, 236.3249312579980028 ) ) ;
#77715 = ORIENTED_EDGE ( 'NONE', *, *, #34447, .F. ) ;
#77716 = CARTESIAN_POINT ( 'NONE',  ( -4.565395397388770427, 1480.772680885790123, 231.0139838447539944 ) ) ;
#77717 = CARTESIAN_POINT ( 'NONE',  ( -41.93729219490000304, 1443.867285198199852, 269.6463924139980008 ) ) ;
#77718 = CARTESIAN_POINT ( 'NONE',  ( 11.88064286090000010, 1433.444786854229960, 151.0525681022980109 ) ) ;
#77719 = CARTESIAN_POINT ( 'NONE',  ( -18.75679884100000194, 1468.090218040589889, 202.1898047414589996 ) ) ;
#77720 = CARTESIAN_POINT ( 'NONE',  ( -110.0629901356764435, 1384.906028625631279, 296.9512903121827208 ) ) ;
#77721 = CARTESIAN_POINT ( 'NONE',  ( -20.22132488579999787, 1484.073267153790084, 213.0491124005889958 ) ) ;
#77722 = CARTESIAN_POINT ( 'NONE',  ( -1.920602012799999869, 1420.567466289690174, 193.8392733480989989 ) ) ;
#77723 = CARTESIAN_POINT ( 'NONE',  ( -5.100895039060000080, 1418.043138886930137, 233.8666107664980132 ) ) ;
#77724 = CARTESIAN_POINT ( 'NONE',  ( -103.9064370230000094, 1389.684541055990167, 306.7300248541590122 ) ) ;
#77725 = CARTESIAN_POINT ( 'NONE',  ( -7.921235470229449405, 1511.346448533420016, 214.8276827278679662 ) ) ;
#77726 = CARTESIAN_POINT ( 'NONE',  ( -6.569693564645711525, 1359.476008147596986, 208.3718459617010978 ) ) ;
#77727 = CARTESIAN_POINT ( 'NONE',  ( -45.77324011850739538, 1438.474511334749877, 266.4156763373180183 ) ) ;
#77728 = CARTESIAN_POINT ( 'NONE',  ( -2.694116389579999993, 1425.979849364829988, 185.2590652528979831 ) ) ;
#77729 = EDGE_LOOP ( 'NONE', ( #85418, #69909, #33935, #30781 ) ) ;
#77730 = CARTESIAN_POINT ( 'NONE',  ( -9.215151402819998339, 1422.993424535609847, 210.2744618676390189 ) ) ;
#77731 = ORIENTED_EDGE ( 'NONE', *, *, #93987, .T. ) ;
#77732 = CARTESIAN_POINT ( 'NONE',  ( -0.7402208985179988820, 1516.992029636990083, 209.8751463226419958 ) ) ;
#77733 = CARTESIAN_POINT ( 'NONE',  ( -2.478673243200000265, 1436.180421119320044, 157.6364458798979911 ) ) ;
#77734 = EDGE_CURVE ( 'NONE', #6510, #57665, #24463, .T. ) ;
#77735 = CARTESIAN_POINT ( 'NONE',  ( 7.537620219123420284, 1425.580748762979965, 212.1821311706370068 ) ) ;
#77736 = CARTESIAN_POINT ( 'NONE',  ( -26.33488014430039925, 1451.993447629259890, 134.9643013293120077 ) ) ;
#77737 = VERTEX_POINT ( 'NONE', #3028 ) ;
#77738 = CARTESIAN_POINT ( 'NONE',  ( -14.45358395259999895, 1470.808655613429892, 194.4307210385980227 ) ) ;
#77740 = CARTESIAN_POINT ( 'NONE',  ( 13.71645562369999993, 1434.810047171300084, 195.7796452459980117 ) ) ;
#77739 = CARTESIAN_POINT ( 'NONE',  ( -2.692976938448824242, 1524.059547553519678, 176.1570252011561593 ) ) ;
#77741 = B_SPLINE_CURVE_WITH_KNOTS ( 'NONE', 5,
 ( #100679, #83887, #104974, #89818, #71420, #55149 ),
 .UNSPECIFIED., .F., .F.,
 ( 6, 6 ),
 ( -74.30665799839999863, -17.67736075759999892 ),
 .UNSPECIFIED. ) ;
#77742 = EDGE_CURVE ( 'NONE', #76242, #74812, #1775, .T. ) ;
#77743 = B_SPLINE_CURVE_WITH_KNOTS ( 'NONE', 3,
 ( #82661, #40097, #49620, #83753, #41207, #77573, #52932, #9264, #85390, #35553, #78110, #86509, #69748, #27167, #1412, #77026, #60225, #17621, #69183, #332, #103289, #26596, #94343, #60793, #34458, #43970, #87066, #70307, #95471, #27713, #78670, #68634, #51825, #42867, #103867, #43423, #102735 ),
 .UNSPECIFIED., .F., .F.,
 ( 4, 3, 3, 3, 3, 3, 3, 3, 3, 3, 3, 3, 4 ),
 ( -12.69765133870000007, -12.53569613955949968, -11.85572679381469996, -11.13826790116400112, -10.38487189775069908, -9.582453197718731275, -8.635551395450828949, -7.667863743602329585, -6.997493992233709825, -6.072779624993440706, -5.268273530587539000, -4.554978577956211083, -3.881604426910000072 ),
 .UNSPECIFIED. ) ;
#77744 = CARTESIAN_POINT ( 'NONE',  ( 11.60004869885203860, 1424.140503711560086, 136.0100193273773357 ) ) ;
#77745 = CARTESIAN_POINT ( 'NONE',  ( -18.23402007437789862, 1508.542070153930126, 211.0639760601119974 ) ) ;
#77746 = CARTESIAN_POINT ( 'NONE',  ( -14.45750500688560081, 1416.828039245989885, 221.3916439204320170 ) ) ;
#77747 = FACE_OUTER_BOUND ( 'NONE', #74012, .T. ) ;
#77748 = ORIENTED_EDGE ( 'NONE', *, *, #11102, .T. ) ;
#77749 = CARTESIAN_POINT ( 'NONE',  ( -4.355561652949340612, 1408.080063563500062, 270.2891561468720170 ) ) ;
#77750 = CARTESIAN_POINT ( 'NONE',  ( -6.951517170504999399, 1517.194816588360027, 207.9969518818670053 ) ) ;
#77751 = CARTESIAN_POINT ( 'NONE',  ( 8.767012977189999390, 1418.317283281629898, 230.8509917594979868 ) ) ;
#77752 = CARTESIAN_POINT ( 'NONE',  ( 9.327571024978329461, 1434.415488575019936, 206.2241823136789947 ) ) ;
#77754 = EDGE_LOOP ( 'NONE', ( #19200, #17402, #64897, #69800 ) ) ;
#77753 = CARTESIAN_POINT ( 'NONE',  ( -4.297805644383835499, 1367.976344583816626, 207.6218459616988241 ) ) ;
#77755 = ORIENTED_EDGE ( 'NONE', *, *, #42986, .F. ) ;
#77756 = CARTESIAN_POINT ( 'NONE',  ( -1.906499846882070084E-08, 1517.051704408389924, 209.1218459511669892 ) ) ;
#77757 = CARTESIAN_POINT ( 'NONE',  ( -0.004805506605713849924, 1408.913228200830190, 186.0222358698079859 ) ) ;
#77758 = DIRECTION ( 'NONE',  ( 0.000000000000000000, 0.000000000000000000, 1.000000000000000000 ) ) ;
#77759 = CARTESIAN_POINT ( 'NONE',  ( -18.72591792251515486, 1409.005171047454724, 266.8216848252018281 ) ) ;
#77760 = CARTESIAN_POINT ( 'NONE',  ( -18.83966063982870054, 1437.724940806150016, 194.4009572081200190 ) ) ;
#77761 = CARTESIAN_POINT ( 'NONE',  ( -19.04810011320000029, 1425.814708983130231, 224.2238500513979886 ) ) ;
#77762 = CARTESIAN_POINT ( 'NONE',  ( 28.38017910033849844, 1468.283441186749997, 268.9888031847070238 ) ) ;
#77763 = CARTESIAN_POINT ( 'NONE',  ( -3.301631116843481983, 1466.760662549056860, 234.9475888533459056 ) ) ;
#77764 = CARTESIAN_POINT ( 'NONE',  ( -16.97240415505549294, 1421.991001403454675, 226.8235528602522777 ) ) ;
#77765 = CARTESIAN_POINT ( 'NONE',  ( 7.322709686834999232, 1516.596789218710001, 205.8608388005369818 ) ) ;
#77766 = ORIENTED_EDGE ( 'NONE', *, *, #76681, .F. ) ;
#77767 = CARTESIAN_POINT ( 'NONE',  ( 19.02527238669184584, 1457.194456449220070, 226.3937467632252378 ) ) ;
#77768 = CARTESIAN_POINT ( 'NONE',  ( 1.477399147100459942, 1480.042335471780007, 182.2939015677119983 ) ) ;
#77769 = CARTESIAN_POINT ( 'NONE',  ( 23.55027989260000254, 1410.975381342730088, 207.7696266105379834 ) ) ;
#77770 = ORIENTED_EDGE ( 'NONE', *, *, #72677, .F. ) ;
#77771 = CARTESIAN_POINT ( 'NONE',  ( 4.490619199204468615, 1508.909942010298437, 212.6094383991669758 ) ) ;
#77772 = CARTESIAN_POINT ( 'NONE',  ( 25.74980778770000001, 1451.774094166629993, 136.0745756758980178 ) ) ;
#77773 = CARTESIAN_POINT ( 'NONE',  ( -4.692464771771249765, 1508.551704408389924, 212.7861425959310111 ) ) ;
#77774 = CARTESIAN_POINT ( 'NONE',  ( -3.078458344860000029, 1389.630721955109948, 203.0177346566789822 ) ) ;
#77775 = CARTESIAN_POINT ( 'NONE',  ( 7.443246446249998982, 1423.092341332720025, 195.6161848952989999 ) ) ;
#77777 = B_SPLINE_SURFACE_WITH_KNOTS ( 'NONE', 5, 1, ( 
 ( #103000, #86770 ),
 ( #10626, #52082 ),
 ( #2797, #37475 ),
 ( #2253, #44793 ),
 ( #10060, #28524 ),
 ( #44233, #78945 ),
 ( #36365, #36917 ),
 ( #45894, #9506 ),
 ( #80030, #26297 ),
 ( #94607, #17883 ),
 ( #86213, #88971 ),
 ( #81657, #54846 ),
 ( #82222, #107974 ),
 ( #20644, #72740 ),
 ( #80583, #5524 ),
 ( #12815, #72207 ),
 ( #106866, #39680 ),
 ( #73847, #64349 ),
 ( #106330, #4963 ),
 ( #46995, #98470 ),
 ( #13900, #47536 ),
 ( #21740, #55942 ),
 ( #63798, #4435 ),
 ( #90063, #13344 ),
 ( #39107, #97912 ),
 ( #22288, #73284 ),
 ( #30157, #29613 ),
 ( #38561, #21184 ),
 ( #107421, #30718 ),
 ( #56489, #55393 ),
 ( #64903, #90620 ),
 ( #71679, #81118 ),
 ( #3899, #48087 ),
 ( #63263, #99011 ),
 ( #12261, #105798 ),
 ( #89523, #29079 ),
 ( #97373, #46451 ),
 ( #38028, #52997 ),
 ( #52446, #79295 ),
 ( #97181, #70926 ),
 ( #86574, #103928 ),
 ( #12074, #36731 ),
 ( #37290, #28886 ),
 ( #70366, #78735 ),
 ( #105042, #105603 ),
 ( #87701, #9867 ),
 ( #54115, #72025 ),
 ( #28331, #61965 ),
 ( #1483, #106141 ),
 ( #2050, #62523 ),
 ( #35615, #71482 ) ),
 .UNSPECIFIED., .F., .F., .F.,
 ( 6, 3, 3, 3, 3, 3, 3, 3, 3, 3, 3, 3, 3, 3, 3, 3, 6 ),
 ( 2, 2 ),
 ( 0.000000000000000000, 28.69702819429999963, 61.04778752440000034, 93.62768910810000023, 123.7336603250000024, 156.1762685979999787, 187.3272846180000215, 220.4669312460000015, 237.3878297990000021, 254.2938300590000154, 289.2398204710000300, 325.3030936050000150, 360.8626869010000178, 395.8828220460000011, 432.6128460950000090, 468.8934854820000169, 502.1482307969999965 ),
 ( -0.0001548847310923010001, 2.001786307029170153 ),
 .UNSPECIFIED. ) ;
#77776 = CARTESIAN_POINT ( 'NONE',  ( 17.05796332999999976, 1409.508737592730085, 194.6785584388979942 ) ) ;
#77778 = CARTESIAN_POINT ( 'NONE',  ( 17.22592482065188335, 1444.324653571828321, 162.9227486220069352 ) ) ;
#77779 = CIRCLE ( 'NONE', #52770, 2.000000000000001776 ) ;
#77780 = CARTESIAN_POINT ( 'NONE',  ( 3.771179646140724540, 1439.700054869645101, 184.6351339312261643 ) ) ;
#77782 = CARTESIAN_POINT ( 'NONE',  ( -19.25680457745775698, 1425.292773199313388, 223.7995632996566826 ) ) ;
#77781 = CARTESIAN_POINT ( 'NONE',  ( 1.319771658879999920, 1416.088550827329982, 232.9278251303979914 ) ) ;
#77783 = CARTESIAN_POINT ( 'NONE',  ( 1.304065981556200127, 1452.805067748419788, 183.4358032751680128 ) ) ;
#77784 = CARTESIAN_POINT ( 'NONE',  ( -3.272667022753710242, 1517.151704408390060, 189.0363362235078171 ) ) ;
#77785 = CARTESIAN_POINT ( 'NONE',  ( -8.931786718119999691, 1380.912887613739940, 217.7591081930590065 ) ) ;
#77786 = CIRCLE ( 'NONE', #108145, 2.000000000000003553 ) ;
#77787 = CARTESIAN_POINT ( 'NONE',  ( 2.596261494520144986, 1525.907212628473872, 240.7735774411710850 ) ) ;
#77788 = ORIENTED_EDGE ( 'NONE', *, *, #48546, .F. ) ;
#77789 = CARTESIAN_POINT ( 'NONE',  ( -1.909775791882407869, 1526.107880201381477, 177.3667237755819031 ) ) ;
#77790 = CARTESIAN_POINT ( 'NONE',  ( 11.77504716261359974, 1432.336839668820176, 150.6178349985629836 ) ) ;
#77791 = CARTESIAN_POINT ( 'NONE',  ( -0.3329445438763140031, 1408.995598260099996, 232.2005901765320175 ) ) ;
#77792 = CARTESIAN_POINT ( 'NONE',  ( -10.50120379640000046, 1388.631521996640004, 201.9833518851789904 ) ) ;
#77793 = CARTESIAN_POINT ( 'NONE',  ( 1.381433737519002669, 1421.416365592073362, 193.7767222259685411 ) ) ;
#77794 = CARTESIAN_POINT ( 'NONE',  ( -8.301987938657498844, 1512.913060387330006, 185.0111222839169898 ) ) ;
#77795 = B_SPLINE_CURVE_WITH_KNOTS ( 'NONE', 3,
 ( #5079, #16080, #39796, #85492, #108085, #76011, #31380, #84945 ),
 .UNSPECIFIED., .F., .F.,
 ( 4, 2, 2, 4 ),
 ( 2.964296775167216948E-17, 0.001073044933456093883, 0.001609567400184125970, 0.002146089866912157841 ),
 .UNSPECIFIED. ) ;
#77796 = CARTESIAN_POINT ( 'NONE',  ( -2.984513020910000147, 1453.913060387330006, 209.1218459616979999 ) ) ;
#77797 = CARTESIAN_POINT ( 'NONE',  ( 43.12279225419995043, 1452.630096070929540, 266.2619628294978043 ) ) ;
#77798 = CARTESIAN_POINT ( 'NONE',  ( 11.91185892230000043, 1433.366769854990025, 149.9329001653979674 ) ) ;
#77799 = CARTESIAN_POINT ( 'NONE',  ( 8.518323191219998591, 1460.717990419130047, 243.9198229383979992 ) ) ;
#77800 = B_SPLINE_SURFACE_WITH_KNOTS ( 'NONE', 5, 5, ( 
 ( #49685, #107913, #23890, #65391, #66502, #39041 ),
 ( #13284, #14940, #41269, #65940, #74344, #40714 ),
 ( #56427, #14391, #99496, #92216, #101149, #81598 ),
 ( #75443, #98955, #22778, #47475, #73222, #67041 ),
 ( #56984, #107365, #90557, #48585, #57542, #13837 ),
 ( #49135, #109579, #82719, #6009, #30661, #58083 ),
 ( #91665, #64846, #31755, #83268, #32319, #6564 ),
 ( #74886, #100607, #103926, #85449, #68154, #86572 ),
 ( #27225, #51313, #42930, #110122, #9864, #92762 ) ),
 .UNSPECIFIED., .F., .F., .F.,
 ( 6, 3, 6 ),
 ( 6, 6 ),
 ( -0.0002510112223089640293, 10.92808819610000093, 17.46068133292229874 ),
 ( -0.0002510112223103900262, 2.000000000000000000 ),
 .UNSPECIFIED. ) ;
#77801 = CARTESIAN_POINT ( 'NONE',  ( -10.16625295280419827, 1461.954337890570059, 208.9248117568549787 ) ) ;
#77802 = CARTESIAN_POINT ( 'NONE',  ( 2.502367656480000147, 1427.111872751849887, 188.6975817531990174 ) ) ;
#77803 = CARTESIAN_POINT ( 'NONE',  ( -1.842962231260000028, 1515.551704408389924, 212.9514660752490158 ) ) ;
#77804 = CARTESIAN_POINT ( 'NONE',  ( -113.4000000000000057, 1389.413060387289988, 304.2218459572590064 ) ) ;
#77805 = CARTESIAN_POINT ( 'NONE',  ( -13.67685946489999971, 1486.238555760329973, 185.2440325359980022 ) ) ;
#77806 = CARTESIAN_POINT ( 'NONE',  ( 9.119196661296259165, 1398.183650043934222, 199.8491675525386313 ) ) ;
#77807 = CARTESIAN_POINT ( 'NONE',  ( -21.91919261220000337, 1509.808421474629995, 231.8378097518979928 ) ) ;
#77808 = CARTESIAN_POINT ( 'NONE',  ( 20.81017606039999990, 1469.236365764530092, 223.5860970572980193 ) ) ;
#77809 = CARTESIAN_POINT ( 'NONE',  ( 4.054153981253102224, 1446.253642626345709, 170.5365981473220813 ) ) ;
#77810 = DIRECTION ( 'NONE',  ( -1.836970198721029688E-16, -1.000000000000000000, 0.000000000000000000 ) ) ;
#77811 = CARTESIAN_POINT ( 'NONE',  ( -11.51055856485790052, 1383.861746106490045, 218.7228895138829898 ) ) ;
#77812 = AXIS2_PLACEMENT_3D ( 'NONE', #30385, #90283, #81330 ) ;
#77813 = CARTESIAN_POINT ( 'NONE',  ( 0.9103411385305409942, 1462.760009460389938, 230.5111369873399951 ) ) ;
#77814 = CARTESIAN_POINT ( 'NONE',  ( 0.7572979362240020995, 1516.829948096479939, 212.5714934102470011 ) ) ;
#77815 = CARTESIAN_POINT ( 'NONE',  ( -15.23895844625580054, 1421.038471381979889, 204.9739905745400108 ) ) ;
#77816 = CARTESIAN_POINT ( 'NONE',  ( 0.1616823930634609940, 1485.255944980259983, 181.8685822356719939 ) ) ;
#77818 = ORIENTED_EDGE ( 'NONE', *, *, #22334, .F. ) ;
#77817 = CARTESIAN_POINT ( 'NONE',  ( 3.368607595359999873, 1442.498527986489989, 217.3357187138090296 ) ) ;
#77819 = CARTESIAN_POINT ( 'NONE',  ( -1.341950169539999793, 1416.837177091229705, 228.0806925298979877 ) ) ;
#77820 = CARTESIAN_POINT ( 'NONE',  ( -8.243035228590668950, 1386.658394140979681, 199.7856276493823486 ) ) ;
#77821 = EDGE_CURVE ( 'NONE', #16145, #59173, #20948, .T. ) ;
#77822 = CARTESIAN_POINT ( 'NONE',  ( -4.647810563630000225, 1474.919191006789788, 199.5028939205090239 ) ) ;
#77824 = VERTEX_POINT ( 'NONE', #70794 ) ;
#77823 = CARTESIAN_POINT ( 'NONE',  ( -33.91369120143989591, 1451.728768194249824, 134.0999999980979851 ) ) ;
#77825 = CARTESIAN_POINT ( 'NONE',  ( -5.842433632679150612, 1508.551704408389924, 219.4797894617979921 ) ) ;
#77826 = VERTEX_POINT ( 'NONE', #62381 ) ;
#77827 = AXIS2_PLACEMENT_3D ( 'NONE', #101375, #67826, #42608 ) ;
#77828 = CARTESIAN_POINT ( 'NONE',  ( -12.97809200588160117, 1390.329422715150031, 212.5574397272170017 ) ) ;
#77829 = CARTESIAN_POINT ( 'NONE',  ( -15.13954165719999878, 1415.426091369430196, 218.9613120750979931 ) ) ;
#77830 = CARTESIAN_POINT ( 'NONE',  ( 2.516232163441119773, 1464.674062513380022, 202.5523638050540001 ) ) ;
#77831 = CARTESIAN_POINT ( 'NONE',  ( -107.6978622682329814, 1380.365081504608042, 309.6627544237097709 ) ) ;
#77832 = DIRECTION ( 'NONE',  ( -0.07222731439955003274, -0.9674608870543032202, 0.2424925711743135259 ) ) ;
#77833 = CARTESIAN_POINT ( 'NONE',  ( 1.875671004969999833, 1456.514200624189925, 219.5762891113990065 ) ) ;
#77834 = CARTESIAN_POINT ( 'NONE',  ( -17.17241001986523941, 1511.187213306747708, 179.6185504016045797 ) ) ;
#77835 = CARTESIAN_POINT ( 'NONE',  ( -67.25262833492540437, 1385.098311572419789, 260.0348044464020631 ) ) ;
#77836 = CARTESIAN_POINT ( 'NONE',  ( -17.67020261369999901, 1412.966317095329941, 192.9698263009980224 ) ) ;
#77837 = CYLINDRICAL_SURFACE ( 'NONE', #78796, 2.000000000000001776 ) ;
#77838 = ORIENTED_EDGE ( 'NONE', *, *, #110454, .T. ) ;
#77839 = DIRECTION ( 'NONE',  ( 0.000000000000000000, 1.000000000000000000, 0.000000000000000000 ) ) ;
#77840 = EDGE_CURVE ( 'NONE', #6139, #32742, #56492, .T. ) ;
#77842 = ORIENTED_EDGE ( 'NONE', *, *, #20828, .T. ) ;
#77841 = CARTESIAN_POINT ( 'NONE',  ( -1.420557929969340050, 1438.189677974030019, 227.6394655603620265 ) ) ;
#77843 = DIRECTION ( 'NONE',  ( 0.000000000000000000, 1.000000000000000000, 0.000000000000000000 ) ) ;
#77844 = ORIENTED_EDGE ( 'NONE', *, *, #105503, .F. ) ;
#77845 =( BOUNDED_SURFACE ( )  B_SPLINE_SURFACE ( 3, 2, ( 
 ( #12121, #21605, #64204 ),
 ( #38962, #97776, #30014 ),
 ( #4292, #29468, #30577 ),
 ( #89927, #73140, #63661 ),
 ( #72595, #46313, #62575 ),
 ( #21051, #107283, #55254 ),
 ( #80442, #98327, #19402 ),
 ( #11579, #89386, #12677 ),
 ( #19964, #38419, #3207 ),
 ( #45756, #45198, #96127 ),
 ( #46857, #106723, #79893 ),
 ( #4816, #105086, #63126 ),
 ( #55810, #28936, #2650 ),
 ( #47392, #54159, #36778 ) ),
 .UNSPECIFIED., .F., .F., .F. ) 
 B_SPLINE_SURFACE_WITH_KNOTS ( ( 4, 2, 2, 2, 2, 2, 4 ),
 ( 3, 3 ),
 ( 0.000000000000000000, 0.0009440840677143950543, 0.001416126101571592473, 0.001888168135428790109, 0.002360210169285987744, 0.002832252203143184946, 0.003776336270857580217 ),
 ( 0.000000000000000000, 1.000000000000000000 ),
 .UNSPECIFIED. ) 
 GEOMETRIC_REPRESENTATION_ITEM ( )  RATIONAL_B_SPLINE_SURFACE ( (
 ( 1.000000000000000000, 0.8070209408750095292, 1.000000000000000000),
 ( 1.000000000000000000, 0.8215603905278417995, 1.000000000000000000),
 ( 1.000000000000000000, 0.8340988699068413448, 1.000000000000000000),
 ( 1.000000000000000000, 0.8516751610454839083, 1.000000000000000000),
 ( 1.000000000000000000, 0.8573697395150315925, 1.000000000000000000),
 ( 1.000000000000000000, 0.8683586635666024067, 1.000000000000000000),
 ( 1.000000000000000000, 0.8736518481709272255, 1.000000000000000000),
 ( 1.000000000000000000, 0.8840377753029367014, 1.000000000000000000),
 ( 1.000000000000000000, 0.8891294171307203564, 1.000000000000000000),
 ( 1.000000000000000000, 0.8992456600573149883, 1.000000000000000000),
 ( 1.000000000000000000, 0.9042785869252324416, 1.000000000000000000),
 ( 1.000000000000000000, 0.9189749222839583842, 1.000000000000000000),
 ( 1.000000000000000000, 0.9283978182347645269, 1.000000000000000000),
 ( 1.000000000000000000, 0.9376006582765933350, 1.000000000000000000) ) ) 
 REPRESENTATION_ITEM ( '' )  SURFACE ( )  );
#77846 = FACE_OUTER_BOUND ( 'NONE', #37673, .T. ) ;
#77847 = CARTESIAN_POINT ( 'NONE',  ( -7.173827098684180115, 1361.757975858857890, 210.6218459616987957 ) ) ;
#77848 = CARTESIAN_POINT ( 'NONE',  ( -6.797648946129999814, 1495.115797578489946, 200.0173552654389937 ) ) ;
#77849 = ADVANCED_FACE ( 'NONE', ( #19212 ), #3576, .T. ) ;
#77850 = CARTESIAN_POINT ( 'NONE',  ( 35.92105933033366938, 1456.729054770310313, 269.5445013229119127 ) ) ;
#77851 = CARTESIAN_POINT ( 'NONE',  ( 21.13431379670319998, 1409.651086887829933, 206.4149708788170301 ) ) ;
#77852 = CARTESIAN_POINT ( 'NONE',  ( 6.240887162079999939, 1397.787773554729938, 220.5258548213979850 ) ) ;
#77853 = DIRECTION ( 'NONE',  ( -1.000000000000000000, 0.000000000000000000, 0.000000000000000000 ) ) ;
#77854 = CARTESIAN_POINT ( 'NONE',  ( -8.437512126890000630, 1512.337580101790081, 211.2823750686789879 ) ) ;
#77855 = CARTESIAN_POINT ( 'NONE',  ( -10.21846136005779115, 1368.315982671009579, 208.3718459617010978 ) ) ;
#77856 = CARTESIAN_POINT ( 'NONE',  ( -29.52630218505378323, 1525.661276915132476, 221.7199201227869310 ) ) ;
#77857 = CARTESIAN_POINT ( 'NONE',  ( -1.717084749545000122, 1516.819260244609950, 206.6456753351970121 ) ) ;
#77858 = CARTESIAN_POINT ( 'NONE',  ( -2.038646110889675178, 1525.960063244516959, 177.0579350083066004 ) ) ;
#77859 = DIRECTION ( 'NONE',  ( 0.000000000000000000, -1.000000000000000000, 0.000000000000000000 ) ) ;
#77860 = CARTESIAN_POINT ( 'NONE',  ( 31.97288361449999883, 1465.739487317430076, 269.9246165631980148 ) ) ;
#77862 = ORIENTED_EDGE ( 'NONE', *, *, #82871, .T. ) ;
#77861 = CARTESIAN_POINT ( 'NONE',  ( 0.5197867694969990904, 1494.713114127890094, 220.2910688317990093 ) ) ;
#77863 = LINE ( 'NONE', #43165, #27703 ) ;
#77864 = VERTEX_POINT ( 'NONE', #86992 ) ;
#77865 = CARTESIAN_POINT ( 'NONE',  ( 26.19682441240000159, 1416.543454811029733, 259.6167016350979679 ) ) ;
#77866 = CARTESIAN_POINT ( 'NONE',  ( -23.83044711870000043, 1430.353408626829832, 204.6119512178680111 ) ) ;
#77869 = CARTESIAN_POINT ( 'NONE',  ( 16.39238061357189835, 1409.586354316659936, 192.5911623901700125 ) ) ;
#77868 = VECTOR ( 'NONE', #1552, 1000.000000000000000 ) ;
#77867 = CARTESIAN_POINT ( 'NONE',  ( -11.61158519821730017, 1426.364169946740049, 135.2602023053949836 ) ) ;
#77870 = CARTESIAN_POINT ( 'NONE',  ( 5.787476994515000861, 1517.070197312179971, 211.9915394291670054 ) ) ;
#77871 = EDGE_CURVE ( 'NONE', #70982, #73683, #47767, .T. ) ;
#77872 = CARTESIAN_POINT ( 'NONE',  ( -9.196349486490202452, 1517.151704408390060, 203.7768694350468195 ) ) ;
#77873 = CARTESIAN_POINT ( 'NONE',  ( -22.64731540989999914, 1507.637957906029897, 208.5229870085950097 ) ) ;
#77874 = CARTESIAN_POINT ( 'NONE',  ( -40.44435334479999966, 1427.769454619329963, 264.0385764254980359 ) ) ;
#77875 = CARTESIAN_POINT ( 'NONE',  ( 18.36180303385479817, 1509.570204029540037, 232.3072875949450236 ) ) ;
#77876 = CARTESIAN_POINT ( 'NONE',  ( 29.40921901591849874, 1509.877385647309893, 209.6267707321559897 ) ) ;
#77877 = CARTESIAN_POINT ( 'NONE',  ( -5.166418613160000284, 1391.906183525989718, 214.5657459001290022 ) ) ;
#77878 = CARTESIAN_POINT ( 'NONE',  ( -34.71462694457399323, 1437.089205478310078, 136.5423016297559968 ) ) ;
#77879 = ORIENTED_EDGE ( 'NONE', *, *, #94808, .T. ) ;
#77880 = CARTESIAN_POINT ( 'NONE',  ( 12.47743726298899958, 1397.381078991009872, 213.9104067551370179 ) ) ;
#77881 = CARTESIAN_POINT ( 'NONE',  ( 10.32735688926459794, 1460.628046964450050, 207.2416929514699859 ) ) ;
#77882 = CARTESIAN_POINT ( 'NONE',  ( -16.78297372800000176, 1460.265260285829982, 228.3353414857980113 ) ) ;
#77883 = ORIENTED_EDGE ( 'NONE', *, *, #3684, .F. ) ;
#77884 = ORIENTED_EDGE ( 'NONE', *, *, #100590, .T. ) ;
#77885 = CARTESIAN_POINT ( 'NONE',  ( -29.24222810794026728, 1509.934246511754054, 211.7448759012906976 ) ) ;
#77886 = CARTESIAN_POINT ( 'NONE',  ( 9.651067907589998995, 1425.440654964710120, 195.4941613134990064 ) ) ;
#77887 = ORIENTED_EDGE ( 'NONE', *, *, #16854, .F. ) ;
#77888 = CYLINDRICAL_SURFACE ( 'NONE', #43868, 1.999999999999999556 ) ;
#77889 = CARTESIAN_POINT ( 'NONE',  ( -12.45534669159577135, 1417.321673587058740, 200.0573570912646915 ) ) ;
#77890 = CARTESIAN_POINT ( 'NONE',  ( 22.28696231330000188, 1506.798305107829947, 209.3970118511340104 ) ) ;
#77891 = CARTESIAN_POINT ( 'NONE',  ( -12.89099770320000005, 1461.186125398530066, 230.5721238860979838 ) ) ;
#77892 = CARTESIAN_POINT ( 'NONE',  ( 7.096077594474770933, 1508.610125823030103, 202.4734937754249984 ) ) ;
#77893 = VECTOR ( 'NONE', #24893, 1000.000000000000000 ) ;
#77894 = CARTESIAN_POINT ( 'NONE',  ( 9.209674294604401013, 1450.304425456110039, 208.7276454369840053 ) ) ;
#77895 = CARTESIAN_POINT ( 'NONE',  ( 4.082704913390428736, 1515.071394844000451, 212.7082235457387185 ) ) ;
#77896 = CARTESIAN_POINT ( 'NONE',  ( -90.92465973820169722, 1384.842308400400043, 293.1021286165930064 ) ) ;
#77897 = EDGE_LOOP ( 'NONE', ( #3310, #23028, #23414, #95482 ) ) ;
#77898 = CARTESIAN_POINT ( 'NONE',  ( -0.7543882209519990889, 1516.727502608469877, 202.5709757879969857 ) ) ;
#77899 = CARTESIAN_POINT ( 'NONE',  ( 5.006259848694999626, 1516.939723362869927, 209.1089481433290018 ) ) ;
#77900 = ORIENTED_EDGE ( 'NONE', *, *, #60243, .F. ) ;
#77901 = CARTESIAN_POINT ( 'NONE',  ( 11.74890926396520108, 1426.742300306969810, 145.0013950776020124 ) ) ;
#77902 = CARTESIAN_POINT ( 'NONE',  ( 12.83373743668885503, 1444.966504083088466, 186.6095280254539830 ) ) ;
#77903 = VERTEX_POINT ( 'NONE', #27102 ) ;
#77904 = CARTESIAN_POINT ( 'NONE',  ( 9.048691962705447622, 1423.897446184702403, 139.1407012399385223 ) ) ;
#77905 = CARTESIAN_POINT ( 'NONE',  ( -3.700607310100329617, 1508.505817376630148, 220.3043853933179719 ) ) ;
#77906 = CARTESIAN_POINT ( 'NONE',  ( 7.315253172540000293, 1509.168514657129890, 237.2865368194979965 ) ) ;
#77907 = AXIS2_PLACEMENT_3D ( 'NONE', #103642, #19057, #96902 ) ;
#77908 = CARTESIAN_POINT ( 'NONE',  ( -11.03352987879990010, 1462.446752253709974, 208.7216463217210105 ) ) ;
#77909 = CARTESIAN_POINT ( 'NONE',  ( -4.954458045509999131, 1424.150364743330101, 185.8728153432979866 ) ) ;
#77910 = CARTESIAN_POINT ( 'NONE',  ( 3.530738010049999875, 1408.338100458330018, 270.3906828179979698 ) ) ;
#77911 = CARTESIAN_POINT ( 'NONE',  ( -3.500000000000000000, 1407.163060387330006, 146.1721969590979882 ) ) ;
#77912 = CARTESIAN_POINT ( 'NONE',  ( -110.0707497544257194, 1384.648932846942671, 296.9551064835548004 ) ) ;
#77913 = CARTESIAN_POINT ( 'NONE',  ( 10.44002158900000055, 1492.834359288489850, 214.0636917351490069 ) ) ;
#77914 = CARTESIAN_POINT ( 'NONE',  ( -30.53571690079999712, 1379.628638755449856, 214.1212922363289977 ) ) ;
#77916 = CARTESIAN_POINT ( 'NONE',  ( 14.45783194710000075, 1416.839692140529905, 196.8516150077980171 ) ) ;
#77915 = CARTESIAN_POINT ( 'NONE',  ( -21.25276517840000068, 1505.388537598189941, 209.6001788282910070 ) ) ;
#77917 = CARTESIAN_POINT ( 'NONE',  ( -4.573812764092838101, 1423.750333358086891, 184.3978805773018905 ) ) ;
#77918 = CARTESIAN_POINT ( 'NONE',  ( 17.81052644217599834, 1417.511519687270038, 225.0007343307930228 ) ) ;
#77919 = CARTESIAN_POINT ( 'NONE',  ( -9.052208719341413357, 1506.643733544970701, 188.8170897969911266 ) ) ;
#77920 = ORIENTED_EDGE ( 'NONE', *, *, #85881, .T. ) ;
#77921 = CARTESIAN_POINT ( 'NONE',  ( 29.61076270571687630, 1526.107880201381477, 197.4926688362025402 ) ) ;
#77922 = CARTESIAN_POINT ( 'NONE',  ( -18.19590854888186726, 1522.382868172863937, 180.0410247165186206 ) ) ;
#77923 = CARTESIAN_POINT ( 'NONE',  ( -2.941051375418705760, 1485.222273148426211, 183.0255250225658870 ) ) ;
#77924 = CARTESIAN_POINT ( 'NONE',  ( -14.52535627939999863, 1415.865102022439942, 214.1001117942190035 ) ) ;
#77926 = ORIENTED_EDGE ( 'NONE', *, *, #24163, .F. ) ;
#77925 = CARTESIAN_POINT ( 'NONE',  ( -0.3731951686936089696, 1515.150224411150020, 204.7946342890899984 ) ) ;
#77927 = CARTESIAN_POINT ( 'NONE',  ( 17.10420012035890025, 1414.913526845469960, 210.6212183496899968 ) ) ;
#77928 = DIRECTION ( 'NONE',  ( 0.9455185755993178454, 0.000000000000000000, -0.3255681544571537578 ) ) ;
#77929 = CARTESIAN_POINT ( 'NONE',  ( -11.49189579029999919, 1426.655527037130241, 148.3077481762979914 ) ) ;
#77930 = CARTESIAN_POINT ( 'NONE',  ( 20.13562578519999846, 1473.995721266390092, 210.1107519762580012 ) ) ;
#77931 = CARTESIAN_POINT ( 'NONE',  ( 3.263471513352690145, 1446.335603773660068, 199.5325906368949802 ) ) ;
#77932 = CARTESIAN_POINT ( 'NONE',  ( -4.992640509747255706, 1391.632012793324975, 203.6213856293937283 ) ) ;
#77933 = CARTESIAN_POINT ( 'NONE',  ( 13.18752275098719906, 1428.876431498459851, 222.4037147343619836 ) ) ;
#77934 = CARTESIAN_POINT ( 'NONE',  ( -16.61115978156500006, 1513.007288725350008, 221.0814365924669858 ) ) ;
#77935 = CARTESIAN_POINT ( 'NONE',  ( 9.265269351469999748, 1412.734572620129939, 230.2246370649980065 ) ) ;
#77936 = CARTESIAN_POINT ( 'NONE',  ( -11.86476110198860034, 1482.098049815899913, 208.3139255992990115 ) ) ;
#77937 = CARTESIAN_POINT ( 'NONE',  ( -15.83861837100000081, 1459.345690884129908, 229.6260692152980027 ) ) ;
#77938 = CARTESIAN_POINT ( 'NONE',  ( -5.012938901904998801, 1517.051603658920158, 206.6410320471169939 ) ) ;
#77939 = CARTESIAN_POINT ( 'NONE',  ( 31.52953872790000034, 1415.569331350129914, 268.9168057298979306 ) ) ;
#77940 = CARTESIAN_POINT ( 'NONE',  ( 1.963370004590500262, 1464.924280329780913, 237.5709148626887952 ) ) ;
#77941 = CARTESIAN_POINT ( 'NONE',  ( 20.81072686770000146, 1430.297633082429911, 197.0877802440980133 ) ) ;
#77942 = CARTESIAN_POINT ( 'NONE',  ( -23.34239156850000185, 1434.464133788829940, 214.4674836295579894 ) ) ;
#77943 = CIRCLE ( 'NONE', #27908, 2.000000000000003553 ) ;
#77944 = CARTESIAN_POINT ( 'NONE',  ( -10.10004869885203682, 1425.894669202444675, 137.5118601406020673 ) ) ;
#77945 = AXIS2_PLACEMENT_3D ( 'NONE', #104529, #80985, #72071 ) ;
#77946 = CARTESIAN_POINT ( 'NONE',  ( 8.759919950853198856, 1423.587268813439778, 144.1551655176990039 ) ) ;
#77947 = CARTESIAN_POINT ( 'NONE',  ( 5.699301886687036856, 1480.231621539390062, 228.7443292491632860 ) ) ;
#77948 = CARTESIAN_POINT ( 'NONE',  ( -6.688849035430000534, 1408.965348140629885, 196.7627783224980078 ) ) ;
#77949 = CARTESIAN_POINT ( 'NONE',  ( -16.25813024210000179, 1415.087797054229895, 203.3133064409179838 ) ) ;
#77950 = CARTESIAN_POINT ( 'NONE',  ( -12.71183112859999831, 1441.878635263719843, 187.9184463588980236 ) ) ;
#77951 = CARTESIAN_POINT ( 'NONE',  ( 21.83550407203919974, 1523.678648413191695, 234.9693198511250785 ) ) ;
#77952 = B_SPLINE_SURFACE_WITH_KNOTS ( 'NONE', 5, 5, ( 
 ( #4211, #27886, #68808, #52549, #70472, #104591 ),
 ( #78282, #9426, #27326, #43590, #86681, #21523 ),
 ( #81433, #77738, #62069, #35732, #102910, #80915 ),
 ( #38342, #29941, #64133, #9976, #98254, #60398 ),
 ( #55735, #26776, #100460, #31046, #90955, #47860 ),
 ( #107762, #40556, #32708, #66344, #83116, #15336 ) ),
 .UNSPECIFIED., .F., .F., .F.,
 ( 6, 6 ),
 ( 6, 6 ),
 ( 30.40177460629999828, 157.7844419379999863 ),
 ( -6.245004513519998715E-17, 1.000000000000000000 ),
 .UNSPECIFIED. ) ;
#77953 = CARTESIAN_POINT ( 'NONE',  ( -33.92723112960000265, 1435.682240498669898, 135.5030908497980136 ) ) ;
#77954 = DIRECTION ( 'NONE',  ( -0.8672669759446604010, 6.017873532443123780E-15, 0.4978433412588780804 ) ) ;
#77955 = VERTEX_POINT ( 'NONE', #70244 ) ;
#77956 = CARTESIAN_POINT ( 'NONE',  ( -3.165841394545000131, 1511.802450769970164, 201.1846294787470129 ) ) ;
#77957 = CARTESIAN_POINT ( 'NONE',  ( -11.52135570437129886, 1409.315394994109965, 199.5950662629080057 ) ) ;
#77958 = CARTESIAN_POINT ( 'NONE',  ( 10.57600485288619829, 1481.555237149170125, 209.3766040892330125 ) ) ;
#77959 = CARTESIAN_POINT ( 'NONE',  ( -12.67256029850000054, 1474.517343106330145, 266.8981073570980129 ) ) ;
#77960 = CARTESIAN_POINT ( 'NONE',  ( -5.851400963819999745, 1449.323580990290111, 210.4453412175489859 ) ) ;
#77961 = CARTESIAN_POINT ( 'NONE',  ( -20.79738390328759223, 1511.187213306747708, 181.2030061003473236 ) ) ;
#77962 = CARTESIAN_POINT ( 'NONE',  ( 29.40443212115383531, 1512.187213306747481, 196.1539082851714966 ) ) ;
#77963 = CARTESIAN_POINT ( 'NONE',  ( -68.78385482150279984, 1384.665972667470214, 293.6584164674959538 ) ) ;
#77964 = CARTESIAN_POINT ( 'NONE',  ( -16.76289271049750340, 1384.945007802349892, 200.9261315889449975 ) ) ;
#77965 = CARTESIAN_POINT ( 'NONE',  ( 18.04679706737850253, 1424.839701421730069, 226.5258000463729786 ) ) ;
#77966 = CARTESIAN_POINT ( 'NONE',  ( 21.92068900019999944, 1509.678547715230025, 227.8376466598980130 ) ) ;
#77967 = CARTESIAN_POINT ( 'NONE',  ( 14.37537801800000103, 1463.298671107329938, 223.1724039782979787 ) ) ;
#77968 = CIRCLE ( 'NONE', #61941, 1.999999999999999556 ) ;
#77969 = CARTESIAN_POINT ( 'NONE',  ( -26.86198109714170101, 1508.007473140129832, 212.0127264923079906 ) ) ;
#77970 = CARTESIAN_POINT ( 'NONE',  ( 4.325231544520000249, 1515.225845272990000, 208.0336405044189974 ) ) ;
#77971 = CARTESIAN_POINT ( 'NONE',  ( -5.688831827459999602, 1508.347319533530253, 181.0331735192980034 ) ) ;
#77972 = TOROIDAL_SURFACE ( 'NONE', #36815, 6.842541678089999913, 1.000000000000000000 ) ;
#77973 = CARTESIAN_POINT ( 'NONE',  ( -22.29341197009999931, 1409.691563488129987, 205.7443763409079907 ) ) ;
#77974 = CARTESIAN_POINT ( 'NONE',  ( 16.36865316639999790, 1414.913060387329779, 208.9007811298039883 ) ) ;
#77975 = CARTESIAN_POINT ( 'NONE',  ( 4.486170154879999927, 1485.164793332289946, 219.0208057013190057 ) ) ;
#77976 = CARTESIAN_POINT ( 'NONE',  ( -1.393816646507355372, 1511.187213306747708, 175.1051575864439656 ) ) ;
#77977 = CARTESIAN_POINT ( 'NONE',  ( -1.127597643542621819, 1410.331959298673837, 233.0285034547154055 ) ) ;
#77978 = CARTESIAN_POINT ( 'NONE',  ( 7.979825105375810246, 1460.922446521970187, 228.8885227319260025 ) ) ;
#77979 = CARTESIAN_POINT ( 'NONE',  ( 16.88555894881584862, 1525.556090473913855, 181.6768911977973744 ) ) ;
#77980 = CARTESIAN_POINT ( 'NONE',  ( -21.47380247972409961, 1487.892794807240080, 202.0847358610229776 ) ) ;
#77981 =( BOUNDED_SURFACE ( )  B_SPLINE_SURFACE ( 1, 2, ( 
 ( #65650, #39330, #14110 ),
 ( #64560, #80792, #98679 ) ),
 .UNSPECIFIED., .F., .F., .F. ) 
 B_SPLINE_SURFACE_WITH_KNOTS ( ( 2, 2 ),
 ( 3, 3 ),
 ( -10000.00000000000000, 10000.00000000000000 ),
 ( 5.300753508068379638, 6.146881668033620016 ),
 .UNSPECIFIED. ) 
 GEOMETRIC_REPRESENTATION_ITEM ( )  RATIONAL_B_SPLINE_SURFACE ( (
 ( 0.8627701935022120683, 0.8231901671891870276, 0.9535799773170169358),
 ( 0.8627701935022120683, 0.8231901671891870276, 0.9535799773170169358) ) ) 
 REPRESENTATION_ITEM ( '' )  SURFACE ( )  );
#77983 = CARTESIAN_POINT ( 'NONE',  ( 11.07188855578698039, 1414.941240495246575, 222.3943915280714521 ) ) ;
#77982 = CARTESIAN_POINT ( 'NONE',  ( -3.034964906435000387, 1517.051704408389924, 217.3038049130670117 ) ) ;
#77984 = CARTESIAN_POINT ( 'NONE',  ( -4.994804046730000557, 1391.714634656189901, 203.6484225187790287 ) ) ;
#77985 = CARTESIAN_POINT ( 'NONE',  ( 9.777811368307929740, 1435.956396579579859, 210.1555867559330295 ) ) ;
#77986 = CARTESIAN_POINT ( 'NONE',  ( -11.07998396640000038, 1490.998932559390141, 210.3063338810989933 ) ) ;
#77987 = CARTESIAN_POINT ( 'NONE',  ( 10.01154216381359952, 1451.059416430699912, 206.0422016317240264 ) ) ;
#77988 = CARTESIAN_POINT ( 'NONE',  ( -1.203807798849710009, 1419.233902311370002, 185.0625641774459780 ) ) ;
#77989 = CARTESIAN_POINT ( 'NONE',  ( 4.030514512585000375, 1516.901952101700090, 204.4990030879170320 ) ) ;
#77990 = CARTESIAN_POINT ( 'NONE',  ( -5.116792858579263026, 1398.065454244455623, 221.0739902772355663 ) ) ;
#77991 = SURFACE_STYLE_FILL_AREA ( #34880 ) ;
#77992 = CYLINDRICAL_SURFACE ( 'NONE', #76942, 1.999999999999995559 ) ;
#77993 = CARTESIAN_POINT ( 'NONE',  ( -19.81810597710000010, 1468.980723873930174, 193.4065930840980059 ) ) ;
#77994 = CARTESIAN_POINT ( 'NONE',  ( 8.040667369584340918, 1505.155755465120137, 217.5954850267839902 ) ) ;
#77995 = CARTESIAN_POINT ( 'NONE',  ( -11.60674135321730027, 1507.508082919659955, 207.5537295141489835 ) ) ;
#77997 = ORIENTED_EDGE ( 'NONE', *, *, #107812, .T. ) ;
#77996 = CARTESIAN_POINT ( 'NONE',  ( -65.80949023495340100, 1379.740780626450032, 276.1504492283160062 ) ) ;
#77998 = ORIENTED_EDGE ( 'NONE', *, *, #63669, .F. ) ;
#77999 = CARTESIAN_POINT ( 'NONE',  ( 11.33466614171230091, 1434.021404067120102, 151.4990630526469886 ) ) ;
#78000 = CARTESIAN_POINT ( 'NONE',  ( 22.08327125186924533, 1523.604703353109699, 184.4267662568470314 ) ) ;
#78001 = ORIENTED_EDGE ( 'NONE', *, *, #87830, .F. ) ;
#78002 = CARTESIAN_POINT ( 'NONE',  ( -105.7961644359999980, 1379.239079028679953, 306.8423032396589747 ) ) ;
#78003 = CARTESIAN_POINT ( 'NONE',  ( -24.21946005650000089, 1509.534793663830214, 195.2515658952980004 ) ) ;
#78004 = CARTESIAN_POINT ( 'NONE',  ( -17.17241001986462123, 1518.913060387330006, 237.6251415217917895 ) ) ;
#78006 = CARTESIAN_POINT ( 'NONE',  ( -21.59687142900000012, 1507.523380033690046, 209.4572543540780032 ) ) ;
#78005 = CARTESIAN_POINT ( 'NONE',  ( 16.34335051667209981, 1433.455134956249822, 190.8190931015600142 ) ) ;
#78007 = CARTESIAN_POINT ( 'NONE',  ( 13.70362658034589920, 1498.107102624340087, 232.4496494982320201 ) ) ;
#78008 = CARTESIAN_POINT ( 'NONE',  ( 0.4496490820779999731, 1488.176790722930036, 181.7536822793979638 ) ) ;
#78009 = DIRECTION ( 'NONE',  ( 0.2843490923843689511, 0.3717034639898259551, 0.8837319324988487379 ) ) ;
#78010 = CARTESIAN_POINT ( 'NONE',  ( 0.01327253640020150012, 1516.940252185109784, 211.9957649727570015 ) ) ;
#78011 = CARTESIAN_POINT ( 'NONE',  ( 37.65468647792339851, 1436.753545005050000, 134.0999999968539953 ) ) ;
#78012 = CARTESIAN_POINT ( 'NONE',  ( -13.40911912816510032, 1421.283099727030049, 209.4572124756780056 ) ) ;
#78013 = CARTESIAN_POINT ( 'NONE',  ( 7.084879043715000435, 1512.024017243130174, 202.1753317553169893 ) ) ;
#78014 = VERTEX_POINT ( 'NONE', #20332 ) ;
#78015 = CARTESIAN_POINT ( 'NONE',  ( 13.76342018928679956, 1434.978124368779845, 148.5737756231810351 ) ) ;
#78016 = ORIENTED_EDGE ( 'NONE', *, *, #82382, .F. ) ;
#78017 = ORIENTED_EDGE ( 'NONE', *, *, #91494, .T. ) ;
#78018 = EDGE_CURVE ( 'NONE', #56695, #78578, #62088, .T. ) ;
#78019 = CARTESIAN_POINT ( 'NONE',  ( -8.297002917174999936, 1511.752511073100095, 215.1658660083070060 ) ) ;
#78020 = CARTESIAN_POINT ( 'NONE',  ( -1.103937759919999984, 1466.689616642629971, 235.4490393618980022 ) ) ;
#78021 = CARTESIAN_POINT ( 'NONE',  ( -7.550503362009299835, 1510.480349264700180, 214.6730346447039892 ) ) ;
#78022 = B_SPLINE_CURVE_WITH_KNOTS ( 'NONE', 5,
 ( #110685, #32867, #110137, #8212, #101164, #33410 ),
 .UNSPECIFIED., .F., .F.,
 ( 6, 6 ),
 ( 0.000000000000000000, 1.000000000000000000 ),
 .UNSPECIFIED. ) ;
#78023 = CARTESIAN_POINT ( 'NONE',  ( -3.453544863754999472, 1517.106845464700200, 216.4586906126469898 ) ) ;
#78024 = CARTESIAN_POINT ( 'NONE',  ( 10.51154376439999893, 1461.171203229189814, 208.7546265782200123 ) ) ;
#78025 = CARTESIAN_POINT ( 'NONE',  ( -18.99986283518648023, 1443.243851081979983, 211.4893642521566051 ) ) ;
#78026 = CARTESIAN_POINT ( 'NONE',  ( -48.92064667475605688, 1379.684638853033221, 237.5054648401685995 ) ) ;
#78027 = CARTESIAN_POINT ( 'NONE',  ( 4.240875174286579785, 1446.389522495240044, 162.6875343836649961 ) ) ;
#78028 = CARTESIAN_POINT ( 'NONE',  ( 8.641620394141629191, 1437.949431946680079, 209.8872740218120043 ) ) ;
#78029 = EDGE_LOOP ( 'NONE', ( #86250, #77284, #14615, #76925, #79765, #16461, #86456 ) ) ;
#78030 = CARTESIAN_POINT ( 'NONE',  ( -2.493699806765000027, 1516.858326417339867, 206.6451124560869914 ) ) ;
#78031 = ORIENTED_EDGE ( 'NONE', *, *, #98649, .F. ) ;
#78032 = CARTESIAN_POINT ( 'NONE',  ( -105.0203220942489963, 1379.361326776869873, 304.0304199180059754 ) ) ;
#78033 = CARTESIAN_POINT ( 'NONE',  ( -18.93308225230000019, 1509.362410706630044, 230.7219330744979686 ) ) ;
#78034 = ORIENTED_EDGE ( 'NONE', *, *, #2138, .T. ) ;
#78035 = CARTESIAN_POINT ( 'NONE',  ( 27.12879168973760002, 1450.023363157879885, 136.5580283348670037 ) ) ;
#78036 = CARTESIAN_POINT ( 'NONE',  ( -14.86692150049999839, 1409.934051351630160, 190.9079559787980145 ) ) ;
#78037 = CARTESIAN_POINT ( 'NONE',  ( -24.38138454299999935, 1442.062445815139881, 212.1316645750080170 ) ) ;
#78038 = CARTESIAN_POINT ( 'NONE',  ( 3.185905804640090100, 1423.706610472649800, 192.7960985019370241 ) ) ;
#78039 = CARTESIAN_POINT ( 'NONE',  ( -6.150613017182610776, 1511.023286695659863, 201.6389880435640123 ) ) ;
#78040 = CARTESIAN_POINT ( 'NONE',  ( -13.34384734591514565, 1434.923148256851618, 146.7534062989944914 ) ) ;
#78041 = FACE_OUTER_BOUND ( 'NONE', #44005, .T. ) ;
#78042 = CARTESIAN_POINT ( 'NONE',  ( 4.492546581380000958, 1453.878649273890005, 217.3453973181289882 ) ) ;
#78044 = CARTESIAN_POINT ( 'NONE',  ( -3.034926079678273325, 1369.200812461397618, 207.6218459616989946 ) ) ;
#78043 = CARTESIAN_POINT ( 'NONE',  ( -26.13601501283269712, 1491.681802943529874, 212.0165345522650000 ) ) ;
#78045 = CARTESIAN_POINT ( 'NONE',  ( -7.326795561505000443, 1516.760434454289907, 214.9020780475669881 ) ) ;
#78046 = CARTESIAN_POINT ( 'NONE',  ( -2.505509636816239727, 1429.193828627990115, 200.0902972570239911 ) ) ;
#78047 = VECTOR ( 'NONE', #25776, 1000.000000000000000 ) ;
#78048 = DIRECTION ( 'NONE',  ( 0.4794255386041986200, 0.000000000000000000, 0.8775825618903752012 ) ) ;
#78050 = EDGE_CURVE ( 'NONE', #52413, #22689, #19109, .T. ) ;
#78049 = CARTESIAN_POINT ( 'NONE',  ( 29.39269299460000084, 1509.939475844130129, 206.8231667076280189 ) ) ;
#78051 = CARTESIAN_POINT ( 'NONE',  ( 3.269184908365000197, 1516.940296199220029, 211.4060453336370244 ) ) ;
#78052 = EDGE_CURVE ( 'NONE', #6924, #5604, #23151, .T. ) ;
#78053 = CARTESIAN_POINT ( 'NONE',  ( 14.77051248179999909, 1409.598147030530072, 192.0760700751979755 ) ) ;
#78054 = CARTESIAN_POINT ( 'NONE',  ( 30.44070839969077014, 1525.425665131984488, 221.4735044094857699 ) ) ;
#78055 = EDGE_CURVE ( 'NONE', #105548, #63893, #38787, .T. ) ;
#78057 = VERTEX_POINT ( 'NONE', #108753 ) ;
#78056 = CARTESIAN_POINT ( 'NONE',  ( -89.79345263500000840, 1390.581174276010188, 301.0845629396590084 ) ) ;
#78058 = CARTESIAN_POINT ( 'NONE',  ( 39.71670573500000501, 1440.913060382410094, 259.0959246117979546 ) ) ;
#78059 = ADVANCED_FACE ( 'NONE', ( #64028 ), #31187, .T. ) ;
#78060 = CARTESIAN_POINT ( 'NONE',  ( 3.052254580091493530, 1451.555641073906145, 183.9065986230910426 ) ) ;
#78061 = DIRECTION ( 'NONE',  ( 6.505213034913001952E-16, 0.02617694830786544691, -0.9996573249755575929 ) ) ;
#78062 = EDGE_CURVE ( 'NONE', #38471, #100597, #67327, .T. ) ;
#78064 = AXIS2_PLACEMENT_3D ( 'NONE', #7906, #108168, #50490 ) ;
#78063 = CARTESIAN_POINT ( 'NONE',  ( -2.556789166010999814, 1507.689321980810064, 237.0181741517399985 ) ) ;
#78065 = CARTESIAN_POINT ( 'NONE',  ( -19.87162007319999901, 1456.113380717730024, 225.4101704608979730 ) ) ;
#78067 = DIRECTION ( 'NONE',  ( -0.4794255386042041156, 5.511896626706600487E-17, 0.8775825618903722036 ) ) ;
#78066 = CARTESIAN_POINT ( 'NONE',  ( 10.97356389379999975, 1432.589699276930105, 151.7700026489980019 ) ) ;
#78068 = CARTESIAN_POINT ( 'NONE',  ( -0.3822501820940000239, 1506.811133726930166, 187.1259390350979857 ) ) ;
#78069 = FACE_OUTER_BOUND ( 'NONE', #83235, .T. ) ;
#78070 = VERTEX_POINT ( 'NONE', #15222 ) ;
#78071 = CARTESIAN_POINT ( 'NONE',  ( 4.031142351675000235, 1516.929569650079884, 204.1114229688670036 ) ) ;
#78072 = CARTESIAN_POINT ( 'NONE',  ( 0.5565654927739999147, 1405.991402147929875, 266.9610393333979914 ) ) ;
#78073 = CARTESIAN_POINT ( 'NONE',  ( 28.26671296840000025, 1509.671138067530137, 207.1993025267279904 ) ) ;
#78074 = CARTESIAN_POINT ( 'NONE',  ( -4.754578092089379674E-06, 1472.619500892389851, 270.3713690308879904 ) ) ;
#78075 = CARTESIAN_POINT ( 'NONE',  ( 5.418632516149999745, 1435.861377308850024, 154.6842388019980206 ) ) ;
#78076 = EDGE_CURVE ( 'NONE', #59861, #10365, #51612, .T. ) ;
#78077 = CARTESIAN_POINT ( 'NONE',  ( 3.618068937029999876, 1466.495810770989920, 219.1439048061990036 ) ) ;
#78078 = CARTESIAN_POINT ( 'NONE',  ( -20.65862765212969876, 1509.573540226620253, 188.2595568902629850 ) ) ;
#78079 = CARTESIAN_POINT ( 'NONE',  ( -19.01764264267205817, 1526.373507135059981, 232.8535685347059427 ) ) ;
#78080 = CARTESIAN_POINT ( 'NONE',  ( -26.05451239549999798, 1447.172171551439988, 137.7976690009980132 ) ) ;
#78081 = CARTESIAN_POINT ( 'NONE',  ( -0.8724913965011420469, 1450.882592297439942, 154.2430449224139863 ) ) ;
#78082 = DIRECTION ( 'NONE',  ( 0.000000000000000000, 0.000000000000000000, 1.000000000000000000 ) ) ;
#78083 = CARTESIAN_POINT ( 'NONE',  ( 10.82177570574990000, 1480.619340521260028, 210.9524986334820085 ) ) ;
#78084 = FACE_OUTER_BOUND ( 'NONE', #64125, .T. ) ;
#78085 = EDGE_CURVE ( 'NONE', #36047, #73608, #108638, .T. ) ;
#78086 = CARTESIAN_POINT ( 'NONE',  ( -6.265666849954051543, 1447.085106900710343, 215.7369580074560815 ) ) ;
#78087 = EDGE_LOOP ( 'NONE', ( #100192, #85645, #59330, #82089 ) ) ;
#78088 = CARTESIAN_POINT ( 'NONE',  ( 1.608351468689999786, 1426.598937817530214, 144.1938086916980239 ) ) ;
#78089 = CARTESIAN_POINT ( 'NONE',  ( 12.40447486740000116, 1434.419892962859876, 146.9204490281980213 ) ) ;
#78090 = EDGE_CURVE ( 'NONE', #40123, #63057, #93043, .T. ) ;
#78091 = CARTESIAN_POINT ( 'NONE',  ( -1.260684556148445212, 1450.744076110377364, 181.7878351591420767 ) ) ;
#78092 = CARTESIAN_POINT ( 'NONE',  ( 15.36367305140250039, 1457.934436068309878, 189.6495915026669934 ) ) ;
#78093 = CARTESIAN_POINT ( 'NONE',  ( -1.282992545539999837E-09, 1475.759805456229969, 269.0456997843980389 ) ) ;
#78094 = CARTESIAN_POINT ( 'NONE',  ( 11.32069328670000097, 1502.651227823090039, 211.1497760302390247 ) ) ;
#78095 = CARTESIAN_POINT ( 'NONE',  ( 8.289978012700000676, 1427.452913477950005, 211.9970543031389809 ) ) ;
#78096 = CARTESIAN_POINT ( 'NONE',  ( -19.47728386984950077, 1384.863915091259969, 220.7402890748070092 ) ) ;
#78097 = AXIS2_PLACEMENT_3D ( 'NONE', #29736, #46571, #20231 ) ;
#78098 = CARTESIAN_POINT ( 'NONE',  ( -18.47106347599999765, 1415.579607678529783, 207.7286614539779634 ) ) ;
#78099 = B_SPLINE_CURVE_WITH_KNOTS ( 'NONE', 5,
 ( #5762, #108202, #12501, #39904, #47758, #55632 ),
 .UNSPECIFIED., .F., .F.,
 ( 6, 6 ),
 ( -65.26196056268710777, -30.37524181780000276 ),
 .UNSPECIFIED. ) ;
#78100 = CARTESIAN_POINT ( 'NONE',  ( -18.09157779502649888, 1416.524489948229984, 209.2020736640780001 ) ) ;
#78101 = CARTESIAN_POINT ( 'NONE',  ( 18.64672481363430379, 1416.851343896850040, 209.6839434896919840 ) ) ;
#78102 = CARTESIAN_POINT ( 'NONE',  ( -13.45503186213775138, 1443.537314858658419, 169.3628516250983012 ) ) ;
#78103 = ORIENTED_EDGE ( 'NONE', *, *, #49528, .F. ) ;
#78104 = CARTESIAN_POINT ( 'NONE',  ( -16.25887119586559848, 1409.480822287279807, 225.0886774072699836 ) ) ;
#78105 = CARTESIAN_POINT ( 'NONE',  ( 9.821550493440000196, 1443.913060387330006, 148.8455630174979945 ) ) ;
#78106 = ORIENTED_EDGE ( 'NONE', *, *, #64421, .F. ) ;
#78107 = VERTEX_POINT ( 'NONE', #23641 ) ;
#78108 = CARTESIAN_POINT ( 'NONE',  ( -14.93566798913168903, 1416.108416094674567, 205.2278682516571280 ) ) ;
#78110 = CARTESIAN_POINT ( 'NONE',  ( 0.8264992237066920433, 1456.771628818370118, 219.7120364133879775 ) ) ;
#78109 = CARTESIAN_POINT ( 'NONE',  ( 1.538503540740000286, 1455.675331449789837, 218.5739177642490176 ) ) ;
#78111 = CARTESIAN_POINT ( 'NONE',  ( 3.347801439296147041, 1523.382868172864164, 176.1543725841967500 ) ) ;
#78112 = CARTESIAN_POINT ( 'NONE',  ( -11.87010322290000097, 1433.046492610579890, 150.1772076958980051 ) ) ;
#78113 = CARTESIAN_POINT ( 'NONE',  ( -2.822636040217339826, 1419.812953946676771, 186.1531589886093911 ) ) ;
#78114 = CARTESIAN_POINT ( 'NONE',  ( 7.478662903260000050, 1425.010047449799913, 212.2620327022589777 ) ) ;
#78115 = CARTESIAN_POINT ( 'NONE',  ( -17.51543818720000090, 1417.552356044260023, 206.7803260803289902 ) ) ;
#78116 = DIRECTION ( 'NONE',  ( -0.4090087482554316534, -0.000000000000000000, -0.9125304618753967700 ) ) ;
#78117 = CARTESIAN_POINT ( 'NONE',  ( 3.732008881810000123, 1450.492772364150142, 184.1420057466980040 ) ) ;
#78118 = CARTESIAN_POINT ( 'NONE',  ( 8.985456466844782497, 1364.704792932128157, 207.6218459616988241 ) ) ;
#78120 = ORIENTED_EDGE ( 'NONE', *, *, #91352, .F. ) ;
#78119 = CARTESIAN_POINT ( 'NONE',  ( 6.749186742440000053, 1455.205488045889979, 217.3783194977189908 ) ) ;
#78121 = ORIENTED_EDGE ( 'NONE', *, *, #45505, .T. ) ;
#78122 = CARTESIAN_POINT ( 'NONE',  ( -12.33746580920000113, 1440.929426004120160, 187.9427475994980057 ) ) ;
#78123 = CARTESIAN_POINT ( 'NONE',  ( 7.459190098609637332, 1510.844697587253677, 202.9343248737379781 ) ) ;
#78124 = CARTESIAN_POINT ( 'NONE',  ( -0.9866794285430001699, 1473.892698774330029, 270.2925939122980594 ) ) ;
#78125 = CARTESIAN_POINT ( 'NONE',  ( 7.522275854169816256, 1500.273529863827207, 200.5607867249156868 ) ) ;
#78126 = CARTESIAN_POINT ( 'NONE',  ( -1.314910794049999776, 1486.515044105329935, 181.6997297598980197 ) ) ;
#78127 = CARTESIAN_POINT ( 'NONE',  ( -31.92312126443670905, 1524.775785348137561, 201.5796050126409966 ) ) ;
#78128 = LINE ( 'NONE', #61370, #67572 ) ;
#78129 = CARTESIAN_POINT ( 'NONE',  ( 21.99779757700000005, 1409.845346003030045, 206.2854406303680150 ) ) ;
#78130 =( NAMED_UNIT ( * ) PLANE_ANGLE_UNIT ( ) SI_UNIT ( $, .RADIAN. ) );
#78131 = CARTESIAN_POINT ( 'NONE',  ( -2.500000000000000000, 1448.561607529700041, 159.6824365648180049 ) ) ;
#78132 = CARTESIAN_POINT ( 'NONE',  ( 8.251048879689999893, 1367.474174444410210, 207.6218459616989946 ) ) ;
#78133 = CARTESIAN_POINT ( 'NONE',  ( 13.38380976650000065, 1409.321262751630002, 216.4729699453379794 ) ) ;
#78134 = CARTESIAN_POINT ( 'NONE',  ( -2.267841090553740280, 1406.812775593299875, 269.6487269905239827 ) ) ;
#78135 = CARTESIAN_POINT ( 'NONE',  ( 29.99620953741496976, 1524.382868172863937, 219.7462484079458704 ) ) ;
#78136 = ORIENTED_EDGE ( 'NONE', *, *, #53056, .F. ) ;
#78137 = CARTESIAN_POINT ( 'NONE',  ( -10.96941897680000011, 1432.344069211809938, 151.7701285249980003 ) ) ;
#78138 = CARTESIAN_POINT ( 'NONE',  ( 13.54145629459999967, 1443.508061120249977, 188.5908682209980327 ) ) ;
#78139 = ORIENTED_EDGE ( 'NONE', *, *, #53572, .F. ) ;
#78140 = EDGE_LOOP ( 'NONE', ( #13216, #88972, #30229, #80031, #79867, #25779, #29250, #72380, #10121, #82415, #6134, #102153, #16223, #77731 ) ) ;
#78141 = EDGE_CURVE ( 'NONE', #64595, #75633, #109861, .T. ) ;
#78142 = B_SPLINE_CURVE_WITH_KNOTS ( 'NONE', 3,
 ( #31536, #56756, #5804, #39945, #74115, #48921, #65711, #99833, #23124, #57329, #6342, #40490, #32094, #94754, #59517, #79084, #102034, #77957, #85800, #86908, #60076, #26436, #1263, #93629, #70152, #18574, #52769, #43263, #94192, #27009, #19127, #61197, #34294, #10198, #69590, #18032, #25320, #42706, #52224, #68477, #44373, #51662, #35964, #60631, #87476, #9635, #17461, #86351, #78518, #44937, #16907, #27554, #9098, #77410, #1829, #95314, #43807, #103708, #35402, #36507, #104264, #34844, #61736, #95860, #716, #51113, #8531, #53328, #10766, #2391, #85237, #76862, #102578, #25874, #69035, #103136, #173, #98605, #88036, #13479, #53901, #70703, #81797, #54443, #79632, #12398, #5099, #28662, #11320, #54985, #55529, #38698, #63937, #3482, #30297, #72874, #81249, #96420, #89110, #37610, #19698, #4564, #62867, #45491, #71812, #2936, #64490, #4027, #63400, #21869, #97516, #28102, #47669, #104814, #46584, #88577, #89655, #96979, #56068, #37053, #11860 ),
 .UNSPECIFIED., .F., .F.,
 ( 4, 3, 3, 3, 3, 3, 3, 3, 3, 3, 3, 3, 3, 3, 3, 3, 3, 3, 3, 3, 3, 3, 3, 3, 3, 3, 3, 3, 3, 3, 3, 3, 3, 3, 3, 3, 3, 3, 3, 3, 4 ),
 ( 15.94786254319999941, 17.28652221311410031, 18.62887769919689873, 19.97220876837939940, 21.31551003014599743, 22.65777570309839817, 23.99648260799839861, 25.33228087000049911, 26.66197833009550067, 27.90025324481390356, 29.21922251675360016, 30.54537470099209884, 31.87781318686680265, 33.21548123473309744, 34.55717461623120101, 35.90156568275600080, 37.27590617873740086, 38.62028396294829946, 39.96291520885479542, 41.30221225282429032, 42.70073160226989728, 44.02712524576659803, 45.34784220011430023, 46.65983834663869345, 46.89628965060690291, 48.21084064340449515, 49.53265281890470817, 50.86114174345969730, 52.24619684876979875, 53.58794959607750741, 54.99465588038880526, 56.40136216470000363, 57.75144886590140914, 59.10083358886660676, 60.44821813932610155, 61.79246594079870647, 63.13251995115560078, 64.46420547887859698, 65.79044557759550571, 67.10676169860950324, 68.30549982530000364 ),
 .UNSPECIFIED. ) ;
#78143 = CARTESIAN_POINT ( 'NONE',  ( -3.943364034450000499, 1453.941432717190082, 199.4131967690690033 ) ) ;
#78144 = CARTESIAN_POINT ( 'NONE',  ( -8.232155009519999567, 1367.485244382299925, 207.6218459616989946 ) ) ;
#78145 = AXIS2_PLACEMENT_3D ( 'NONE', #58788, #95935, #68315 ) ;
#78146 = EDGE_CURVE ( 'NONE', #96293, #83569, #3099, .T. ) ;
#78147 = CARTESIAN_POINT ( 'NONE',  ( -3.254401441735000233, 1516.919782530640077, 213.1645757730269963 ) ) ;
#78148 = CARTESIAN_POINT ( 'NONE',  ( 3.385713881024999594, 1511.191277613550028, 216.7448064569670123 ) ) ;
#78149 = ORIENTED_EDGE ( 'NONE', *, *, #91698, .F. ) ;
#78150 = CARTESIAN_POINT ( 'NONE',  ( -64.85694393360000731, 1378.892054699950222, 269.1292758489590256 ) ) ;
#78151 = CARTESIAN_POINT ( 'NONE',  ( -106.0202621536679999, 1378.913060387289988, 302.8609204498379768 ) ) ;
#78152 = CARTESIAN_POINT ( 'NONE',  ( -3.457266643525000127, 1516.691414181030041, 203.3491180233569935 ) ) ;
#78153 = ADVANCED_FACE ( 'NONE', ( #24715 ), #33021, .T. ) ;
#78154 = CARTESIAN_POINT ( 'NONE',  ( -27.56049296109999958, 1508.045672656129909, 205.3679835307079884 ) ) ;
#78155 = CARTESIAN_POINT ( 'NONE',  ( -2.234923082067399758, 1512.341036938790012, 201.5226187867249905 ) ) ;
#78156 = CARTESIAN_POINT ( 'NONE',  ( -50.83427392639999454, 1384.622306023270085, 226.1831986462590010 ) ) ;
#78157 = CARTESIAN_POINT ( 'NONE',  ( -63.63661578303909749, 1384.696032145409845, 252.0136171407070265 ) ) ;
#78158 = CARTESIAN_POINT ( 'NONE',  ( -4.305815836009999842, 1409.063422789429978, 194.9846847171979789 ) ) ;
#78159 = CARTESIAN_POINT ( 'NONE',  ( -109.1462309409999989, 1385.214558625939844, 311.2612093662589814 ) ) ;
#78161 = ORIENTED_EDGE ( 'NONE', *, *, #31621, .T. ) ;
#78160 = CARTESIAN_POINT ( 'NONE',  ( -10.82839717969999960, 1445.293858117500122, 185.2652248665980039 ) ) ;
#78162 = DIRECTION ( 'NONE',  ( 1.755985294532469921E-16, -1.000000000000000000, 1.338183447452831989E-16 ) ) ;
#78163 = CARTESIAN_POINT ( 'NONE',  ( 22.56155900549999771, 1488.679832657330053, 222.5656005121980172 ) ) ;
#78164 = CARTESIAN_POINT ( 'NONE',  ( 19.47156422787159968, 1467.105613706720078, 225.2196683951030138 ) ) ;
#78165 = CARTESIAN_POINT ( 'NONE',  ( -25.15095490240000231, 1436.448645567330004, 137.6015634021979679 ) ) ;
#78166 = CARTESIAN_POINT ( 'NONE',  ( -6.546951720715000533, 1516.606339319019980, 211.9964348928969855 ) ) ;
#78167 = CARTESIAN_POINT ( 'NONE',  ( -68.73088892949999718, 1379.748097453069931, 280.1074355248589995 ) ) ;
#78168 = VECTOR ( 'NONE', #52091, 1000.000000000000000 ) ;
#78169 = CARTESIAN_POINT ( 'NONE',  ( 17.05938516367379876, 1517.051704408300111, 223.0487112149370148 ) ) ;
#78170 = CARTESIAN_POINT ( 'NONE',  ( 20.49831092009999978, 1496.178973653789853, 204.1013708937389879 ) ) ;
#78172 = EDGE_CURVE ( 'NONE', #68723, #107075, #90587, .T. ) ;
#78171 = CARTESIAN_POINT ( 'NONE',  ( -11.60004869885203860, 1423.633889433519244, 135.8155558205586999 ) ) ;
#78173 = CARTESIAN_POINT ( 'NONE',  ( -0.7559395363919990674, 1516.972341476009888, 207.9998125401569951 ) ) ;
#78174 = ORIENTED_EDGE ( 'NONE', *, *, #72432, .F. ) ;
#78175 = CARTESIAN_POINT ( 'NONE',  ( 0.000000000000000000, 1420.584111001019892, 209.1218459616989946 ) ) ;
#78176 = CARTESIAN_POINT ( 'NONE',  ( -6.472888217819999568, 1410.296278320529836, 231.2922198908979965 ) ) ;
#78177 =( BOUNDED_CURVE ( )  B_SPLINE_CURVE ( 3, ( #100093, #4925, #6034, #56449 ),
 .UNSPECIFIED., .F., .T. ) 
 B_SPLINE_CURVE_WITH_KNOTS ( ( 4, 4 ),
 ( 0.5395807524062695704, 1.539014399150256507 ),
 .UNSPECIFIED. ) 
 CURVE ( )  GEOMETRIC_REPRESENTATION_ITEM ( )  RATIONAL_B_SPLINE_CURVE ( ( 1.000000000000000000, 0.9184788592064836443, 0.9184788592064836443, 1.000000000000000000 ) ) 
 REPRESENTATION_ITEM ( '' )  );
#78178 = CARTESIAN_POINT ( 'NONE',  ( -27.62594988560000075, 1384.837137189770147, 225.6315537474590371 ) ) ;
#78179 = EDGE_CURVE ( 'NONE', #35149, #8260, #41798, .T. ) ;
#78180 = ORIENTED_EDGE ( 'NONE', *, *, #27154, .T. ) ;
#78181 = CARTESIAN_POINT ( 'NONE',  ( -14.28317992867999919, 1385.297258702939871, 219.2703623637189878 ) ) ;
#78182 = FACE_OUTER_BOUND ( 'NONE', #66922, .T. ) ;
#78183 = CARTESIAN_POINT ( 'NONE',  ( 12.10947664135730051, 1433.934507095030085, 149.7604101384789885 ) ) ;
#78184 = CARTESIAN_POINT ( 'NONE',  ( 16.39369216350290159, 1478.707785154150088, 230.0407356733170161 ) ) ;
#78185 = CARTESIAN_POINT ( 'NONE',  ( -21.84620687390529881, 1509.359330091720039, 227.5754383244390056 ) ) ;
#78186 = CARTESIAN_POINT ( 'NONE',  ( -2.559321582819999996, 1409.169965997630015, 187.1278009686979829 ) ) ;
#78187 = CARTESIAN_POINT ( 'NONE',  ( -20.64978683589999875, 1464.413060387330006, 208.6332757997560066 ) ) ;
#78188 = CARTESIAN_POINT ( 'NONE',  ( -0.1622974587355989762, 1420.471025021490050, 182.7601356185510042 ) ) ;
#78189 = EDGE_CURVE ( 'NONE', #20574, #36754, #83545, .T. ) ;
#78191 = CARTESIAN_POINT ( 'NONE',  ( 13.94974641142899863, 1428.477645029930045, 195.9751451731039822 ) ) ;
#78190 = CARTESIAN_POINT ( 'NONE',  ( 3.456007385174999946, 1516.647534046129977, 215.6697273451470096 ) ) ;
#78192 = CARTESIAN_POINT ( 'NONE',  ( -8.867335203187609594, 1385.164153589130137, 218.6750454735870051 ) ) ;
#78193 = CARTESIAN_POINT ( 'NONE',  ( -2.291514335905000088, 1517.194972660189933, 216.8481778957070105 ) ) ;
#78194 = CIRCLE ( 'NONE', #104979, 2.000000000000003553 ) ;
#78195 = ORIENTED_EDGE ( 'NONE', *, *, #90435, .F. ) ;
#78196 = CARTESIAN_POINT ( 'NONE',  ( -11.49746945758320038, 1414.913060387399810, 197.9010059328040256 ) ) ;
#78197 = CARTESIAN_POINT ( 'NONE',  ( -0.7401336709869998920, 1504.313428565929826, 180.8842383983980255 ) ) ;
#78198 = ORIENTED_EDGE ( 'NONE', *, *, #21299, .T. ) ;
#78199 = CARTESIAN_POINT ( 'NONE',  ( 3.865613834079999922, 1421.793636752730208, 184.2641810182979896 ) ) ;
#78200 = EDGE_CURVE ( 'NONE', #8750, #107607, #27499, .T. ) ;
#78201 = CARTESIAN_POINT ( 'NONE',  ( 7.558973819147550621, 1511.169205552290123, 203.0547742380890099 ) ) ;
#78202 = UNCERTAINTY_MEASURE_WITH_UNIT (LENGTH_MEASURE( 1.000000000000000082E-05 ), #35457, 'distance_accuracy_value', 'NONE');
#78203 = CARTESIAN_POINT ( 'NONE',  ( 4.123426501090060370, 1424.433584402349879, 191.6254363278619905 ) ) ;
#78204 = CARTESIAN_POINT ( 'NONE',  ( -33.72300830903907354, 1524.397344074319108, 198.6568221122821001 ) ) ;
#78205 = CARTESIAN_POINT ( 'NONE',  ( -740.1067050525047080, 11216.44053380569312, -1627.040744445698465 ) ) ;
#78206 = CARTESIAN_POINT ( 'NONE',  ( 18.01569507700000017, 1415.245980409429876, 210.3065621575879902 ) ) ;
#78207 = CARTESIAN_POINT ( 'NONE',  ( -29.13505175353617105, 1526.073429442291854, 221.0961561632167047 ) ) ;
#78208 = CARTESIAN_POINT ( 'NONE',  ( 9.142604584464409712, 1459.538234665719983, 203.9517274866290109 ) ) ;
#78209 = CARTESIAN_POINT ( 'NONE',  ( -11.98890328080000067, 1442.756953654919926, 147.5994355510979688 ) ) ;
#78210 = CARTESIAN_POINT ( 'NONE',  ( 17.28367426750000035, 1438.551524929770039, 190.7595339831979970 ) ) ;
#78212 = CARTESIAN_POINT ( 'NONE',  ( -5.050863578716279001, 1391.819074324308986, 203.5808726994333426 ) ) ;
#78211 = CARTESIAN_POINT ( 'NONE',  ( 11.72865777870000059, 1490.920838208090117, 205.3345067772989978 ) ) ;
#78213 = CARTESIAN_POINT ( 'NONE',  ( 11.89956352200635514, 1433.602129414034835, 150.4843578385222429 ) ) ;
#78214 = EDGE_LOOP ( 'NONE', ( #52843, #27325, #97704, #42387 ) ) ;
#78215 = CARTESIAN_POINT ( 'NONE',  ( 1.555056480579879885, 1415.348334734329910, 191.0095454046629868 ) ) ;
#78216 = CARTESIAN_POINT ( 'NONE',  ( -4.987082680427599612, 1508.551704408389924, 212.3948994024580088 ) ) ;
#78217 = EDGE_CURVE ( 'NONE', #73589, #89045, #96554, .T. ) ;
#78218 = AXIS2_PLACEMENT_3D ( 'NONE', #69149, #95439, #52899 ) ;
#78219 = CARTESIAN_POINT ( 'NONE',  ( -23.76810219530000268, 1436.580689387229995, 212.1216956802879849 ) ) ;
#78220 = DIRECTION ( 'NONE',  ( 1.755985294532464991E-16, -1.000000000000000000, 1.338183447452830017E-16 ) ) ;
#78221 = CARTESIAN_POINT ( 'NONE',  ( -3.767230627251568542, 1426.013493162819032, 186.0052132243664857 ) ) ;
#78222 = EDGE_CURVE ( 'NONE', #27899, #94269, #97916, .T. ) ;
#78223 = CARTESIAN_POINT ( 'NONE',  ( -10.82822666317459870, 1452.534930380020796, 150.8032249176135906 ) ) ;
#78224 = CARTESIAN_POINT ( 'NONE',  ( -11.00840296587000111, 1470.178642279830001, 211.9751469970929918 ) ) ;
#78225 = CARTESIAN_POINT ( 'NONE',  ( -2.298652125478059638, 1486.462338610419920, 220.8290092987670050 ) ) ;
#78226 = CARTESIAN_POINT ( 'NONE',  ( 12.98226561589999939, 1414.913060387329779, 198.3280246956980193 ) ) ;
#78227 = CARTESIAN_POINT ( 'NONE',  ( -91.70122676012400120, 1383.769245710449923, 309.0451135184819691 ) ) ;
#78228 = CARTESIAN_POINT ( 'NONE',  ( 20.30910795649999656, 1452.203850710330016, 143.8526422108979830 ) ) ;
#78229 = CARTESIAN_POINT ( 'NONE',  ( -5.085463042024069402, 1391.851494597096007, 214.6322330144460864 ) ) ;
#78230 = CARTESIAN_POINT ( 'NONE',  ( -2.589417882402239801, 1516.541553964140121, 201.4126244432099782 ) ) ;
#78232 = ORIENTED_EDGE ( 'NONE', *, *, #40406, .F. ) ;
#78231 = CARTESIAN_POINT ( 'NONE',  ( 10.56298886728909991, 1452.344034128999965, 208.9192460544000198 ) ) ;
#78233 = CARTESIAN_POINT ( 'NONE',  ( -18.54348539920661310, 1458.676082630350265, 227.5712260952941506 ) ) ;
#78234 = CARTESIAN_POINT ( 'NONE',  ( -73.68066259569999943, 1383.781794063629832, 298.8244620241590042 ) ) ;
#78235 = CARTESIAN_POINT ( 'NONE',  ( 20.44002321923020205, 1509.591610260329844, 230.3558478251790120 ) ) ;
#78236 = ORIENTED_EDGE ( 'NONE', *, *, #76813, .T. ) ;
#78237 = ORIENTED_EDGE ( 'NONE', *, *, #82806, .F. ) ;
#78238 = CARTESIAN_POINT ( 'NONE',  ( 18.87514223596030050, 1508.290019403229735, 229.9499626354140105 ) ) ;
#78239 = CARTESIAN_POINT ( 'NONE',  ( 29.17014196280698357, 1526.382868172864164, 201.0245104653888006 ) ) ;
#78240 = CARTESIAN_POINT ( 'NONE',  ( 36.46881799559510284, 1437.630696346240029, 136.5444991984829812 ) ) ;
#78242 = CARTESIAN_POINT ( 'NONE',  ( -35.51625744890000647, 1458.123784601630177, 261.8360505382980250 ) ) ;
#78241 = CARTESIAN_POINT ( 'NONE',  ( 19.73776679929999744, 1452.815214894130122, 209.1683919043709921 ) ) ;
#78243 = CARTESIAN_POINT ( 'NONE',  ( 8.736406163737710173, 1436.941576091229763, 209.9790183900369982 ) ) ;
#78244 = VECTOR ( 'NONE', #5643, 1000.000000000000000 ) ;
#78245 = CARTESIAN_POINT ( 'NONE',  ( -108.7558059640000039, 1382.069376407850086, 297.7710658298590261 ) ) ;
#78246 = DIRECTION ( 'NONE',  ( -1.000000000000000000, -0.000000000000000000, 0.000000000000000000 ) ) ;
#78247 = CARTESIAN_POINT ( 'NONE',  ( -19.21347146162490205, 1475.323696206919976, 227.8639392199079907 ) ) ;
#78248 = CARTESIAN_POINT ( 'NONE',  ( 2.331552110770000130, 1409.931811533030213, 185.5473801112979686 ) ) ;
#78249 = CARTESIAN_POINT ( 'NONE',  ( 6.032762746330000425, 1424.401310572229931, 186.1143022581979949 ) ) ;
#78250 = CARTESIAN_POINT ( 'NONE',  ( -11.10313724959999959, 1434.937811603489990, 151.7082816907980032 ) ) ;
#78251 = CARTESIAN_POINT ( 'NONE',  ( 8.909955910623979847, 1434.607648340320111, 206.3240839377490090 ) ) ;
#78252 = CARTESIAN_POINT ( 'NONE',  ( -15.68969716385069901, 1421.005191948239826, 203.3991960173040070 ) ) ;
#78253 = AXIS2_PLACEMENT_3D ( 'NONE', #85283, #8582, #42752 ) ;
#78254 = CARTESIAN_POINT ( 'NONE',  ( 0.04349594477419999744, 1452.084370642229942, 153.9873474275979959 ) ) ;
#78255 = CARTESIAN_POINT ( 'NONE',  ( 2.439425361020000071, 1464.676489221029897, 236.7027247366980021 ) ) ;
#78256 = VERTEX_POINT ( 'NONE', #48731 ) ;
#78257 = CARTESIAN_POINT ( 'NONE',  ( -11.53818992870000137, 1506.400027429489910, 207.4085574012289896 ) ) ;
#78258 = CARTESIAN_POINT ( 'NONE',  ( 22.28449968809999859, 1476.748388319289916, 209.6248863100890105 ) ) ;
#78259 = CARTESIAN_POINT ( 'NONE',  ( -43.48864174949999750, 1442.487458641120156, 270.3367078953979785 ) ) ;
#78260 = DIRECTION ( 'NONE',  ( -1.000000000000000000, 0.000000000000000000, 0.000000000000000000 ) ) ;
#78261 = CARTESIAN_POINT ( 'NONE',  ( 9.522333297019999421, 1438.200918636809774, 153.1793569429979982 ) ) ;
#78262 = CARTESIAN_POINT ( 'NONE',  ( -14.65012730729999824, 1474.165513649029890, 223.7053439215980006 ) ) ;
#78263 = CARTESIAN_POINT ( 'NONE',  ( 12.86224528119999988, 1519.913060387329779, 190.2411470757980112 ) ) ;
#78264 = CARTESIAN_POINT ( 'NONE',  ( 2.785137360674800000, 1409.020299217710090, 230.3656739585919979 ) ) ;
#78265 = DIRECTION ( 'NONE',  ( 0.000000000000000000, 0.000000000000000000, 1.000000000000000000 ) ) ;
#78266 = CARTESIAN_POINT ( 'NONE',  ( -4.149035421649998945, 1416.659952005129981, 232.5357826803979719 ) ) ;
#78267 = FACE_OUTER_BOUND ( 'NONE', #3659, .T. ) ;
#78268 = CARTESIAN_POINT ( 'NONE',  ( 0.05823133897989880153, 1360.390585217559874, 207.6218459616989946 ) ) ;
#78269 = CARTESIAN_POINT ( 'NONE',  ( -45.83452011949149352, 1439.843055403779999, 268.7569621144950247 ) ) ;
#78270 = CARTESIAN_POINT ( 'NONE',  ( -2.500000000000000000, 1428.691959813929998, 184.5792689180979949 ) ) ;
#78271 = ORIENTED_EDGE ( 'NONE', *, *, #94728, .F. ) ;
#78272 = DIRECTION ( 'NONE',  ( -1.836970198721029688E-16, -1.000000000000000000, 0.000000000000000000 ) ) ;
#78273 = ORIENTED_EDGE ( 'NONE', *, *, #102850, .T. ) ;
#78274 = CARTESIAN_POINT ( 'NONE',  ( -5.775625115495000017, 1516.745833913490060, 209.8771724060850090 ) ) ;
#78275 = ADVANCED_FACE ( 'NONE', ( #22931 ), #69269, .F. ) ;
#78276 = CARTESIAN_POINT ( 'NONE',  ( -7.269615836804730336, 1508.603735221707211, 203.6084103740970193 ) ) ;
#78277 = AXIS2_PLACEMENT_3D ( 'NONE', #29719, #99660, #38122 ) ;
#78278 = CARTESIAN_POINT ( 'NONE',  ( -25.91590772737680126, 1441.261220175949802, 138.4451201564890255 ) ) ;
#78279 = CARTESIAN_POINT ( 'NONE',  ( -16.18321133039999893, 1425.423028787829935, 190.7319080598980179 ) ) ;
#78280 = CARTESIAN_POINT ( 'NONE',  ( 1.879472310086659936, 1495.752734514360100, 221.3175895178520136 ) ) ;
#78281 = EDGE_LOOP ( 'NONE', ( #43451, #5746, #95022, #79045 ) ) ;
#78282 = CARTESIAN_POINT ( 'NONE',  ( -15.00906777690000027, 1488.801231226830168, 193.7268783320979821 ) ) ;
#78284 = CARTESIAN_POINT ( 'NONE',  ( 14.28229724340000040, 1470.816572150529964, 194.5131132564980021 ) ) ;
#78283 = CARTESIAN_POINT ( 'NONE',  ( 5.268140179660000477, 1505.035622830590000, 220.7476737412989962 ) ) ;
#78285 = CARTESIAN_POINT ( 'NONE',  ( 6.554778533645000849, 1516.929962200689943, 201.4024535497269994 ) ) ;
#78286 = CARTESIAN_POINT ( 'NONE',  ( -11.54861850680875435, 1426.051521667020324, 138.9191312498616071 ) ) ;
#78287 = EDGE_CURVE ( 'NONE', #57816, #7082, #76371, .T. ) ;
#78288 = CARTESIAN_POINT ( 'NONE',  ( -1.876581345759999797, 1456.020558252990213, 215.5707636483290059 ) ) ;
#78289 = CARTESIAN_POINT ( 'NONE',  ( -8.305912316622009683, 1438.481564584539910, 206.5261465373520195 ) ) ;
#78290 = ORIENTED_EDGE ( 'NONE', *, *, #72108, .F. ) ;
#78291 = CARTESIAN_POINT ( 'NONE',  ( -0.5908173565667990124, 1410.389843549470015, 269.3346523052649673 ) ) ;
#78292 = CARTESIAN_POINT ( 'NONE',  ( 4.031168767865001001, 1516.805675336850072, 208.3649472324300120 ) ) ;
#78293 = CARTESIAN_POINT ( 'NONE',  ( 4.949847236731660161, 1418.068533308110091, 233.9905393452280009 ) ) ;
#78294 = DIRECTION ( 'NONE',  ( 0.3255681544571546460, 0.000000000000000000, 0.9455185755993176233 ) ) ;
#78295 = ADVANCED_FACE ( 'NONE', ( #71761 ), #56715, .T. ) ;
#78297 = ORIENTED_EDGE ( 'NONE', *, *, #102131, .F. ) ;
#78296 = CARTESIAN_POINT ( 'NONE',  ( -7.811405798899279773, 1367.739269854455870, 210.6218459616987957 ) ) ;
#78298 = ORIENTED_EDGE ( 'NONE', *, *, #92734, .F. ) ;
#78299 = DIRECTION ( 'NONE',  ( 0.000000000000000000, -1.000000000000000000, 6.123233995736769734E-17 ) ) ;
#78300 = CARTESIAN_POINT ( 'NONE',  ( -4.320810598459999596, 1425.290410123230004, 186.1758918437979844 ) ) ;
#78301 = CARTESIAN_POINT ( 'NONE',  ( -10.78266347204017883, 1438.594363250573679, 152.4465531432095418 ) ) ;
#78302 = CIRCLE ( 'NONE', #108759, 2.000000000000000444 ) ;
#78303 = CARTESIAN_POINT ( 'NONE',  ( 2.372478608332516892, 1522.862737210649811, 174.8996806668726549 ) ) ;
#78304 = CARTESIAN_POINT ( 'NONE',  ( -18.43142101346469985, 1424.689440642639966, 194.8163951100160034 ) ) ;
#78305 = CARTESIAN_POINT ( 'NONE',  ( -18.25008163810000283, 1425.818581969829893, 225.5639177453979869 ) ) ;
#78306 = CARTESIAN_POINT ( 'NONE',  ( 33.11929144969669636, 1465.571379411549970, 267.3866912509090525 ) ) ;
#78307 = B_SPLINE_CURVE_WITH_KNOTS ( 'NONE', 5,
 ( #18647, #77484, #85870, #60701, #25942, #52296 ),
 .UNSPECIFIED., .F., .F.,
 ( 6, 6 ),
 ( 0.000000000000000000, 1.000000000000000000 ),
 .UNSPECIFIED. ) ;
#78308 = CARTESIAN_POINT ( 'NONE',  ( -11.46335139447689855, 1391.913060387289988, 207.5095624942730126 ) ) ;
#78309 = CARTESIAN_POINT ( 'NONE',  ( 9.095534004770000180, 1445.600425117210079, 184.8596504565979899 ) ) ;
#78310 = CARTESIAN_POINT ( 'NONE',  ( -4.624099329465000352, 1516.962555622980062, 205.8665050058069994 ) ) ;
#78311 = VERTEX_POINT ( 'NONE', #106957 ) ;
#78312 = CARTESIAN_POINT ( 'NONE',  ( -0.3646785421350010048, 1445.165625539289977, 215.3775912058289919 ) ) ;
#78313 = CARTESIAN_POINT ( 'NONE',  ( 1.479947764255840070, 1478.089622790649855, 182.3790958322389884 ) ) ;
#78314 = CARTESIAN_POINT ( 'NONE',  ( 23.61060712979999821, 1411.111110838729928, 207.8239932459379986 ) ) ;
#78315 = ORIENTED_EDGE ( 'NONE', *, *, #41387, .T. ) ;
#78316 = CARTESIAN_POINT ( 'NONE',  ( -3.968827101022720072, 1521.951704408389787, 229.5396913742049776 ) ) ;
#78317 = EDGE_CURVE ( 'NONE', #34791, #21200, #72561, .T. ) ;
#78318 = CARTESIAN_POINT ( 'NONE',  ( 25.51240218741290278, 1451.577767330780034, 136.5542256109710024 ) ) ;
#78319 = CYLINDRICAL_SURFACE ( 'NONE', #93665, 2.000000000000003553 ) ;
#78320 = CARTESIAN_POINT ( 'NONE',  ( -3.078458351979999730, 1388.284543639960020, 200.7814874055890186 ) ) ;
#78321 = EDGE_CURVE ( 'NONE', #83093, #508, #92563, .T. ) ;
#78322 = B_SPLINE_CURVE_WITH_KNOTS ( 'NONE', 5,
 ( #87813, #12180, #97291, #45815, #46371, #9977, #78283, #103850, #102715 ),
 .UNSPECIFIED., .F., .F.,
 ( 6, 3, 6 ),
 ( -3.420211715829999832, -1.710105857910000138, 0.000000000000000000 ),
 .UNSPECIFIED. ) ;
#78323 = DIRECTION ( 'NONE',  ( -1.224646799147350002E-16, 1.836970198721029688E-16, 1.000000000000000000 ) ) ;
#78324 = CARTESIAN_POINT ( 'NONE',  ( 17.69895706029999971, 1410.894947626029989, 192.9683006637980043 ) ) ;
#78325 = CARTESIAN_POINT ( 'NONE',  ( -3.874459836649999822, 1495.423322680889896, 197.4164389294989803 ) ) ;
#78326 = CARTESIAN_POINT ( 'NONE',  ( 3.206067321177020979, 1439.684559099622675, 184.2987211024194778 ) ) ;
#78328 = CARTESIAN_POINT ( 'NONE',  ( -19.86494872359075003, 1426.191873834269927, 222.7246227809951336 ) ) ;
#78327 = CARTESIAN_POINT ( 'NONE',  ( 2.046266125239999845, 1417.477797419130184, 235.2693601201980016 ) ) ;
#78329 = AXIS2_PLACEMENT_3D ( 'NONE', #14592, #22415, #65020 ) ;
#78330 = CARTESIAN_POINT ( 'NONE',  ( 1.111973768122940021, 1450.991701817079957, 182.4208154947999958 ) ) ;
#78331 = EDGE_CURVE ( 'NONE', #944, #30887, #69256, .T. ) ;
#78332 = CARTESIAN_POINT ( 'NONE',  ( 18.50343566175140353, 1467.878388117720078, 228.1213590980190133 ) ) ;
#78333 = CARTESIAN_POINT ( 'NONE',  ( -8.472397538460000987, 1381.589775986109998, 218.2249286227190055 ) ) ;
#78334 = CIRCLE ( 'NONE', #33622, 2.458500000000000352 ) ;
#78335 = CARTESIAN_POINT ( 'NONE',  ( -5.774609660074999873, 1516.777260590120022, 213.7418541773069762 ) ) ;
#78336 = CARTESIAN_POINT ( 'NONE',  ( 3.017174818680797177, 1525.408337840050081, 241.3338438474178815 ) ) ;
#78337 = ORIENTED_EDGE ( 'NONE', *, *, #100969, .T. ) ;
#78338 = CARTESIAN_POINT ( 'NONE',  ( -17.14339296960000070, 1417.642190471430013, 207.4869690162090023 ) ) ;
#78339 = CARTESIAN_POINT ( 'NONE',  ( -24.34268787264259970, 1442.549328851149994, 212.2035684885649687 ) ) ;
#78340 = CARTESIAN_POINT ( 'NONE',  ( -0.4546767127886620075, 1409.373319351459941, 232.7794293636910083 ) ) ;
#78341 = B_SPLINE_CURVE_WITH_KNOTS ( 'NONE', 5,
 ( #54429, #38138, #64474, #13461, #79619, #72320, #71797, #63385, #72858, #12927, #55512, #90179 ),
 .UNSPECIFIED., .F., .F.,
 ( 6, 3, 3, 6 ),
 ( 0.000000000000000000, 0.3850691707344797710, 0.6691521531983583015, 1.000000000000000000 ),
 .UNSPECIFIED. ) ;
#78342 = ADVANCED_FACE ( 'NONE', ( #94992 ), #44043, .T. ) ;
#78343 = VECTOR ( 'NONE', #18911, 1000.000000000000000 ) ;
#78344 = CARTESIAN_POINT ( 'NONE',  ( -19.09790268268400126, 1508.458003811930212, 210.0050661408479868 ) ) ;
#78345 = CARTESIAN_POINT ( 'NONE',  ( -33.91369269983620427, 1450.440666099120108, 136.2454419983430114 ) ) ;
#78346 = CARTESIAN_POINT ( 'NONE',  ( -4.328991615394409465, 1515.082251143310032, 207.7602669075220092 ) ) ;
#78347 = CARTESIAN_POINT ( 'NONE',  ( -18.41412373400000035, 1444.997163189090088, 209.1218459616979999 ) ) ;
#78348 = CARTESIAN_POINT ( 'NONE',  ( -2.649360860297129694, 1451.956705521739877, 184.7216075439289966 ) ) ;
#78349 = CARTESIAN_POINT ( 'NONE',  ( 11.30061245240000112, 1433.709615238220067, 151.5117488965980215 ) ) ;
#78350 = CARTESIAN_POINT ( 'NONE',  ( 1.110223024629999949E-15, 1454.846680951630105, 214.3676144195279676 ) ) ;
#78351 = CARTESIAN_POINT ( 'NONE',  ( 26.56266887126210108, 1440.913060393550040, 224.7525115906159954 ) ) ;
#78352 = CARTESIAN_POINT ( 'NONE',  ( -14.34085026152870057, 1421.948958043559969, 196.2628561903719913 ) ) ;
#78353 = ADVANCED_FACE ( 'NONE', ( #78182 ), #108077, .T. ) ;
#78354 = DIRECTION ( 'NONE',  ( -9.152776640618289361E-47, 1.000000000000000000, -1.836970198721029688E-16 ) ) ;
#78355 = CARTESIAN_POINT ( 'NONE',  ( 10.22342693278199910, 1462.397256940530042, 211.7726961121359750 ) ) ;
#78356 = CARTESIAN_POINT ( 'NONE',  ( -1.961418762362024282, 1526.143142182216707, 240.4212258933359578 ) ) ;
#78357 = CARTESIAN_POINT ( 'NONE',  ( -29.00753178363559570, 1509.926023647250076, 200.7080847602200038 ) ) ;
#78358 = AXIS2_PLACEMENT_3D ( 'NONE', #75626, #25178, #109760 ) ;
#78359 = ADVANCED_FACE ( 'NONE', ( #72557 ), #38382, .T. ) ;
#78360 = CARTESIAN_POINT ( 'NONE',  ( 19.06924801490000121, 1449.793579036090023, 224.4195381262979936 ) ) ;
#78361 = CARTESIAN_POINT ( 'NONE',  ( -17.59976141832330043, 1419.797097700060021, 206.6695233765389901 ) ) ;
#78362 = CARTESIAN_POINT ( 'NONE',  ( 5.807361285020000314E-16, 1430.453334911130241, 150.3332009510979788 ) ) ;
#78363 = CARTESIAN_POINT ( 'NONE',  ( -27.67491638513010344, 1383.844931811260039, 225.5862836080119962 ) ) ;
#78364 = CARTESIAN_POINT ( 'NONE',  ( 16.66442746070229930, 1492.498864031070070, 193.3249227824980210 ) ) ;
#78365 = EDGE_CURVE ( 'NONE', #69308, #91119, #81856, .T. ) ;
#78366 = CARTESIAN_POINT ( 'NONE',  ( -1.702754409475000008, 1517.014196759610059, 212.5856132281170119 ) ) ;
#78367 = CYLINDRICAL_SURFACE ( 'NONE', #36164, 2.000000000000003109 ) ;
#78368 = CARTESIAN_POINT ( 'NONE',  ( 0.1610941246609420008, 1485.608819109279921, 181.8534184629149877 ) ) ;
#78370 = VERTEX_POINT ( 'NONE', #37299 ) ;
#78369 = CARTESIAN_POINT ( 'NONE',  ( -8.181958980964999739, 1517.051704408389924, 206.0868810637969943 ) ) ;
#78371 = DIRECTION ( 'NONE',  ( 0.000000000000000000, 0.000000000000000000, 1.000000000000000000 ) ) ;
#78372 = B_SPLINE_CURVE_WITH_KNOTS ( 'NONE', 3,
 ( #81333, #3026, #4114, #71345, #4647, #88120, #80257, #64578, #29840, #38785, #107098, #81887, #11409, #37149, #30387, #88668, #98697, #21957, #11946, #47752, #3574, #37698, #71901, #58360, #15220, #110401, #24713, #108751, #91946, #92485, #58911, #100351, #57821, #42106, #49412, #49956, #23074, #50516, #6830, #90842 ),
 .UNSPECIFIED., .F., .F.,
 ( 4, 3, 3, 3, 3, 3, 3, 3, 3, 3, 3, 3, 3, 4 ),
 ( -1.459712257500000110, -1.414311702603749943, -1.300049757133459938, -1.184105919937280094, -1.067104322070629996, -0.9485798734533590348, -0.8293278323600270507, -0.7096591974163730665, -0.5899191834374760690, -0.4656630299999721112, -0.3474018752853509362, -0.2302575540096110096, -0.1144180656139759389, 2.220446049250313081E-16 ),
 .UNSPECIFIED. ) ;
#78373 = CARTESIAN_POINT ( 'NONE',  ( -10.57956098816219459, 1390.295224638445688, 202.7063012876982668 ) ) ;
#78374 = CARTESIAN_POINT ( 'NONE',  ( 22.08327125186944428, 1523.604703353109699, 233.8169256665487694 ) ) ;
#78376 = ORIENTED_EDGE ( 'NONE', *, *, #1758, .F. ) ;
#78375 = CARTESIAN_POINT ( 'NONE',  ( -32.21013329178911988, 1524.412928176729110, 216.0988866155133508 ) ) ;
#78377 = CARTESIAN_POINT ( 'NONE',  ( -5.593318843000940177, 1508.551704408389924, 219.5394102594769947 ) ) ;
#78378 = ORIENTED_EDGE ( 'NONE', *, *, #49397, .T. ) ;
#78379 = CARTESIAN_POINT ( 'NONE',  ( -14.32988524930309993, 1380.323806007950225, 209.8281070544639988 ) ) ;
#78380 = CARTESIAN_POINT ( 'NONE',  ( -16.44108894340000049, 1415.931669658129977, 216.8029115086079628 ) ) ;
#78381 = CARTESIAN_POINT ( 'NONE',  ( -0.4986843622567649348, 1508.982343520079894, 238.8510830230749775 ) ) ;
#78382 = CARTESIAN_POINT ( 'NONE',  ( -2.824362723775959427, 1367.715796969916255, 209.3184871409762309 ) ) ;
#78383 = AXIS2_PLACEMENT_3D ( 'NONE', #86524, #51838, #94932 ) ;
#78384 = CARTESIAN_POINT ( 'NONE',  ( 0.2700213805099990205, 1431.728054808090064, 218.6309394840390041 ) ) ;
#78385 = CARTESIAN_POINT ( 'NONE',  ( -12.30520345314149822, 1377.738549314298552, 208.6947277391683144 ) ) ;
#78386 = CARTESIAN_POINT ( 'NONE',  ( 14.70986748862159921, 1409.426740279159958, 206.5596626142009882 ) ) ;
#78387 = CARTESIAN_POINT ( 'NONE',  ( -11.15007135000000105, 1391.248055150329947, 203.8486859877390032 ) ) ;
#78388 = CARTESIAN_POINT ( 'NONE',  ( -78.28007596846539684, 1385.150550643550105, 280.7138181926990228 ) ) ;
#78389 = CARTESIAN_POINT ( 'NONE',  ( -16.66093153799999982, 1410.867388830529990, 191.7374817029979681 ) ) ;
#78390 = CARTESIAN_POINT ( 'NONE',  ( 9.799815244658731217, 1423.431771991869937, 209.4823171178350094 ) ) ;
#78391 = EDGE_LOOP ( 'NONE', ( #22435, #106505, #53833, #8114 ) ) ;
#78392 = CARTESIAN_POINT ( 'NONE',  ( 10.81586312699060137, 1489.669647427700056, 207.5188354526409853 ) ) ;
#78394 = ORIENTED_EDGE ( 'NONE', *, *, #54820, .F. ) ;
#78393 = CARTESIAN_POINT ( 'NONE',  ( 12.78776258891489981, 1416.851343896290018, 222.2791104166909975 ) ) ;
#78395 = CARTESIAN_POINT ( 'NONE',  ( 33.91369278643569629, 1437.010534640189690, 136.5611839302279691 ) ) ;
#78396 = ORIENTED_EDGE ( 'NONE', *, *, #92452, .F. ) ;
#78397 = CARTESIAN_POINT ( 'NONE',  ( 6.039844978529999686, 1450.200509822089998, 208.6657062937080127 ) ) ;
#78398 = CARTESIAN_POINT ( 'NONE',  ( -7.592149787980000397, 1361.964468435470053, 207.6218459616989946 ) ) ;
#78399 = CARTESIAN_POINT ( 'NONE',  ( -11.71170459750000070, 1433.766298954200238, 151.0909624611979893 ) ) ;
#78400 = CARTESIAN_POINT ( 'NONE',  ( 29.84411685202790565, 1462.363335203606994, 269.4691510201575966 ) ) ;
#78401 = CARTESIAN_POINT ( 'NONE',  ( -30.80549360313072427, 1524.130440953581001, 221.8448932001217031 ) ) ;
#78402 = FACE_OUTER_BOUND ( 'NONE', #77546, .T. ) ;
#78403 = CARTESIAN_POINT ( 'NONE',  ( 32.21013329178848750, 1524.412928176728428, 202.1448053078787552 ) ) ;
#78404 = CARTESIAN_POINT ( 'NONE',  ( -7.079928805590961716, 1516.557407140219766, 211.5970724783486219 ) ) ;
#78405 = CARTESIAN_POINT ( 'NONE',  ( -105.3788045886400084, 1309.112692017090239, 304.2218459572590064 ) ) ;
#78406 = CARTESIAN_POINT ( 'NONE',  ( -8.232155009518420385, 1367.485244382291967, 210.6218459616991936 ) ) ;
#78407 = FACE_OUTER_BOUND ( 'NONE', #91742, .T. ) ;
#78408 = CYLINDRICAL_SURFACE ( 'NONE', #78817, 2.000000000000003553 ) ;
#78409 = CARTESIAN_POINT ( 'NONE',  ( 3.251611325815000342, 1516.779243033999819, 206.8234764622770001 ) ) ;
#78410 = TOROIDAL_SURFACE ( 'NONE', #57006, 6.842541678089999913, 1.000000000000000000 ) ;
#78411 = DIRECTION ( 'NONE',  ( -1.000000000000000000, 0.000000000000000000, 0.000000000000000000 ) ) ;
#78412 = CARTESIAN_POINT ( 'NONE',  ( 11.78824854703250047, 1517.151704408390060, 211.4132493584619965 ) ) ;
#78413 = CARTESIAN_POINT ( 'NONE',  ( 6.817746255100000319, 1475.057956560229968, 269.6447263236980234 ) ) ;
#78416 = ORIENTED_EDGE ( 'NONE', *, *, #87728, .F. ) ;
#78415 = CARTESIAN_POINT ( 'NONE',  ( -2.719997508650000118, 1496.976443727390006, 221.2163582191989804 ) ) ;
#78414 = VECTOR ( 'NONE', #62767, 999.9999999999998863 ) ;
#78417 = CARTESIAN_POINT ( 'NONE',  ( 11.36018337630000019, 1414.996442546230128, 222.2791104318980047 ) ) ;
#78418 = VERTEX_POINT ( 'NONE', #54673 ) ;
#78419 = VECTOR ( 'NONE', #88128, 1000.000000000000227 ) ;
#78420 = CARTESIAN_POINT ( 'NONE',  ( 9.638115859579080791, 1516.551188146539971, 214.4931927712729873 ) ) ;
#78421 = CARTESIAN_POINT ( 'NONE',  ( -26.47779523690000048, 1469.247571742229866, 208.2308877974680001 ) ) ;
#78423 = CARTESIAN_POINT ( 'NONE',  ( 16.40767016540999634, 1409.511151603330063, 193.0217009399570145 ) ) ;
#78422 = CARTESIAN_POINT ( 'NONE',  ( -10.97659976954949990, 1425.661045819329956, 113.0066238976479980 ) ) ;
#78424 = CARTESIAN_POINT ( 'NONE',  ( -3.252530653725000054, 1516.827328999679821, 212.0018028951869837 ) ) ;
#78425 = CARTESIAN_POINT ( 'NONE',  ( 18.37396616818673678, 1509.673958510744797, 185.4069322651564846 ) ) ;
#78426 = CARTESIAN_POINT ( 'NONE',  ( -21.84849975889999740, 1489.480617680329942, 208.5290360645649912 ) ) ;
#78427 = CARTESIAN_POINT ( 'NONE',  ( -28.66942461389999863, 1426.582479899429927, 248.2467662554980166 ) ) ;
#78428 = CARTESIAN_POINT ( 'NONE',  ( 18.52468149035910017, 1509.577301616600153, 232.1917227349059942 ) ) ;
#78429 = CARTESIAN_POINT ( 'NONE',  ( 17.24781598545795802, 1460.195507983534526, 228.5738697325721773 ) ) ;
#78430 = CARTESIAN_POINT ( 'NONE',  ( 4.475991544341880513, 1508.551704408389924, 213.1231739162390113 ) ) ;
#78431 = CARTESIAN_POINT ( 'NONE',  ( 2.994688454485729956, 1464.609795419120246, 236.6065850994260131 ) ) ;
#78432 = ORIENTED_EDGE ( 'NONE', *, *, #15257, .F. ) ;
#78433 = CARTESIAN_POINT ( 'NONE',  ( 12.59185353107299932, 1397.673301978809832, 213.9584579308699972 ) ) ;
#78434 = CARTESIAN_POINT ( 'NONE',  ( 9.301629471904078628, 1462.018477543640074, 206.2660014330650142 ) ) ;
#78435 = CARTESIAN_POINT ( 'NONE',  ( -18.32069918539999875, 1457.567609363029987, 229.9399091793980006 ) ) ;
#78436 = ORIENTED_EDGE ( 'NONE', *, *, #80813, .T. ) ;
#78437 = ORIENTED_EDGE ( 'NONE', *, *, #88419, .F. ) ;
#78438 = CARTESIAN_POINT ( 'NONE',  ( -29.24670345068486910, 1509.934423202144217, 211.7350478754418930 ) ) ;
#78439 = CARTESIAN_POINT ( 'NONE',  ( -6.356853423171860307, 1423.329120530439923, 150.6733129965809894 ) ) ;
#78440 = EDGE_LOOP ( 'NONE', ( #82127, #101152, #48575, #100668, #100813 ) ) ;
#78441 = CARTESIAN_POINT ( 'NONE',  ( 0.5075932631809999540, 1412.056819125330094, 184.9972924272980208 ) ) ;
#78442 = CIRCLE ( 'NONE', #13994, 1.000000000000000888 ) ;
#78443 = DIRECTION ( 'NONE',  ( 1.755985294532464991E-16, -1.000000000000000000, 1.338183447452830017E-16 ) ) ;
#78444 = DIRECTION ( 'NONE',  ( -0.6736849260863837507, 0.000000000000000000, 0.7390186874254154326 ) ) ;
#78445 = CARTESIAN_POINT ( 'NONE',  ( -2.412918666629999986, 1461.195343464629786, 234.9240695220980228 ) ) ;
#78446 = CARTESIAN_POINT ( 'NONE',  ( 7.320051246071350270, 1508.610505975320166, 203.0404454350509695 ) ) ;
#78447 = CARTESIAN_POINT ( 'NONE',  ( 9.721563988697850434, 1451.950384167230141, 209.1155634365840115 ) ) ;
#78448 = CARTESIAN_POINT ( 'NONE',  ( 19.41157449629999832, 1457.417846740989944, 209.1218459616989946 ) ) ;
#78449 = CARTESIAN_POINT ( 'NONE',  ( -100.3573076095590011, 1384.875324114890191, 296.3320123604629543 ) ) ;
#78450 = EDGE_LOOP ( 'NONE', ( #81322, #95255, #51376, #100685 ) ) ;
#78451 = CARTESIAN_POINT ( 'NONE',  ( -2.487103457664999961, 1516.577434278289957, 202.5755431900869894 ) ) ;
#78452 = CARTESIAN_POINT ( 'NONE',  ( -7.713648872314999849, 1516.710624944440042, 209.8745175203999906 ) ) ;
#78453 = ORIENTED_EDGE ( 'NONE', *, *, #77428, .T. ) ;
#78454 = CARTESIAN_POINT ( 'NONE',  ( 11.85272800890160028, 1431.406550633420011, 149.9031061979179924 ) ) ;
#78455 = ADVANCED_FACE ( 'NONE', ( #71491 ), #61973, .F. ) ;
#78456 = DIRECTION ( 'NONE',  ( -0.9125304618754029873, 0.000000000000000000, -0.4090087482554177756 ) ) ;
#78457 = ORIENTED_EDGE ( 'NONE', *, *, #96154, .F. ) ;
#78458 = DIRECTION ( 'NONE',  ( 0.08014523039090584722, -0.9891236767552784581, -0.1233332644816800827 ) ) ;
#78459 = ADVANCED_FACE ( 'NONE', ( #4248 ), #37849, .F. ) ;
#78460 = CARTESIAN_POINT ( 'NONE',  ( -4.835422890569469168, 1508.443244997879901, 220.2371915919370053 ) ) ;
#78461 = DIRECTION ( 'NONE',  ( 0.000000000000000000, 0.000000000000000000, 1.000000000000000000 ) ) ;
#78462 = CARTESIAN_POINT ( 'NONE',  ( 32.86802468386292730, 1501.977400791986611, 217.2040256693915410 ) ) ;
#78463 = CARTESIAN_POINT ( 'NONE',  ( -4.785570096949999908, 1423.623530998630031, 184.5509701510979710 ) ) ;
#78464 = CARTESIAN_POINT ( 'NONE',  ( 3.400294879866609943, 1410.489090383209941, 269.3360835134739659 ) ) ;
#78465 = CARTESIAN_POINT ( 'NONE',  ( 32.38845791999500534, 1523.382868172864164, 216.1254071228445639 ) ) ;
#78466 = CARTESIAN_POINT ( 'NONE',  ( -109.9754776966811392, 1384.008075049679974, 297.0180362684087640 ) ) ;
#78467 = CARTESIAN_POINT ( 'NONE',  ( 11.24566101859999812, 1493.273975466890079, 214.3640310562390141 ) ) ;
#78468 = CARTESIAN_POINT ( 'NONE',  ( -21.16646057260000191, 1379.602502976239975, 209.5833567688460164 ) ) ;
#78469 = SPHERICAL_SURFACE ( 'NONE', #39205, 7.299999999999999822 ) ;
#78471 = CARTESIAN_POINT ( 'NONE',  ( 10.49331861557109846, 1469.560031205900032, 204.9147316216790102 ) ) ;
#78470 = CARTESIAN_POINT ( 'NONE',  ( -20.22175671919999829, 1505.497798682489929, 209.1006163569459773 ) ) ;
#78472 = CARTESIAN_POINT ( 'NONE',  ( -68.59216743299973018, 1379.747776907655634, 280.1820150774575495 ) ) ;
#78473 = CARTESIAN_POINT ( 'NONE',  ( -9.963890954553210833, 1439.503587905810036, 208.3753853002669985 ) ) ;
#78474 = CARTESIAN_POINT ( 'NONE',  ( -13.86092847646930082, 1410.765486861110048, 227.1170286572800023 ) ) ;
#78475 = ORIENTED_EDGE ( 'NONE', *, *, #50763, .F. ) ;
#78476 = CARTESIAN_POINT ( 'NONE',  ( 17.26713005559999914, 1428.027535763729929, 234.3916895853979838 ) ) ;
#78477 = DIRECTION ( 'NONE',  ( 0.000000000000000000, -0.000000000000000000, 1.000000000000000000 ) ) ;
#78478 = B_SPLINE_SURFACE_WITH_KNOTS ( 'NONE', 5, 5, ( 
 ( #108327, #31060, #100473, #56831, #83126, #14254, #83668, #75297, #23756 ),
 ( #74740, #40569, #4756, #13137, #5874, #91530, #65788, #65241, #32721 ),
 ( #66902, #99908, #48994, #108878, #66355, #24308, #58488, #47321, #81448 ),
 ( #56276, #13685, #47872, #82009, #5315, #73644, #99352, #22627, #27095 ),
 ( #86433, #69111, #1341, #16439, #18114, #43347, #85313, #35480, #52309 ),
 ( #68009, #42233, #26518, #110530, #69673, #33814, #8608, #102119, #25398 ),
 ( #33264, #59048, #59591, #92616, #9724, #43889, #103212, #51183, #42784 ),
 ( #76943, #51747, #60716, #78033, #25953, #50093, #93169, #15893, #60148 ),
 ( #75837, #24845, #94838, #253, #76381, #103796, #84220, #109987, #34380 ) ),
 .UNSPECIFIED., .F., .F., .F.,
 ( 6, 3, 6 ),
 ( 6, 3, 6 ),
 ( 1.119735183810000034, 3.314582533139999843, 6.273244355579999265 ),
 ( 0.000000000000000000, 1.000000000000000000, 2.000000000000000000 ),
 .UNSPECIFIED. ) ;
#78479 = CARTESIAN_POINT ( 'NONE',  ( -18.10570579381849043, 1525.713797967456912, 180.1226510103712144 ) ) ;
#78480 = CARTESIAN_POINT ( 'NONE',  ( 5.246441130820000076, 1506.817910960390009, 219.5624344324990034 ) ) ;
#78481 = CYLINDRICAL_SURFACE ( 'NONE', #70620, 33.13701971169416538 ) ;
#78483 = ORIENTED_EDGE ( 'NONE', *, *, #96543, .T. ) ;
#78482 = CARTESIAN_POINT ( 'NONE',  ( -0.1783569643517119996, 1515.156623775960043, 204.7948018622450093 ) ) ;
#78484 = CARTESIAN_POINT ( 'NONE',  ( -15.62663836450985855, 1415.708812752953463, 209.6394265537848582 ) ) ;
#78485 = CARTESIAN_POINT ( 'NONE',  ( 11.26937486967429969, 1478.652699849539886, 205.8601904136019982 ) ) ;
#78486 = CARTESIAN_POINT ( 'NONE',  ( -16.22969151800000276, 1416.527220236440144, 208.6990027614089911 ) ) ;
#78487 = CARTESIAN_POINT ( 'NONE',  ( -7.821732098484999618, 1516.863303996349941, 201.3872288444869980 ) ) ;
#78488 = CARTESIAN_POINT ( 'NONE',  ( 11.28295019303499913, 1512.609537213029853, 225.3524656301670177 ) ) ;
#78489 = CARTESIAN_POINT ( 'NONE',  ( 4.362764246034863902, 1370.448454204201653, 209.4935560900470648 ) ) ;
#78490 = FACE_OUTER_BOUND ( 'NONE', #94632, .T. ) ;
#78491 = CARTESIAN_POINT ( 'NONE',  ( 13.40566205669149902, 1429.098591087019940, 222.0107402452829888 ) ) ;
#78492 = CARTESIAN_POINT ( 'NONE',  ( -15.78856002036499717, 1512.525301340740043, 222.7193983515670084 ) ) ;
#78493 = CARTESIAN_POINT ( 'NONE',  ( 11.23079704630000109, 1415.077546157430106, 229.5486842020980021 ) ) ;
#78494 = CARTESIAN_POINT ( 'NONE',  ( -11.29380069599010028, 1482.268690959019978, 207.2091524315400193 ) ) ;
#78495 = CARTESIAN_POINT ( 'NONE',  ( -16.21296007320000143, 1459.516395508230062, 228.9531164853979988 ) ) ;
#78497 = AXIS2_PLACEMENT_3D ( 'NONE', #75247, #107171, #82534 ) ;
#78496 = CARTESIAN_POINT ( 'NONE',  ( -0.01327257453019850021, 1516.940252185109784, 206.2479269295770052 ) ) ;
#78498 = CARTESIAN_POINT ( 'NONE',  ( 21.81698820680000495, 1410.329754421929920, 269.1143266171980031 ) ) ;
#78499 = CARTESIAN_POINT ( 'NONE',  ( -33.45065857237986506, 1524.841055067849993, 219.4656524796156987 ) ) ;
#78500 = EDGE_CURVE ( 'NONE', #91965, #9014, #36191, .T. ) ;
#78501 = CARTESIAN_POINT ( 'NONE',  ( -20.55201027734695884, 1526.382868172863937, 236.4070436938631872 ) ) ;
#78502 = CIRCLE ( 'NONE', #58835, 10.00000000000000888 ) ;
#78503 = CARTESIAN_POINT ( 'NONE',  ( 19.34978595810000002, 1469.161539876029792, 191.0314867524980116 ) ) ;
#78504 = CARTESIAN_POINT ( 'NONE',  ( -21.78276816909999880, 1430.096355600930110, 220.5348153272979914 ) ) ;
#78505 = CARTESIAN_POINT ( 'NONE',  ( -12.31203607247529952, 1378.312412832470272, 208.4582867090369973 ) ) ;
#78506 = LINE ( 'NONE', #69580, #49501 ) ;
#78507 =( BOUNDED_CURVE ( )  B_SPLINE_CURVE ( 3, ( #95862, #79086, #69593, #53331 ),
 .UNSPECIFIED., .F., .F. ) 
 B_SPLINE_CURVE_WITH_KNOTS ( ( 4, 4 ),
 ( 5.085528608296080222, 5.733722764883870227 ),
 .UNSPECIFIED. ) 
 CURVE ( )  GEOMETRIC_REPRESENTATION_ITEM ( )  RATIONAL_B_SPLINE_CURVE ( ( 1.000000000000000000, 0.9652924339432646939, 0.9652924339432646939, 1.000000000000000000 ) ) 
 REPRESENTATION_ITEM ( '' )  );
#78508 = CARTESIAN_POINT ( 'NONE',  ( 7.629404627771598335, 1479.880594065073410, 228.0747595323517771 ) ) ;
#78509 = EDGE_CURVE ( 'NONE', #46650, #110498, #96022, .T. ) ;
#78510 = CARTESIAN_POINT ( 'NONE',  ( -19.72497237273909931, 1506.501081260519868, 199.2811559755782014 ) ) ;
#78511 = CARTESIAN_POINT ( 'NONE',  ( -17.84625751240000113, 1415.088275290029969, 207.8799776997580011 ) ) ;
#78512 = CARTESIAN_POINT ( 'NONE',  ( -12.47743317399999974, 1441.795364512870037, 187.8062295142980247 ) ) ;
#78513 = CARTESIAN_POINT ( 'NONE',  ( 21.96543842109177902, 1523.313115944345327, 235.2592135320308273 ) ) ;
#78514 = CARTESIAN_POINT ( 'NONE',  ( -31.76432995890000299, 1436.935670857599916, 136.6280379864980148 ) ) ;
#78515 = CARTESIAN_POINT ( 'NONE',  ( -0.8190328885345301568, 1418.969064690915957, 184.8287215811062651 ) ) ;
#78516 = ORIENTED_EDGE ( 'NONE', *, *, #1118, .F. ) ;
#78517 = CARTESIAN_POINT ( 'NONE',  ( -31.23437356469425907, 1512.187213306747481, 221.8968241038848248 ) ) ;
#78518 = CARTESIAN_POINT ( 'NONE',  ( -14.93003779297889899, 1409.434428795590065, 209.1736875269810128 ) ) ;
#78519 = CARTESIAN_POINT ( 'NONE',  ( -13.23573713899709858, 1508.551704408300111, 210.3365014446919758 ) ) ;
#78520 = DIRECTION ( 'NONE',  ( 0.000000000000000000, 0.000000000000000000, -1.000000000000000000 ) ) ;
#78521 = CARTESIAN_POINT ( 'NONE',  ( -44.77906958589999675, 1451.150212632430112, 268.5354239598979689 ) ) ;
#78523 = CIRCLE ( 'NONE', #107128, 1.999999954377635225 ) ;
#78522 = CARTESIAN_POINT ( 'NONE',  ( -11.82810778686869924, 1481.586904978749999, 209.9993492298939941 ) ) ;
#78524 = CARTESIAN_POINT ( 'NONE',  ( 0.4837104977199940259, 1418.710257852230143, 184.7118620339130075 ) ) ;
#78525 = CARTESIAN_POINT ( 'NONE',  ( -15.93623144086499899, 1516.904916668740043, 193.9453790007669909 ) ) ;
#78526 = CARTESIAN_POINT ( 'NONE',  ( -64.31866039319710637, 1384.679996067239927, 287.7687853453900289 ) ) ;
#78527 = CARTESIAN_POINT ( 'NONE',  ( -17.60051359271830052, 1384.946495389480106, 201.0930959932179860 ) ) ;
#78528 = CARTESIAN_POINT ( 'NONE',  ( 17.04506599712540194, 1423.842078673229935, 228.2841224977100296 ) ) ;
#78529 = CARTESIAN_POINT ( 'NONE',  ( 14.85820445110000065, 1414.971262582530017, 216.9249339935579997 ) ) ;
#78530 = CARTESIAN_POINT ( 'NONE',  ( -3.229222591820000154, 1433.444289491620111, 155.4497426196979859 ) ) ;
#78531 = CARTESIAN_POINT ( 'NONE',  ( -25.84539468360279812, 1482.717571151330048, 211.4979452547460141 ) ) ;
#78532 = CARTESIAN_POINT ( 'NONE',  ( 4.261736558349999981, 1515.372048625790057, 207.2788822659889831 ) ) ;
#78533 = CARTESIAN_POINT ( 'NONE',  ( -10.12762402319999921, 1509.205805730729935, 181.4374674442979938 ) ) ;
#78534 = CARTESIAN_POINT ( 'NONE',  ( -23.76303430200000122, 1410.238322737530098, 208.1246107068909907 ) ) ;
#78535 = CARTESIAN_POINT ( 'NONE',  ( 16.56387297150000393, 1416.216596894529857, 201.3979519333380210 ) ) ;
#78536 = CARTESIAN_POINT ( 'NONE',  ( 3.476014316090000111, 1485.192983848789936, 219.6841126116989926 ) ) ;
#78537 = CARTESIAN_POINT ( 'NONE',  ( 3.825556360259999789, 1423.414717582890034, 193.7421645440990119 ) ) ;
#78538 = CARTESIAN_POINT ( 'NONE',  ( -106.7768089814430112, 1391.913060387289988, 306.1367433662150006 ) ) ;
#78539 = CARTESIAN_POINT ( 'NONE',  ( 20.83586984089999916, 1457.604279698989785, 206.7633391697789875 ) ) ;
#78540 = CARTESIAN_POINT ( 'NONE',  ( -6.961841786822310141, 1508.551566289579796, 215.6737177159799899 ) ) ;
#78541 = CARTESIAN_POINT ( 'NONE',  ( 24.04367183766050076, 1494.655699982339911, 207.1743773502899728 ) ) ;
#78543 = CARTESIAN_POINT ( 'NONE',  ( -9.916501125940001771, 1380.324599945550062, 201.6733442065789745 ) ) ;
#78542 = CARTESIAN_POINT ( 'NONE',  ( -22.47141948400000189, 1410.193803399830131, 211.4552637418080110 ) ) ;
#78544 = CARTESIAN_POINT ( 'NONE',  ( -5.236048287610000074, 1391.923671795290147, 203.6379494214189947 ) ) ;
#78545 = CARTESIAN_POINT ( 'NONE',  ( 9.817701725550250558, 1435.668645397809996, 209.4942759991459980 ) ) ;
#78546 = CARTESIAN_POINT ( 'NONE',  ( -15.46160582433359920, 1420.394257567060095, 210.8293740474650235 ) ) ;
#78547 = CARTESIAN_POINT ( 'NONE',  ( -10.02185219040000064, 1364.916310432309956, 210.6218459616991936 ) ) ;
#78548 = CARTESIAN_POINT ( 'NONE',  ( 1.705466410464999916, 1517.120861839400050, 204.1076508302870138 ) ) ;
#78549 = CARTESIAN_POINT ( 'NONE',  ( -14.37359814958930038, 1486.056774777669943, 185.9402136656559890 ) ) ;
#78550 = CARTESIAN_POINT ( 'NONE',  ( 1.455000239979999943, 1507.073729426630052, 236.7651042955980074 ) ) ;
#78551 = CARTESIAN_POINT ( 'NONE',  ( 10.46238070710109902, 1503.718831861420085, 214.1759217846949923 ) ) ;
#78552 = AXIS2_PLACEMENT_3D ( 'NONE', #15136, #31955, #66148 ) ;
#78553 = CARTESIAN_POINT ( 'NONE',  ( 40.05116234797749541, 1447.068974477369920, 136.6106942782779754 ) ) ;
#78555 = ORIENTED_EDGE ( 'NONE', *, *, #100179, .F. ) ;
#78554 = CARTESIAN_POINT ( 'NONE',  ( -64.29128857122019269, 1379.736509255219971, 273.6614271908390492 ) ) ;
#78556 = B_SPLINE_CURVE_WITH_KNOTS ( 'NONE', 3,
 ( #107154, #90341, #39404, #108811, #73581, #107712, #65173, #32105, #25330, #51674, #58968, #109917, #9109, #24236, #51122, #85246, #726, #66833, #84697, #84151, #103147, #18043, #7451, #76871, #76314, #67937, #77422, #94201, #60085, #94765, #52236, #93102, #85811, #33196, #67387, #75228, #93638, #75768, #24772, #185, #43276, #102044, #86365 ),
 .UNSPECIFIED., .F., .F.,
 ( 4, 3, 3, 3, 3, 3, 3, 3, 3, 3, 3, 3, 3, 3, 4 ),
 ( 0.7655572723410000169, 0.9910019231850759613, 1.224379699286819889, 1.462078616762300109, 1.704827355037529912, 1.793853281190000093, 2.038466588173669880, 2.281256469890939886, 2.316155491860000026, 2.583989317150000353, 2.855920918845609613, 3.139267314119390306, 3.387490793019999558, 3.680707214893210732, 3.835724788439999422 ),
 .UNSPECIFIED. ) ;
#78557 = ORIENTED_EDGE ( 'NONE', *, *, #25126, .F. ) ;
#78558 = CARTESIAN_POINT ( 'NONE',  ( 11.96574013264010006, 1433.577777978849781, 149.9770704080709720 ) ) ;
#78559 = CARTESIAN_POINT ( 'NONE',  ( 21.53712143570552939, 1523.621879633028811, 183.9400870382961841 ) ) ;
#78560 = ORIENTED_EDGE ( 'NONE', *, *, #83296, .F. ) ;
#78561 = CARTESIAN_POINT ( 'NONE',  ( -105.3679517439999955, 1379.024053303089886, 305.1804760158589716 ) ) ;
#78562 = CARTESIAN_POINT ( 'NONE',  ( -10.33201215501379977, 1448.420692391850025, 208.1592603127500070 ) ) ;
#78564 = CARTESIAN_POINT ( 'NONE',  ( 4.743041381730000339, 1427.184332118029943, 133.6118001900980232 ) ) ;
#78563 = CYLINDRICAL_SURFACE ( 'NONE', #88954, 2.000000000000003553 ) ;
#78565 = CARTESIAN_POINT ( 'NONE',  ( 12.61234839950090070, 1460.710915196400038, 224.9907160281699987 ) ) ;
#78566 = CIRCLE ( 'NONE', #35623, 2.000000000000009770 ) ;
#78567 = FACE_OUTER_BOUND ( 'NONE', #5965, .T. ) ;
#78568 = CARTESIAN_POINT ( 'NONE',  ( 10.35429883085484981, 1439.070324005060911, 152.7368639322063189 ) ) ;
#78569 = CARTESIAN_POINT ( 'NONE',  ( -24.21915031236209970, 1444.789092827589911, 211.4477932164650156 ) ) ;
#78570 = B_SPLINE_SURFACE_WITH_KNOTS ( 'NONE', 5, 4, ( 
 ( #83045, #40487, #81372, #32643, #24220 ),
 ( #16359, #86346, #75755, #9092, #69029 ),
 ( #25868, #59512, #84684, #35397, #69585 ),
 ( #50003, #15799, #25314, #85232, #67371 ),
 ( #93624, #24757, #101470, #58955, #50558 ),
 ( #16902, #76299, #84137, #17456, #7982 ) ),
 .UNSPECIFIED., .F., .F., .F.,
 ( 6, 6 ),
 ( 5, 5 ),
 ( 0.000000000000000000, 111.1101480259999903 ),
 ( 25.81581217359999769, 39.03307591160000101 ),
 .UNSPECIFIED. ) ;
#78571 = CARTESIAN_POINT ( 'NONE',  ( 0.7574259850960020080, 1516.837969789639828, 212.3776558342370038 ) ) ;
#78572 = CARTESIAN_POINT ( 'NONE',  ( 14.22819488943649979, 1415.834070663119974, 197.0873419266759754 ) ) ;
#78573 = CARTESIAN_POINT ( 'NONE',  ( -2.854778372953739929, 1430.015594105409718, 207.6316838851879822 ) ) ;
#78574 = CARTESIAN_POINT ( 'NONE',  ( 6.124171326874999544, 1514.216129015430170, 201.4528617218270199 ) ) ;
#78575 = ORIENTED_EDGE ( 'NONE', *, *, #101841, .T. ) ;
#78576 = CARTESIAN_POINT ( 'NONE',  ( 13.91219551702819857, 1436.092364807330114, 150.2494214597319910 ) ) ;
#78577 = ORIENTED_EDGE ( 'NONE', *, *, #75537, .F. ) ;
#78578 = VERTEX_POINT ( 'NONE', #46820 ) ;
#78579 = ORIENTED_EDGE ( 'NONE', *, *, #9026, .F. ) ;
#78580 = CARTESIAN_POINT ( 'NONE',  ( 12.57924958998592402, 1445.046140314299691, 169.4707391365555793 ) ) ;
#78581 = CARTESIAN_POINT ( 'NONE',  ( -1.463875870539999902, 1465.932623932230172, 235.6053488212979801 ) ) ;
#78582 = CARTESIAN_POINT ( 'NONE',  ( 12.68313602754479952, 1500.389166761179922, 208.5581353062109997 ) ) ;
#78583 = CARTESIAN_POINT ( 'NONE',  ( -7.769371101339999974, 1384.910032728360193, 218.9178649038489937 ) ) ;
#78584 = CARTESIAN_POINT ( 'NONE',  ( -1.061334967899610016, 1465.179010130149891, 198.1705584392809953 ) ) ;
#78585 = AXIS2_PLACEMENT_3D ( 'NONE', #104525, #3201, #2645 ) ;
#78586 = CARTESIAN_POINT ( 'NONE',  ( 12.20373648401209898, 1421.751843755290110, 208.2739721469480116 ) ) ;
#78587 = CARTESIAN_POINT ( 'NONE',  ( -34.88314824369056311, 1379.640034327572494, 217.8691061211530382 ) ) ;
#78588 = CARTESIAN_POINT ( 'NONE',  ( 4.221461520009319734, 1446.221124511070002, 168.5615742123870291 ) ) ;
#78589 = AXIS2_PLACEMENT_3D ( 'NONE', #61475, #88311, #11604 ) ;
#78590 = CARTESIAN_POINT ( 'NONE',  ( 8.661166186259681155, 1437.607905750159944, 209.2119232992200182 ) ) ;
#78591 = ORIENTED_EDGE ( 'NONE', *, *, #17967, .F. ) ;
#78592 = CARTESIAN_POINT ( 'NONE',  ( -1.717084749545000122, 1516.819260244609950, 206.6456753351970121 ) ) ;
#78593 = ORIENTED_EDGE ( 'NONE', *, *, #28685, .T. ) ;
#78594 = CARTESIAN_POINT ( 'NONE',  ( 32.68061409889739366, 1440.913060387330006, 257.1432865577979783 ) ) ;
#78595 = DIRECTION ( 'NONE',  ( 0.000000000000000000, 1.000000000000000000, 0.000000000000000000 ) ) ;
#78596 = EDGE_LOOP ( 'NONE', ( #46781, #109657, #62594, #43752 ) ) ;
#78597 = CARTESIAN_POINT ( 'NONE',  ( -6.827666136118519802, 1508.551704606160001, 202.6664247900299927 ) ) ;
#78598 = CARTESIAN_POINT ( 'NONE',  ( -14.07231417549999897, 1409.404476426829888, 191.3682123889980176 ) ) ;
#78599 = CARTESIAN_POINT ( 'NONE',  ( -34.18677586421195258, 1522.382868172863937, 198.4504086008750505 ) ) ;
#78600 = CARTESIAN_POINT ( 'NONE',  ( -11.01884469515209908, 1414.913527275050001, 195.9427818023129930 ) ) ;
#78601 = CARTESIAN_POINT ( 'NONE',  ( -0.8109757519344622523, 1455.440442885683069, 218.5281743464129534 ) ) ;
#78602 = CARTESIAN_POINT ( 'NONE',  ( -2.372478608332516892, 1522.382868172863937, 174.8996806668726549 ) ) ;
#78603 = CARTESIAN_POINT ( 'NONE',  ( 0.000000000000000000, 1389.913060387289988, 209.1218459616989946 ) ) ;
#78604 = CARTESIAN_POINT ( 'NONE',  ( -4.372755355000000677, 1508.294786316789896, 220.5537717656990253 ) ) ;
#78606 = CARTESIAN_POINT ( 'NONE',  ( 8.534313171132479781, 1434.919546690739935, 206.3689509244539693 ) ) ;
#78605 = CARTESIAN_POINT ( 'NONE',  ( -11.16643434163729864, 1471.372555858320084, 206.7508257846899937 ) ) ;
#78607 = AXIS2_PLACEMENT_3D ( 'NONE', #29850, #39910, #55636 ) ;
#78608 = B_SPLINE_SURFACE_WITH_KNOTS ( 'NONE', 5, 5, ( 
 ( #17956, #59456, #77891, #36429, #35332, #19056, #16841, #61128, #649, #68413, #1199, #104741, #93566, #25807, #94126, #78445, #77347, #27474, #43195, #102516, #60005, #18505, #1759, #52703 ),
 ( #51043, #17397, #34780, #86837, #10130, #35897, #53260, #10694, #53825, #21801, #72806, #87964, #2855, #20172, #11253, #106395, #81179, #45413, #80645, #19623, #20709, #12876, #38086, #71172 ),
 ( #56001, #46511, #47055, #54369, #29135, #90125, #28585, #105294, #4495, #38628, #64410, #63862, #97978, #28030, #72262, #80088, #62786, #96901, #3408, #47595, #3959, #81722, #98533, #63324 ),
 ( #88499, #79557, #13408, #29678, #106933, #21244, #5029, #30222, #11783, #39173, #62219, #12322, #73349, #36978, #45950, #96346, #37538, #89585, #71740, #105857, #97444, #54908, #89032, #55457 ),
 ( #41402, #90681, #100726, #92890, #99622, #108032, #13969, #32976, #57116, #75569, #91242, #50368, #109163, #109702, #15604, #92332, #49260, #41950, #15061, #101263, #84494, #6684, #82834, #83941 ),
 ( #14521, #40839, #31328, #67166, #75013, #48712, #6126, #74467, #91785, #23479, #73906, #64958, #32449, #7784, #24010, #58751, #24562, #39740, #30779, #16165, #22908, #66625, #58204, #49810 ) ),
 .UNSPECIFIED., .F., .F., .F.,
 ( 6, 6 ),
 ( 6, 3, 3, 3, 3, 3, 3, 6 ),
 ( 52.54788734150000096, 99.04053960890000496 ),
 ( 27.66747964320000008, 34.02592213510000363, 36.52949902339999966, 37.78128746749999323, 38.40718168960000156, 39.03307591160000101, 39.70872026930000231, 40.38436462709999830 ),
 .UNSPECIFIED. ) ;
#78609 = CARTESIAN_POINT ( 'NONE',  ( 1.132949076425000090, 1516.693851263360102, 214.1195642086070166 ) ) ;
#78610 = CARTESIAN_POINT ( 'NONE',  ( 22.90250716390000107, 1409.721554320030009, 209.3445813094469941 ) ) ;
#78611 = CARTESIAN_POINT ( 'NONE',  ( 5.762402162469949296, 1511.083508941950186, 216.8055985269170094 ) ) ;
#78612 = ADVANCED_FACE ( 'NONE', ( #70934 ), #67025, .F. ) ;
#78613 = CARTESIAN_POINT ( 'NONE',  ( -18.31941652021487954, 1517.151704408390060, 214.4156261991469421 ) ) ;
#78614 = CARTESIAN_POINT ( 'NONE',  ( 3.461995158685000185, 1516.906233342200039, 211.9877574868770012 ) ) ;
#78615 = CARTESIAN_POINT ( 'NONE',  ( 15.06903345039999920, 1410.389868239730049, 191.5311856341979819 ) ) ;
#78616 = CARTESIAN_POINT ( 'NONE',  ( 29.91204167771608269, 1525.042412244735488, 222.1820579943630776 ) ) ;
#78618 = ORIENTED_EDGE ( 'NONE', *, *, #14249, .T. ) ;
#78617 = CARTESIAN_POINT ( 'NONE',  ( -97.51726726849999238, 1390.553429058280017, 303.6087006878590273 ) ) ;
#78619 = CARTESIAN_POINT ( 'NONE',  ( -16.94363731710831189, 1525.231909165016305, 236.8652039782725751 ) ) ;
#78620 = CIRCLE ( 'NONE', #107221, 0.9999999999999976685 ) ;
#78621 = CARTESIAN_POINT ( 'NONE',  ( 29.66529950099999624, 1450.991311272329767, 244.2516413617979936 ) ) ;
#78622 = EDGE_CURVE ( 'NONE', #84204, #100346, #53124, .T. ) ;
#78623 = CARTESIAN_POINT ( 'NONE',  ( -7.548380910495000151, 1510.399296111369949, 213.9269235281369959 ) ) ;
#78624 = CARTESIAN_POINT ( 'NONE',  ( -3.665607323393529793, 1507.166784210740161, 236.6858246876950034 ) ) ;
#78625 = CARTESIAN_POINT ( 'NONE',  ( -20.99439929950000305, 1454.025623455230061, 225.3869460595979888 ) ) ;
#78627 = CARTESIAN_POINT ( 'NONE',  ( 17.82217580153020009, 1410.175561989269909, 222.8366056556930062 ) ) ;
#78626 = CARTESIAN_POINT ( 'NONE',  ( 11.30788561520000002, 1432.726986962210049, 151.5212569857980327 ) ) ;
#78628 = CARTESIAN_POINT ( 'NONE',  ( 0.2728724028810000091, 1488.801231226530035, 187.6229463501980206 ) ) ;
#78629 = CARTESIAN_POINT ( 'NONE',  ( -105.6749141713339952, 1378.070069343479872, 305.5932407599049725 ) ) ;
#78630 = ORIENTED_EDGE ( 'NONE', *, *, #29302, .F. ) ;
#78631 = CARTESIAN_POINT ( 'NONE',  ( -7.333070173014999860, 1516.955859323880077, 203.3428461583270064 ) ) ;
#78632 = CARTESIAN_POINT ( 'NONE',  ( 1.810797400909999994E-09, 1405.989059426729909, 266.9611530680980422 ) ) ;
#78633 = DIRECTION ( 'NONE',  ( 1.000000000000000000, 0.000000000000000000, 0.000000000000000000 ) ) ;
#78634 = CARTESIAN_POINT ( 'NONE',  ( 18.82307291165939844, 1468.777348105939836, 269.3734094525160572 ) ) ;
#78635 = CARTESIAN_POINT ( 'NONE',  ( 5.386772287290000349, 1432.443201990170110, 154.6097844173980036 ) ) ;
#78636 = CARTESIAN_POINT ( 'NONE',  ( -27.13948102820610231, 1449.857017199720076, 136.5863992428030258 ) ) ;
#78637 = CARTESIAN_POINT ( 'NONE',  ( -0.4530963034073862139, 1469.489877109852841, 219.1639567478746642 ) ) ;
#78638 = CARTESIAN_POINT ( 'NONE',  ( -44.14497367832510122, 1440.913060404099951, 264.5199370315700094 ) ) ;
#78639 = AXIS2_PLACEMENT_3D ( 'NONE', #55415, #82799, #30742 ) ;
#78640 = CARTESIAN_POINT ( 'NONE',  ( 36.08172904959410232, 1449.985944480599983, 136.2472095414419755 ) ) ;
#78641 = DIRECTION ( 'NONE',  ( 0.000000000000000000, -0.9990482215818579093, 0.04361938736533144123 ) ) ;
#78642 = CARTESIAN_POINT ( 'NONE',  ( 0.08548078369580100477, 1431.416326821289886, 200.5909471841690106 ) ) ;
#78643 = CARTESIAN_POINT ( 'NONE',  ( 2.491511751652589979, 1449.258137923909999, 154.2481093066819824 ) ) ;
#78644 = CARTESIAN_POINT ( 'NONE',  ( 3.648450305909999525, 1506.945872735989951, 220.2261833973989837 ) ) ;
#78645 =( BOUNDED_CURVE ( )  B_SPLINE_CURVE ( 3, ( #72911, #98641, #45530, #64527 ),
 .UNSPECIFIED., .F., .T. ) 
 B_SPLINE_CURVE_WITH_KNOTS ( ( 4, 4 ),
 ( 4.164116178399805079, 5.260656259123209999 ),
 .UNSPECIFIED. ) 
 CURVE ( )  GEOMETRIC_REPRESENTATION_ITEM ( )  RATIONAL_B_SPLINE_CURVE ( ( 1.000000000000000000, 0.9022849824783407691, 0.9022849824783407691, 1.000000000000000000 ) ) 
 REPRESENTATION_ITEM ( '' )  );
#78646 = CARTESIAN_POINT ( 'NONE',  ( 2.487935084889999704, 1508.551704408389924, 214.1089244042930204 ) ) ;
#78647 = ORIENTED_EDGE ( 'NONE', *, *, #58040, .T. ) ;
#78648 = AXIS2_PLACEMENT_3D ( 'NONE', #101492, #50026, #41620 ) ;
#78649 = CARTESIAN_POINT ( 'NONE',  ( -39.48812356999999906, 1431.587789824249967, 268.3665355199980240 ) ) ;
#78650 = CARTESIAN_POINT ( 'NONE',  ( -0.003583650733678669757, 1485.228942655789979, 198.2304589643989630 ) ) ;
#78651 = CARTESIAN_POINT ( 'NONE',  ( 9.903675653824370428, 1469.012720000510171, 207.5205053474399790 ) ) ;
#78652 = CARTESIAN_POINT ( 'NONE',  ( -0.6528690470989999550, 1417.364746825729981, 235.5198400807980192 ) ) ;
#78653 = CARTESIAN_POINT ( 'NONE',  ( -4.249354323605699868, 1446.471035334290036, 161.2178408973400110 ) ) ;
#78654 = CARTESIAN_POINT ( 'NONE',  ( -30.31404213106243617, 1524.330813522192102, 196.4516891724783534 ) ) ;
#78655 = CARTESIAN_POINT ( 'NONE',  ( 7.729485065020000434, 1423.503497352910017, 212.7167255717090200 ) ) ;
#78656 = CARTESIAN_POINT ( 'NONE',  ( -22.14384457810140105, 1384.855528056009916, 221.9556210832379861 ) ) ;
#78657 = CIRCLE ( 'NONE', #30368, 1.999999999999999556 ) ;
#78658 = CARTESIAN_POINT ( 'NONE',  ( -18.72518989680000345, 1416.274718422629803, 208.3778101247369818 ) ) ;
#78659 = CARTESIAN_POINT ( 'NONE',  ( 11.87399071922619953, 1432.929227292529959, 149.9807480848299974 ) ) ;
#78660 = CARTESIAN_POINT ( 'NONE',  ( 26.61739034963180117, 1435.433209610839867, 135.4670460917660080 ) ) ;
#78661 = CARTESIAN_POINT ( 'NONE',  ( -12.53380499169999851, 1445.052233488290085, 169.4755105685979970 ) ) ;
#78662 = EDGE_LOOP ( 'NONE', ( #83917, #38562, #63102, #92340, #25512, #90064, #5430, #85883, #107116 ) ) ;
#78663 = CARTESIAN_POINT ( 'NONE',  ( -17.27769651085920088, 1410.881435910499931, 225.9445911753860230 ) ) ;
#78664 = DIRECTION ( 'NONE',  ( 1.755985294532469921E-16, -1.000000000000000000, 1.338183447452831989E-16 ) ) ;
#78665 = EDGE_LOOP ( 'NONE', ( #58546, #99736, #26591, #62865 ) ) ;
#78666 = CARTESIAN_POINT ( 'NONE',  ( -2.600041615418440255, 1436.399642545620054, 227.4320274269610138 ) ) ;
#78667 = LINE ( 'NONE', #8136, #59983 ) ;
#78668 = LINE ( 'NONE', #96014, #28518 ) ;
#78670 = CARTESIAN_POINT ( 'NONE',  ( -2.409860608258060033, 1457.727041476990053, 219.5092956769670138 ) ) ;
#78669 = DIRECTION ( 'NONE',  ( 1.000000000000000000, 0.000000000000000000, 0.000000000000000000 ) ) ;
#78671 = CARTESIAN_POINT ( 'NONE',  ( 0.1892422376850020072, 1450.986474787589941, 189.9359345321989849 ) ) ;
#78672 = CARTESIAN_POINT ( 'NONE',  ( -9.811963572550000734, 1449.015260455689940, 207.4086770326589999 ) ) ;
#78673 = CIRCLE ( 'NONE', #101900, 3678.960170865509554 ) ;
#78674 = CARTESIAN_POINT ( 'NONE',  ( 3.454172615424999648, 1517.122088787240045, 201.3974225380069925 ) ) ;
#78675 = CARTESIAN_POINT ( 'NONE',  ( 7.661576622320000141, 1424.780314478109858, 211.9949546932489852 ) ) ;
#78676 = CARTESIAN_POINT ( 'NONE',  ( -17.65532971150000208, 1419.497219977419945, 207.2321558962389929 ) ) ;
#78677 = DIRECTION ( 'NONE',  ( -4.440892098500627739E-15, 0.000000000000000000, -1.000000000000000000 ) ) ;
#78678 = CARTESIAN_POINT ( 'NONE',  ( 7.599119408734999581, 1512.336926113599930, 206.7298288840769942 ) ) ;
#78679 = CARTESIAN_POINT ( 'NONE',  ( 2.863305601979999615, 1449.090055474780002, 183.5657516826979929 ) ) ;
#78680 = CARTESIAN_POINT ( 'NONE',  ( 8.808043405595423536, 1365.554312915578294, 207.6218459616988241 ) ) ;
#78682 = ORIENTED_EDGE ( 'NONE', *, *, #48069, .F. ) ;
#78681 = CARTESIAN_POINT ( 'NONE',  ( 6.446188137380000072, 1454.172846498590161, 216.1779746046189814 ) ) ;
#78683 = ORIENTED_EDGE ( 'NONE', *, *, #6527, .F. ) ;
#78684 = CARTESIAN_POINT ( 'NONE',  ( -40.71170020219999941, 1443.968826064090081, 137.1159894999980224 ) ) ;
#78685 = EDGE_CURVE ( 'NONE', #76272, #16145, #4817, .T. ) ;
#78686 = CARTESIAN_POINT ( 'NONE',  ( 1.146809930359999896, 1466.701590537929860, 235.3106089818980138 ) ) ;
#78687 = CARTESIAN_POINT ( 'NONE',  ( 0.2538829723067779764, 1420.503732877419907, 182.7635795570130028 ) ) ;
#78688 = DIRECTION ( 'NONE',  ( -1.755985294532469921E-16, 1.000000000000000000, -1.338183447452831989E-16 ) ) ;
#78689 = CARTESIAN_POINT ( 'NONE',  ( -3.526834439349999961, 1486.375772999530000, 181.8601271665980050 ) ) ;
#78690 = AXIS2_PLACEMENT_3D ( 'NONE', #30334, #47704, #23023 ) ;
#78692 = ADVANCED_FACE ( 'NONE', ( #83154 ), #85677, .F. ) ;
#78691 = CARTESIAN_POINT ( 'NONE',  ( -32.05702909905236453, 1524.477587234266139, 201.5541149372814402 ) ) ;
#78693 = DIRECTION ( 'NONE',  ( 1.755985294532469921E-16, -1.000000000000000000, 1.338183447452831989E-16 ) ) ;
#78694 = CARTESIAN_POINT ( 'NONE',  ( -34.99243995798710216, 1450.827641384700200, 136.1403221839539981 ) ) ;
#78695 = EDGE_CURVE ( 'NONE', #6800, #44714, #6656, .T. ) ;
#78696 = SURFACE_STYLE_USAGE ( .BOTH. , #97695 ) ;
#78697 = CARTESIAN_POINT ( 'NONE',  ( 33.93525352000410322, 1435.841465267310014, 135.9408836255369977 ) ) ;
#78698 = CARTESIAN_POINT ( 'NONE',  ( 32.64368752077381686, 1435.637503394754049, 135.1055172344166522 ) ) ;
#78699 = CARTESIAN_POINT ( 'NONE',  ( -0.01096400588092319960, 1407.225809178260079, 196.1218459624460024 ) ) ;
#78700 = DIRECTION ( 'NONE',  ( -0.2342910579933019377, -0.2476038117450569398, -0.9401064049104748133 ) ) ;
#78701 = CARTESIAN_POINT ( 'NONE',  ( -11.20854089327220038, 1414.996442620800053, 195.7122650692939771 ) ) ;
#78702 = VERTEX_POINT ( 'NONE', #22654 ) ;
#78703 = CARTESIAN_POINT ( 'NONE',  ( -10.96917002040000000, 1432.328099320269985, 151.7701195717980056 ) ) ;
#78704 = CARTESIAN_POINT ( 'NONE',  ( 13.49481936589999975, 1445.992738435850015, 188.9449086255979751 ) ) ;
#78705 = B_SPLINE_SURFACE_WITH_KNOTS ( 'NONE', 5, 5, ( 
 ( #31484, #99782, #65665, #101422, #83000, #6293, #40440, #68429, #16858 ),
 ( #86854, #95261, #8478, #17413, #104209, #1215, #35350, #69537, #85744 ),
 ( #34246, #103657, #26956, #60580, #18522, #9042, #2334, #27496, #61146 ),
 ( #86302, #60024, #102531, #17975, #43215, #1776, #52719, #94700, #79033 ),
 ( #77364, #52171, #10146, #61683, #68984, #26385, #10711, #9586, #76806 ),
 ( #103085, #94142, #95806, #25823, #34796, #44319, #43757, #51610, #70096 ),
 ( #78463, #36446, #51062, #53277, #77909, #665, #35913, #19073, #87416 ),
 ( #44883, #101985, #25271, #59472, #93582, #85192, #42652, #122, #53844 ),
 ( #71190, #96921, #72280, #28604, #28046, #105312, #38645, #90141, #54386 ) ),
 .UNSPECIFIED., .F., .F., .F.,
 ( 6, 3, 6 ),
 ( 6, 3, 6 ),
 ( 5.472486514890000819, 9.497846738619999840, 12.82121481780000138 ),
 ( 0.000000000000000000, 1.000000000000000000, 2.000000000000000000 ),
 .UNSPECIFIED. ) ;
#78706 = ORIENTED_EDGE ( 'NONE', *, *, #82080, .F. ) ;
#78707 = ORIENTED_EDGE ( 'NONE', *, *, #97972, .T. ) ;
#78708 = CARTESIAN_POINT ( 'NONE',  ( -3.821721059369999729, 1454.437606006089936, 200.1305965264490112 ) ) ;
#78709 = CARTESIAN_POINT ( 'NONE',  ( -5.986709854369999917, 1361.264879806939916, 207.6218459616989946 ) ) ;
#78710 = CARTESIAN_POINT ( 'NONE',  ( 7.334328272665000092, 1517.005755693489846, 214.1256940922069987 ) ) ;
#78711 = CARTESIAN_POINT ( 'NONE',  ( 3.077691717124999560, 1511.730395268069969, 216.9250477754170277 ) ) ;
#78712 = ORIENTED_EDGE ( 'NONE', *, *, #45494, .F. ) ;
#78713 = CARTESIAN_POINT ( 'NONE',  ( -94.35247987469999487, 1379.531630663759870, 302.8771378034590498 ) ) ;
#78714 = CARTESIAN_POINT ( 'NONE',  ( 7.747670780530000023, 1416.518938592030054, 225.7538447804980137 ) ) ;
#78715 = CARTESIAN_POINT ( 'NONE',  ( -3.263521942484999716, 1516.676340709600026, 203.3494421577970002 ) ) ;
#78716 = CARTESIAN_POINT ( 'NONE',  ( 5.343479918049999888, 1396.099658817830004, 218.7752541424879951 ) ) ;
#78717 = B_SPLINE_SURFACE_WITH_KNOTS ( 'NONE', 5, 5, ( 
 ( #58852, #23575, #92984, #66717, #101360, #58302 ),
 ( #25212, #16798, #92424, #84585, #6771, #15160 ),
 ( #100823, #43154, #85133, #8420, #102480, #7876 ),
 ( #51002, #15699, #24650, #101926, #42044, #76196 ),
 ( #84037, #25769, #40935, #49902, #100294, #57768 ),
 ( #7335, #42592, #57, #76745, #34188, #59968 ),
 ( #94083, #17353, #49351, #41499, #51548, #85685 ),
 ( #8982, #75113, #77310, #608, #35855, #70583 ),
 ( #19016, #18463, #95202, #36939, #1716, #52660 ) ),
 .UNSPECIFIED., .F., .F., .F.,
 ( 6, 3, 6 ),
 ( 6, 6 ),
 ( 13.59708442930000061, 23.84265563570000168, 33.33692106499999852 ),
 ( 0.000000000000000000, 2.000000000000000000 ),
 .UNSPECIFIED. ) ;
#78718 = CARTESIAN_POINT ( 'NONE',  ( -106.7752590979999923, 1385.237353006989906, 297.1314966531590471 ) ) ;
#78719 = CARTESIAN_POINT ( 'NONE',  ( -53.13991455628549687, 1384.634500711259989, 230.4819378445650102 ) ) ;
#78720 = CARTESIAN_POINT ( 'NONE',  ( -0.01010286742719850028, 1516.939452820819952, 201.4022050290969901 ) ) ;
#78721 = CARTESIAN_POINT ( 'NONE',  ( -5.667817220899999953, 1409.110984927429854, 230.5553178883980081 ) ) ;
#78722 = CIRCLE ( 'NONE', #71046, 1.999999999999999556 ) ;
#78724 = ORIENTED_EDGE ( 'NONE', *, *, #5669, .T. ) ;
#78723 = CARTESIAN_POINT ( 'NONE',  ( -9.116846773499998946, 1445.598699692060109, 184.9636421048979855 ) ) ;
#78725 = CARTESIAN_POINT ( 'NONE',  ( 29.24087330780000116, 1451.891771913630237, 134.8528131887979953 ) ) ;
#78726 = CARTESIAN_POINT ( 'NONE',  ( 11.02433906870393265, 1425.200908241132538, 139.1360266714638101 ) ) ;
#78727 = CARTESIAN_POINT ( 'NONE',  ( 21.03150544155480262, 1507.789100631340261, 226.0652199028830012 ) ) ;
#78728 = CARTESIAN_POINT ( 'NONE',  ( 17.02668221408760019, 1422.112876149069962, 226.8213126862850118 ) ) ;
#78729 = CARTESIAN_POINT ( 'NONE',  ( -24.32488869200000181, 1435.346926706200065, 136.3493805836980073 ) ) ;
#78731 = CARTESIAN_POINT ( 'NONE',  ( 1.135460316954999938, 1516.790374942449944, 212.3751473514870156 ) ) ;
#78730 = AXIS2_PLACEMENT_3D ( 'NONE', #24688, #66207, #23611 ) ;
#78732 = CARTESIAN_POINT ( 'NONE',  ( -67.70136529139999482, 1379.745769832329870, 277.8225302446590490 ) ) ;
#78733 = CARTESIAN_POINT ( 'NONE',  ( -109.9849726248329915, 1384.916895159399928, 311.4561123681800154 ) ) ;
#78734 = CARTESIAN_POINT ( 'NONE',  ( -30.44069153017106544, 1525.425686270225015, 221.4734925813270081 ) ) ;
#78735 = CARTESIAN_POINT ( 'NONE',  ( 24.11200303724299943, 1496.633659200180091, 206.8275310043889874 ) ) ;
#78736 = CARTESIAN_POINT ( 'NONE',  ( 7.337297311985000015, 1517.135701590510052, 209.8615382079770200 ) ) ;
#78737 = EDGE_LOOP ( 'NONE', ( #105436, #51075, #47998, #76498 ) ) ;
#78738 = CARTESIAN_POINT ( 'NONE',  ( 2.500000000000000000, 1432.302110539269961, 157.4936333739979943 ) ) ;
#78739 = CARTESIAN_POINT ( 'NONE',  ( -0.6620138580789999283, 1412.846677813530050, 233.2438720524980056 ) ) ;
#78740 = CARTESIAN_POINT ( 'NONE',  ( -32.09555170170000338, 1384.821019989420165, 229.9571600258589967 ) ) ;
#78741 = EDGE_LOOP ( 'NONE', ( #23297, #45964, #89977 ) ) ;
#78742 = DIRECTION ( 'NONE',  ( 0.4990868182759217730, -0.2476038119106064028, -0.8304244096548186738 ) ) ;
#78743 = DIRECTION ( 'NONE',  ( -0.6736849260863841948, 0.000000000000000000, 0.7390186874254148774 ) ) ;
#78744 = CARTESIAN_POINT ( 'NONE',  ( 12.12754418595840100, 1433.981883138469811, 149.9562185505259890 ) ) ;
#78745 = EDGE_CURVE ( 'NONE', #21185, #86873, #72364, .T. ) ;
#78746 = CARTESIAN_POINT ( 'NONE',  ( 15.49878809011119962, 1469.005027229599818, 230.0777613073749706 ) ) ;
#78747 = CARTESIAN_POINT ( 'NONE',  ( -25.23663147221330050, 1509.794343225200009, 222.8844807554229988 ) ) ;
#78748 = CARTESIAN_POINT ( 'NONE',  ( -2.644001908849999971, 1409.509886481130025, 186.7831889129979857 ) ) ;
#78749 = PLANE ( 'NONE',  #34075 ) ;
#78750 = CARTESIAN_POINT ( 'NONE',  ( -0.01543823104247980284, 1420.444145791279880, 182.6744822797599852 ) ) ;
#78751 = CIRCLE ( 'NONE', #57289, 3678.960196675449879 ) ;
#78753 = DIRECTION ( 'NONE',  ( 0.7059212408186743559, 0.02465132495770355758, 0.7078612250567569708 ) ) ;
#78752 = CARTESIAN_POINT ( 'NONE',  ( -6.552897405075000847, 1516.858146885269889, 215.6784973415170157 ) ) ;
#78754 = CARTESIAN_POINT ( 'NONE',  ( 19.65556712749999946, 1509.582207825729938, 187.2736428280979908 ) ) ;
#78755 = CARTESIAN_POINT ( 'NONE',  ( -5.360152366205530150, 1422.242722016050038, 144.1549655170190078 ) ) ;
#78756 = ORIENTED_EDGE ( 'NONE', *, *, #42604, .F. ) ;
#78757 = CARTESIAN_POINT ( 'NONE',  ( -11.74757148147149977, 1414.971390223329990, 197.2503777628510022 ) ) ;
#78758 = CARTESIAN_POINT ( 'NONE',  ( 3.451191875628180750, 1523.678648413191695, 175.1707361340005207 ) ) ;
#78759 = EDGE_LOOP ( 'NONE', ( #83238, #85276, #13543, #57457 ) ) ;
#78760 = CARTESIAN_POINT ( 'NONE',  ( 11.75869035672759999, 1519.551704408389924, 227.2994842695800060 ) ) ;
#78761 = B_SPLINE_CURVE_WITH_KNOTS ( 'NONE', 3,
 ( #35942, #47641, #72310, #90169, #12917, #82340 ),
 .UNSPECIFIED., .F., .F.,
 ( 4, 2, 4 ),
 ( 1.040834085586084257E-17, 0.001087661325621735488, 0.002175322651243460567 ),
 .UNSPECIFIED. ) ;
#78762 = CARTESIAN_POINT ( 'NONE',  ( 10.15354923512214036, 1435.473398722268257, 152.3868440969227152 ) ) ;
#78763 = CARTESIAN_POINT ( 'NONE',  ( 7.920874050670489552, 1511.346048414110101, 203.4159230979989843 ) ) ;
#78764 = CARTESIAN_POINT ( 'NONE',  ( 2.924270561990000239, 1442.750123219389934, 217.5134303114490137 ) ) ;
#78765 = CARTESIAN_POINT ( 'NONE',  ( -34.61172972909721324, 1523.342713519622976, 200.0387150244875443 ) ) ;
#78766 = CARTESIAN_POINT ( 'NONE',  ( 1829.302631503766179, 11216.44053380570585, 1606.259476111525828 ) ) ;
#78767 = AXIS2_PLACEMENT_3D ( 'NONE', #958, #41286, #17139 ) ;
#78768 = CARTESIAN_POINT ( 'NONE',  ( -2.500000001370000113, 1448.248591364029835, 156.2049463022979978 ) ) ;
#78769 = CARTESIAN_POINT ( 'NONE',  ( -18.59208672289999953, 1425.224709566930187, 227.1497469740980080 ) ) ;
#78770 = CARTESIAN_POINT ( 'NONE',  ( -19.43950658530000197, 1435.604459603690202, 145.6038571952979908 ) ) ;
#78771 = CARTESIAN_POINT ( 'NONE',  ( -5.402270704262029710, 1464.396980422829984, 199.5157612532009921 ) ) ;
#78772 = DIRECTION ( 'NONE',  ( -5.980589973904019347E-17, 1.000000000000000000, -1.736889445713099699E-16 ) ) ;
#78774 = CARTESIAN_POINT ( 'NONE',  ( 1.600048698852036821, 1401.254281879943164, 137.0999999980979851 ) ) ;
#78773 = CARTESIAN_POINT ( 'NONE',  ( -111.9617233841873940, 1305.913060387289988, 301.5890982715878863 ) ) ;
#78775 = LINE ( 'NONE', #104523, #40316 ) ;
#78776 = ORIENTED_EDGE ( 'NONE', *, *, #33035, .T. ) ;
#78777 = CARTESIAN_POINT ( 'NONE',  ( 0.5987183461865049905, 1507.212886145319999, 186.4932301926239688 ) ) ;
#78778 = CARTESIAN_POINT ( 'NONE',  ( -112.0992599419676452, 1391.413060387289988, 306.3568108987562937 ) ) ;
#78779 = ADVANCED_FACE ( 'NONE', ( #65816 ), #83981, .T. ) ;
#78780 = CARTESIAN_POINT ( 'NONE',  ( -11.91180745165941879, 1433.366507474078617, 149.9330222961037009 ) ) ;
#78781 = CARTESIAN_POINT ( 'NONE',  ( -1.835776439160000217, 1484.769563154189882, 198.4308762110990187 ) ) ;
#78782 = B_SPLINE_CURVE_WITH_KNOTS ( 'NONE', 3,
 ( #5261, #6906, #99297, #91475, #39414, #15829, #65186, #50032, #14198, #73591, #41063, #32667, #38849, #31006, #75240, #4706, #73028, #22572, #13631, #57350, #98763, #22024, #66845, #58431, #109390, #48385, #56776, #92559, #82527 ),
 .UNSPECIFIED., .F., .F.,
 ( 4, 2, 2, 1, 1, 2, 2, 2, 2, 2, 2, 2, 1, 2, 2, 4 ),
 ( 0.000000000000000000, 0.1250000000005312417, 0.1875000000007969181, 0.2187500000009944268, 0.2343750000010931256, 0.2421875000011424472, 0.2500000000011917689, 0.3750000000012347345, 0.4375000000011303736, 0.5000000000010259571, 0.6250000000013459234, 0.6875000000015057955, 0.7187500000017689183, 0.7343750000019237945, 0.7500000000020786706, 1.000000000000000000 ),
 .UNSPECIFIED. ) ;
#78783 = CARTESIAN_POINT ( 'NONE',  ( -18.62830157129999620, 1508.852446407129946, 229.9890140626980042 ) ) ;
#78784 = CARTESIAN_POINT ( 'NONE',  ( -3.511054680705768316, 1426.007948959481382, 185.8822184451843498 ) ) ;
#78785 = CARTESIAN_POINT ( 'NONE',  ( -16.19492410612830113, 1409.478599598990058, 194.0661808939520085 ) ) ;
#78786 = CARTESIAN_POINT ( 'NONE',  ( -25.00976051679999657, 1436.598010167069788, 137.9330532114979917 ) ) ;
#78787 = CARTESIAN_POINT ( 'NONE',  ( -8.864783858735460598, 1488.500646863400107, 216.8084363924249942 ) ) ;
#78788 = CARTESIAN_POINT ( 'NONE',  ( 19.38664720319999901, 1498.811923108090014, 221.8202413673990065 ) ) ;
#78789 = CARTESIAN_POINT ( 'NONE',  ( -97.83732743130200049, 1383.765384414209848, 310.3688010583850314 ) ) ;
#78790 = CARTESIAN_POINT ( 'NONE',  ( -109.2723729720279948, 1384.466068673930067, 311.2384636710350492 ) ) ;
#78791 = CARTESIAN_POINT ( 'NONE',  ( -4.993214567250789493, 1391.653935164599716, 214.7089805434449943 ) ) ;
#78792 = CARTESIAN_POINT ( 'NONE',  ( -2.100767134424469607, 1516.527474870850256, 201.4129930513860245 ) ) ;
#78794 = ORIENTED_EDGE ( 'NONE', *, *, #14745, .F. ) ;
#78793 = CARTESIAN_POINT ( 'NONE',  ( 23.24537980070000032, 1509.679808356930153, 191.7928441131979866 ) ) ;
#78795 = CARTESIAN_POINT ( 'NONE',  ( -18.20051592215423142, 1459.364021588609603, 227.8976272857560730 ) ) ;
#78796 = AXIS2_PLACEMENT_3D ( 'NONE', #45906, #35278, #1698 ) ;
#78797 = CARTESIAN_POINT ( 'NONE',  ( -66.86281825880000440, 1379.216504766910020, 275.7591398340589990 ) ) ;
#78798 = CARTESIAN_POINT ( 'NONE',  ( 20.15304608505310213, 1509.294231923400048, 229.9324461821670127 ) ) ;
#78799 = ORIENTED_EDGE ( 'NONE', *, *, #23975, .F. ) ;
#78800 = ORIENTED_EDGE ( 'NONE', *, *, #41570, .T. ) ;
#78801 = CARTESIAN_POINT ( 'NONE',  ( 19.77970829033609945, 1507.818029077260007, 229.2755469930129948 ) ) ;
#78802 = CARTESIAN_POINT ( 'NONE',  ( -15.93619147924319890, 1463.426196661189806, 221.8456080550549814 ) ) ;
#78803 = CARTESIAN_POINT ( 'NONE',  ( 13.14149025202757670, 1443.060851088390791, 169.3996772419945103 ) ) ;
#78805 = CARTESIAN_POINT ( 'NONE',  ( -6.814834796379999560, 1474.725719091730070, 264.8986983612979884 ) ) ;
#78804 = FACE_OUTER_BOUND ( 'NONE', #37924, .T. ) ;
#78806 = B_SPLINE_CURVE_WITH_KNOTS ( 'NONE', 3,
 ( #14962, #46961, #39066, #73245, #5481, #97873, #56448, #4398, #21148, #40185, #55355, #81081, #64313, #47497, #89488, #90027, #38526, #13860, #63760, #98976, #57010, #12783, #31231, #72703, #73810, #23374, #30681, #55909, #72172, #48607, #106828, #22804, #4924, #30118, #98432, #107385, #22250, #21704, #99519, #13304, #65967, #106290, #91138, #57565, #48044, #49157, #31780, #90580, #14415, #82183, #83289, #6587, #60308, #23911, #50265, #84926, #8219, #92787, #84394, #86047, #26118 ),
 .UNSPECIFIED., .F., .F.,
 ( 4, 3, 3, 3, 3, 3, 3, 3, 3, 3, 3, 3, 3, 3, 3, 3, 3, 3, 3, 3, 4 ),
 ( 7.020647373213010134, 7.318242487455970391, 7.663999848964880179, 7.934526232592060246, 8.156304087536639713, 8.278825267203739457, 8.449185380093728881, 8.482857723717689424, 8.514868418927969529, 8.765148280566069872, 9.022911409362329493, 9.297145710536121044, 9.587002469640040658, 9.900769533069599504, 10.04480025696140011, 10.11612467641749902, 10.52133809873689962, 10.85847357495339871, 11.00458707344359865, 11.32809206207529940, 11.65159705070689888 ),
 .UNSPECIFIED. ) ;
#78807 = DIRECTION ( 'NONE',  ( 0.8090169943747088643, 0.000000000000000000, 0.5877852522928015411 ) ) ;
#78808 = B_SPLINE_CURVE_WITH_KNOTS ( 'NONE', 3,
 ( #107297, #3769, #63676, #13215, #97787, #21063, #81527, #73722, #39547, #22707, #56905, #88849, #98342, #38975, #38431, #74273, #90489, #40091, #30025, #20514, #4829, #37903, #89400, #46869, #12688, #28950, #72607, #63139, #97240, #30591, #54722, #72084, #98889, #4304, #91038, #31134, #46326, #21615, #64218, #14325, #82654, #22157, #73153, #56357, #48515, #13764, #5946, #47948, #12134, #80997, #82088, #106737, #5390, #107845, #65319 ),
 .UNSPECIFIED., .F., .F.,
 ( 4, 3, 3, 3, 3, 3, 3, 3, 3, 3, 3, 3, 3, 3, 3, 3, 3, 3, 4 ),
 ( 9.902195898209999569, 10.17210527304969858, 10.45530577765890001, 10.70141353110000004, 11.00396970312500144, 11.32322756693239896, 11.52456852350000105, 11.84989040643209890, 12.16242387753359999, 12.38020728900000123, 12.74551463662050033, 13.12275145103740037, 13.53252099862019975, 13.95359103776459975, 14.40783883235129892, 14.91487510228819957, 15.44821056779149870, 15.94145638527190023, 16.40090783169999966 ),
 .UNSPECIFIED. ) ;
#78809 = CARTESIAN_POINT ( 'NONE',  ( -107.2362392430000000, 1382.245772082230133, 298.1239918761589820 ) ) ;
#78810 = CARTESIAN_POINT ( 'NONE',  ( 26.47490684719999976, 1509.166822683030205, 201.9133613274379968 ) ) ;
#78811 = DIRECTION ( 'NONE',  ( -0.05490754757727549923, 0.004515313913275745793, -0.9984812332534417356 ) ) ;
#78812 = CARTESIAN_POINT ( 'NONE',  ( 5.526936513739999945, 1409.106065263330038, 188.1071742970979983 ) ) ;
#78813 = CARTESIAN_POINT ( 'NONE',  ( 5.580754349969999417, 1425.065972486529972, 185.9108535249980036 ) ) ;
#78814 = CARTESIAN_POINT ( 'NONE',  ( -12.38112447369999991, 1436.607677290789979, 151.2275677899980053 ) ) ;
#78815 = CARTESIAN_POINT ( 'NONE',  ( 7.950846525131810338, 1435.011334183859844, 205.5091519021299860 ) ) ;
#78816 = CARTESIAN_POINT ( 'NONE',  ( -13.58955623155380188, 1422.057351869020067, 203.7669116114399799 ) ) ;
#78817 = AXIS2_PLACEMENT_3D ( 'NONE', #1720, #17918, #3804 ) ;
#78818 = CARTESIAN_POINT ( 'NONE',  ( -19.08699729579999982, 1452.246527754430190, 144.6803158024980007 ) ) ;
#78819 = CARTESIAN_POINT ( 'NONE',  ( -29.99620953741502660, 1524.382868172863937, 198.4974435154502999 ) ) ;
#78820 = EDGE_LOOP ( 'NONE', ( #14909, #6283, #16831, #83727, #20662, #103484 ) ) ;
#78821 = CARTESIAN_POINT ( 'NONE',  ( -4.246466822330569713, 1508.879013277289914, 212.8697876484229994 ) ) ;
#78822 = EDGE_CURVE ( 'NONE', #105990, #100644, #81693, .T. ) ;
#78823 =( BOUNDED_SURFACE ( )  B_SPLINE_SURFACE ( 3, 2, ( 
 ( #19308, #897, #61369 ),
 ( #61920, #10939, #87653 ),
 ( #95488, #26618, #77591 ),
 ( #36142, #45114, #79809 ),
 ( #19871, #18755, #88201 ),
 ( #45671, #87087, #10371 ),
 ( #35022, #60813, #86529 ),
 ( #17642, #78127, #9280 ),
 ( #3115, #9824, #44545 ),
 ( #43992, #78691, #85981 ),
 ( #37243, #1431, #2007 ),
 ( #51844, #26049, #2566 ),
 ( #36688, #35574, #94361 ),
 ( #69768, #47845, #39444 ) ),
 .UNSPECIFIED., .F., .F., .F. ) 
 B_SPLINE_SURFACE_WITH_KNOTS ( ( 4, 2, 2, 2, 2, 2, 4 ),
 ( 3, 3 ),
 ( 6.873841773558098112E-17, 0.0009443072508236353231, 0.001416460876235418670, 0.001888614501647201908, 0.002360768127058984929, 0.002832921752470768384, 0.003777229003294335294 ),
 ( 0.000000000000000000, 1.000000000000000000 ),
 .UNSPECIFIED. ) 
 GEOMETRIC_REPRESENTATION_ITEM ( )  RATIONAL_B_SPLINE_SURFACE ( (
 ( 1.000000000000000000, 0.9376006582765963326, 1.000000000000000000),
 ( 1.000000000000000000, 0.9283977714734873432, 1.000000000000000000),
 ( 1.000000000000000000, 0.9189750060482670957, 1.000000000000000000),
 ( 1.000000000000000000, 0.9042792056126127687, 1.000000000000000000),
 ( 1.000000000000000000, 0.8992469033848606852, 1.000000000000000000),
 ( 1.000000000000000000, 0.8891280264676786338, 1.000000000000000000),
 ( 1.000000000000000000, 0.8840337471672635727, 1.000000000000000000),
 ( 1.000000000000000000, 0.8736395124166199677, 1.000000000000000000),
 ( 1.000000000000000000, 0.8683406746562497558, 1.000000000000000000),
 ( 1.000000000000000000, 0.8573361860698035519, 1.000000000000000000),
 ( 1.000000000000000000, 0.8516508399500833937, 1.000000000000000000),
 ( 1.000000000000000000, 0.8340914917056792000, 1.000000000000000000),
 ( 1.000000000000000000, 0.8215597275869019889, 1.000000000000000000),
 ( 1.000000000000000000, 0.8070209408750123048, 1.000000000000000000) ) ) 
 REPRESENTATION_ITEM ( '' )  SURFACE ( )  );
#78824 = ADVANCED_FACE ( 'NONE', ( #108217 ), #32115, .F. ) ;
#78825 = CARTESIAN_POINT ( 'NONE',  ( 16.66443530766549941, 1492.498764680389968, 193.3249378481789904 ) ) ;
#78826 = CARTESIAN_POINT ( 'NONE',  ( -44.43454715010000200, 1442.549948691149893, 270.0922452043980115 ) ) ;
#78827 = CARTESIAN_POINT ( 'NONE',  ( 7.535268056249999624, 1422.940929649649888, 195.7043803497990098 ) ) ;
#78828 = CARTESIAN_POINT ( 'NONE',  ( 17.22039721829999692, 1409.679124255730130, 223.1987974457980215 ) ) ;
#78829 = EDGE_CURVE ( 'NONE', #41356, #86539, #78194, .T. ) ;
#78830 = CARTESIAN_POINT ( 'NONE',  ( -14.61250254350000155, 1485.050473465629921, 224.2691043937979885 ) ) ;
#78832 = ADVANCED_FACE ( 'NONE', ( #34265 ), #75190, .F. ) ;
#78831 = CARTESIAN_POINT ( 'NONE',  ( 33.42844755917195698, 1501.977400791986611, 222.1271778627166213 ) ) ;
#78833 = PLANE ( 'NONE',  #76709 ) ;
#78834 = CARTESIAN_POINT ( 'NONE',  ( 1.399926847669999974, 1507.072115598929940, 236.8180522793980174 ) ) ;
#78835 = CARTESIAN_POINT ( 'NONE',  ( -6.229487579010000609, 1417.187363815429990, 231.8072993723980062 ) ) ;
#78836 = EDGE_CURVE ( 'NONE', #48650, #55354, #63503, .T. ) ;
#78837 = AXIS2_PLACEMENT_3D ( 'NONE', #101927, #93530, #25770 ) ;
#78838 = CARTESIAN_POINT ( 'NONE',  ( -10.32785586960000046, 1461.601613025990218, 211.2212836765089889 ) ) ;
#78839 = CARTESIAN_POINT ( 'NONE',  ( 0.06294878256441671649, 1358.513759169126160, 208.3718459617010978 ) ) ;
#78840 = CARTESIAN_POINT ( 'NONE',  ( -45.37234497165430014, 1435.615442251129934, 266.4280287536979586 ) ) ;
#78841 = LINE ( 'NONE', #2152, #19349 ) ;
#78842 = ORIENTED_EDGE ( 'NONE', *, *, #24948, .T. ) ;
#78843 = CARTESIAN_POINT ( 'NONE',  ( 23.99508155959999911, 1435.335429155559950, 136.6133439143980013 ) ) ;
#78844 = ADVANCED_FACE ( 'NONE', ( #59491 ), #51084, .T. ) ;
#78845 = ORIENTED_EDGE ( 'NONE', *, *, #39222, .T. ) ;
#78846 = CARTESIAN_POINT ( 'NONE',  ( 3.460866170685000132, 1517.020847257979995, 209.8575449048190080 ) ) ;
#78847 = CIRCLE ( 'NONE', #132, 1.000000000000000888 ) ;
#78848 = CARTESIAN_POINT ( 'NONE',  ( 7.012921650808690899, 1508.551704408389696, 202.7299073050613174 ) ) ;
#78849 = B_SPLINE_CURVE_WITH_KNOTS ( 'NONE', 5,
 ( #30442, #83055, #13617, #48927, #89252, #13070 ),
 .UNSPECIFIED., .F., .F.,
 ( 6, 6 ),
 ( 0.000000000000000000, 1.000000000000000000 ),
 .UNSPECIFIED. ) ;
#78850 = CARTESIAN_POINT ( 'NONE',  ( -2.470168521978402421, 1523.481610426287716, 242.8787258963054398 ) ) ;
#78851 = CARTESIAN_POINT ( 'NONE',  ( -15.63847246700000149, 1410.407006983229849, 191.1385721762979699 ) ) ;
#78852 = CARTESIAN_POINT ( 'NONE',  ( 0.8674825893500259788, 1495.985514189309924, 221.4329466185600097 ) ) ;
#78853 = ORIENTED_EDGE ( 'NONE', *, *, #16619, .T. ) ;
#78854 = CARTESIAN_POINT ( 'NONE',  ( -16.44161674339963142, 1409.512373515832905, 225.1669987584983232 ) ) ;
#78855 = AXIS2_PLACEMENT_3D ( 'NONE', #61351, #10352, #36669 ) ;
#78857 = CARTESIAN_POINT ( 'NONE',  ( -28.82451532742571487, 1526.348417187218956, 198.1911182592219518 ) ) ;
#78856 = CARTESIAN_POINT ( 'NONE',  ( 0.4061596876509999676, 1451.157747844730238, 182.5691048874980140 ) ) ;
#78858 = EDGE_CURVE ( 'NONE', #63089, #103670, #47759, .T. ) ;
#78859 =( BOUNDED_CURVE ( )  B_SPLINE_CURVE ( 3, ( #59147, #49087, #93268, #50722 ),
 .UNSPECIFIED., .F., .T. ) 
 B_SPLINE_CURVE_WITH_KNOTS ( ( 4, 4 ),
 ( 1.028227595440492026, 2.113365490006624992 ),
 .UNSPECIFIED. ) 
 CURVE ( )  GEOMETRIC_REPRESENTATION_ITEM ( )  RATIONAL_B_SPLINE_CURVE ( ( 1.000000000000000000, 0.9042567095595046567, 0.9042567095595046567, 1.000000000000000000 ) ) 
 REPRESENTATION_ITEM ( '' )  );
#78860 = DIRECTION ( 'NONE',  ( 0.4999999999998399614, 0.7071067811867740582, 0.4999999999998399614 ) ) ;
#78861 = CIRCLE ( 'NONE', #93145, 2.000000000000003553 ) ;
#78862 = CARTESIAN_POINT ( 'NONE',  ( -17.06985514805390025, 1508.522286251240075, 212.9373325725379971 ) ) ;
#78863 = CARTESIAN_POINT ( 'NONE',  ( 8.650035068340001132, 1470.670675412089849, 214.4250021573690219 ) ) ;
#78864 = EDGE_CURVE ( 'NONE', #52333, #85422, #100500, .T. ) ;
#78865 = CARTESIAN_POINT ( 'NONE',  ( -8.499221297664830033, 1438.111010583779944, 207.3306852776750020 ) ) ;
#78866 = ORIENTED_EDGE ( 'NONE', *, *, #92525, .T. ) ;
#78867 = CARTESIAN_POINT ( 'NONE',  ( -16.68259885503249862, 1411.554578397300020, 270.3635884854259643 ) ) ;
#78868 = CARTESIAN_POINT ( 'NONE',  ( -3.462835665494999660, 1517.038650117239968, 208.0021282158369900 ) ) ;
#78869 = CARTESIAN_POINT ( 'NONE',  ( 8.049312594969689982, 1418.917536817879864, 232.8636318953529667 ) ) ;
#78870 = CARTESIAN_POINT ( 'NONE',  ( 8.385113454956041323, 1436.167270151570165, 207.1929903346489823 ) ) ;
#78872 = VERTEX_POINT ( 'NONE', #105898 ) ;
#78871 = CARTESIAN_POINT ( 'NONE',  ( -4.078508008763815695, 1366.999314411288651, 209.6218459617148824 ) ) ;
#78873 = ORIENTED_EDGE ( 'NONE', *, *, #109978, .T. ) ;
#78874 = ADVANCED_FACE ( 'NONE', ( #95828 ), #35360, .T. ) ;
#78875 = CARTESIAN_POINT ( 'NONE',  ( 3.149414619133680482, 1370.221588481574372, 210.2153961732977905 ) ) ;
#78876 = CARTESIAN_POINT ( 'NONE',  ( -0.5818514064668890429, 1408.933379414289902, 186.2126681199449934 ) ) ;
#78877 = CARTESIAN_POINT ( 'NONE',  ( 3.688094639622395920, 1424.199184244893104, 183.9771557187304438 ) ) ;
#78878 = CARTESIAN_POINT ( 'NONE',  ( -6.096353515327549211, 1406.294149656895570, 266.9463287792909227 ) ) ;
#78879 = EDGE_CURVE ( 'NONE', #64021, #69131, #88979, .T. ) ;
#78880 = CARTESIAN_POINT ( 'NONE',  ( -17.67363391227470260, 1415.089996090750219, 207.5652716405009812 ) ) ;
#78881 = CARTESIAN_POINT ( 'NONE',  ( -23.42424912799999959, 1430.786185988730040, 212.0133531227079970 ) ) ;
#78882 = CARTESIAN_POINT ( 'NONE',  ( 5.300423936813779768, 1475.561024740650055, 269.2948677518700151 ) ) ;
#78883 = CARTESIAN_POINT ( 'NONE',  ( -11.66938051635290208, 1391.913060387229962, 209.0107206413649976 ) ) ;
#78884 = CARTESIAN_POINT ( 'NONE',  ( 10.82658308979999973, 1445.294115142620058, 185.4165881730980061 ) ) ;
#78885 = CARTESIAN_POINT ( 'NONE',  ( -5.786527600464999033, 1517.025653221279981, 205.6708125431369751 ) ) ;
#78886 = ORIENTED_EDGE ( 'NONE', *, *, #67514, .T. ) ;
#78887 = CARTESIAN_POINT ( 'NONE',  ( 22.76145762336689771, 1411.068184256920404, 214.2186865606036861 ) ) ;
#78888 = CARTESIAN_POINT ( 'NONE',  ( 1.473900770646640046, 1482.958075957350047, 182.1667372775690126 ) ) ;
#78889 = VERTEX_POINT ( 'NONE', #69560 ) ;
#78890 = CARTESIAN_POINT ( 'NONE',  ( 3.273042392802009815, 1508.551704408389924, 204.1347633686989980 ) ) ;
#78891 = CARTESIAN_POINT ( 'NONE',  ( 26.19227466039749785, 1451.106985942830079, 136.5081610195809958 ) ) ;
#78892 = CARTESIAN_POINT ( 'NONE',  ( 14.00875078090000159, 1416.819756528429934, 196.3921943334979971 ) ) ;
#78893 = CARTESIAN_POINT ( 'NONE',  ( -50.70014224199999830, 1389.561552466730063, 232.3334791991590009 ) ) ;
#78894 = CARTESIAN_POINT ( 'NONE',  ( -1.925297170580940076, 1522.051704408389924, 187.5582988486569889 ) ) ;
#78895 = CARTESIAN_POINT ( 'NONE',  ( 19.04580826369999969, 1410.500985970229976, 195.3929509149980106 ) ) ;
#78896 = CARTESIAN_POINT ( 'NONE',  ( 16.90742463041998178, 1444.994950788469168, 162.4348201727410981 ) ) ;
#78897 = CARTESIAN_POINT ( 'NONE',  ( 3.050517026533811293, 1439.677820960868303, 184.1494276813981799 ) ) ;
#78899 = CARTESIAN_POINT ( 'NONE',  ( -14.01398736212220086, 1379.590348564800024, 211.9184487047760115 ) ) ;
#78898 = CARTESIAN_POINT ( 'NONE',  ( -0.02597213800960000013, 1416.108377370330118, 233.5481719747979810 ) ) ;
#78900 = CARTESIAN_POINT ( 'NONE',  ( 0.8424627026991029499, 1452.935544315429979, 183.3439428731419980 ) ) ;
#78901 = CARTESIAN_POINT ( 'NONE',  ( 2.500000000000000000, 1448.210448412289907, 170.5244215879980061 ) ) ;
#78902 = CARTESIAN_POINT ( 'NONE',  ( 2.877113070465000089, 1516.697242742309982, 214.1184881303969973 ) ) ;
#78903 = CARTESIAN_POINT ( 'NONE',  ( -3.835404308830568265, 1412.913060387329779, 202.1011854665805743 ) ) ;
#78904 = EDGE_LOOP ( 'NONE', ( #85296, #48168, #77570, #49193, #23024 ) ) ;
#78905 = CARTESIAN_POINT ( 'NONE',  ( -17.40249709480000107, 1417.619717898290219, 206.9114233350790073 ) ) ;
#78906 = AXIS2_PLACEMENT_3D ( 'NONE', #49780, #22878, #56524 ) ;
#78907 = DIRECTION ( 'NONE',  ( 1.137551646196209927E-09, 1.000000000000000000, -9.990831686207409361E-10 ) ) ;
#78908 = CARTESIAN_POINT ( 'NONE',  ( -10.07374399369030016, 1483.508491176670077, 202.7669571214699999 ) ) ;
#78909 = EDGE_CURVE ( 'NONE', #69529, #17806, #52337, .T. ) ;
#78910 = CARTESIAN_POINT ( 'NONE',  ( -8602.628222780835131, 50.13405481578727318, -10923.45535519210353 ) ) ;
#78911 = ADVANCED_FACE ( 'NONE', ( #10735 ), #68872, .F. ) ;
#78912 = CARTESIAN_POINT ( 'NONE',  ( -0.1448779671327833363, 1421.022422678020575, 193.7177100718903091 ) ) ;
#78913 = AXIS2_PLACEMENT_3D ( 'NONE', #99488, #75436, #109572 ) ;
#78914 = CARTESIAN_POINT ( 'NONE',  ( 0.3821805048270000005, 1506.433683729329914, 231.1012307613979999 ) ) ;
#78915 = CARTESIAN_POINT ( 'NONE',  ( -17.24149055319999846, 1446.934121893590145, 209.1218459616979999 ) ) ;
#78916 = CARTESIAN_POINT ( 'NONE',  ( 38.96329220849997910, 1459.274185255430666, 266.3801432638982760 ) ) ;
#78917 = CARTESIAN_POINT ( 'NONE',  ( -12.31911163787790109, 1378.288338451009849, 209.5493042496160001 ) ) ;
#78918 = CARTESIAN_POINT ( 'NONE',  ( -26.61274952006059991, 1468.149000416469789, 269.9851188083980560 ) ) ;
#78919 = CARTESIAN_POINT ( 'NONE',  ( -9.775905228975700467, 1461.154446592330032, 210.2374177378800084 ) ) ;
#78920 = CARTESIAN_POINT ( 'NONE',  ( -16.94833435341390171, 1419.662971730580011, 201.4173425967440210 ) ) ;
#78921 = VERTEX_POINT ( 'NONE', #78485 ) ;
#78922 = DIRECTION ( 'NONE',  ( 0.000000000000000000, -1.000000000000000000, 0.000000000000000000 ) ) ;
#78923 = DIRECTION ( 'NONE',  ( 0.9858563016923833633, 0.000000000000000000, 0.1675928173085483863 ) ) ;
#78924 = EDGE_CURVE ( 'NONE', #104968, #50471, #59075, .T. ) ;
#78925 = LINE ( 'NONE', #61573, #99645 ) ;
#78926 = FACE_OUTER_BOUND ( 'NONE', #17408, .T. ) ;
#78927 = CARTESIAN_POINT ( 'NONE',  ( -15.15175306172240077, 1509.481969237379872, 236.4739884436810087 ) ) ;
#78928 = CARTESIAN_POINT ( 'NONE',  ( 25.66628087189999974, 1469.241412578029895, 213.4071819949780036 ) ) ;
#78929 = CARTESIAN_POINT ( 'NONE',  ( -17.27256466963439863, 1419.895559490180403, 207.2304356867004458 ) ) ;
#78930 = CARTESIAN_POINT ( 'NONE',  ( -15.40310530260000021, 1508.176735222329853, 231.4698242431979907 ) ) ;
#78931 = CARTESIAN_POINT ( 'NONE',  ( -35.19207028348809985, 1383.835214657470260, 234.1679424143649726 ) ) ;
#78932 = CARTESIAN_POINT ( 'NONE',  ( -2.487923629571139994, 1508.884229736110001, 204.6305622231600125 ) ) ;
#78933 = CARTESIAN_POINT ( 'NONE',  ( 10.24761658979999979, 1409.091680548530121, 219.5424323772980131 ) ) ;
#78934 = CARTESIAN_POINT ( 'NONE',  ( -2173.981453289206911, -8382.262153571264207, 1975.191541669308435 ) ) ;
#78935 = CARTESIAN_POINT ( 'NONE',  ( 0.1648540493162710119, 1483.364881617609853, 181.9498374863690060 ) ) ;
#78937 = VERTEX_POINT ( 'NONE', #95285 ) ;
#78936 = CARTESIAN_POINT ( 'NONE',  ( 3.736539510769999684, 1442.283932804090000, 217.1659672788889850 ) ) ;
#78938 = CARTESIAN_POINT ( 'NONE',  ( -0.5200257807070000071, 1450.894900823180024, 181.6063032255979977 ) ) ;
#78939 = AXIS2_PLACEMENT_3D ( 'NONE', #42794, #25963, #51757 ) ;
#78940 = EDGE_CURVE ( 'NONE', #88625, #43749, #48362, .T. ) ;
#78941 = CARTESIAN_POINT ( 'NONE',  ( -10.18734585702747886, 1389.825619450207569, 202.1025026781494205 ) ) ;
#78942 = CARTESIAN_POINT ( 'NONE',  ( -4.633158249500000103, 1476.260951450290122, 199.8663068878290119 ) ) ;
#78944 = VERTEX_POINT ( 'NONE', #73942 ) ;
#78943 = CARTESIAN_POINT ( 'NONE',  ( -32.70814417905852167, 1524.201816949777822, 217.1264145000764074 ) ) ;
#78945 = CARTESIAN_POINT ( 'NONE',  ( 14.17510881067400064, 1428.761380490490183, 195.0896992289169987 ) ) ;
#78946 = ORIENTED_EDGE ( 'NONE', *, *, #1915, .T. ) ;
#78947 = AXIS2_PLACEMENT_3D ( 'NONE', #55927, #90047, #47521 ) ;
#78948 = CARTESIAN_POINT ( 'NONE',  ( -13.37269592510800109, 1390.548568132430091, 209.7987342400010107 ) ) ;
#78949 = CARTESIAN_POINT ( 'NONE',  ( -1.864982813339999934, 1489.661995449090227, 188.3491068096989807 ) ) ;
#78950 = CARTESIAN_POINT ( 'NONE',  ( -4.453834213590135427, 1509.079627139014747, 238.2871813933543876 ) ) ;
#78951 = EDGE_CURVE ( 'NONE', #100304, #22289, #67002, .T. ) ;
#78952 = CARTESIAN_POINT ( 'NONE',  ( -3.007336967298251729, 1369.006237963355716, 210.6121239941897159 ) ) ;
#78953 = CARTESIAN_POINT ( 'NONE',  ( -2.429964404760000196, 1432.449532658489943, 217.5898836994890075 ) ) ;
#78954 = DIRECTION ( 'NONE',  ( 0.4978433412588781914, 0.000000000000000000, 0.8672669759446606230 ) ) ;
#78955 = CARTESIAN_POINT ( 'NONE',  ( 12.43454791605049969, 1409.347284361509992, 217.4061878439790121 ) ) ;
#78956 = LINE ( 'NONE', #46461, #36545 ) ;
#78957 = CARTESIAN_POINT ( 'NONE',  ( -101.8647915021330022, 1385.225522266660164, 296.5844919615699951 ) ) ;
#78958 = CARTESIAN_POINT ( 'NONE',  ( -17.43112864230000270, 1424.169315834030158, 191.5803361794979764 ) ) ;
#78959 = CARTESIAN_POINT ( 'NONE',  ( -3.523962699983150149, 1476.511731499819916, 220.0526012347959863 ) ) ;
#78960 = EDGE_LOOP ( 'NONE', ( #29123, #82568, #57838, #52101 ) ) ;
#78961 = CIRCLE ( 'NONE', #53970, 11.73460161499999899 ) ;
#78962 = CARTESIAN_POINT ( 'NONE',  ( 10.79524667479070033, 1489.627639623460027, 207.4011449438049794 ) ) ;
#78964 = ORIENTED_EDGE ( 'NONE', *, *, #46651, .T. ) ;
#78963 = DIRECTION ( 'NONE',  ( 0.9455185755993178454, 0.000000000000000000, -0.3255681544571537578 ) ) ;
#78965 = CARTESIAN_POINT ( 'NONE',  ( -19.83859993069999916, 1467.194195006989958, 209.1218459616989946 ) ) ;
#78966 = VERTEX_POINT ( 'NONE', #72843 ) ;
#78967 = ADVANCED_FACE ( 'NONE', ( #108073 ), #21290, .T. ) ;
#78968 = CARTESIAN_POINT ( 'NONE',  ( 23.59424604019999805, 1507.884706830530149, 222.5751569823979992 ) ) ;
#78969 = CARTESIAN_POINT ( 'NONE',  ( -3.603740778195532624, 1362.725725758258250, 209.6218459617148824 ) ) ;
#78970 = CARTESIAN_POINT ( 'NONE',  ( -11.97668390569999985, 1433.616603791269881, 149.8660147765980071 ) ) ;
#78971 = EDGE_CURVE ( 'NONE', #105450, #109428, #13611, .T. ) ;
#78972 = CARTESIAN_POINT ( 'NONE',  ( 29.50369192380506433, 1509.962379296385507, 211.7848930765254920 ) ) ;
#78973 = CARTESIAN_POINT ( 'NONE',  ( -31.76119286153722499, 1522.906363951597314, 221.9477464134160414 ) ) ;
#78974 = CARTESIAN_POINT ( 'NONE',  ( 4.911909971580000089, 1396.617946523930186, 220.6495969109980138 ) ) ;
#78975 = CARTESIAN_POINT ( 'NONE',  ( 1.381906298289999890, 1417.049103970330179, 233.2953579960980051 ) ) ;
#78976 = CARTESIAN_POINT ( 'NONE',  ( -7.211758761846644106, 1516.538242702012212, 211.1938241164952217 ) ) ;
#78977 = CARTESIAN_POINT ( 'NONE',  ( -0.5378485204050000856, 1471.144553927230163, 182.4732557751979982 ) ) ;
#78978 = CARTESIAN_POINT ( 'NONE',  ( -8.784417309943542307, 1369.490261236509468, 209.6218459617033432 ) ) ;
#78979 = DIRECTION ( 'NONE',  ( 0.000000000000000000, 1.000000000000000000, 0.000000000000000000 ) ) ;
#78980 = EDGE_CURVE ( 'NONE', #36364, #56488, #103269, .T. ) ;
#78981 = CARTESIAN_POINT ( 'NONE',  ( -4.625693903144999730, 1517.042661899400173, 206.8353996064669786 ) ) ;
#78982 = CARTESIAN_POINT ( 'NONE',  ( -13.04882216325809985, 1434.812040110809903, 149.3440682124420107 ) ) ;
#78983 =( GEOMETRIC_REPRESENTATION_CONTEXT ( 3 ) GLOBAL_UNCERTAINTY_ASSIGNED_CONTEXT ( ( #97207 ) ) GLOBAL_UNIT_ASSIGNED_CONTEXT ( ( #106100, #88755, #36690 ) ) REPRESENTATION_CONTEXT ( 'NONE', 'WORKASPACE' ) );
#78984 = CARTESIAN_POINT ( 'NONE',  ( 11.58690141939999840, 1425.690684998030292, 133.5558073867980227 ) ) ;
#78985 = CARTESIAN_POINT ( 'NONE',  ( 0.4117221240290019901, 1496.667641243389880, 196.7318124780990161 ) ) ;
#78986 = CARTESIAN_POINT ( 'NONE',  ( -1.133238050829999954, 1495.637768932689823, 220.4196360831990091 ) ) ;
#78987 = ADVANCED_FACE ( 'NONE', ( #107528 ), #43830, .T. ) ;
#78988 = CARTESIAN_POINT ( 'NONE',  ( 40.54813384580009483, 1444.189903829430023, 137.0615966367320198 ) ) ;
#78989 = ORIENTED_EDGE ( 'NONE', *, *, #110441, .T. ) ;
#78990 = CARTESIAN_POINT ( 'NONE',  ( 13.07344732962040013, 1516.551188146170034, 192.4513774157680075 ) ) ;
#78991 = CARTESIAN_POINT ( 'NONE',  ( -27.49404549240000151, 1488.693617964029954, 209.3049790079790000 ) ) ;
#78993 = CARTESIAN_POINT ( 'NONE',  ( 17.09872249335660044, 1410.735067943620152, 192.0960184572400067 ) ) ;
#78992 = CARTESIAN_POINT ( 'NONE',  ( -10.38662965184200004, 1425.402516998919964, 95.13675362039579397 ) ) ;
#78994 = CARTESIAN_POINT ( 'NONE',  ( 5.011678838024999472, 1516.989560013210166, 212.3778133565769792 ) ) ;
#78995 = CARTESIAN_POINT ( 'NONE',  ( 0.6591021011063420421, 1395.936076739869804, 198.1345608290150153 ) ) ;
#78996 = CARTESIAN_POINT ( 'NONE',  ( -19.59664182070000038, 1435.002040243690089, 208.4023078862850014 ) ) ;
#78997 = CARTESIAN_POINT ( 'NONE',  ( -34.21122779019999882, 1429.487523400830014, 254.6787106624979629 ) ) ;
#78998 = CARTESIAN_POINT ( 'NONE',  ( -1.222313235619999938, 1487.670855816090125, 219.9174996087990053 ) ) ;
#78999 = CARTESIAN_POINT ( 'NONE',  ( 28.49886664283559767, 1509.035040371930108, 209.4553795045120239 ) ) ;
#79000 = FACE_OUTER_BOUND ( 'NONE', #56792, .T. ) ;
#79001 = CYLINDRICAL_SURFACE ( 'NONE', #6076, 0.9999999999999465983 ) ;
#79002 = ORIENTED_EDGE ( 'NONE', *, *, #88133, .T. ) ;
#79003 = CARTESIAN_POINT ( 'NONE',  ( 10.81377540340000110, 1493.463431426289844, 215.2021047779490175 ) ) ;
#79004 = CARTESIAN_POINT ( 'NONE',  ( 9.698097846587389270, 1462.705833979410045, 208.0596819494889758 ) ) ;
#79005 = ADVANCED_FACE ( 'NONE', ( #59908 ), #44330, .F. ) ;
#79006 = CARTESIAN_POINT ( 'NONE',  ( -16.69641803230000221, 1458.740222332030044, 230.3336308253980178 ) ) ;
#79007 = ORIENTED_EDGE ( 'NONE', *, *, #39126, .T. ) ;
#79008 = EDGE_LOOP ( 'NONE', ( #9719, #34154, #48311, #5981, #67473, #105268, #64947, #92974, #80802, #51730, #86000, #27877, #105098 ) ) ;
#79009 = CARTESIAN_POINT ( 'NONE',  ( 9.109326017966379752, 1452.537928671039708, 211.6759096298679879 ) ) ;
#79010 = CARTESIAN_POINT ( 'NONE',  ( 7.158179755560000856, 1423.953782493189919, 195.2758576736989937 ) ) ;
#79011 = ORIENTED_EDGE ( 'NONE', *, *, #37130, .F. ) ;
#79012 = AXIS2_PLACEMENT_3D ( 'NONE', #48096, #45096, #79236 ) ;
#79013 = CARTESIAN_POINT ( 'NONE',  ( -5.273680927263949769, 1398.098440474080235, 199.4684377759750191 ) ) ;
#79014 = CARTESIAN_POINT ( 'NONE',  ( 8.076329059878878169, 1446.679444598521059, 154.0159284771656871 ) ) ;
#79015 = ADVANCED_FACE ( 'NONE', ( #8918 ), #83422, .T. ) ;
#79016 = FACE_OUTER_BOUND ( 'NONE', #15192, .T. ) ;
#79017 = CARTESIAN_POINT ( 'NONE',  ( 27.40792072111510080, 1509.298959737374616, 206.1637269058524282 ) ) ;
#79018 = CARTESIAN_POINT ( 'NONE',  ( 2.025872226998560510, 1421.136586182680048, 183.1659243740039926 ) ) ;
#79019 = FILL_AREA_STYLE_COLOUR ( '', #103519 ) ;
#79020 = CARTESIAN_POINT ( 'NONE',  ( 18.81609481059999922, 1456.479165729590022, 204.5196734937790097 ) ) ;
#79021 = CARTESIAN_POINT ( 'NONE',  ( 0.1681676109750000203, 1420.473121951529947, 182.7464980200980165 ) ) ;
#79022 = CARTESIAN_POINT ( 'NONE',  ( -2.292940207144999576, 1516.565291103010168, 202.5758065368070220 ) ) ;
#79023 = CARTESIAN_POINT ( 'NONE',  ( 5.014195101815000832, 1517.120861839400050, 210.8273123806970091 ) ) ;
#79024 = ORIENTED_EDGE ( 'NONE', *, *, #52467, .T. ) ;
#79025 = CARTESIAN_POINT ( 'NONE',  ( 11.86554121557050046, 1432.296927349550060, 149.9822551877360013 ) ) ;
#79026 = CIRCLE ( 'NONE', #57603, 1.000000000000000000 ) ;
#79027 = CARTESIAN_POINT ( 'NONE',  ( 13.21297046888754068, 1444.693905304529835, 187.3376099162051673 ) ) ;
#79028 = ORIENTED_EDGE ( 'NONE', *, *, #60483, .T. ) ;
#79029 = DIRECTION ( 'NONE',  ( 0.000000000000000000, 0.000000000000000000, -1.000000000000000000 ) ) ;
#79030 = CARTESIAN_POINT ( 'NONE',  ( -5.868857667190599869, 1508.551703962909869, 219.6331723996029837 ) ) ;
#79031 = CARTESIAN_POINT ( 'NONE',  ( 2.881519388670000126, 1507.413003788429933, 235.9584917197979905 ) ) ;
#79032 = CARTESIAN_POINT ( 'NONE',  ( -5.613020775148240382, 1470.678943295929912, 217.6304317108330224 ) ) ;
#79033 = CARTESIAN_POINT ( 'NONE',  ( -6.451353027019999686, 1421.812455514629846, 186.8014209383979960 ) ) ;
#79034 = CARTESIAN_POINT ( 'NONE',  ( 1.417322805690939935, 1410.048863607139992, 269.8655646141270381 ) ) ;
#79035 = CARTESIAN_POINT ( 'NONE',  ( 9.196086508652181024, 1450.899357183659959, 210.0407472026730034 ) ) ;
#79036 = CARTESIAN_POINT ( 'NONE',  ( -8.928049104570000338, 1472.922707491090023, 201.8104512964389983 ) ) ;
#79037 = CARTESIAN_POINT ( 'NONE',  ( 9.553964019109999484, 1492.165809702890101, 214.7542154822990028 ) ) ;
#79038 = CARTESIAN_POINT ( 'NONE',  ( -30.36057678899999601, 1379.678206996359904, 214.3682391549489807 ) ) ;
#79039 = CARTESIAN_POINT ( 'NONE',  ( 8.960106487924051066, 1425.021082012188799, 195.6425420597072673 ) ) ;
#79041 = CARTESIAN_POINT ( 'NONE',  ( 16.36456115949343015, 1519.551704408389924, 198.1507535207238391 ) ) ;
#79040 = CARTESIAN_POINT ( 'NONE',  ( -17.26759053627300133, 1429.542278724649805, 191.2131399352340111 ) ) ;
#79042 = CARTESIAN_POINT ( 'NONE',  ( -67.68653639037678715, 1379.747580689172310, 278.9655481580869036 ) ) ;
#79043 = CARTESIAN_POINT ( 'NONE',  ( -9.956812081275220550, 1439.552395354249938, 208.2581519739229918 ) ) ;
#79044 = CARTESIAN_POINT ( 'NONE',  ( -7.855404022624998817, 1514.254015528259970, 202.3343151538169877 ) ) ;
#79045 = ORIENTED_EDGE ( 'NONE', *, *, #85411, .F. ) ;
#79046 = CARTESIAN_POINT ( 'NONE',  ( 1.199040866600000048E-14, 1419.211677883429957, 248.0989693021979861 ) ) ;
#79047 = VECTOR ( 'NONE', #80827, 1000.000000000000114 ) ;
#79048 = DIRECTION ( 'NONE',  ( 0.01594118961724032973, -0.9969860201949399814, -0.07592597717146747083 ) ) ;
#79049 = CARTESIAN_POINT ( 'NONE',  ( -19.39983987835444879, 1522.382868172863937, 178.9515629539737631 ) ) ;
#79050 = CARTESIAN_POINT ( 'NONE',  ( 3.944248398050000048, 1506.370035955090088, 220.2366324052989626 ) ) ;
#79051 = CARTESIAN_POINT ( 'NONE',  ( 17.47708894566800097, 1409.791774897460300, 270.0791891301039982 ) ) ;
#79053 = VERTEX_POINT ( 'NONE', #33016 ) ;
#79052 = CARTESIAN_POINT ( 'NONE',  ( -1.407451548162420130, 1515.079400017670196, 204.7927796877619926 ) ) ;
#79054 = DIRECTION ( 'NONE',  ( 0.000000000000000000, 0.000000000000000000, -1.000000000000000000 ) ) ;
#79055 = DIRECTION ( 'NONE',  ( 1.000000000000000000, 0.000000000000000000, 0.000000000000000000 ) ) ;
#79056 = DIRECTION ( 'NONE',  ( -0.4090087482554316534, 0.000000000000000000, -0.9125304618753967700 ) ) ;
#79057 = CARTESIAN_POINT ( 'NONE',  ( 5.200787045398697295, 1440.223982444788362, 217.6291937790904285 ) ) ;
#79058 = CARTESIAN_POINT ( 'NONE',  ( 12.18811178233499959, 1511.857118786289902, 224.3850700526670039 ) ) ;
#79059 = CARTESIAN_POINT ( 'NONE',  ( -9.117626234630000326, 1442.289878148370008, 185.2642562222980018 ) ) ;
#79060 = CARTESIAN_POINT ( 'NONE',  ( 19.47548006807109999, 1509.632698354770127, 231.9332913439310175 ) ) ;
#79061 = CARTESIAN_POINT ( 'NONE',  ( -109.1312182564879976, 1384.932234318600194, 313.2646789733740320 ) ) ;
#79062 = CARTESIAN_POINT ( 'NONE',  ( -4.424139982966695861, 1432.332219231797808, 155.5697322143722943 ) ) ;
#79063 = CARTESIAN_POINT ( 'NONE',  ( 2.917282800289999756, 1415.076022899730106, 231.8410176321980032 ) ) ;
#79064 = CARTESIAN_POINT ( 'NONE',  ( 9.961228442255011473, 1469.533171005829900, 210.4989064630590008 ) ) ;
#79065 = CARTESIAN_POINT ( 'NONE',  ( -16.02253603680000182, 1459.141923948030126, 230.3636548079979889 ) ) ;
#79066 = CARTESIAN_POINT ( 'NONE',  ( -4.624736897314999595, 1516.994127245590107, 206.2540423059970180 ) ) ;
#79067 = CARTESIAN_POINT ( 'NONE',  ( 44.05617169130000121, 1429.881624369530073, 266.7430392887980020 ) ) ;
#79068 = CARTESIAN_POINT ( 'NONE',  ( -32.40058737600715233, 1524.130440953581001, 216.9356993550890138 ) ) ;
#79069 = CARTESIAN_POINT ( 'NONE',  ( 20.26752588049999915, 1435.348985798829972, 144.1465333546979934 ) ) ;
#79070 = CARTESIAN_POINT ( 'NONE',  ( 19.68293457889999942, 1488.589411887629922, 190.0755286157979924 ) ) ;
#79071 = CARTESIAN_POINT ( 'NONE',  ( -23.10492689500000196, 1433.621912620239982, 215.5179811059879853 ) ) ;
#79072 = CARTESIAN_POINT ( 'NONE',  ( -5.080289282479999002, 1480.093209919690253, 228.8812397303989883 ) ) ;
#79073 = CARTESIAN_POINT ( 'NONE',  ( -9.885589491230001968, 1475.057254907329934, 266.9235355597979833 ) ) ;
#79074 = CARTESIAN_POINT ( 'NONE',  ( -3.317807041231336485E-31, 1414.677402202029953, 209.1218459616989946 ) ) ;
#79075 = CARTESIAN_POINT ( 'NONE',  ( -41.10478585342460178, 1442.607632416070146, 136.7995045943229968 ) ) ;
#79076 = CARTESIAN_POINT ( 'NONE',  ( -7.121584071090000023, 1409.161751583130126, 195.9581075130980139 ) ) ;
#79077 = CARTESIAN_POINT ( 'NONE',  ( -17.56697300799999795, 1414.971439108430104, 207.9608875356680073 ) ) ;
#79078 = CARTESIAN_POINT ( 'NONE',  ( -11.97846764590000035, 1441.462071183699891, 187.7017596415979881 ) ) ;
#79079 = CARTESIAN_POINT ( 'NONE',  ( -7.616835117835059954, 1383.928091763239991, 219.0006089918529995 ) ) ;
#79080 = CARTESIAN_POINT ( 'NONE',  ( 18.18312599666770168, 1429.576275455930045, 208.4333127768320253 ) ) ;
#79081 = CARTESIAN_POINT ( 'NONE',  ( -1.203801419936314954, 1419.233897949102811, 185.0625596308904051 ) ) ;
#79082 = ORIENTED_EDGE ( 'NONE', *, *, #19897, .F. ) ;
#79083 = CARTESIAN_POINT ( 'NONE',  ( 5.551188674472009588, 1510.480349264700180, 216.6723492941099778 ) ) ;
#79084 = CARTESIAN_POINT ( 'NONE',  ( -11.07873686478040121, 1409.299938403639999, 199.0863655858090056 ) ) ;
#79085 = CARTESIAN_POINT ( 'NONE',  ( -12.89242915326980032, 1508.551704408300111, 210.2815080484370185 ) ) ;
#79086 = CARTESIAN_POINT ( 'NONE',  ( -21.58938578137761866, 1409.666978351642001, 210.4204379443588664 ) ) ;
#79087 = CARTESIAN_POINT ( 'NONE',  ( -45.63714053399999671, 1445.950958213619970, 268.9747508869979811 ) ) ;
#79088 = CARTESIAN_POINT ( 'NONE',  ( -11.87098815724909961, 1481.783871394969992, 209.3733780729720024 ) ) ;
#79089 = CARTESIAN_POINT ( 'NONE',  ( 0.1761179889197699855, 1419.971149309630164, 184.0347958421160115 ) ) ;
#79090 = CARTESIAN_POINT ( 'NONE',  ( -25.89799839909999690, 1509.146170697830030, 218.4252831721279904 ) ) ;
#79091 = CARTESIAN_POINT ( 'NONE',  ( -74.12207176259649088, 1384.651791245910090, 299.2615222811550098 ) ) ;
#79092 = CARTESIAN_POINT ( 'NONE',  ( -29.17863452356749931, 1384.967235213910044, 205.1305293287510096 ) ) ;
#79093 = CARTESIAN_POINT ( 'NONE',  ( 16.85987604637189818, 1423.620959927220156, 227.7720207472910090 ) ) ;
#79094 = CARTESIAN_POINT ( 'NONE',  ( 13.01304944610000192, 1416.520646107730045, 221.6242398431980121 ) ) ;
#79095 = CARTESIAN_POINT ( 'NONE',  ( 14.80905694640000192, 1474.177104242629866, 223.3992951678980035 ) ) ;
#79096 = DIRECTION ( 'NONE',  ( -1.000000000000000000, 0.000000000000000000, 0.000000000000000000 ) ) ;
#79097 = CARTESIAN_POINT ( 'NONE',  ( 2.114990338821392868, 1370.171684715506444, 206.8534323859588824 ) ) ;
#79098 = CARTESIAN_POINT ( 'NONE',  ( -8.848352231939999868, 1384.927997118699750, 199.9247642750889895 ) ) ;
#79099 = FACE_OUTER_BOUND ( 'NONE', #67031, .T. ) ;
#79100 = CARTESIAN_POINT ( 'NONE',  ( 18.04214300190000131, 1416.520646107730045, 208.7607579491829881 ) ) ;
#79101 = AXIS2_PLACEMENT_3D ( 'NONE', #96829, #11707, #56475 ) ;
#79102 = CARTESIAN_POINT ( 'NONE',  ( -2.829801042252522159, 1451.871858332230204, 184.7457192350124160 ) ) ;
#79103 = CARTESIAN_POINT ( 'NONE',  ( 4.548814465829999598, 1424.046559047009850, 193.1022451195989618 ) ) ;
#79104 = ADVANCED_FACE ( 'NONE', ( #32487 ), #50950, .F. ) ;
#79105 = CARTESIAN_POINT ( 'NONE',  ( 22.40106396050000015, 1409.695322778229865, 210.5405262121579995 ) ) ;
#79106 = CARTESIAN_POINT ( 'NONE',  ( -106.6090143111130004, 1391.913060387289988, 305.6150165752750354 ) ) ;
#79107 = CARTESIAN_POINT ( 'NONE',  ( 7.830182259921620869, 1460.133318085240035, 228.9032440295520132 ) ) ;
#79108 = CARTESIAN_POINT ( 'NONE',  ( -5.360171697043470296, 1422.243961768539748, 144.5806141462400092 ) ) ;
#79110 = CARTESIAN_POINT ( 'NONE',  ( -9.131333920219999456, 1383.714870296950039, 200.1584639485390085 ) ) ;
#79109 = CARTESIAN_POINT ( 'NONE',  ( -10.97356441630000212, 1432.589727400840047, 151.7700027225980079 ) ) ;
#79111 = CARTESIAN_POINT ( 'NONE',  ( -5.146359519290000684, 1391.913486199090130, 203.5916337600390023 ) ) ;
#79112 = CARTESIAN_POINT ( 'NONE',  ( 0.3821805048270000005, 1506.433683729329914, 231.1012307613979999 ) ) ;
#79113 = CARTESIAN_POINT ( 'NONE',  ( -11.77655089729999816, 1490.342630228989947, 209.9285965979820219 ) ) ;
#79114 = DIRECTION ( 'NONE',  ( 0.9900962604114871279, -0.1403901532130690244, 1.186453863995930381E-14 ) ) ;
#79115 = CARTESIAN_POINT ( 'NONE',  ( -9.516636888329999877, 1366.309137899869938, 210.6218459616991936 ) ) ;
#79116 = CARTESIAN_POINT ( 'NONE',  ( -7.334957394705000411, 1517.030858226499959, 204.5055736355369902 ) ) ;
#79117 = CARTESIAN_POINT ( 'NONE',  ( -2.596261494520238688, 1525.907212628473644, 240.7735774411713123 ) ) ;
#79118 = CARTESIAN_POINT ( 'NONE',  ( -16.74544130042350076, 1485.914225547749993, 187.7220481146609927 ) ) ;
#79119 = CIRCLE ( 'NONE', #25436, 1.000000000000000888 ) ;
#79120 = CARTESIAN_POINT ( 'NONE',  ( 10.93254534338380068, 1502.901713907840076, 213.3630869133220074 ) ) ;
#79121 = CARTESIAN_POINT ( 'NONE',  ( -4.276331814141159704, 1441.049878954770065, 157.0171284178840097 ) ) ;
#79123 = ORIENTED_EDGE ( 'NONE', *, *, #110361, .F. ) ;
#79122 = CARTESIAN_POINT ( 'NONE',  ( -67.15060528540000462, 1379.747519056979854, 278.1647121851589759 ) ) ;
#79124 = ADVANCED_FACE ( 'NONE', ( #11691 ), #29050, .F. ) ;
#79125 = VERTEX_POINT ( 'NONE', #107946 ) ;
#79126 = CARTESIAN_POINT ( 'NONE',  ( 11.82610189953429902, 1433.713742287859759, 150.7576001896150046 ) ) ;
#79127 = FACE_OUTER_BOUND ( 'NONE', #103357, .T. ) ;
#79128 = VERTEX_POINT ( 'NONE', #72711 ) ;
#79129 = CARTESIAN_POINT ( 'NONE',  ( -2.283769792747494698, 1456.639021601948798, 199.9092664731689979 ) ) ;
#79130 = FACE_OUTER_BOUND ( 'NONE', #46452, .T. ) ;
#79132 = CARTESIAN_POINT ( 'NONE',  ( 13.89869200000000049, 1452.835253893030085, 223.8385666725980059 ) ) ;
#79131 = CARTESIAN_POINT ( 'NONE',  ( 15.97992989932220098, 1420.985315616920161, 191.2040731956429909 ) ) ;
#79133 = CARTESIAN_POINT ( 'NONE',  ( 11.98951922200000020, 1442.759074889710064, 150.6922381223979812 ) ) ;
#79134 = CARTESIAN_POINT ( 'NONE',  ( 1.430900451930000150, 1488.174586716330168, 181.9313141933980091 ) ) ;
#79135 = CARTESIAN_POINT ( 'NONE',  ( -105.9863851607009906, 1378.913060388959821, 305.2978657741859934 ) ) ;
#79136 = DIRECTION ( 'NONE',  ( 0.9455185755993178454, 0.000000000000000000, -0.3255681544571539243 ) ) ;
#79137 = CARTESIAN_POINT ( 'NONE',  ( -2.284199401535000007, 1516.940296199220029, 212.3910308785969789 ) ) ;
#79138 = CARTESIAN_POINT ( 'NONE',  ( 38.70428745349820332, 1437.478004125059897, 134.0999999972650016 ) ) ;
#79139 = CARTESIAN_POINT ( 'NONE',  ( -11.60879801380000131, 1421.965952794710120, 210.6472336029989947 ) ) ;
#79140 = EDGE_LOOP ( 'NONE', ( #101442, #41928, #90136, #60717, #7771 ) ) ;
#79141 = CARTESIAN_POINT ( 'NONE',  ( 13.81563158420089898, 1434.988513889579963, 148.7679932446569921 ) ) ;
#79142 = CARTESIAN_POINT ( 'NONE',  ( -0.002530016318419649971, 1432.316930810580061, 200.6915054315279860 ) ) ;
#79143 = ORIENTED_EDGE ( 'NONE', *, *, #36043, .F. ) ;
#79144 = VERTEX_POINT ( 'NONE', #4931 ) ;
#79145 = ORIENTED_EDGE ( 'NONE', *, *, #14249, .F. ) ;
#79146 = CARTESIAN_POINT ( 'NONE',  ( 12.79376191942176355, 1444.983190770407418, 169.4500884308193918 ) ) ;
#79147 = CARTESIAN_POINT ( 'NONE',  ( -3.168849912869999841, 1464.840305621330117, 237.5147281217979867 ) ) ;
#79148 = CARTESIAN_POINT ( 'NONE',  ( 20.54534055259999903, 1497.714303034489831, 214.2326470396490095 ) ) ;
#79149 = CARTESIAN_POINT ( 'NONE',  ( -7.545227633159999669, 1384.915097837209942, 219.0875773561589881 ) ) ;
#79150 = CARTESIAN_POINT ( 'NONE',  ( 1.184628359070449832, 1465.692306277839862, 198.1686851201980062 ) ) ;
#79152 = EDGE_CURVE ( 'NONE', #21147, #32555, #108575, .T. ) ;
#79151 = EDGE_CURVE ( 'NONE', #96612, #14943, #13310, .T. ) ;
#79153 = CARTESIAN_POINT ( 'NONE',  ( -17.47732762797510375, 1448.300284982579797, 218.1790054843986866 ) ) ;
#79154 = CARTESIAN_POINT ( 'NONE',  ( -42.46926378087947995, 1379.662295881295449, 226.7269345055754854 ) ) ;
#79155 = CARTESIAN_POINT ( 'NONE',  ( 4.240346634148639993, 1446.384605460860030, 162.7848567526920078 ) ) ;
#79156 = EDGE_CURVE ( 'NONE', #79540, #35766, #64008, .T. ) ;
#79157 = DIRECTION ( 'NONE',  ( 0.000000000000000000, 1.000000000000000000, 0.000000000000000000 ) ) ;
#79158 = ORIENTED_EDGE ( 'NONE', *, *, #92525, .F. ) ;
#79159 = CARTESIAN_POINT ( 'NONE',  ( 2.476450664134999702, 1516.843453247299749, 206.8221896160070230 ) ) ;
#79161 = VERTEX_POINT ( 'NONE', #12232 ) ;
#79160 = B_SPLINE_CURVE_WITH_KNOTS ( 'NONE', 5,
 ( #77157, #40781, #67661, #41341, #74957, #75510 ),
 .UNSPECIFIED., .F., .F.,
 ( 6, 6 ),
 ( 0.000000000000000000, 1.000000000000000000 ),
 .UNSPECIFIED. ) ;
#79162 = CARTESIAN_POINT ( 'NONE',  ( 24.52819686174909819, 1440.913060387330006, 237.5178590015389943 ) ) ;
#79163 = CARTESIAN_POINT ( 'NONE',  ( -18.54934599400000295, 1509.628428428030020, 185.6625796504979746 ) ) ;
#79164 = ORIENTED_EDGE ( 'NONE', *, *, #36424, .T. ) ;
#79165 = CARTESIAN_POINT ( 'NONE',  ( -6.769697780263440379, 1509.032013233849966, 201.8557327794140122 ) ) ;
#79166 = CARTESIAN_POINT ( 'NONE',  ( -15.00074258620000123, 1410.809359295230024, 190.7496526661980170 ) ) ;
#79167 = CARTESIAN_POINT ( 'NONE',  ( -57.30544179059780419, 1379.717622275232316, 260.4455970689041351 ) ) ;
#79169 = CARTESIAN_POINT ( 'NONE',  ( 15.18091657867779887, 1512.335564144490036, 196.2297506243189957 ) ) ;
#79168 = CARTESIAN_POINT ( 'NONE',  ( -24.89939544960000006, 1440.978110081060095, 210.4300214544979895 ) ) ;
#79170 = CARTESIAN_POINT ( 'NONE',  ( -11.20854072740000085, 1414.996442553730049, 195.7122652358980304 ) ) ;
#79171 = B_SPLINE_CURVE_WITH_KNOTS ( 'NONE', 5,
 ( #10086, #96866, #10652, #36392, #54329, #45914, #44260, #19014, #80050 ),
 .UNSPECIFIED., .F., .F.,
 ( 6, 3, 6 ),
 ( 0.000000000000000000, 0.4153946668491772520, 1.000000000000000000 ),
 .UNSPECIFIED. ) ;
#79172 = CYLINDRICAL_SURFACE ( 'NONE', #20685, 0.9999999999999942268 ) ;
#79173 = CARTESIAN_POINT ( 'NONE',  ( -12.34777630145106464, 1434.274821752217804, 147.3832369842282333 ) ) ;
#79174 = CARTESIAN_POINT ( 'NONE',  ( -12.40409029009999919, 1434.420083644240094, 149.2722339323979952 ) ) ;
#79175 = CARTESIAN_POINT ( 'NONE',  ( 20.10060672000000181, 1435.200054686760041, 143.0090892206980016 ) ) ;
#79177 = DIRECTION ( 'NONE',  ( 0.6339197603454396202, 4.315842897467507453E-06, 0.7733988217116404273 ) ) ;
#79176 = CARTESIAN_POINT ( 'NONE',  ( 4.645519865709999863, 1464.326374023630024, 236.0120472652980084 ) ) ;
#79178 = CARTESIAN_POINT ( 'NONE',  ( 7.718134629434999283, 1516.881930554049859, 216.4517759834270123 ) ) ;
#79179 = CARTESIAN_POINT ( 'NONE',  ( 11.75869035672759999, 1517.151704408390060, 227.2994842695800060 ) ) ;
#79180 = CARTESIAN_POINT ( 'NONE',  ( 5.554947007364200218, 1511.433089852210060, 217.3313357707569935 ) ) ;
#79181 = CARTESIAN_POINT ( 'NONE',  ( 28.30178298809999760, 1508.659383665829864, 208.9628371413840000 ) ) ;
#79182 = CARTESIAN_POINT ( 'NONE',  ( 1.135460316954999938, 1516.790374942449944, 212.3751473514870156 ) ) ;
#79183 = CARTESIAN_POINT ( 'NONE',  ( -18.10327300539999840, 1416.823634022829992, 209.2064603946170109 ) ) ;
#79184 =( BOUNDED_CURVE ( )  B_SPLINE_CURVE ( 3, ( #22996, #4574, #74543, #22430 ),
 .UNSPECIFIED., .F., .F. ) 
 B_SPLINE_CURVE_WITH_KNOTS ( ( 4, 4 ),
 ( 2.995780018818399615, 3.061202631949359709 ),
 .UNSPECIFIED. ) 
 CURVE ( )  GEOMETRIC_REPRESENTATION_ITEM ( )  RATIONAL_B_SPLINE_CURVE ( ( 1.000000000000000000, 0.9996433552776613496, 0.9996433552776613496, 1.000000000000000000 ) ) 
 REPRESENTATION_ITEM ( '' )  );
#79185 = CARTESIAN_POINT ( 'NONE',  ( 30.95230591800835995, 1524.659802833170943, 221.7850325738306765 ) ) ;
#79187 = ORIENTED_EDGE ( 'NONE', *, *, #43955, .F. ) ;
#79186 = CARTESIAN_POINT ( 'NONE',  ( -98.66388059649999320, 1388.280417272740124, 297.3587652689590186 ) ) ;
#79188 = CARTESIAN_POINT ( 'NONE',  ( -16.54283724222759488, 1524.843178112495707, 237.3984430206447200 ) ) ;
#79189 = CARTESIAN_POINT ( 'NONE',  ( 22.11712025849999819, 1461.968260155829967, 248.4077083995979933 ) ) ;
#79190 = CARTESIAN_POINT ( 'NONE',  ( -17.73420755029999896, 1458.087872027529784, 230.3493948207980395 ) ) ;
#79191 = CARTESIAN_POINT ( 'NONE',  ( -14.16362978420000118, 1415.677402215299935, 203.9764128900390006 ) ) ;
#79192 = CARTESIAN_POINT ( 'NONE',  ( -5.668048117390779517, 1509.094485824230105, 237.7474958631910056 ) ) ;
#79193 = CARTESIAN_POINT ( 'NONE',  ( -22.47453833620000196, 1450.822336665940156, 220.0988823947979824 ) ) ;
#79195 = CARTESIAN_POINT ( 'NONE',  ( 19.01627661470000064, 1456.566751503029991, 225.7645316237980069 ) ) ;
#79194 = CARTESIAN_POINT ( 'NONE',  ( -21.72999032162606525, 1411.032272965445372, 201.5736073022784467 ) ) ;
#79196 = CARTESIAN_POINT ( 'NONE',  ( 0.2703785145419999592, 1470.804162800830227, 188.4112092155980065 ) ) ;
#79197 = CARTESIAN_POINT ( 'NONE',  ( -103.7134603450270021, 1379.995765815970117, 305.6207973536889995 ) ) ;
#79198 = ORIENTED_EDGE ( 'NONE', *, *, #75681, .F. ) ;
#79199 = CARTESIAN_POINT ( 'NONE',  ( 2.480813884984999884, 1517.051603658920158, 204.1089070683270279 ) ) ;
#79200 = CARTESIAN_POINT ( 'NONE',  ( 0.5499324067410000794, 1406.779957305129756, 269.6499793198979660 ) ) ;
#79201 = DIRECTION ( 'NONE',  ( -0.9786619618251657382, 0.000000000000000000, 0.2054769195713179730 ) ) ;
#79202 = CARTESIAN_POINT ( 'NONE',  ( 12.79131911510310005, 1470.700977594940014, 269.6259408100920041 ) ) ;
#79203 = CARTESIAN_POINT ( 'NONE',  ( 2.478710532469999617, 1435.788277702919913, 157.6232518516980008 ) ) ;
#79204 = CARTESIAN_POINT ( 'NONE',  ( -27.87287880750000113, 1445.634712502449929, 137.2901167009979986 ) ) ;
#79205 = B_SPLINE_CURVE_WITH_KNOTS ( 'NONE', 3,
 ( #101921, #16794, #75655, #109795, #24646, #84033, #7332, #110339, #33073, #101357, #17911, #50457, #85129, #42588, #84581, #76741, #58847, #35288, #52107, #92980, #53, #85681, #7873, #86237, #51544, #102476, #42041, #25765, #33611, #43696, #59964, #34734, #77850, #1158, #8978, #58298, #43149, #62746, #10084, #44819, #35851, #29098, #63284, #88456, #10650, #44258, #52656, #37496, #69474, #11209, #18459, #105820, #88991, #104696, #86793, #11743, #78400, #12279, #71702, #27433, #61616, #27991, #28547, #1711, #97398, #20667, #45912, #103594, #62176, #70035, #71132, #3370, #46473, #53215, #80048, #96864, #45372, #105253, #20133, #70579, #96303, #26894 ),
 .UNSPECIFIED., .F., .F.,
 ( 4, 2, 2, 1, 1, 1, 1, 2, 2, 2, 2, 1, 1, 1, 1, 1, 1, 2, 2, 2, 2, 2, 1, 1, 1, 1, 1, 1, 2, 2, 2, 2, 2, 2, 2, 1, 1, 1, 1, 1, 2, 2, 2, 2, 2, 1, 1, 1, 1, 1, 2, 2, 2, 4 ),
 ( 0.000000000000000000, 0.06249999999717108234, 0.09374999999575661658, 0.1093749999950493351, 0.1171874999947023904, 0.1210937499945289597, 0.1230468749944356316, 0.1240234374943823825, 0.1249999999943291334, 0.1874999999906900305, 0.2187499999888705138, 0.2343749999879550239, 0.2421874999875027745, 0.2460937499872765666, 0.2480468749871633793, 0.2490234374871120038, 0.2495117187370914924, 0.2497558593620759493, 0.2499999999870604062, 0.3124999999819546015, 0.3437499999793964811, 0.3593749999781175597, 0.3671874999774781267, 0.3710937499771584935, 0.3730468749769986769, 0.3740234374769187964, 0.3745117187268751091, 0.3747558593518534042, 0.3748779296643461323, 0.3749999999768389158, 0.4062499999757702707, 0.4374999999747016255, 0.4687499999736333134, 0.4843749999730991296, 0.4921874999728319544, 0.4960937499727078315, 0.4980468749726460476, 0.4990234374726151279, 0.4995117187226121858, 0.4997558593476237876, 0.4998779296601298938, 0.4999999999726359445, 0.6249999999793900418, 0.6874999999827670072, 0.7187499999844575438, 0.7343749999853008692, 0.7421874999857207555, 0.7460937499859289224, 0.7480468749860331723, 0.7490234374860871291, 0.7495117187361139965, 0.7499999999861407529, 0.8749999999930704320, 1.000000000000000000 ),
 .UNSPECIFIED. ) ;
#79206 = CARTESIAN_POINT ( 'NONE',  ( -45.22500823550609539, 1440.913060396110041, 265.7132613544649757 ) ) ;
#79207 = CARTESIAN_POINT ( 'NONE',  ( -26.18941195200000394, 1448.070469784879833, 137.2980963937980050 ) ) ;
#79208 = CARTESIAN_POINT ( 'NONE',  ( -11.41402561306639996, 1500.969831351809944, 208.5831151434670119 ) ) ;
#79209 = LINE ( 'NONE', #62423, #28832 ) ;
#79210 = CARTESIAN_POINT ( 'NONE',  ( 2.501005634817679901, 1448.957421962729995, 154.2481697353020138 ) ) ;
#79211 = CARTESIAN_POINT ( 'NONE',  ( 3.063200971469999701, 1505.793422128889915, 221.5342279770990217 ) ) ;
#79212 = CARTESIAN_POINT ( 'NONE',  ( -5.369110597919999783, 1438.274585814490138, 207.8054623959989726 ) ) ;
#79213 = ORIENTED_EDGE ( 'NONE', *, *, #50102, .T. ) ;
#79214 = CARTESIAN_POINT ( 'NONE',  ( 0.8115383875230000044, 1428.579607037230062, 149.5143047311979672 ) ) ;
#79215 = CARTESIAN_POINT ( 'NONE',  ( 2.203042164229999766, 1485.447018732490051, 198.5856978324989939 ) ) ;
#79216 = CARTESIAN_POINT ( 'NONE',  ( 8.093949986950837783, 1466.712779916819954, 203.1193089748180114 ) ) ;
#79217 = CARTESIAN_POINT ( 'NONE',  ( -0.7768863733780000391, 1475.978544761829880, 267.2347138124980006 ) ) ;
#79218 = B_SPLINE_CURVE_WITH_KNOTS ( 'NONE', 5,
 ( #72058, #3743, #79328, #106174, #97214, #37322 ),
 .UNSPECIFIED., .F., .F.,
 ( 6, 6 ),
 ( 239.1631355520000000, 244.0515247689999967 ),
 .UNSPECIFIED. ) ;
#79219 = DIRECTION ( 'NONE',  ( 0.9980318515193541407, 1.681712440757244397E-31, 0.06270903725022322628 ) ) ;
#79220 = CARTESIAN_POINT ( 'NONE',  ( -31.97743984922253446, 1525.878013734321030, 198.0760624713092284 ) ) ;
#79221 = CARTESIAN_POINT ( 'NONE',  ( 3.156166260290000025, 1466.544008048530031, 236.1241471695980181 ) ) ;
#79222 = CARTESIAN_POINT ( 'NONE',  ( -22.88685215929439920, 1384.853117157140105, 222.3623658345020146 ) ) ;
#79223 = CARTESIAN_POINT ( 'NONE',  ( -18.76071169450000298, 1415.996778985530000, 207.9585495669979878 ) ) ;
#79224 = CARTESIAN_POINT ( 'NONE',  ( 11.86919408122879993, 1432.567571621249954, 149.9818808296639929 ) ) ;
#79225 = CARTESIAN_POINT ( 'NONE',  ( 26.55522734722419997, 1435.968459176769784, 136.4840774741649909 ) ) ;
#79226 = CARTESIAN_POINT ( 'NONE',  ( -7.275039510604740300, 1396.167110366489851, 217.4379085327780103 ) ) ;
#79227 = CARTESIAN_POINT ( 'NONE',  ( -14.89068146630000022, 1422.385042061529930, 229.1196406006980055 ) ) ;
#79228 = CARTESIAN_POINT ( 'NONE',  ( -16.90423294166100021, 1409.877128282629883, 225.7261434717579789 ) ) ;
#79229 = CARTESIAN_POINT ( 'NONE',  ( 9.788350359310001636, 1441.600846913620217, 148.8293326998980035 ) ) ;
#79230 = VERTEX_POINT ( 'NONE', #106299 ) ;
#79231 = CARTESIAN_POINT ( 'NONE',  ( -11.39540616852265131, 1501.162789497870790, 208.1690291723011796 ) ) ;
#79232 = CARTESIAN_POINT ( 'NONE',  ( 2.425147433399999830, 1410.373299717429973, 231.7452901618979979 ) ) ;
#79233 = CARTESIAN_POINT ( 'NONE',  ( -1.254332932929999922, 1509.200097200889786, 218.0171177365190260 ) ) ;
#79235 = CARTESIAN_POINT ( 'NONE',  ( -9.962652008186671182, 1439.046469533959907, 209.4352736110479896 ) ) ;
#79234 = CARTESIAN_POINT ( 'NONE',  ( 10.49341911620000189, 1425.372128361229898, 101.9093738396979916 ) ) ;
#79236 = DIRECTION ( 'NONE',  ( -0.8090169943749507819, 0.000000000000000000, -0.5877852522924685852 ) ) ;
#79237 = CARTESIAN_POINT ( 'NONE',  ( -12.53380498098199602, 1442.773887284840612, 151.6125157144320212 ) ) ;
#79238 = B_SPLINE_CURVE_WITH_KNOTS ( 'NONE', 5,
 ( #81642, #4947, #39089, #99548, #22273, #90606 ),
 .UNSPECIFIED., .F., .F.,
 ( 6, 6 ),
 ( 0.000000000000000000, 1.000000000000000000 ),
 .UNSPECIFIED. ) ;
#79239 = CARTESIAN_POINT ( 'NONE',  ( 5.778999773775000293, 1516.955859323880077, 201.7887757972170277 ) ) ;
#79240 = CARTESIAN_POINT ( 'NONE',  ( 7.684424406179999778, 1424.938446056360135, 211.9182770897589876 ) ) ;
#79241 = CARTESIAN_POINT ( 'NONE',  ( -19.73707534100000061, 1467.795347597790169, 204.3773262252089751 ) ) ;
#79242 = FACE_OUTER_BOUND ( 'NONE', #79959, .T. ) ;
#79243 = CARTESIAN_POINT ( 'NONE',  ( 8.464772015878841316, 1522.051704408389924, 233.7053289272604104 ) ) ;
#79244 = CARTESIAN_POINT ( 'NONE',  ( 2.831794687379999953, 1449.370045669049887, 183.5403809041980026 ) ) ;
#79245 = CARTESIAN_POINT ( 'NONE',  ( 8.052903166426546022, 1365.111483269165774, 208.3718459617061285 ) ) ;
#79247 = ORIENTED_EDGE ( 'NONE', *, *, #32911, .F. ) ;
#79246 = CARTESIAN_POINT ( 'NONE',  ( -3.168849847270283959, 1464.840305569651491, 237.5147278964450948 ) ) ;
#79248 = ORIENTED_EDGE ( 'NONE', *, *, #5642, .F. ) ;
#79249 = ADVANCED_FACE ( 'NONE', ( #13867 ), #90590, .F. ) ;
#79250 = CARTESIAN_POINT ( 'NONE',  ( -41.48883687280000032, 1443.959535018250108, 136.5760642042980066 ) ) ;
#79251 = CARTESIAN_POINT ( 'NONE',  ( 0.1053863349198899957, 1507.126692871930118, 237.3870350735109866 ) ) ;
#79252 = CARTESIAN_POINT ( 'NONE',  ( 15.96958168569999970, 1519.913060387329779, 226.4768549569980109 ) ) ;
#79253 = CARTESIAN_POINT ( 'NONE',  ( -7.669726197924999767, 1510.984078637139874, 213.9427911786070240 ) ) ;
#79254 = CARTESIAN_POINT ( 'NONE',  ( -109.3833719510217293, 1306.483669372788654, 310.9930631313186495 ) ) ;
#79255 = CARTESIAN_POINT ( 'NONE',  ( 11.60004869885203682, 1426.786827912535728, 134.3786173235958472 ) ) ;
#79256 = CARTESIAN_POINT ( 'NONE',  ( 15.09047375999176843, 1517.051704408389924, 215.6125241866901661 ) ) ;
#79257 = EDGE_CURVE ( 'NONE', #99467, #32820, #21227, .T. ) ;
#79258 = DIRECTION ( 'NONE',  ( -0.2054769195713296581, 0.000000000000000000, 0.9786619618251632957 ) ) ;
#79259 = CARTESIAN_POINT ( 'NONE',  ( -2.500000000000000000, 1448.763984273669848, 157.0970650823900314 ) ) ;
#79260 = CARTESIAN_POINT ( 'NONE',  ( 6.662077426295040183, 1396.145705257569944, 217.9277218839869761 ) ) ;
#79261 = CARTESIAN_POINT ( 'NONE',  ( 3.460935634467220190, 1409.033918922830026, 194.4343271261309951 ) ) ;
#79262 = CARTESIAN_POINT ( 'NONE',  ( -3.834150157287569805, 1405.859129154519906, 267.5313358287059486 ) ) ;
#79263 = CARTESIAN_POINT ( 'NONE',  ( 40.26396426040000165, 1444.186530281040177, 137.1012295722979957 ) ) ;
#79264 = ORIENTED_EDGE ( 'NONE', *, *, #24897, .T. ) ;
#79265 = CARTESIAN_POINT ( 'NONE',  ( -11.57624701299999970, 1432.320296571700055, 151.1967064316980043 ) ) ;
#79266 = CARTESIAN_POINT ( 'NONE',  ( 11.79480876540000089, 1441.728078750129953, 187.9005510439980071 ) ) ;
#79267 = ORIENTED_EDGE ( 'NONE', *, *, #75380, .F. ) ;
#79268 = ORIENTED_EDGE ( 'NONE', *, *, #34941, .T. ) ;
#79269 = CARTESIAN_POINT ( 'NONE',  ( -3.980518584870000431, 1455.210856568990039, 200.5685208411690326 ) ) ;
#79270 = CARTESIAN_POINT ( 'NONE',  ( 9.971295257839999593, 1364.502667329740007, 207.6218459616989946 ) ) ;
#79271 = CARTESIAN_POINT ( 'NONE',  ( -7.714371541114999786, 1516.738222552470233, 214.9014490703569891 ) ) ;
#79272 = CARTESIAN_POINT ( 'NONE',  ( 2.325731103684999912, 1511.751588929339960, 216.7056378762670192 ) ) ;
#79273 = VERTEX_POINT ( 'NONE', #37997 ) ;
#79274 = CARTESIAN_POINT ( 'NONE',  ( 16.56647452670000220, 1428.020747124390027, 201.4090148566590130 ) ) ;
#79275 = CARTESIAN_POINT ( 'NONE',  ( -78.35932141380000360, 1379.348932152990074, 291.3894706377590182 ) ) ;
#79276 = EDGE_CURVE ( 'NONE', #103585, #87841, #106801, .T. ) ;
#79277 = CARTESIAN_POINT ( 'NONE',  ( -106.2764360894749984, 1378.913060387289988, 302.2763280471240250 ) ) ;
#79278 = CARTESIAN_POINT ( 'NONE',  ( 2.480187016714999970, 1517.025470194390209, 204.4964864072570094 ) ) ;
#79279 = CARTESIAN_POINT ( 'NONE',  ( -16.02094686025720094, 1507.732436784892116, 185.5304883000871428 ) ) ;
#79280 = CARTESIAN_POINT ( 'NONE',  ( -41.26944936248266771, 1435.051291618910000, 269.6336527597242707 ) ) ;
#79281 = CARTESIAN_POINT ( 'NONE',  ( 0.000000000000000000, 1450.913060387330006, 198.0847581327979867 ) ) ;
#79282 = CARTESIAN_POINT ( 'NONE',  ( -3.706743637329999785, 1410.419263482230235, 232.3104563135979959 ) ) ;
#79284 = ORIENTED_EDGE ( 'NONE', *, *, #105656, .T. ) ;
#79283 = CARTESIAN_POINT ( 'NONE',  ( -11.75640701318574699, 1511.791180387471059, 193.9413991097462997 ) ) ;
#79285 = CARTESIAN_POINT ( 'NONE',  ( 30.80316622530000004, 1451.837341253830118, 134.8070091183980139 ) ) ;
#79286 = DIRECTION ( 'NONE',  ( -1.000000000000000000, 0.000000000000000000, 0.000000000000000000 ) ) ;
#79287 = CARTESIAN_POINT ( 'NONE',  ( -13.36083802519999963, 1384.539077642469920, 218.9649430346489964 ) ) ;
#79288 = CARTESIAN_POINT ( 'NONE',  ( -4.860709314987225582, 1442.585814854372302, 201.1804672816271022 ) ) ;
#79289 = CARTESIAN_POINT ( 'NONE',  ( -25.47400523009999773, 1435.387084339240118, 135.4904355849980107 ) ) ;
#79290 = CARTESIAN_POINT ( 'NONE',  ( 24.79113421610179913, 1415.879394787770252, 269.6862526298410216 ) ) ;
#79291 = CARTESIAN_POINT ( 'NONE',  ( -2.282915221395000138, 1516.876240617270014, 211.6158662526670184 ) ) ;
#79292 = CARTESIAN_POINT ( 'NONE',  ( -66.43975051640001084, 1379.742919361219947, 275.2749399108590183 ) ) ;
#79293 = CARTESIAN_POINT ( 'NONE',  ( 0.01703802077549729579, 1507.628843765722650, 237.4425282897537386 ) ) ;
#79294 = CARTESIAN_POINT ( 'NONE',  ( 16.01085410965039912, 1427.818095826660056, 200.6391735007109673 ) ) ;
#79295 = CARTESIAN_POINT ( 'NONE',  ( -21.47380431054590133, 1487.892812373600009, 202.0847385657529856 ) ) ;
#79296 = CARTESIAN_POINT ( 'NONE',  ( -4.618583430005000601, 1516.939762005280045, 209.1349059721700030 ) ) ;
#79297 = ORIENTED_EDGE ( 'NONE', *, *, #87677, .F. ) ;
#79298 = CARTESIAN_POINT ( 'NONE',  ( 15.33708232923881987, 1509.448643104055918, 184.3329835401579260 ) ) ;
#79299 = CARTESIAN_POINT ( 'NONE',  ( -14.16989803769999945, 1420.440733405429910, 227.4201729013980184 ) ) ;
#79300 = CARTESIAN_POINT ( 'NONE',  ( -32.09327717010000214, 1384.955453299609871, 229.9590027138590074 ) ) ;
#79301 = ORIENTED_EDGE ( 'NONE', *, *, #105036, .F. ) ;
#79302 = CARTESIAN_POINT ( 'NONE',  ( -26.97945814876269921, 1385.247242750549958, 225.1983066302449856 ) ) ;
#79303 = CARTESIAN_POINT ( 'NONE',  ( -2.792418666239999681, 1429.036568613389818, 200.1755848472290040 ) ) ;
#79304 = CARTESIAN_POINT ( 'NONE',  ( 16.65976538191360135, 1469.007159623620055, 229.3912229546239985 ) ) ;
#79305 =( BOUNDED_CURVE ( )  B_SPLINE_CURVE ( 3, ( #103916, #33947, #86011, #102788 ),
 .UNSPECIFIED., .F., .T. ) 
 B_SPLINE_CURVE_WITH_KNOTS ( ( 4, 4 ),
 ( 4.424142070271249949, 5.579787944462250238 ),
 .UNSPECIFIED. ) 
 CURVE ( )  GEOMETRIC_REPRESENTATION_ITEM ( )  RATIONAL_B_SPLINE_CURVE ( ( 1.000000000000000000, 0.8917691662044565648, 0.8917691662044565648, 1.000000000000000000 ) ) 
 REPRESENTATION_ITEM ( '' )  );
#79306 = CARTESIAN_POINT ( 'NONE',  ( -22.73782236065209972, 1507.861788290109871, 224.9164081595820051 ) ) ;
#79307 = CARTESIAN_POINT ( 'NONE',  ( -1.802301037019999885, 1409.910657972530089, 186.0681197405980072 ) ) ;
#79308 = CARTESIAN_POINT ( 'NONE',  ( -0.2331143098109999812, 1408.921200918430031, 231.7611568695980111 ) ) ;
#79309 = CARTESIAN_POINT ( 'NONE',  ( -14.27756185697911029, 1416.835288273484821, 221.7190706085977467 ) ) ;
#79310 = AXIS2_PLACEMENT_3D ( 'NONE', #109513, #73156, #65322 ) ;
#79312 = CARTESIAN_POINT ( 'NONE',  ( 15.50537652237009922, 1477.920142942969960, 194.4487094663240043 ) ) ;
#79311 = CARTESIAN_POINT ( 'NONE',  ( -7.328049318385000177, 1516.809497469189864, 215.6772390872569929 ) ) ;
#79313 = CARTESIAN_POINT ( 'NONE',  ( 18.87980474539999776, 1507.654596655130035, 188.5454329983980131 ) ) ;
#79314 = CARTESIAN_POINT ( 'NONE',  ( 10.21479392009059950, 1470.289319449759887, 209.7510399118739883 ) ) ;
#79315 = ORIENTED_EDGE ( 'NONE', *, *, #8708, .F. ) ;
#79316 = CARTESIAN_POINT ( 'NONE',  ( -12.81185530964340025, 1416.835419214280137, 196.2456592538570135 ) ) ;
#79317 = CARTESIAN_POINT ( 'NONE',  ( -11.87933480400000086, 1508.913060324029857, 182.4413436122979988 ) ) ;
#79318 = ORIENTED_EDGE ( 'NONE', *, *, #76138, .T. ) ;
#79319 = CARTESIAN_POINT ( 'NONE',  ( 2.446918720040000217, 1417.581962241529936, 234.9465420055979905 ) ) ;
#79320 = B_SPLINE_CURVE_WITH_KNOTS ( 'NONE', 3,
 ( #103747, #26472, #94792, #110490, #52263, #16943, #60666, #751, #60108, #85838 ),
 .UNSPECIFIED., .F., .F.,
 ( 4, 2, 2, 2, 4 ),
 ( -2.055505557828499974, -1.540184857421819986, -1.025851360773140097, -0.5122551694543180378, 0.000000000000000000 ),
 .UNSPECIFIED. ) ;
#79321 = CARTESIAN_POINT ( 'NONE',  ( -20.92767404034537648, 1511.187213306747708, 182.8548762971666406 ) ) ;
#79322 = CARTESIAN_POINT ( 'NONE',  ( 3.007039662469999985, 1441.535621289990104, 218.1727171078889853 ) ) ;
#79323 = CARTESIAN_POINT ( 'NONE',  ( -33.52308185467866508, 1525.402221411349728, 200.6636391946740616 ) ) ;
#79324 = CARTESIAN_POINT ( 'NONE',  ( -16.57358609848514064, 1410.166789121471311, 191.9182324867213936 ) ) ;
#79325 = CARTESIAN_POINT ( 'NONE',  ( 4.363122647530000009, 1423.854802298929826, 172.2701767054979882 ) ) ;
#79326 = CARTESIAN_POINT ( 'NONE',  ( -18.16339525799999777, 1424.367498598930069, 225.5894832976980240 ) ) ;
#79327 = CARTESIAN_POINT ( 'NONE',  ( -18.07916955490000177, 1435.128322693429936, 145.8330392763979830 ) ) ;
#79328 = CARTESIAN_POINT ( 'NONE',  ( -19.70212423939999979, 1465.426585210689836, 207.1871696898290054 ) ) ;
#79329 = DIRECTION ( 'NONE',  ( -0.9455185755993182894, 0.000000000000000000, 0.3255681544571523145 ) ) ;
#79331 = CARTESIAN_POINT ( 'NONE',  ( 0.5620975284970839425, 1416.851343896850040, 190.4751211475700075 ) ) ;
#79330 = CARTESIAN_POINT ( 'NONE',  ( 0.5943821362729999613, 1416.311719779230089, 190.5346383329979858 ) ) ;
#79332 = CARTESIAN_POINT ( 'NONE',  ( 0.4151546846821905778, 1522.382868172863937, 244.9330574173806951 ) ) ;
#79333 = ORIENTED_EDGE ( 'NONE', *, *, #71060, .F. ) ;
#79334 = CARTESIAN_POINT ( 'NONE',  ( 1.325823199544269748, 1507.620489763490014, 186.1815209864240046 ) ) ;
#79335 = CARTESIAN_POINT ( 'NONE',  ( 26.96771577539999853, 1508.002232633729818, 206.7596878312280069 ) ) ;
#79336 = CARTESIAN_POINT ( 'NONE',  ( -24.09224057910000028, 1438.023770130810135, 211.8323676549379968 ) ) ;
#79337 = CARTESIAN_POINT ( 'NONE',  ( -5.090491209510000559, 1484.752177510490128, 198.8227071155990018 ) ) ;
#79338 = CARTESIAN_POINT ( 'NONE',  ( -16.67868778038742406, 1417.215853041899663, 207.0928179806824971 ) ) ;
#79339 = CARTESIAN_POINT ( 'NONE',  ( -30.31940284292399213, 1518.913060387330006, 222.4933038710547919 ) ) ;
#79340 = CARTESIAN_POINT ( 'NONE',  ( 5.312679136500000787, 1493.059131431590231, 218.8466398904690209 ) ) ;
#79341 = DIRECTION ( 'NONE',  ( -1.000000000000000000, 0.000000000000000000, 0.000000000000000000 ) ) ;
#79342 = CARTESIAN_POINT ( 'NONE',  ( -7.703229051499217661, 1511.126521620429685, 214.5635182500827511 ) ) ;
#79343 = CARTESIAN_POINT ( 'NONE',  ( -7.440906847757699616, 1489.915291769369787, 217.2245407447130106 ) ) ;
#79344 = CARTESIAN_POINT ( 'NONE',  ( 22.14279320874160106, 1473.984109767550081, 210.1089530530229865 ) ) ;
#79345 = CARTESIAN_POINT ( 'NONE',  ( -79.77560727129458940, 1383.777144559889848, 303.5005229431759517 ) ) ;
#79346 = CARTESIAN_POINT ( 'NONE',  ( -109.8098934281339893, 1384.480849638239988, 311.3605537058619461 ) ) ;
#79347 = DIRECTION ( 'NONE',  ( 0.000000000000000000, -1.000000000000000000, 0.000000000000000000 ) ) ;
#79348 = CARTESIAN_POINT ( 'NONE',  ( -2.152805114430509814, 1516.527314490149820, 201.4129972511030076 ) ) ;
#79350 = ORIENTED_EDGE ( 'NONE', *, *, #26356, .F. ) ;
#79349 = CARTESIAN_POINT ( 'NONE',  ( 21.50111106039999953, 1509.340465056330004, 190.1785649164980043 ) ) ;
#79351 = CARTESIAN_POINT ( 'NONE',  ( -8.775825618903727587, 1374.031200045389824, 204.3275905756569841 ) ) ;
#79352 = B_SPLINE_CURVE_WITH_KNOTS ( 'NONE', 3,
 ( #17229, #1590, #51426, #9422, #93414, #9972, #77192, #50345, #17787, #52543, #33493, #60393, #86675, #34067, #103464, #59841, #102367, #27322 ),
 .UNSPECIFIED., .F., .F.,
 ( 4, 2, 1, 1, 2, 2, 2, 1, 1, 2, 4 ),
 ( 0.5596618113830474917, 0.5734223797774827824, 0.5871829481719181842, 0.6147040849608105262, 0.6697463585384014761, 0.7798309056937928752, 0.7935914740879851381, 0.8073520424821772901, 0.8348731792705625931, 0.8899154528471214798, 1.000000000000000000 ),
 .UNSPECIFIED. ) ;
#79353 = CARTESIAN_POINT ( 'NONE',  ( -88.69635973610000690, 1381.890970305359815, 292.9935112231589756 ) ) ;
#79354 = CARTESIAN_POINT ( 'NONE',  ( 13.10606020890037016, 1517.151704408390060, 225.8214468947291493 ) ) ;
#79355 = ORIENTED_EDGE ( 'NONE', *, *, #84249, .F. ) ;
#79356 = ORIENTED_EDGE ( 'NONE', *, *, #87713, .F. ) ;
#79357 = CARTESIAN_POINT ( 'NONE',  ( -7.828738281090000584, 1492.799651794089868, 208.3779021618599927 ) ) ;
#79358 = CARTESIAN_POINT ( 'NONE',  ( -109.1656556500000050, 1384.956445634750025, 297.1328572680590128 ) ) ;
#79359 = CARTESIAN_POINT ( 'NONE',  ( 13.14376209273458329, 1443.062932975139347, 169.3993363818228488 ) ) ;
#79361 = CARTESIAN_POINT ( 'NONE',  ( 3.706798618510000143, 1486.448926241190065, 219.2581982017989901 ) ) ;
#79360 = CARTESIAN_POINT ( 'NONE',  ( 22.00315959510000141, 1506.810797420329891, 208.8865261091119976 ) ) ;
#79362 = B_SPLINE_CURVE_WITH_KNOTS ( 'NONE', 3,
 ( #5377, #108391, #108945, #90476 ),
 .UNSPECIFIED., .F., .F.,
 ( 4, 4 ),
 ( 0.000000000000000000, 0.0002220129587134773411 ),
 .UNSPECIFIED. ) ;
#79363 = CARTESIAN_POINT ( 'NONE',  ( 8.977937034530510729, 1435.738637591490033, 208.3987603176270227 ) ) ;
#79364 = CARTESIAN_POINT ( 'NONE',  ( -11.12212972500000063, 1433.940546708779948, 151.6712922175980225 ) ) ;
#79365 = CARTESIAN_POINT ( 'NONE',  ( 2.452021889690000123, 1486.921751305789940, 216.7943168417889979 ) ) ;
#79366 = CARTESIAN_POINT ( 'NONE',  ( -19.68929325700000277, 1486.263866003429939, 189.9954379505980171 ) ) ;
#79367 = CARTESIAN_POINT ( 'NONE',  ( 5.966377939340000047, 1409.624321257429983, 186.9574265255979810 ) ) ;
#79368 = DIRECTION ( 'NONE',  ( -1.755985294532469921E-16, 1.000000000000000000, -1.338183447452831989E-16 ) ) ;
#79369 = CARTESIAN_POINT ( 'NONE',  ( -12.84239781829999849, 1435.935717376499952, 150.8114785589980045 ) ) ;
#79370 = FACE_OUTER_BOUND ( 'NONE', #3366, .T. ) ;
#79371 = CARTESIAN_POINT ( 'NONE',  ( -16.41672048914309912, 1420.652106645439744, 203.2831381211010182 ) ) ;
#79372 = CARTESIAN_POINT ( 'NONE',  ( -9.452332281189999463, 1451.760532249029893, 152.6698088060980183 ) ) ;
#79373 = FACE_OUTER_BOUND ( 'NONE', #4892, .T. ) ;
#79374 = ORIENTED_EDGE ( 'NONE', *, *, #58460, .F. ) ;
#79375 = CARTESIAN_POINT ( 'NONE',  ( -13.02153297019999911, 1507.740364904889930, 209.3504333174379894 ) ) ;
#79376 = CARTESIAN_POINT ( 'NONE',  ( -5.367627633762589667, 1490.060063169970135, 185.8829590531140070 ) ) ;
#79377 = CARTESIAN_POINT ( 'NONE',  ( -44.43455565579999700, 1440.913065169949959, 270.0922445381979742 ) ) ;
#79378 = LINE ( 'NONE', #3246, #21215 ) ;
#79379 = CARTESIAN_POINT ( 'NONE',  ( 17.84751137929999842, 1410.898165765230260, 223.1918699671979880 ) ) ;
#79380 = FACE_OUTER_BOUND ( 'NONE', #21444, .T. ) ;
#79381 = B_SPLINE_CURVE_WITH_KNOTS ( 'NONE', 3,
 ( #27507, #53855, #3435, #52182, #18534, #37566, #26397, #71767, #1225, #79585, #86313, #17987, #1785, #53288, #45984, #60591, #2345, #52729, #104219, #44331, #11814, #95816, #9597, #77918, #70107, #87991, #10722, #2890, #35361, #54397, #103668, #69547, #96372, #19651, #88530, #80116, #26968, #61156, #95272, #105322 ),
 .UNSPECIFIED., .F., .F.,
 ( 4, 3, 3, 3, 3, 3, 3, 3, 3, 3, 3, 3, 3, 4 ),
 ( -25.42450308940000170, -24.37555945047400030, -23.28024511109189731, -22.14444905835580002, -20.97885384835930012, -19.74476178579540075, -18.44871831345919944, -17.06465298523080065, -15.53335940394270054, -12.73670746646559948, -11.09712870486940162, -9.657147941009078806, -8.324531407576071018, -7.064711944746168371 ),
 .UNSPECIFIED. ) ;
#79382 = CARTESIAN_POINT ( 'NONE',  ( 12.29727565780000020, 1497.713060387329961, 191.0778421084980039 ) ) ;
#79383 = FACE_OUTER_BOUND ( 'NONE', #84069, .T. ) ;
#79384 = CARTESIAN_POINT ( 'NONE',  ( -14.33548068480000026, 1422.080119723229927, 229.2153237933979710 ) ) ;
#79385 = CARTESIAN_POINT ( 'NONE',  ( -1.342620828053903592, 1484.506070987844851, 182.3616606809996483 ) ) ;
#79386 = CARTESIAN_POINT ( 'NONE',  ( 9.093835586129998205, 1363.023136422000107, 207.6218459616989946 ) ) ;
#79387 = CARTESIAN_POINT ( 'NONE',  ( -44.01834660311930492, 1430.717886937790126, 268.5615389372139816 ) ) ;
#79388 = CARTESIAN_POINT ( 'NONE',  ( 18.86688640473602874, 1511.187213306747708, 237.4611898188519774 ) ) ;
#79389 = ORIENTED_EDGE ( 'NONE', *, *, #90472, .F. ) ;
#79390 = CARTESIAN_POINT ( 'NONE',  ( -8.012082702599998996, 1424.887577014409999, 210.3493509962989947 ) ) ;
#79391 = CIRCLE ( 'NONE', #25715, 1.999999999999999556 ) ;
#79392 = EDGE_LOOP ( 'NONE', ( #15346, #64255, #110074, #7501 ) ) ;
#79393 = CARTESIAN_POINT ( 'NONE',  ( 0.007128837152181529378, 1517.006509894990131, 209.8686634857439799 ) ) ;
#79394 = CARTESIAN_POINT ( 'NONE',  ( 3.087661701989000029, 1369.842518917919961, 211.2713650144889925 ) ) ;
#79395 = CARTESIAN_POINT ( 'NONE',  ( -20.59684415610000130, 1507.762623716230109, 190.3921826404979925 ) ) ;
#79396 = CARTESIAN_POINT ( 'NONE',  ( -9.380213083140001018, 1425.410769174930010, 187.4587521971979811 ) ) ;
#79397 = AXIS2_PLACEMENT_3D ( 'NONE', #100603, #18663, #60720 ) ;
#79398 = LINE ( 'NONE', #96754, #80502 ) ;
#79399 = B_SPLINE_SURFACE_WITH_KNOTS ( 'NONE', 5, 5, ( 
 ( #86589, #18817, #87147, #10435, #61977, #96091, #4783, #6452, #5344 ),
 ( #65821, #73677, #82611, #99385, #107250, #64174, #91559, #5902, #83159 ),
 ( #55221, #22108, #38929, #56863, #29982, #106691, #90993, #89351, #107804 ),
 ( #98295, #73109, #14834, #47354, #89894, #21570, #12645, #80954, #39503 ),
 ( #74229, #90440, #30543, #97746, #46823, #14283, #48473, #64733, #40047 ),
 ( #49023, #40599, #21017, #65272, #56308, #81482, #108359, #23235, #63632 ),
 ( #82038, #31641, #98847, #38388, #22661, #4253, #13718, #74770, #108910 ),
 ( #99940, #57433, #72564, #55780, #13165, #47903, #31090, #32748, #24871 ),
 ( #33846, #15922, #93198, #51210, #42258, #17574, #41703, #68037, #25980 ) ),
 .UNSPECIFIED., .F., .F., .F.,
 ( 6, 3, 6 ),
 ( 6, 3, 6 ),
 ( 19.77745610209999683, 22.54012251900000052, 25.30278893590000067 ),
 ( 0.000000000000000000, 1.500000000000000000, 3.000000000000000000 ),
 .UNSPECIFIED. ) ;
#79400 = EDGE_LOOP ( 'NONE', ( #23296, #96620, #14345, #93774 ) ) ;
#79402 = CARTESIAN_POINT ( 'NONE',  ( 29.78220350812342332, 1526.382868172863937, 196.5089261231633202 ) ) ;
#79401 = CARTESIAN_POINT ( 'NONE',  ( -2.487421823092379913, 1523.954914175592194, 175.4471414341940942 ) ) ;
#79403 = CARTESIAN_POINT ( 'NONE',  ( 5.779627054084999216, 1516.977993847330026, 201.4011957967969977 ) ) ;
#79404 = B_SPLINE_CURVE_WITH_KNOTS ( 'NONE', 4,
 ( #94567, #7809, #103522, #17839, #9471 ),
 .UNSPECIFIED., .F., .F.,
 ( 5, 5 ),
 ( 3.613988937050000239, 5.260361675040000407 ),
 .UNSPECIFIED. ) ;
#79405 = CARTESIAN_POINT ( 'NONE',  ( -18.67521810751130218, 1508.457196392550031, 210.8041937590900261 ) ) ;
#79406 = CARTESIAN_POINT ( 'NONE',  ( 8.695521651920000039, 1472.655120818390060, 215.9601142780390148 ) ) ;
#79407 = CARTESIAN_POINT ( 'NONE',  ( -9.393416945061629164, 1439.826643058699801, 207.2591784000079826 ) ) ;
#79408 = ORIENTED_EDGE ( 'NONE', *, *, #81624, .T. ) ;
#79409 = CARTESIAN_POINT ( 'NONE',  ( -16.42979742323149850, 1412.363408827170133, 269.8873871863210070 ) ) ;
#79410 = CARTESIAN_POINT ( 'NONE',  ( -7.339107240745000205, 1517.203017563489766, 207.9963360818169917 ) ) ;
#79411 = CARTESIAN_POINT ( 'NONE',  ( -2.409586283469999923, 1426.663880916129983, 144.1938086916980239 ) ) ;
#79412 = CARTESIAN_POINT ( 'NONE',  ( -3.750000000000000000, 1524.051704408389924, 209.1218459616989946 ) ) ;
#79414 = EDGE_LOOP ( 'NONE', ( #107736, #90834, #16905, #20604, #59402, #108704 ) ) ;
#79413 = CARTESIAN_POINT ( 'NONE',  ( -7.690112133868802324, 1366.641875226467164, 207.6218459616988241 ) ) ;
#79415 = ORIENTED_EDGE ( 'NONE', *, *, #88448, .T. ) ;
#79416 = CARTESIAN_POINT ( 'NONE',  ( 42.06154873321850118, 1454.182881615767201, 269.0741535282402879 ) ) ;
#79417 = EDGE_CURVE ( 'NONE', #27144, #98691, #61648, .T. ) ;
#79418 = CARTESIAN_POINT ( 'NONE',  ( -0.3306155012354299871, 1467.554131235530122, 220.2123213960779822 ) ) ;
#79419 = CARTESIAN_POINT ( 'NONE',  ( 3.639664930319541636, 1424.874334646760644, 184.8560718889175121 ) ) ;
#79420 = CARTESIAN_POINT ( 'NONE',  ( 19.60792669039999936, 1475.100271358290229, 204.3343059087790152 ) ) ;
#79421 = B_SPLINE_CURVE_WITH_KNOTS ( 'NONE', 5,
 ( #83158, #32747, #107803, #108909, #66927, #66383, #31640, #6451, #65271 ),
 .UNSPECIFIED., .F., .F.,
 ( 6, 3, 6 ),
 ( 0.000000000000000000, 0.5000000000000001110, 1.000000000000000000 ),
 .UNSPECIFIED. ) ;
#79422 = COLOUR_RGB ( '', 0.40784314, 0.44705882, 0.49803922) ;
#79423 = CARTESIAN_POINT ( 'NONE',  ( -18.22757619631530090, 1415.441076447700198, 207.5675272910649767 ) ) ;
#79424 = CARTESIAN_POINT ( 'NONE',  ( -22.50079280529999792, 1430.784053779030046, 216.6565829457279904 ) ) ;
#79425 = CARTESIAN_POINT ( 'NONE',  ( 10.67568936471529994, 1475.522394824059802, 267.8226452972320430 ) ) ;
#79426 = CARTESIAN_POINT ( 'NONE',  ( -9.791756963356650800, 1464.727237775841331, 232.4252867197243120 ) ) ;
#79427 = CARTESIAN_POINT ( 'NONE',  ( 5.558723128650000511, 1446.585823782530042, 184.2862713098979839 ) ) ;
#79428 = CARTESIAN_POINT ( 'NONE',  ( 4.995725969715000048, 1516.651306816259876, 206.8263604310569690 ) ) ;
#79429 = EDGE_LOOP ( 'NONE', ( #91850, #101592, #82604, #18991 ) ) ;
#79430 = CARTESIAN_POINT ( 'NONE',  ( 18.75028616197712950, 1410.930186477558209, 221.9761678810336036 ) ) ;
#79431 = CARTESIAN_POINT ( 'NONE',  ( 1.473031652072160025, 1483.720148366529884, 182.1335069566439984 ) ) ;
#79432 = VERTEX_POINT ( 'NONE', #101735 ) ;
#79433 = CARTESIAN_POINT ( 'NONE',  ( -0.6472592568835300320, 1457.969941384779986, 229.6490092412300044 ) ) ;
#79434 = CARTESIAN_POINT ( 'NONE',  ( 26.11955021798470256, 1451.995689794530108, 135.1738199034059846 ) ) ;
#79435 = CARTESIAN_POINT ( 'NONE',  ( -13.02322703936409987, 1416.825784014559986, 196.6108461303639672 ) ) ;
#79436 = CARTESIAN_POINT ( 'NONE',  ( -39.74720592359999927, 1386.640108147219962, 212.4723510803390241 ) ) ;
#79437 = DIRECTION ( 'NONE',  ( 1.755985294532464991E-16, -1.000000000000000000, 1.338183447452830017E-16 ) ) ;
#79438 = CARTESIAN_POINT ( 'NONE',  ( 17.85589594940000424, 1410.900194280930009, 193.2270198764980194 ) ) ;
#79439 = CARTESIAN_POINT ( 'NONE',  ( 12.91247410300000276, 1445.052233488288948, 177.4417055768979026 ) ) ;
#79440 = CARTESIAN_POINT ( 'NONE',  ( 17.60627508980000044, 1410.895669370830092, 224.8086596393980017 ) ) ;
#79442 = CARTESIAN_POINT ( 'NONE',  ( -14.03675672165638311, 1379.586046047017817, 211.8650569067899880 ) ) ;
#79441 = CARTESIAN_POINT ( 'NONE',  ( -0.02516806119179999801, 1415.404723302029879, 233.4400559027980080 ) ) ;
#79443 = CARTESIAN_POINT ( 'NONE',  ( 1.074521542462559820, 1452.881655443580257, 183.3871671006969848 ) ) ;
#79444 = CARTESIAN_POINT ( 'NONE',  ( -7.880843563809999175, 1383.349707206300081, 218.7727698555990230 ) ) ;
#79445 = CARTESIAN_POINT ( 'NONE',  ( 7.331812085974999782, 1516.906641539930206, 215.6759973964769870 ) ) ;
#79446 = CARTESIAN_POINT ( 'NONE',  ( -32.86470158750932313, 1523.580203803270933, 217.2021180890991445 ) ) ;
#79447 = VERTEX_POINT ( 'NONE', #7689 ) ;
#79448 = FACE_OUTER_BOUND ( 'NONE', #7665, .T. ) ;
#79449 = CARTESIAN_POINT ( 'NONE',  ( -9.542478684123411270, 1481.357605987509942, 204.5426329703269914 ) ) ;
#79450 = CARTESIAN_POINT ( 'NONE',  ( -9.587265584406980068, 1483.699063712610041, 202.0552589649070114 ) ) ;
#79451 = EDGE_CURVE ( 'NONE', #81018, #71944, #29988, .T. ) ;
#79452 = CARTESIAN_POINT ( 'NONE',  ( 4.486733114842439640, 1517.051705360449887, 201.5292726349509849 ) ) ;
#79453 = EDGE_CURVE ( 'NONE', #67656, #51303, #84436, .T. ) ;
#79454 = CARTESIAN_POINT ( 'NONE',  ( -38.01811172100560299, 1448.806981927099969, 136.3823620645019901 ) ) ;
#79455 = EDGE_CURVE ( 'NONE', #81426, #85274, #77660, .T. ) ;
#79456 = CARTESIAN_POINT ( 'NONE',  ( -10.64712356781720004, 1462.974733331459902, 206.1443014032890062 ) ) ;
#79457 = CARTESIAN_POINT ( 'NONE',  ( 1.376676550539999851E-14, 1458.952956304630106, 234.3916895801979763 ) ) ;
#79458 = CARTESIAN_POINT ( 'NONE',  ( 45.67177343720949523, 1440.913060382069943, 266.1885934449759930 ) ) ;
#79459 = CARTESIAN_POINT ( 'NONE',  ( 11.41977517999999847, 1433.011620482069929, 151.3551162631979992 ) ) ;
#79460 = CARTESIAN_POINT ( 'NONE',  ( -44.70486280913989674, 1448.425642251100044, 269.0002212091439446 ) ) ;
#79461 = CARTESIAN_POINT ( 'NONE',  ( -9.594642682941978862, 1460.625312738239700, 210.3248870281339862 ) ) ;
#79462 = CARTESIAN_POINT ( 'NONE',  ( -21.92914334769999840, 1508.011510023030041, 226.2921371285980001 ) ) ;
#79463 = CARTESIAN_POINT ( 'NONE',  ( -17.68330801639999805, 1419.886192764050065, 207.3225218594289743 ) ) ;
#79464 = VERTEX_POINT ( 'NONE', #61437 ) ;
#79465 = CARTESIAN_POINT ( 'NONE',  ( -105.7715868071176004, 1391.141956858045887, 306.3730018047383510 ) ) ;
#79466 = VECTOR ( 'NONE', #68402, 1000.000000000000000 ) ;
#79467 = CARTESIAN_POINT ( 'NONE',  ( 15.56469051819999905, 1506.798305132829910, 225.0756798403980099 ) ) ;
#79468 = CARTESIAN_POINT ( 'NONE',  ( -4.703685162790000263, 1486.384485551830039, 182.0120322998980100 ) ) ;
#79469 = CARTESIAN_POINT ( 'NONE',  ( -5.775166187770511605, 1509.036904563493863, 201.6091405521827937 ) ) ;
#79470 = CARTESIAN_POINT ( 'NONE',  ( 12.07139996528260006, 1501.489333478010167, 211.6019455624989973 ) ) ;
#79471 = CARTESIAN_POINT ( 'NONE',  ( 24.42679094799999717, 1430.357408108330219, 211.6184629891579903 ) ) ;
#79472 = AXIS2_PLACEMENT_3D ( 'NONE', #105115, #90919, #14205 ) ;
#79473 = DIRECTION ( 'NONE',  ( -0.8672669759446666182, 0.000000000000000000, -0.4978433412588672557 ) ) ;
#79474 = CARTESIAN_POINT ( 'NONE',  ( -12.57479191030000010, 1509.295195185829925, 234.7571869286980188 ) ) ;
#79475 = CARTESIAN_POINT ( 'NONE',  ( -22.22211278303320015, 1383.851195146140071, 221.8019234694140209 ) ) ;
#79476 =( BOUNDED_CURVE ( )  B_SPLINE_CURVE ( 5, ( #9672, #87508, #10229, #11354, #97011, #69621, #35997, #105404, #28696, #1863, #62901, #54477, #53362, #79115, #88614, #44406, #3518, #37643, #96452, #78547, #104849, #105965, #61769, #19156, #2423, #36540, #70736, #62327, #98087, #81831, #82940, #72369, #12972, #64521, #91351, #14631, #39845, #72906, #106499, #4062, #99728, #38187, #13514, #108697, #21358, #48818, #40385, #63974, #107595, #31988, #55565, #12432, #29786, #98636, #21904, #38731, #89690, #22455, #6232, #66177, #46622, #74562, #47155, #81281, #80753, #65060, #47702, #89146, #5134, #4597, #5700, #39290, #107046, #23020, #30332, #20823, #56101, #90230 ),
 .UNSPECIFIED., .F., .F. ) 
 B_SPLINE_CURVE_WITH_KNOTS ( ( 6, 3, 3, 3, 3, 3, 3, 3, 3, 3, 3, 3, 3, 3, 3, 3, 3, 3, 3, 3, 3, 3, 3, 3, 3, 6 ),
 ( 0.03051383316186220829, 3.902585213099999617, 6.240861926940000082, 6.790072646650000543, 8.377982366400001268, 8.928580102349998882, 10.97133995140000096, 12.98949692179999893, 13.60228008900000063, 15.24737252870000148, 15.86745694640000259, 18.51059426890000026, 22.57641725190000059, 26.75087197449999721, 31.16005629229999840, 33.90953505430000092, 34.60237748540000524, 36.31249047570000243, 36.97255805550000218, 38.99052022429999909, 41.04947707190000017, 41.62972334150000364, 43.19545136810000230, 43.76106149099999953, 46.17824368760000908, 50.04091111600000374 ),
 .UNSPECIFIED. ) 
 CURVE ( )  GEOMETRIC_REPRESENTATION_ITEM ( )  RATIONAL_B_SPLINE_CURVE ( ( 0.2500000000000000000, 0.2500000000000000000, 0.2500000000000000000, 0.2500000000000000000, 0.2500000000000000000, 0.2500000000000000000, 0.2500000000000000000, 0.2500000000000000000, 0.2500000000000000000, 0.2500000000000000000, 0.2500000000000000000, 0.2500000000000000000, 0.2500000000000000000, 0.2500000000000000000, 0.2500000000000000000, 0.2500000000000000000, 0.2500000000000000000, 0.2500000000000000000, 0.2500000000000000000, 0.2500000000000000000, 0.2500000000000000000, 0.2500000000000000000, 0.2500000000000000000, 0.2500000000000000000, 0.2500000000000000000, 0.2500000000000000000, 0.2500000000000000000, 0.2500000000000000000, 0.2500000000000000000, 0.2500000000000000000, 0.2500000000000000000, 0.2500000000000000000, 0.2500000000000000000, 0.2500000000000000000, 0.2500000000000000000, 0.2500000000000000000, 0.2500000000000000000, 0.2500000000000000000, 0.2500000000000000000, 0.2500000000000000000, 0.2500000000000000000, 0.2500000000000000000, 0.2500000000000000000, 0.2500000000000000000, 0.2500000000000000000, 0.2500000000000000000, 0.2500000000000000000, 0.2500000000000000000, 0.2500000000000000000, 0.2500000000000000000, 0.2500000000000000000, 0.2500000000000000000, 0.2500000000000000000, 0.2500000000000000000, 0.2500000000000000000, 0.2500000000000000000, 0.2500000000000000000, 0.2500000000000000000, 0.2500000000000000000, 0.2500000000000000000, 0.2500000000000000000, 0.2500000000000000000, 0.2500000000000000000, 0.2500000000000000000, 0.2500000000000000000, 0.2500000000000000000, 0.2500000000000000000, 0.2500000000000000000, 0.2500000000000000000, 0.2500000000000000000, 0.2500000000000000000, 0.2500000000000000000, 0.2500000000000000000, 0.2500000000000000000, 0.2500000000000000000, 0.2500000000000000000, 0.2500000000000000000, 0.2500000000000000000 ) ) 
 REPRESENTATION_ITEM ( '' )  );
#79477 = CARTESIAN_POINT ( 'NONE',  ( -4.492641829143109611, 1508.880977751779938, 206.0044442880380018 ) ) ;
#79478 = DIRECTION ( 'NONE',  ( -0.9455185755993178454, 0.000000000000000000, 0.3255681544571537578 ) ) ;
#79479 = ADVANCED_FACE ( 'NONE', ( #34546 ), #27811, .F. ) ;
#79480 = CARTESIAN_POINT ( 'NONE',  ( 203.9558787908000284, -8382.262153571269664, -1760.903728536709878 ) ) ;
#79481 = CARTESIAN_POINT ( 'NONE',  ( 8.971908151997389780, 1451.470056219970047, 211.4421882215459902 ) ) ;
#79483 = ORIENTED_EDGE ( 'NONE', *, *, #51660, .T. ) ;
#79482 = CARTESIAN_POINT ( 'NONE',  ( 3.289090359600000291, 1441.224765589789968, 218.4797294130789851 ) ) ;
#79484 = CARTESIAN_POINT ( 'NONE',  ( -16.68463233076019492, 1445.052233488289630, 162.0935120523188857 ) ) ;
#79485 = CARTESIAN_POINT ( 'NONE',  ( -8.346053580011268735, 1386.932765083509366, 199.8874523339913765 ) ) ;
#79486 = CARTESIAN_POINT ( 'NONE',  ( -4.912638278920000268, 1474.545047148890035, 199.2507986654790102 ) ) ;
#79488 = ORIENTED_EDGE ( 'NONE', *, *, #73247, .T. ) ;
#79487 = CARTESIAN_POINT ( 'NONE',  ( -38.02701353892550173, 1450.427746997079794, 134.0999999984749991 ) ) ;
#79489 = FACE_OUTER_BOUND ( 'NONE', #79008, .T. ) ;
#79490 = EDGE_LOOP ( 'NONE', ( #107258, #83856, #76128, #107766 ) ) ;
#79491 = EDGE_CURVE ( 'NONE', #99599, #18619, #35053, .T. ) ;
#79492 = CARTESIAN_POINT ( 'NONE',  ( -12.31705391887590118, 1391.331872793070033, 211.5890497232870189 ) ) ;
#79493 = CARTESIAN_POINT ( 'NONE',  ( -3.866774376410000436, 1489.349301186990033, 188.6533245077989989 ) ) ;
#79494 = CARTESIAN_POINT ( 'NONE',  ( 33.36586802512179162, 1512.187213306747481, 216.3367586934468818 ) ) ;
#79495 = EDGE_CURVE ( 'NONE', #22249, #14981, #33492, .T. ) ;
#79496 = CARTESIAN_POINT ( 'NONE',  ( 17.10950584751149961, 1472.077583655310036, 198.3318500205459998 ) ) ;
#79497 = CARTESIAN_POINT ( 'NONE',  ( -3.117383295799999843, 1432.833160025789994, 217.3708154071790091 ) ) ;
#79498 = CARTESIAN_POINT ( 'NONE',  ( -14.74045126690000096, 1418.924813655680055, 213.5838659850790009 ) ) ;
#79499 = CARTESIAN_POINT ( 'NONE',  ( 9.257676694381489213, 1409.236345580020043, 220.8738777432600102 ) ) ;
#79500 = DIRECTION ( 'NONE',  ( -9.551066682124683589E-08, 1.946171191268429024E-07, -0.9999999999999764633 ) ) ;
#79501 = CARTESIAN_POINT ( 'NONE',  ( -104.2741735075869940, 1385.231329888970095, 296.8622915881020390 ) ) ;
#79502 = CARTESIAN_POINT ( 'NONE',  ( -18.11586804879999946, 1430.614621825330005, 192.0644440209979962 ) ) ;
#79503 = CARTESIAN_POINT ( 'NONE',  ( 10.03481087325400090, 1426.170452349230118, 208.8300883510670189 ) ) ;
#79504 = EDGE_CURVE ( 'NONE', #71507, #97242, #33646, .T. ) ;
#79505 = CARTESIAN_POINT ( 'NONE',  ( 11.65430695225310131, 1491.292500647989982, 207.0498289997640029 ) ) ;
#79507 = VERTEX_POINT ( 'NONE', #18282 ) ;
#79506 = DIRECTION ( 'NONE',  ( 0.03489949694567519994, 0.9993908270106039993, -7.428258325848019394E-09 ) ) ;
#79508 = ORIENTED_EDGE ( 'NONE', *, *, #80218, .F. ) ;
#79510 = AXIS2_PLACEMENT_3D ( 'NONE', #33000, #101849, #93455 ) ;
#79509 = CARTESIAN_POINT ( 'NONE',  ( 18.37311908421290241, 1459.092070059970183, 227.7653000740450011 ) ) ;
#79511 = CARTESIAN_POINT ( 'NONE',  ( -11.21624399399999916, 1434.255326149100028, 151.6033521221980038 ) ) ;
#79512 = CARTESIAN_POINT ( 'NONE',  ( 29.52276419461297152, 1509.964122545872442, 211.6544716486868367 ) ) ;
#79513 = CARTESIAN_POINT ( 'NONE',  ( 12.27763887519870067, 1427.216651625929899, 207.3866983009849889 ) ) ;
#79514 = CARTESIAN_POINT ( 'NONE',  ( 5.086366865409999605, 1397.753027540630001, 221.1576708939979881 ) ) ;
#79515 = CARTESIAN_POINT ( 'NONE',  ( 31.92299894892067513, 1524.776010967693537, 201.5796163247183870 ) ) ;
#79516 = CARTESIAN_POINT ( 'NONE',  ( -6.287493054558040306, 1516.709230591747882, 213.2274840498923254 ) ) ;
#79517 = CARTESIAN_POINT ( 'NONE',  ( -1.192273007929999906, 1462.370957484029987, 183.1676254752979958 ) ) ;
#79518 = CARTESIAN_POINT ( 'NONE',  ( -11.16589708279419391, 1364.318862766833718, 210.6218459617030021 ) ) ;
#79519 = DIRECTION ( 'NONE',  ( -0.8236474686107856380, -0.5669078173018518019, -0.01484500364079635246 ) ) ;
#79520 = CARTESIAN_POINT ( 'NONE',  ( -7.726331963605000297, 1517.194972660189933, 206.8303316343270239 ) ) ;
#79521 = CARTESIAN_POINT ( 'NONE',  ( -12.92355159029609979, 1434.740261887239967, 149.3124598003599885 ) ) ;
#79522 = B_SPLINE_SURFACE_WITH_KNOTS ( 'NONE', 4, 5, ( 
 ( #2016, #103320, #18218, #10381, #36152, #70336 ),
 ( #5295, #99333, #97702, #39453, #37253, #79819 ),
 ( #3125, #13120, #65222, #38881, #73626, #56257 ),
 ( #106644, #38336, #89303, #81427, #47303, #89848 ),
 ( #54629, #88762, #71993, #12599, #73062, #64681 ) ),
 .UNSPECIFIED., .F., .F., .F.,
 ( 5, 5 ),
 ( 6, 6 ),
 ( 9.410946460789999080, 10.17443977840000002 ),
 ( 0.000000000000000000, 2.000000000000000000 ),
 .UNSPECIFIED. ) ;
#79523 = CARTESIAN_POINT ( 'NONE',  ( 19.39983987835422496, 1522.382868172863937, 239.2921289694223219 ) ) ;
#79524 = CARTESIAN_POINT ( 'NONE',  ( 19.61399504222830004, 1475.927339034750048, 226.7148328204089864 ) ) ;
#79525 = CARTESIAN_POINT ( 'NONE',  ( -14.85004060048409968, 1489.439381932599872, 194.1045853035489870 ) ) ;
#79526 = B_SPLINE_CURVE_WITH_KNOTS ( 'NONE', 5,
 ( #107710, #31544, #57875, #33195, #65721, #58419 ),
 .UNSPECIFIED., .F., .F.,
 ( 6, 6 ),
 ( 0.000000000000000000, 1.000000000000000000 ),
 .UNSPECIFIED. ) ;
#79527 = CARTESIAN_POINT ( 'NONE',  ( 41.32873071537510157, 1444.134764045589918, 136.5772078548479840 ) ) ;
#79528 = ORIENTED_EDGE ( 'NONE', *, *, #59039, .T. ) ;
#79529 = CARTESIAN_POINT ( 'NONE',  ( 6.526375164530000106, 1408.296884814930081, 262.4989465380980391 ) ) ;
#79530 = CARTESIAN_POINT ( 'NONE',  ( -26.53391208829999925, 1488.685287628730066, 204.7973103800780166 ) ) ;
#79532 = CARTESIAN_POINT ( 'NONE',  ( -0.8911603994707960608, 1507.483750189549937, 231.9683985349379896 ) ) ;
#79531 = CARTESIAN_POINT ( 'NONE',  ( -10.42417239279969898, 1425.389265345479998, 97.52672419341850230 ) ) ;
#79533 = CARTESIAN_POINT ( 'NONE',  ( 7.337793712495000342, 1517.145312756229941, 211.9940546803969994 ) ) ;
#79534 = DIRECTION ( 'NONE',  ( 0.9455185755993178454, 0.000000000000000000, -0.3255681544571539243 ) ) ;
#79535 = CARTESIAN_POINT ( 'NONE',  ( -35.93744546429999787, 1433.966419625349999, 254.6052901707979572 ) ) ;
#79536 = CARTESIAN_POINT ( 'NONE',  ( 15.69795926444620271, 1517.151704408390060, 222.7678737639049871 ) ) ;
#79537 = CARTESIAN_POINT ( 'NONE',  ( 29.47598808511030199, 1509.906165459849944, 209.6382085403890017 ) ) ;
#79538 = CARTESIAN_POINT ( 'NONE',  ( -15.69795926856320101, 1521.951704408389787, 195.4758181589010064 ) ) ;
#79539 = CARTESIAN_POINT ( 'NONE',  ( 31.78277078219999296, 1450.942628683829980, 136.2347627311980034 ) ) ;
#79540 = VERTEX_POINT ( 'NONE', #10452 ) ;
#79541 = CARTESIAN_POINT ( 'NONE',  ( -2.500000000000000000, 1432.254430813080035, 157.4928808715980040 ) ) ;
#79542 = CARTESIAN_POINT ( 'NONE',  ( 14.79241649771974743, 1514.564622118912894, 225.3747096568645816 ) ) ;
#79543 = CARTESIAN_POINT ( 'NONE',  ( -3.829620113920000346, 1515.551704408389924, 206.7917118429090237 ) ) ;
#79544 = VERTEX_POINT ( 'NONE', #8781 ) ;
#79545 = EDGE_LOOP ( 'NONE', ( #60847, #55181, #81636, #90233 ) ) ;
#79546 = VECTOR ( 'NONE', #18957, 1000.000000000000227 ) ;
#79547 = CARTESIAN_POINT ( 'NONE',  ( 9.261703887511778532, 1452.295026765300008, 211.0154049713290192 ) ) ;
#79548 = CARTESIAN_POINT ( 'NONE',  ( -22.71348251198360302, 1409.706229765729859, 208.9920888512519923 ) ) ;
#79549 = ADVANCED_FACE ( 'NONE', ( #9897 ), #32716, .F. ) ;
#79550 = VERTEX_POINT ( 'NONE', #53588 ) ;
#79551 = CARTESIAN_POINT ( 'NONE',  ( -2.469737631213410278, 1507.227429411520006, 221.7265308815400147 ) ) ;
#79552 = CARTESIAN_POINT ( 'NONE',  ( -9.670206149040000199, 1461.150141550089984, 208.5232313836649780 ) ) ;
#79553 = ADVANCED_FACE ( 'NONE', ( #62557 ), #44241, .T. ) ;
#79554 = AXIS2_PLACEMENT_3D ( 'NONE', #80821, #106568, #81903 ) ;
#79555 = DIRECTION ( 'NONE',  ( -7.436362843295819681E-17, 1.000000000000000000, -1.457576885956999882E-16 ) ) ;
#79556 = VECTOR ( 'NONE', #11864, 1000.000000000000000 ) ;
#79557 = CARTESIAN_POINT ( 'NONE',  ( -15.00193899359999961, 1489.054902418029997, 230.6310622563979962 ) ) ;
#79558 = CARTESIAN_POINT ( 'NONE',  ( 6.140127931138819939, 1508.880864730590019, 201.6144229198349933 ) ) ;
#79559 = ORIENTED_EDGE ( 'NONE', *, *, #98768, .T. ) ;
#79560 = CARTESIAN_POINT ( 'NONE',  ( 11.73702549210000079, 1426.695992139529835, 144.1699184469979969 ) ) ;
#79561 = DIRECTION ( 'NONE',  ( -0.9417419115949053898, 0.3363363969979660806, 0.000000000000000000 ) ) ;
#79562 = CARTESIAN_POINT ( 'NONE',  ( -108.8816724165859995, 1384.900720007879954, 297.1232481292220200 ) ) ;
#79563 = ORIENTED_EDGE ( 'NONE', *, *, #73548, .T. ) ;
#79564 = CARTESIAN_POINT ( 'NONE',  ( 4.030514512585000375, 1516.901952101700090, 204.4990030879170320 ) ) ;
#79565 = VERTEX_POINT ( 'NONE', #66813 ) ;
#79566 = CARTESIAN_POINT ( 'NONE',  ( 11.86374746855640083, 1432.171576367579974, 149.9798746170999948 ) ) ;
#79567 = EDGE_CURVE ( 'NONE', #77824, #59860, #29696, .T. ) ;
#79568 = CARTESIAN_POINT ( 'NONE',  ( 13.37674189238196831, 1444.464913678520134, 187.6830941488352948 ) ) ;
#79569 = ORIENTED_EDGE ( 'NONE', *, *, #62533, .T. ) ;
#79570 = ORIENTED_EDGE ( 'NONE', *, *, #81012, .F. ) ;
#79571 = CARTESIAN_POINT ( 'NONE',  ( -15.76866869242515889, 1506.436298853504013, 193.8022778273726203 ) ) ;
#79572 = CARTESIAN_POINT ( 'NONE',  ( -4.767896964821690453, 1508.551704797160028, 219.9121068361049822 ) ) ;
#79573 = CARTESIAN_POINT ( 'NONE',  ( 8.908297959360000462, 1507.934933949130027, 234.8994657747980170 ) ) ;
#79574 = CARTESIAN_POINT ( 'NONE',  ( -9.699736313928079667, 1472.031488563110088, 212.1561346718199843 ) ) ;
#79575 = CARTESIAN_POINT ( 'NONE',  ( 21.12668385848170161, 1452.175300330200116, 141.8024459500680052 ) ) ;
#79576 = CARTESIAN_POINT ( 'NONE',  ( 3.148011791780000124, 1408.641849370629870, 270.4279803160980009 ) ) ;
#79577 = CARTESIAN_POINT ( 'NONE',  ( -109.1450416020000063, 1385.242479493820156, 297.1468691531589457 ) ) ;
#79578 = CARTESIAN_POINT ( 'NONE',  ( -6.386479664280000357, 1475.602365189490001, 200.9502241406889880 ) ) ;
#79579 = CARTESIAN_POINT ( 'NONE',  ( -2.187611056739820370, 1421.597788280269924, 193.5642244024440117 ) ) ;
#79580 = FACE_OUTER_BOUND ( 'NONE', #14930, .T. ) ;
#79581 = CARTESIAN_POINT ( 'NONE',  ( 8.936510400883047822, 1425.002876951823964, 195.6473277186463520 ) ) ;
#79583 = CARTESIAN_POINT ( 'NONE',  ( 14.36570857389999922, 1435.002040243630063, 195.7737178941980005 ) ) ;
#79582 = CARTESIAN_POINT ( 'NONE',  ( -18.11269319780000231, 1504.989642490190136, 208.9951304212659977 ) ) ;
#79584 = CARTESIAN_POINT ( 'NONE',  ( -29.90839080445297782, 1379.722162689491142, 217.8816187646463902 ) ) ;
#79585 = CARTESIAN_POINT ( 'NONE',  ( 17.94842024908709632, 1421.978012596150165, 225.1306823722440242 ) ) ;
#79586 = CARTESIAN_POINT ( 'NONE',  ( -6.809551170575000256, 1512.240414293130016, 201.8588037525169909 ) ) ;
#79587 = EDGE_LOOP ( 'NONE', ( #55160, #75263, #103753, #4186 ) ) ;
#79588 = CARTESIAN_POINT ( 'NONE',  ( 18.93537658700000037, 1413.766156166430164, 268.3665355202980436 ) ) ;
#79589 = PLANE ( 'NONE',  #40842 ) ;
#79590 = CARTESIAN_POINT ( 'NONE',  ( -74.95997362772719441, 1385.008095471610204, 300.0149541100690271 ) ) ;
#79591 = CARTESIAN_POINT ( 'NONE',  ( -20.85167258424259629, 1525.730671215490020, 234.0535516931209656 ) ) ;
#79593 = EDGE_CURVE ( 'NONE', #54152, #77692, #21992, .T. ) ;
#79592 = AXIS2_PLACEMENT_3D ( 'NONE', #34221, #43190, #76780 ) ;
#79594 = CARTESIAN_POINT ( 'NONE',  ( -8.162204519790000390, 1384.930475412839996, 199.6393846580689910 ) ) ;
#79595 = CARTESIAN_POINT ( 'NONE',  ( -14.80753115500000128, 1415.677402202029953, 211.4744607310090032 ) ) ;
#79597 = ORIENTED_EDGE ( 'NONE', *, *, #32618, .T. ) ;
#79596 = CARTESIAN_POINT ( 'NONE',  ( 12.76115332701539984, 1421.043083730220133, 203.4305847601519872 ) ) ;
#79598 = CARTESIAN_POINT ( 'NONE',  ( -16.66450378662129950, 1418.448320473469948, 203.1257116146589965 ) ) ;
#79599 = CARTESIAN_POINT ( 'NONE',  ( -24.29684349240000074, 1443.814603648100046, 211.2876295167179705 ) ) ;
#79600 = CARTESIAN_POINT ( 'NONE',  ( -15.92611295390000059, 1415.966327314990167, 209.5991268886040189 ) ) ;
#79601 = CARTESIAN_POINT ( 'NONE',  ( -1.736489803575699931, 1429.592721204729969, 199.8987770947680076 ) ) ;
#79602 = CARTESIAN_POINT ( 'NONE',  ( 18.42577555256999844, 1424.509265906519886, 223.4215472205989954 ) ) ;
#79603 = CARTESIAN_POINT ( 'NONE',  ( 0.1955981720603170160, 1416.913060341699975, 225.1861339145730199 ) ) ;
#79604 = AXIS2_PLACEMENT_3D ( 'NONE', #74019, #108154, #93541 ) ;
#79605 = CARTESIAN_POINT ( 'NONE',  ( 21.81700915577159705, 1509.753451845790096, 229.9156308900480212 ) ) ;
#79606 = CARTESIAN_POINT ( 'NONE',  ( 13.28372496219609822, 1428.987819674619914, 222.1683325723000166 ) ) ;
#79607 = CARTESIAN_POINT ( 'NONE',  ( 11.97075771579980596, 1433.593156705993579, 149.8706697297947699 ) ) ;
#79608 = CARTESIAN_POINT ( 'NONE',  ( 16.42992099730000177, 1412.750267290230113, 226.7405470936979839 ) ) ;
#79609 = ADVANCED_FACE ( 'NONE', ( #90880 ), #108789, .T. ) ;
#79610 = CARTESIAN_POINT ( 'NONE',  ( -3.527120678209999749, 1475.290298288389977, 218.8061202455889998 ) ) ;
#79611 = CARTESIAN_POINT ( 'NONE',  ( -15.80102657300000146, 1459.267675803429938, 229.9937850598980162 ) ) ;
#79612 = CARTESIAN_POINT ( 'NONE',  ( -2.494020320564999782, 1516.876240617270014, 206.8389307488369866 ) ) ;
#79613 = CARTESIAN_POINT ( 'NONE',  ( 45.85460769310000018, 1438.922387676499966, 268.7562792744979561 ) ) ;
#79614 = CARTESIAN_POINT ( 'NONE',  ( -18.14294508140000062, 1410.043204499329931, 224.1267514446980158 ) ) ;
#79615 = CARTESIAN_POINT ( 'NONE',  ( 22.42231863760000010, 1436.510268101429801, 142.5443955390980193 ) ) ;
#79616 = B_SPLINE_SURFACE_WITH_KNOTS ( 'NONE', 5, 5, ( 
 ( #13409, #5593, #73907, #31329, #54370, #80089 ),
 ( #83942, #16166, #7242, #58752, #8328, #101827 ),
 ( #14523, #85037, #42492, #76104, #66626, #83383 ),
 ( #76648, #75014, #57673, #67719, #93436, #82835 ),
 ( #15062, #109164, #110800, #34091, #74468, #32977 ),
 ( #57117, #41403, #49811, #58205, #25120, #68284 ) ),
 .UNSPECIFIED., .F., .F., .F.,
 ( 6, 6 ),
 ( 6, 6 ),
 ( 7.548656686150459372, 12.57640183258060063 ),
 ( 0.000000000000000000, 0.5000176499934829710 ),
 .UNSPECIFIED. ) ;
#79617 = CARTESIAN_POINT ( 'NONE',  ( 22.18897252830000255, 1508.010880766430091, 192.3772255266979982 ) ) ;
#79618 = EDGE_CURVE ( 'NONE', #61077, #20210, #80037, .T. ) ;
#79619 = CARTESIAN_POINT ( 'NONE',  ( 23.78270988279999898, 1434.944176083839920, 215.5045224494480181 ) ) ;
#79620 = CARTESIAN_POINT ( 'NONE',  ( -13.74068978706669952, 1379.630235450999862, 208.0692380938309896 ) ) ;
#79621 = CARTESIAN_POINT ( 'NONE',  ( 12.78776258870000149, 1416.851343894929869, 222.7045348337980215 ) ) ;
#79622 = CARTESIAN_POINT ( 'NONE',  ( -15.52550892592270060, 1418.207173107500012, 203.0520299323999893 ) ) ;
#79623 = CARTESIAN_POINT ( 'NONE',  ( -35.70148625528900510, 1436.782343446300047, 136.4713999753330143 ) ) ;
#79624 = CARTESIAN_POINT ( 'NONE',  ( -19.47833338605401821, 1506.473666148849816, 198.8548778393590624 ) ) ;
#79625 = CARTESIAN_POINT ( 'NONE',  ( -15.42329654610000134, 1414.772672120240031, 208.8174072822980065 ) ) ;
#79626 = CARTESIAN_POINT ( 'NONE',  ( -13.34543549089999992, 1442.214279694210063, 188.2228390031980041 ) ) ;
#79627 = CARTESIAN_POINT ( 'NONE',  ( -27.85054259011099731, 1508.556494693910054, 210.5418393889420088 ) ) ;
#79628 = CARTESIAN_POINT ( 'NONE',  ( -31.78594533009999878, 1436.083197293939975, 136.3653833256979908 ) ) ;
#79629 = CARTESIAN_POINT ( 'NONE',  ( -13.62133678120479985, 1452.879579795280051, 223.2680741433150047 ) ) ;
#79630 = ORIENTED_EDGE ( 'NONE', *, *, #89939, .T. ) ;
#79631 = CARTESIAN_POINT ( 'NONE',  ( 5.929777003983391914, 1510.642476694421475, 216.6410903641369146 ) ) ;
#79632 = CARTESIAN_POINT ( 'NONE',  ( -10.82804715662830120, 1409.291184126150029, 219.4290004596960273 ) ) ;
#79633 = CARTESIAN_POINT ( 'NONE',  ( 31.81407709660768290, 1522.382868172863937, 196.2902540610627682 ) ) ;
#79634 = EDGE_CURVE ( 'NONE', #82322, #71856, #14720, .T. ) ;
#79635 = CARTESIAN_POINT ( 'NONE',  ( -12.66301831902579877, 1508.551708339549805, 209.9035433704430034 ) ) ;
#79636 = CARTESIAN_POINT ( 'NONE',  ( -5.098844004812243647, 1422.101748936080412, 138.2836814087048651 ) ) ;
#79637 = CARTESIAN_POINT ( 'NONE',  ( -42.40186856140000771, 1456.064825133729755, 268.3356964774980042 ) ) ;
#79638 = CARTESIAN_POINT ( 'NONE',  ( -30.01483979339426966, 1525.231887713368451, 196.6362079710710020 ) ) ;
#79639 = CARTESIAN_POINT ( 'NONE',  ( 5.370527602886283169, 1422.356908813907012, 139.1416118586824666 ) ) ;
#79640 = EDGE_CURVE ( 'NONE', #4089, #75020, #11564, .T. ) ;
#79641 = CARTESIAN_POINT ( 'NONE',  ( -4.438186827019999854E-16, 1395.913060387330006, 217.1218459616979999 ) ) ;
#79642 = CARTESIAN_POINT ( 'NONE',  ( -103.2712462040139911, 1384.594671018880035, 311.0952753235899877 ) ) ;
#79643 = CARTESIAN_POINT ( 'NONE',  ( -40.62403037922339877, 1384.991413212550015, 213.4871031860279800 ) ) ;
#79644 = CARTESIAN_POINT ( 'NONE',  ( 18.16724748010459933, 1425.011512764430108, 226.2496254856820030 ) ) ;
#79645 = CARTESIAN_POINT ( 'NONE',  ( 22.52353380589999787, 1509.699599519530011, 227.8169178641979897 ) ) ;
#79646 = CARTESIAN_POINT ( 'NONE',  ( 15.56469051819999905, 1506.798305132929954, 225.0756798403980099 ) ) ;
#79647 = CARTESIAN_POINT ( 'NONE',  ( -26.52533711670449890, 1495.354429453090006, 211.2459270037799968 ) ) ;
#79648 = FACE_OUTER_BOUND ( 'NONE', #53964, .T. ) ;
#79649 = DIRECTION ( 'NONE',  ( 0.2495203186574841137, -0.1962602071994360708, -0.9482729257165904979 ) ) ;
#79651 = LINE ( 'NONE', #105390, #92268 ) ;
#79650 = AXIS2_PLACEMENT_3D ( 'NONE', #62155, #86773, #35827 ) ;
#79652 = CARTESIAN_POINT ( 'NONE',  ( 27.43355929049999986, 1507.980920699130138, 207.4175378521480013 ) ) ;
#79653 = CARTESIAN_POINT ( 'NONE',  ( -11.80119706069999985, 1415.163755984130148, 195.8322853899979918 ) ) ;
#79654 = CARTESIAN_POINT ( 'NONE',  ( -1.577403822089999963, 1422.569002067519932, 192.5427128247989970 ) ) ;
#79655 = CARTESIAN_POINT ( 'NONE',  ( 23.24640105429999792, 1409.889347847929912, 210.7611772360680220 ) ) ;
#79656 = B_SPLINE_SURFACE_WITH_KNOTS ( 'NONE', 5, 1, ( 
 ( #46459, #107430 ),
 ( #13909, #54313 ),
 ( #55949, #73295 ),
 ( #48095, #81125 ),
 ( #88978, #12267 ),
 ( #30725, #97923 ) ),
 .UNSPECIFIED., .F., .F., .F.,
 ( 6, 6 ),
 ( 2, 2 ),
 ( 0.000000000000000000, 3.890291737050000087 ),
 ( 0.000000000000000000, 14.00000000000000000 ),
 .UNSPECIFIED. ) ;
#79657 = DIRECTION ( 'NONE',  ( -1.000000000000000000, 0.000000000000000000, 0.000000000000000000 ) ) ;
#79658 = CARTESIAN_POINT ( 'NONE',  ( 20.84774931509999973, 1457.996261225589933, 206.6760932923689893 ) ) ;
#79659 = CARTESIAN_POINT ( 'NONE',  ( -15.03158816200000025, 1422.458662492329950, 229.1221043826980122 ) ) ;
#79661 = CARTESIAN_POINT ( 'NONE',  ( -13.53579909870000009, 1380.123783341879971, 205.1599962651189912 ) ) ;
#79660 = CARTESIAN_POINT ( 'NONE',  ( -11.57592119009999898, 1432.301067315389901, 151.1967988364980044 ) ) ;
#79662 = CARTESIAN_POINT ( 'NONE',  ( -5.024578973489999711, 1391.800828890389994, 203.6117233725290134 ) ) ;
#79663 = CARTESIAN_POINT ( 'NONE',  ( -102.2221789262000016, 1377.418846546390114, 304.2218459572590064 ) ) ;
#79664 = CARTESIAN_POINT ( 'NONE',  ( 16.56943046651975848, 1526.189899547014875, 235.5982391528384312 ) ) ;
#79665 = CARTESIAN_POINT ( 'NONE',  ( -23.20186844609999710, 1425.882783674430129, 212.0388266151180119 ) ) ;
#79666 = CARTESIAN_POINT ( 'NONE',  ( -1.328211266513899869, 1420.347263902439863, 184.8989585457709950 ) ) ;
#79667 = CARTESIAN_POINT ( 'NONE',  ( -3.265407155974999753, 1516.754149861460064, 204.5121726906670006 ) ) ;
#79668 = DIRECTION ( 'NONE',  ( 0.000000000000000000, 0.000000000000000000, -1.000000000000000000 ) ) ;
#79669 = CARTESIAN_POINT ( 'NONE',  ( -18.11634809011280112, 1485.171219500319921, 188.9687042995529964 ) ) ;
#79670 = CARTESIAN_POINT ( 'NONE',  ( 13.73040295794826626, 1521.951704408389787, 227.6346699037790984 ) ) ;
#79671 = CARTESIAN_POINT ( 'NONE',  ( -11.68980366881247335, 1421.933377081587423, 210.6412079282914362 ) ) ;
#79673 = ORIENTED_EDGE ( 'NONE', *, *, #19247, .F. ) ;
#79672 = CARTESIAN_POINT ( 'NONE',  ( -64.33487710937569659, 1379.738747083599947, 273.6361551471470079 ) ) ;
#79674 = EDGE_LOOP ( 'NONE', ( #10102, #58905, #8644, #24542, #42785 ) ) ;
#79675 = CARTESIAN_POINT ( 'NONE',  ( 27.14773470689999968, 1508.594019929430033, 214.4840992054080004 ) ) ;
#79676 = ORIENTED_EDGE ( 'NONE', *, *, #19284, .T. ) ;
#79677 = DIRECTION ( 'NONE',  ( -1.132411226124150056E-06, 0.9999999999963642416, 2.447241413984286834E-06 ) ) ;
#79678 = AXIS2_PLACEMENT_3D ( 'NONE', #45191, #107274, #45749 ) ;
#79679 = CARTESIAN_POINT ( 'NONE',  ( 1.414439329599999962, 1414.913528139129994, 192.0350025121979911 ) ) ;
#79681 = CARTESIAN_POINT ( 'NONE',  ( 0.5892548269570000441, 1508.868282030629871, 179.9181551937980146 ) ) ;
#79680 = CARTESIAN_POINT ( 'NONE',  ( -2.913665321129999787E-15, 1426.935925255829943, 133.6118001900980232 ) ) ;
#79682 = CARTESIAN_POINT ( 'NONE',  ( 11.94046459599999999, 1438.194204504490017, 147.6340003373980210 ) ) ;
#79683 = CARTESIAN_POINT ( 'NONE',  ( -25.17222414333650349, 1451.970523125299906, 135.9900793875290219 ) ) ;
#79684 = CARTESIAN_POINT ( 'NONE',  ( -2.130922737000000122, 1467.954349366689939, 220.0452206860990145 ) ) ;
#79685 = CARTESIAN_POINT ( 'NONE',  ( 5.558638042260000134, 1409.107172305129779, 229.7071683781979914 ) ) ;
#79686 = CARTESIAN_POINT ( 'NONE',  ( -3.253141175365000137, 1516.858171774179937, 212.3894494859370070 ) ) ;
#79688 = CIRCLE ( 'NONE', #86852, 1.000000000000005551 ) ;
#79687 = CARTESIAN_POINT ( 'NONE',  ( 39.48425676673629425, 1438.208629468120080, 134.0999999978120059 ) ) ;
#79689 = CARTESIAN_POINT ( 'NONE',  ( -6.696214959435129899, 1424.446799123830033, 209.0310039315669997 ) ) ;
#79690 = CARTESIAN_POINT ( 'NONE',  ( -0.5642542037087260320, 1421.257282776259899, 227.9630948969180224 ) ) ;
#79691 = ORIENTED_EDGE ( 'NONE', *, *, #31923, .T. ) ;
#79692 = CARTESIAN_POINT ( 'NONE',  ( -19.86464710129999744, 1441.435714617490021, 212.6459466283089910 ) ) ;
#79693 = CARTESIAN_POINT ( 'NONE',  ( -10.53295592549999959, 1391.913060387289988, 204.1405351054689845 ) ) ;
#79694 = EDGE_LOOP ( 'NONE', ( #84833, #81712, #1890, #94426 ) ) ;
#79695 = VERTEX_POINT ( 'NONE', #41026 ) ;
#79696 = EDGE_LOOP ( 'NONE', ( #14292, #52043, #25032, #67523 ) ) ;
#79697 = CARTESIAN_POINT ( 'NONE',  ( 12.53380499174499896, 1445.052233488290085, 169.4755105688890069 ) ) ;
#79698 = CARTESIAN_POINT ( 'NONE',  ( -0.3690468201050000063, 1465.421769112429956, 236.2943548505980118 ) ) ;
#79699 = EDGE_CURVE ( 'NONE', #50703, #94116, #97924, .T. ) ;
#79700 = CARTESIAN_POINT ( 'NONE',  ( 21.44083111125928909, 1450.933478988742081, 143.9289517833655623 ) ) ;
#79701 = CARTESIAN_POINT ( 'NONE',  ( -7.545064063079999883, 1384.907232460160003, 219.0876311382089909 ) ) ;
#79702 = CARTESIAN_POINT ( 'NONE',  ( -2.253566441613126910E-10, 1426.918876941764893, 137.0999999980980135 ) ) ;
#79703 = LINE ( 'NONE', #96489, #65804 ) ;
#79704 = CARTESIAN_POINT ( 'NONE',  ( -66.34541600742676337, 1379.742690955398075, 275.0820465578231619 ) ) ;
#79705 = CARTESIAN_POINT ( 'NONE',  ( 4.229824676192839306, 1446.290629315919887, 165.0048999265850114 ) ) ;
#79706 = CARTESIAN_POINT ( 'NONE',  ( 8.658163031318741432, 1437.533170863820033, 209.0585791703279881 ) ) ;
#79707 = ORIENTED_EDGE ( 'NONE', *, *, #9305, .F. ) ;
#79708 = CARTESIAN_POINT ( 'NONE',  ( 0.7352271172030020452, 1516.963431999339946, 207.4067364850470199 ) ) ;
#79709 = ORIENTED_EDGE ( 'NONE', *, *, #70277, .T. ) ;
#79710 = CARTESIAN_POINT ( 'NONE',  ( 29.78885521565789674, 1440.913060387330006, 251.6509508777969870 ) ) ;
#79711 = ADVANCED_FACE ( 'NONE', ( #64612 ), #51869, .F. ) ;
#79712 = DIRECTION ( 'NONE',  ( 0.000000000000000000, 0.000000000000000000, 1.000000000000000000 ) ) ;
#79713 = ORIENTED_EDGE ( 'NONE', *, *, #82353, .F. ) ;
#79714 = CARTESIAN_POINT ( 'NONE',  ( -7.512715662404939820, 1509.034509512849809, 202.9804584623499863 ) ) ;
#79715 = CARTESIAN_POINT ( 'NONE',  ( -13.63985639130000038, 1409.389374668229948, 191.6355463836979709 ) ) ;
#79716 = CARTESIAN_POINT ( 'NONE',  ( -32.12438293513578458, 1379.634397414435625, 220.1697278361670271 ) ) ;
#79718 = CARTESIAN_POINT ( 'NONE',  ( 6.813936602420000099, 1469.517477258589906, 209.5520740031860214 ) ) ;
#79717 = CARTESIAN_POINT ( 'NONE',  ( -24.30106948394094957, 1439.034099877470453, 212.0667701832317675 ) ) ;
#79719 = CARTESIAN_POINT ( 'NONE',  ( -9.547530987552349302, 1437.933916352150163, 211.7113974646419763 ) ) ;
#79720 = CARTESIAN_POINT ( 'NONE',  ( -6.375350519788010040, 1511.068351247050032, 201.7267438082049864 ) ) ;
#79721 = CARTESIAN_POINT ( 'NONE',  ( 27.22939932153649778, 1441.374094540659826, 137.3495838342670083 ) ) ;
#79722 = DIRECTION ( 'NONE',  ( -3.247745162871014848E-19, -1.000000000000000000, -7.717164782866489769E-18 ) ) ;
#79723 = CARTESIAN_POINT ( 'NONE',  ( -4.455463436649999664, 1508.108973204389940, 220.6784667051990141 ) ) ;
#79725 = CARTESIAN_POINT ( 'NONE',  ( 3.330134165755000097, 1515.051704408389924, 204.7920544413669859 ) ) ;
#79724 = CARTESIAN_POINT ( 'NONE',  ( 2.858162928570000094, 1466.265918564530011, 234.1316300927979910 ) ) ;
#79726 = CARTESIAN_POINT ( 'NONE',  ( 1.130002494264999990, 1516.621991115350056, 216.0576472317669925 ) ) ;
#79727 = CARTESIAN_POINT ( 'NONE',  ( 0.000000000000000000, 1523.382868172864164, 209.1218459616979999 ) ) ;
#79728 = CARTESIAN_POINT ( 'NONE',  ( 6.044713202946720543, 1511.753217516670247, 217.4189031040939994 ) ) ;
#79729 = CARTESIAN_POINT ( 'NONE',  ( 29.22958591730000322, 1509.933780019529877, 206.4713312915380072 ) ) ;
#79730 = CARTESIAN_POINT ( 'NONE',  ( 2.298369469825000344, 1516.779243033999819, 212.3734572960470075 ) ) ;
#79731 = DIRECTION ( 'NONE',  ( -0.001027118858030306352, 0.9999913661844073154, -0.004026485253177600199 ) ) ;
#79732 = DIRECTION ( 'NONE',  ( 0.000000000000000000, 0.000000000000000000, 1.000000000000000000 ) ) ;
#79734 = EDGE_LOOP ( 'NONE', ( #100785, #492, #52819, #3715 ) ) ;
#79733 = CARTESIAN_POINT ( 'NONE',  ( -103.7270236659999938, 1386.773311355200121, 297.0694254661589753 ) ) ;
#79735 = CARTESIAN_POINT ( 'NONE',  ( -17.42134945962463988, 1525.253972588476699, 237.1661777806035332 ) ) ;
#79736 = CARTESIAN_POINT ( 'NONE',  ( 28.66942461040000012, 1455.243640875029996, 248.2467662549979934 ) ) ;
#79737 = ADVANCED_FACE ( 'NONE', ( #30831 ), #90739, .T. ) ;
#79738 = CARTESIAN_POINT ( 'NONE',  ( 29.00779973304128134, 1526.382868172864164, 217.2942086403122630 ) ) ;
#79739 = CARTESIAN_POINT ( 'NONE',  ( -26.49480178416090226, 1509.838279253159953, 221.7449016213969912 ) ) ;
#79740 = CARTESIAN_POINT ( 'NONE',  ( 1.799212021300000020, 1414.514225440530026, 232.3796572949979975 ) ) ;
#79741 = ADVANCED_FACE ( 'NONE', ( #31932 ), #84888, .T. ) ;
#79742 = CARTESIAN_POINT ( 'NONE',  ( -20.46956895259999953, 1454.794904290429940, 224.5075067967979976 ) ) ;
#79743 = EDGE_CURVE ( 'NONE', #39621, #25855, #103053, .T. ) ;
#79745 = CARTESIAN_POINT ( 'NONE',  ( 2.500000000000000000, 1432.253675377960008, 157.4927705404979861 ) ) ;
#79744 = CARTESIAN_POINT ( 'NONE',  ( -20.67788066618572529, 1410.996043025710378, 199.4490997680371152 ) ) ;
#79746 = CARTESIAN_POINT ( 'NONE',  ( -9.045810569538431878, 1449.339667039310143, 210.6515513332149681 ) ) ;
#79747 = CARTESIAN_POINT ( 'NONE',  ( -106.2248512509999898, 1379.716103201010128, 307.8123243076590256 ) ) ;
#79748 = ORIENTED_EDGE ( 'NONE', *, *, #59780, .T. ) ;
#79749 = CARTESIAN_POINT ( 'NONE',  ( 7.713117802984999827, 1516.690345681169902, 204.1174038931170003 ) ) ;
#79750 = CARTESIAN_POINT ( 'NONE',  ( 3.426893344479999826, 1406.086097517129929, 266.9564242903979903 ) ) ;
#79751 = CARTESIAN_POINT ( 'NONE',  ( -1.842962231260000028, 1515.064792882589927, 213.4512947377390049 ) ) ;
#79752 = ADVANCED_FACE ( 'NONE', ( #48764 ), #33943, .T. ) ;
#79753 = CIRCLE ( 'NONE', #10029, 7.799999999999999822 ) ;
#79754 = CARTESIAN_POINT ( 'NONE',  ( 42.85031254769640441, 1445.998884488219801, 270.2009481598719844 ) ) ;
#79755 = DIRECTION ( 'NONE',  ( 0.3090169943749515591, -0.000000000000000000, 0.9510565162951523099 ) ) ;
#79756 = CARTESIAN_POINT ( 'NONE',  ( 10.81433178877583501, 1424.654531174282056, 138.0162591780839136 ) ) ;
#79757 = CARTESIAN_POINT ( 'NONE',  ( -36.52292854368610620, 1440.913060387330006, 253.7928692754429676 ) ) ;
#79758 = LINE ( 'NONE', #6183, #87899 ) ;
#79759 = CARTESIAN_POINT ( 'NONE',  ( 2.356271506361870216, 1449.642660013894783, 154.4296805934006898 ) ) ;
#79760 = DIRECTION ( 'NONE',  ( -1.407418274235009893E-17, -1.000000000000000000, 2.576261870300909820E-17 ) ) ;
#79761 = CARTESIAN_POINT ( 'NONE',  ( 1.174890886735320050, 1450.814461567769968, 154.7898993816909865 ) ) ;
#79762 = CARTESIAN_POINT ( 'NONE',  ( 0.6715583085099990912, 1506.489872953789927, 221.9351472385990007 ) ) ;
#79763 = CARTESIAN_POINT ( 'NONE',  ( -1.546869376352204339, 1416.835807507126901, 228.0212684238467489 ) ) ;
#79764 = AXIS2_PLACEMENT_3D ( 'NONE', #41972, #76671, #83963 ) ;
#79765 = ORIENTED_EDGE ( 'NONE', *, *, #17252, .F. ) ;
#79766 = CARTESIAN_POINT ( 'NONE',  ( -7.553102830249999400, 1423.481562104430168, 234.3916895697979612 ) ) ;
#79767 = CARTESIAN_POINT ( 'NONE',  ( 3.535327689299999854, 1487.160995979990048, 197.6951163427989968 ) ) ;
#79768 = FACE_OUTER_BOUND ( 'NONE', #91103, .T. ) ;
#79769 = CARTESIAN_POINT ( 'NONE',  ( -1.312418798399999753, 1475.035471520030114, 269.6495476954979722 ) ) ;
#79770 = CARTESIAN_POINT ( 'NONE',  ( 1.332267629549999902E-15, 1413.913060387330006, 209.1218459616989946 ) ) ;
#79771 = CARTESIAN_POINT ( 'NONE',  ( -27.92763793890000201, 1508.597377666530065, 210.3373496168879910 ) ) ;
#79772 = EDGE_CURVE ( 'NONE', #28187, #14911, #108435, .T. ) ;
#79773 = CARTESIAN_POINT ( 'NONE',  ( -2.499999999999999556, 1448.225424448829699, 183.4745085405895679 ) ) ;
#79774 = CARTESIAN_POINT ( 'NONE',  ( -33.85357780581230003, 1384.813694486169879, 232.6238098525020064 ) ) ;
#79775 = DIRECTION ( 'NONE',  ( 0.000000000000000000, 1.000000000000000000, 0.000000000000000000 ) ) ;
#79776 = CARTESIAN_POINT ( 'NONE',  ( -9.779853762240000137, 1481.708752394490148, 205.0329629307690027 ) ) ;
#79777 = CARTESIAN_POINT ( 'NONE',  ( 26.64494604805370059, 1435.509179537890077, 135.8250902819609962 ) ) ;
#79779 = ADVANCED_FACE ( 'NONE', ( #75617 ), #34866, .F. ) ;
#79778 = CARTESIAN_POINT ( 'NONE',  ( -3.852081035159350186, 1396.047578021569961, 219.4511520228920176 ) ) ;
#79780 = B_SPLINE_CURVE_WITH_KNOTS ( 'NONE', 5,
 ( #47517, #30138, #12797, #11702, #46432, #55924 ),
 .UNSPECIFIED., .F., .F.,
 ( 6, 6 ),
 ( 0.000000000000000000, 1.000000000000000000 ),
 .UNSPECIFIED. ) ;
#79781 = CARTESIAN_POINT ( 'NONE',  ( -15.97381121195400056, 1420.723668288270119, 227.0315409032249931 ) ) ;
#79782 = CARTESIAN_POINT ( 'NONE',  ( -16.78937331912329967, 1410.728390654980103, 226.4051236745929998 ) ) ;
#79783 = FACE_OUTER_BOUND ( 'NONE', #17674, .T. ) ;
#79784 = ORIENTED_EDGE ( 'NONE', *, *, #21439, .F. ) ;
#79785 = CARTESIAN_POINT ( 'NONE',  ( -1.813815691101789973, 1436.230605934150162, 227.5234084965020145 ) ) ;
#79786 = CARTESIAN_POINT ( 'NONE',  ( -13.58372279061449994, 1508.526660466229941, 210.1193507368990367 ) ) ;
#79787 = CARTESIAN_POINT ( 'NONE',  ( -11.84030381978469926, 1430.235986086469893, 151.0624496547240199 ) ) ;
#79789 = CARTESIAN_POINT ( 'NONE',  ( -11.02428140916500077, 1512.359593911809952, 193.2458125109669993 ) ) ;
#79788 = CARTESIAN_POINT ( 'NONE',  ( 11.23805577879999973, 1426.459959828230012, 108.0450254846979874 ) ) ;
#79790 = CARTESIAN_POINT ( 'NONE',  ( 11.68426330212614239, 1428.980873612041023, 140.1562216286907869 ) ) ;
#79791 = CARTESIAN_POINT ( 'NONE',  ( -11.23388613411650638, 1445.063428794548372, 151.7784653951601399 ) ) ;
#79792 = CARTESIAN_POINT ( 'NONE',  ( -4.761835944330000459, 1382.817942041290053, 203.6389619452989734 ) ) ;
#79793 = CARTESIAN_POINT ( 'NONE',  ( 7.638852881150000051, 1424.646166941220145, 212.0768851055590005 ) ) ;
#79794 = CARTESIAN_POINT ( 'NONE',  ( -9.660544699540000835, 1432.353341358199941, 148.7316627034979888 ) ) ;
#79795 = CARTESIAN_POINT ( 'NONE',  ( 5.709868603420000355, 1508.901606182030037, 181.0882369999980028 ) ) ;
#79796 = DIRECTION ( 'NONE',  ( 0.3363363969981477131, 0.6659120918162938496, -0.6659120918162938496 ) ) ;
#79797 = CARTESIAN_POINT ( 'NONE',  ( -47.85632535846249880, 1378.658246217350097, 243.6236061017949908 ) ) ;
#79798 = CARTESIAN_POINT ( 'NONE',  ( 6.612365369791289638, 1366.252322145174958, 208.3718459617061285 ) ) ;
#79800 = ORIENTED_EDGE ( 'NONE', *, *, #956, .T. ) ;
#79799 = CARTESIAN_POINT ( 'NONE',  ( -3.348648543330357441, 1523.530935881284904, 242.0864759303845801 ) ) ;
#79801 = VERTEX_POINT ( 'NONE', #35607 ) ;
#79802 = CIRCLE ( 'NONE', #101173, 1.000000000000000888 ) ;
#79803 = CARTESIAN_POINT ( 'NONE',  ( -14.52606424000000018, 1443.052989431600054, 188.9151166515979980 ) ) ;
#79804 = CARTESIAN_POINT ( 'NONE',  ( -5.555854370870000558, 1409.107075097130291, 188.5359587977980027 ) ) ;
#79805 = FACE_OUTER_BOUND ( 'NONE', #8754, .T. ) ;
#79806 = CARTESIAN_POINT ( 'NONE',  ( -8.170896261794998949, 1511.354819475749991, 213.9493513980370096 ) ) ;
#79808 = LINE ( 'NONE', #70325, #68337 ) ;
#79807 = CARTESIAN_POINT ( 'NONE',  ( -7.811670192970000315, 1384.136991477590072, 218.8584676683489931 ) ) ;
#79809 = CARTESIAN_POINT ( 'NONE',  ( -31.79805362023597226, 1525.506926151470680, 201.2206259782555549 ) ) ;
#79810 = FACE_OUTER_BOUND ( 'NONE', #104893, .T. ) ;
#79811 = CARTESIAN_POINT ( 'NONE',  ( -41.57727771173860276, 1445.035119975709904, 135.5177309179229894 ) ) ;
#79812 = SURFACE_SIDE_STYLE ('',( #54079 ) ) ;
#79813 = CARTESIAN_POINT ( 'NONE',  ( -2.500000000000000000, 1448.283978340080012, 164.7255006787519847 ) ) ;
#79814 = CARTESIAN_POINT ( 'NONE',  ( 9.773096794904308382, 1396.254344449989958, 214.3031617136149976 ) ) ;
#79815 = CARTESIAN_POINT ( 'NONE',  ( -39.26371633287709528, 1437.713075516209983, 136.4559412716930353 ) ) ;
#79816 = CARTESIAN_POINT ( 'NONE',  ( -2.304693369170319972, 1405.812077718989940, 268.4818566354389873 ) ) ;
#79817 = CARTESIAN_POINT ( 'NONE',  ( 0.000000000000000000, 1413.913060387330006, 209.1218459616979999 ) ) ;
#79818 = ORIENTED_EDGE ( 'NONE', *, *, #81537, .T. ) ;
#79819 = CARTESIAN_POINT ( 'NONE',  ( 4.029435563379999863, 1425.967794969329816, 185.3373052141980111 ) ) ;
#79820 = CARTESIAN_POINT ( 'NONE',  ( 21.11881948555302557, 1525.651286436460168, 233.3142521953524238 ) ) ;
#79821 = ORIENTED_EDGE ( 'NONE', *, *, #41875, .F. ) ;
#79822 = EDGE_LOOP ( 'NONE', ( #34364, #107415, #32829, #13555 ) ) ;
#79823 = CARTESIAN_POINT ( 'NONE',  ( -3.558362537839999895, 1455.955980043889895, 200.3550983807189994 ) ) ;
#79824 = CARTESIAN_POINT ( 'NONE',  ( -5.247433916371702978, 1368.770886448055762, 207.6218459616990515 ) ) ;
#79825 = CARTESIAN_POINT ( 'NONE',  ( 5.782749401605000727, 1516.858301627840092, 214.8983370654769942 ) ) ;
#79826 = CARTESIAN_POINT ( 'NONE',  ( 2.892503378805000303, 1511.980236064749988, 216.8996406803269963 ) ) ;
#79827 = ORIENTED_EDGE ( 'NONE', *, *, #25434, .F. ) ;
#79828 = DIRECTION ( 'NONE',  ( -9.120877578445558697E-47, 1.000000000000000000, -1.836970198721029688E-16 ) ) ;
#79829 = CARTESIAN_POINT ( 'NONE',  ( -64.29757574260000297, 1379.513720862740229, 269.4006999320590126 ) ) ;
#79830 =( BOUNDED_CURVE ( )  B_SPLINE_CURVE ( 3, ( #7989, #24227, #93094, #92539 ),
 .UNSPECIFIED., .F., .F. ) 
 B_SPLINE_CURVE_WITH_KNOTS ( ( 4, 4 ),
 ( 3.141592653589793116, 4.712388980384689674 ),
 .UNSPECIFIED. ) 
 CURVE ( )  GEOMETRIC_REPRESENTATION_ITEM ( )  RATIONAL_B_SPLINE_CURVE ( ( 1.000000000000000000, 0.8047378541243649375, 0.8047378541243649375, 1.000000000000000000 ) ) 
 REPRESENTATION_ITEM ( '' )  );
#79831 = CARTESIAN_POINT ( 'NONE',  ( -106.0563374611769945, 1378.913060387289988, 302.7607369287470078 ) ) ;
#79832 = CARTESIAN_POINT ( 'NONE',  ( 1.703779605225000049, 1517.057265928030120, 205.0766634521770015 ) ) ;
#79833 = CARTESIAN_POINT ( 'NONE',  ( 11.41833509600000163, 1492.743966792589845, 212.4764448217789834 ) ) ;
#79834 = CARTESIAN_POINT ( 'NONE',  ( -41.56672249360055815, 1436.264666313427597, 269.6392715097015298 ) ) ;
#79835 = CARTESIAN_POINT ( 'NONE',  ( 9.275662108596250732, 1461.991666016340105, 206.1939425705140252 ) ) ;
#79836 = CARTESIAN_POINT ( 'NONE',  ( -4.049849602479999255, 1409.054484251730173, 230.6815826274979884 ) ) ;
#79838 = ORIENTED_EDGE ( 'NONE', *, *, #81705, .F. ) ;
#79837 = CARTESIAN_POINT ( 'NONE',  ( -1.549455982270276921, 1452.110832695822410, 183.9727752664628042 ) ) ;
#79839 = FACE_OUTER_BOUND ( 'NONE', #103967, .T. ) ;
#79840 = CARTESIAN_POINT ( 'NONE',  ( -26.20202373978780130, 1440.913060467019932, 222.9344598648480087 ) ) ;
#79841 = CARTESIAN_POINT ( 'NONE',  ( 20.49599333844873783, 1525.960063244516959, 233.8638087104922931 ) ) ;
#79842 = DIRECTION ( 'NONE',  ( -0.6736849260863841948, 0.000000000000000000, 0.7390186874254148774 ) ) ;
#79843 = CARTESIAN_POINT ( 'NONE',  ( 36.48439800688450418, 1420.562376931399967, 269.8440692582560700 ) ) ;
#79844 = CARTESIAN_POINT ( 'NONE',  ( -2.478306858074999841, 1516.938330505699923, 212.5844667883370107 ) ) ;
#79845 = CARTESIAN_POINT ( 'NONE',  ( -66.60970852960001309, 1379.742673636729933, 275.7100306615589602 ) ) ;
#79846 = DIRECTION ( 'NONE',  ( 0.000000000000000000, -0.8286769424886156754, -0.5597271880011900347 ) ) ;
#79847 = CARTESIAN_POINT ( 'NONE',  ( 11.54155030333390108, 1426.278799798020145, 195.2408946065239945 ) ) ;
#79848 = CARTESIAN_POINT ( 'NONE',  ( -0.3788383082595139784, 1408.926289712549988, 186.6322538385570056 ) ) ;
#79849 = CARTESIAN_POINT ( 'NONE',  ( 4.042388501175000037, 1517.045004075700035, 209.8579434088520088 ) ) ;
#79850 = ORIENTED_EDGE ( 'NONE', *, *, #91819, .F. ) ;
#79851 = CARTESIAN_POINT ( 'NONE',  ( 2.500000000000000000, 1438.733025222760034, 157.7103763496980093 ) ) ;
#79852 = CARTESIAN_POINT ( 'NONE',  ( -0.9510881122189999148, 1420.454310056129998, 233.4992290069980072 ) ) ;
#79853 = CARTESIAN_POINT ( 'NONE',  ( 5.347888905970906492, 1422.377615597161594, 137.0999999981554254 ) ) ;
#79854 = VERTEX_POINT ( 'NONE', #45145 ) ;
#79855 = CARTESIAN_POINT ( 'NONE',  ( -35.77507902226459890, 1385.205099667260129, 235.2908270135410191 ) ) ;
#79856 = CARTESIAN_POINT ( 'NONE',  ( -4.490619218195398332, 1508.909942012477359, 206.6339108000523481 ) ) ;
#79857 = EDGE_CURVE ( 'NONE', #91877, #84761, #101657, .T. ) ;
#79858 = CARTESIAN_POINT ( 'NONE',  ( 15.79979472558019893, 1478.706781717480226, 230.3901329066689811 ) ) ;
#79859 = CARTESIAN_POINT ( 'NONE',  ( 19.97269026569999895, 1507.847566758330004, 189.1149477268980093 ) ) ;
#79860 = CARTESIAN_POINT ( 'NONE',  ( -29.73378234562438749, 1526.349684470114653, 217.2224020302186602 ) ) ;
#79861 = CARTESIAN_POINT ( 'NONE',  ( -0.009250756501870001022, 1410.298659367929758, 233.2341916293980262 ) ) ;
#79862 = CARTESIAN_POINT ( 'NONE',  ( -0.02494278528423909957, 1420.444533703900106, 182.6761653814459976 ) ) ;
#79864 = CARTESIAN_POINT ( 'NONE',  ( 22.08622291487997558, 1523.456924617338700, 184.4183880513681402 ) ) ;
#79863 = CARTESIAN_POINT ( 'NONE',  ( -1.708102627415000185, 1517.199196846569976, 215.6864246554469844 ) ) ;
#79865 = CARTESIAN_POINT ( 'NONE',  ( 18.68654020960000040, 1509.565608750529918, 186.8439702849979938 ) ) ;
#79866 = CARTESIAN_POINT ( 'NONE',  ( 10.04531431606059932, 1469.136521703999961, 209.2681548814119878 ) ) ;
#79867 = ORIENTED_EDGE ( 'NONE', *, *, #106736, .T. ) ;
#79868 = CARTESIAN_POINT ( 'NONE',  ( 1.710012720495000194, 1517.232977404109988, 201.3945188173769907 ) ) ;
#79869 = CARTESIAN_POINT ( 'NONE',  ( -16.78942537780000066, 1508.913060324029857, 185.4904754144979790 ) ) ;
#79870 = VERTEX_POINT ( 'NONE', #71473 ) ;
#79871 = DIRECTION ( 'NONE',  ( 0.2342910577437130604, -0.2476038162833715528, 0.9401064037773823046 ) ) ;
#79872 = ADVANCED_FACE ( 'NONE', ( #61400 ), #27219, .F. ) ;
#79873 = CARTESIAN_POINT ( 'NONE',  ( 4.500000000000000000, 1425.929641636930000, 172.2701767017979932 ) ) ;
#79874 = FACE_OUTER_BOUND ( 'NONE', #10488, .T. ) ;
#79875 = CARTESIAN_POINT ( 'NONE',  ( 3.181172984599999864, 1442.605928313790173, 217.4126502567789885 ) ) ;
#79876 = CARTESIAN_POINT ( 'NONE',  ( -27.18296536300610100, 1509.563679778480036, 201.2124616717040055 ) ) ;
#79877 = CARTESIAN_POINT ( 'NONE',  ( 10.94754737549849821, 1490.097295750230160, 208.8086307138860036 ) ) ;
#79878 = CARTESIAN_POINT ( 'NONE',  ( -17.64146421497870065, 1419.304501645640130, 207.1873797621490212 ) ) ;
#79879 = CARTESIAN_POINT ( 'NONE',  ( -18.27807275150000166, 1423.991801469829852, 225.3729312157979905 ) ) ;
#79880 = CARTESIAN_POINT ( 'NONE',  ( -22.74371025250000145, 1435.291990449120249, 140.0265565429980086 ) ) ;
#79881 = EDGE_CURVE ( 'NONE', #63032, #34701, #80490, .T. ) ;
#79882 = CARTESIAN_POINT ( 'NONE',  ( -0.5883740847710429156, 1477.659013864529925, 230.4497675389389997 ) ) ;
#79883 = DIRECTION ( 'NONE',  ( -0.9455185755993178454, 0.000000000000000000, 0.3255681544571539243 ) ) ;
#79885 = CARTESIAN_POINT ( 'NONE',  ( -15.83997831783995736, 1431.256282991279932, 220.2014388792205182 ) ) ;
#79884 = CARTESIAN_POINT ( 'NONE',  ( 0.8805854391707040874, 1409.878736129950084, 233.0125103023929967 ) ) ;
#79886 = CARTESIAN_POINT ( 'NONE',  ( 2.314969334973908666, 1525.402221411349728, 243.6179210388352203 ) ) ;
#79887 = ORIENTED_EDGE ( 'NONE', *, *, #32172, .T. ) ;
#79888 = CARTESIAN_POINT ( 'NONE',  ( 1.550352066763079906, 1415.948038442049892, 190.4790932164650030 ) ) ;
#79889 = CARTESIAN_POINT ( 'NONE',  ( -30.31940284292426924, 1523.456872492435195, 195.7503880523418616 ) ) ;
#79890 = CARTESIAN_POINT ( 'NONE',  ( -11.90008666459999986, 1434.920851464509951, 147.6452002888979962 ) ) ;
#79891 = CARTESIAN_POINT ( 'NONE',  ( -4.780581990890000021, 1483.100110836790009, 199.6018351111989944 ) ) ;
#79892 = CARTESIAN_POINT ( 'NONE',  ( 0.000000000000000000, 1519.913060387329779, 209.1218459616979999 ) ) ;
#79893 = CARTESIAN_POINT ( 'NONE',  ( -2.311636021096358018, 1525.506916460682305, 241.8052139131910963 ) ) ;
#79894 = CARTESIAN_POINT ( 'NONE',  ( -10.98084453577630093, 1433.016921785290151, 151.7694248368179899 ) ) ;
#79895 = CARTESIAN_POINT ( 'NONE',  ( -24.84524933634759947, 1439.550688600570084, 210.4208596888960017 ) ) ;
#79896 = CARTESIAN_POINT ( 'NONE',  ( -11.18353437974609932, 1470.314597740729823, 211.2446877208680007 ) ) ;
#79897 = CARTESIAN_POINT ( 'NONE',  ( -6.007801178118840291, 1489.444426110659833, 218.3574661116689981 ) ) ;
#79898 = CARTESIAN_POINT ( 'NONE',  ( -21.44637799630000075, 1506.412602296789828, 216.0243671510289971 ) ) ;
#79899 = CARTESIAN_POINT ( 'NONE',  ( -84.93366321518800532, 1383.773587948340264, 306.4644327478220589 ) ) ;
#79900 = CARTESIAN_POINT ( 'NONE',  ( -109.5468108793060082, 1383.526318514589775, 311.1941293573789835 ) ) ;
#79901 = CARTESIAN_POINT ( 'NONE',  ( 22.08622291482350519, 1518.913060387330006, 233.8253038720783366 ) ) ;
#79903 = EDGE_CURVE ( 'NONE', #78702, #38027, #95521, .T. ) ;
#79902 = CARTESIAN_POINT ( 'NONE',  ( 0.008257837813740559821, 1516.936920898230028, 201.4022722931759972 ) ) ;
#79905 = ORIENTED_EDGE ( 'NONE', *, *, #106358, .F. ) ;
#79904 = DIRECTION ( 'NONE',  ( 0.7074300732568278294, -0.02470400251969398844, 0.7063514732138287400 ) ) ;
#79906 = CARTESIAN_POINT ( 'NONE',  ( -73.92520625790000111, 1379.263703378919899, 287.0831489011590065 ) ) ;
#79907 = PLANE ( 'NONE',  #96213 ) ;
#79908 = ORIENTED_EDGE ( 'NONE', *, *, #19333, .T. ) ;
#79909 = VERTEX_POINT ( 'NONE', #3147 ) ;
#79910 = LINE ( 'NONE', #45775, #13328 ) ;
#79911 = CARTESIAN_POINT ( 'NONE',  ( -109.3504194409999855, 1384.949684486699880, 297.1387111212590071 ) ) ;
#79912 = CARTESIAN_POINT ( 'NONE',  ( 12.95705078732472515, 1442.923589581116175, 169.4279645666727561 ) ) ;
#79914 = CARTESIAN_POINT ( 'NONE',  ( -31.44036148889999538, 1456.450349409130013, 254.7811646097979974 ) ) ;
#79913 = CARTESIAN_POINT ( 'NONE',  ( 29.71190172082722114, 1419.366236750363669, 269.4677692610073905 ) ) ;
#79915 = CARTESIAN_POINT ( 'NONE',  ( 8.999746791583771000, 1435.834253586629984, 208.6187618879379784 ) ) ;
#79916 = CARTESIAN_POINT ( 'NONE',  ( -11.32027785699999889, 1433.946929803360035, 151.5080542412979980 ) ) ;
#79917 = CARTESIAN_POINT ( 'NONE',  ( 3.749012616329999936, 1480.578083832889888, 229.2223542577989974 ) ) ;
#79918 = CARTESIAN_POINT ( 'NONE',  ( -19.67553321019999757, 1485.964808132929875, 190.1451763510979731 ) ) ;
#79919 = CARTESIAN_POINT ( 'NONE',  ( 9.907168344889999645, 1409.425378975729927, 189.1781829689979872 ) ) ;
#79920 = CARTESIAN_POINT ( 'NONE',  ( 4.936249769079999794, 1423.379993255829959, 184.2513112279979737 ) ) ;
#79921 = CARTESIAN_POINT ( 'NONE',  ( 1.842963219480119985, 1515.064792700640055, 213.4512947425059792 ) ) ;
#79922 = CARTESIAN_POINT ( 'NONE',  ( 5.445836176130000261, 1441.097906882780080, 154.8052917028979607 ) ) ;
#79923 = DIRECTION ( 'NONE',  ( -1.000000000000000000, 0.000000000000000000, 0.000000000000000000 ) ) ;
#79924 = CARTESIAN_POINT ( 'NONE',  ( -6.040726587390000013, 1452.702113566630032, 152.1320015699980104 ) ) ;
#79925 = ORIENTED_EDGE ( 'NONE', *, *, #39098, .T. ) ;
#79926 = ORIENTED_EDGE ( 'NONE', *, *, #99685, .F. ) ;
#79927 = CARTESIAN_POINT ( 'NONE',  ( -11.89363985299999982, 1506.209575258589894, 208.4879603470639893 ) ) ;
#79928 = CARTESIAN_POINT ( 'NONE',  ( -11.80575459840840047, 1482.971163947439891, 228.2220767440819884 ) ) ;
#79929 = CARTESIAN_POINT ( 'NONE',  ( -10.86918694159999887, 1472.641908963629930, 270.3751304083979790 ) ) ;
#79930 = CARTESIAN_POINT ( 'NONE',  ( 10.39122783130000016, 1420.703789618900146, 197.9464487691990087 ) ) ;
#79931 = CARTESIAN_POINT ( 'NONE',  ( 3.255911231930000316, 1435.946191916090129, 155.5160642224979881 ) ) ;
#79932 = CARTESIAN_POINT ( 'NONE',  ( -14.51158588560000062, 1474.168193539429922, 223.7580015587980142 ) ) ;
#79933 = CARTESIAN_POINT ( 'NONE',  ( 10.60236678890000128, 1431.113060387329824, 193.5879272064979943 ) ) ;
#79934 = CARTESIAN_POINT ( 'NONE',  ( -12.52061335139999976, 1420.940692459130105, 230.1659492372980083 ) ) ;
#79935 = AXIS2_PLACEMENT_3D ( 'NONE', #94423, #77647, #86592 ) ;
#79936 = CARTESIAN_POINT ( 'NONE',  ( -6.579934403380000241, 1457.806054071189919, 216.0580061265189897 ) ) ;
#79937 = CARTESIAN_POINT ( 'NONE',  ( 8.947167975125823958, 1361.631581952299712, 207.6218459616987673 ) ) ;
#79938 = CARTESIAN_POINT ( 'NONE',  ( -44.91570373049209763, 1434.529260160309832, 266.2100032643309646 ) ) ;
#79939 = ORIENTED_EDGE ( 'NONE', *, *, #52826, .F. ) ;
#79940 = CARTESIAN_POINT ( 'NONE',  ( -9.253356380629998768, 1423.298286757820051, 209.1001181959080100 ) ) ;
#79941 = EDGE_LOOP ( 'NONE', ( #57928, #20001, #59820, #39673, #65133 ) ) ;
#79942 = CARTESIAN_POINT ( 'NONE',  ( 6.952166382295000169, 1517.213554313520035, 210.8305935944869987 ) ) ;
#79943 = CARTESIAN_POINT ( 'NONE',  ( 2.895377824650565923, 1447.016636168100604, 182.3842140122979743 ) ) ;
#79944 = CARTESIAN_POINT ( 'NONE',  ( 13.03169765326649987, 1424.752599651019864, 222.9539081381209940 ) ) ;
#79945 = DIRECTION ( 'NONE',  ( 0.8304244102910536274, -0.2476038100681244025, 0.4990868181313787844 ) ) ;
#79946 = AXIS2_PLACEMENT_3D ( 'NONE', #95850, #61187, #18021 ) ;
#79947 = CARTESIAN_POINT ( 'NONE',  ( -1.190766908926550238, 1496.523138748749943, 221.4220572319329960 ) ) ;
#79948 = ORIENTED_EDGE ( 'NONE', *, *, #50184, .F. ) ;
#79949 = CARTESIAN_POINT ( 'NONE',  ( -113.4000000000000057, 1392.913060387289988, 304.2218459572590064 ) ) ;
#79950 = CARTESIAN_POINT ( 'NONE',  ( -4.035490750684999739, 1516.630499592039996, 201.4102952541169884 ) ) ;
#79951 = CARTESIAN_POINT ( 'NONE',  ( 6.420745879690000102, 1472.574659317690021, 217.2589463166690109 ) ) ;
#79952 = CARTESIAN_POINT ( 'NONE',  ( -8.414692022134790506, 1438.300249502180122, 206.9250335065700028 ) ) ;
#79953 = EDGE_LOOP ( 'NONE', ( #26311, #23824, #30864, #62373 ) ) ;
#79954 = CARTESIAN_POINT ( 'NONE',  ( -26.32366284865300088, 1415.625410839150163, 270.3533368716700238 ) ) ;
#79955 = CARTESIAN_POINT ( 'NONE',  ( 2.491655725414999800, 1516.977504706749869, 209.8569557413499922 ) ) ;
#79956 = CARTESIAN_POINT ( 'NONE',  ( -2.205156445730000137, 1428.435894572430016, 91.31218443469779800 ) ) ;
#79957 = DIRECTION ( 'NONE',  ( -0.000000000000000000, -1.000000000000000000, -0.000000000000000000 ) ) ;
#79959 = EDGE_LOOP ( 'NONE', ( #106685, #63854, #34200, #49564 ) ) ;
#79958 = CARTESIAN_POINT ( 'NONE',  ( -7.622296587833937487, 1365.431469736285635, 209.6218459617148824 ) ) ;
#79960 = ORIENTED_EDGE ( 'NONE', *, *, #20315, .F. ) ;
#79961 = CARTESIAN_POINT ( 'NONE',  ( 45.62277040061831457, 1441.770530636094918, 268.9751422883944656 ) ) ;
#79962 = CARTESIAN_POINT ( 'NONE',  ( 2.477236684321269866, 1466.740809377600044, 219.8979591610699913 ) ) ;
#79963 = DIRECTION ( 'NONE',  ( 0.000000000000000000, 1.000000000000000000, 0.000000000000000000 ) ) ;
#79964 = CARTESIAN_POINT ( 'NONE',  ( -0.01749107806689290112, 1408.977739893769922, 186.0382551112710132 ) ) ;
#79965 = AXIS2_PLACEMENT_3D ( 'NONE', #34387, #101560, #94846 ) ;
#79966 = FACE_OUTER_BOUND ( 'NONE', #33510, .T. ) ;
#79967 = CARTESIAN_POINT ( 'NONE',  ( 5.386185205460879644, 1432.347042709529887, 154.6076275981190236 ) ) ;
#79968 = CARTESIAN_POINT ( 'NONE',  ( -13.68772360880000072, 1420.178243169430061, 222.0123197414980041 ) ) ;
#79969 = CARTESIAN_POINT ( 'NONE',  ( -1.653188813474884666, 1467.000319734719596, 235.3477346490027742 ) ) ;
#79970 = CARTESIAN_POINT ( 'NONE',  ( 10.69046686070000085, 1445.373974055579993, 185.6902835676980033 ) ) ;
#79971 = CARTESIAN_POINT ( 'NONE',  ( -1.136547623115000016, 1516.839862955080207, 206.6438706166370025 ) ) ;
#79972 = ORIENTED_EDGE ( 'NONE', *, *, #45953, .T. ) ;
#79973 = DIRECTION ( 'NONE',  ( 5.980589973904019347E-17, -1.000000000000000000, 1.736889445713099699E-16 ) ) ;
#79974 = CARTESIAN_POINT ( 'NONE',  ( 1.474754854666479931, 1482.224443677059980, 182.1987295621239866 ) ) ;
#79975 = ORIENTED_EDGE ( 'NONE', *, *, #96028, .T. ) ;
#79976 = CARTESIAN_POINT ( 'NONE',  ( 3.915817772150960607, 1457.457976147669569, 228.5041087852198132 ) ) ;
#79977 = CARTESIAN_POINT ( 'NONE',  ( 24.33536485855309905, 1452.047573491060120, 136.5413356103030083 ) ) ;
#79978 = CARTESIAN_POINT ( 'NONE',  ( -13.84855700446339988, 1443.315687757889918, 195.7951355894199992 ) ) ;
#79979 = CARTESIAN_POINT ( 'NONE',  ( -31.91283005400000050, 1386.630794634020049, 206.3242904142690008 ) ) ;
#79980 = CARTESIAN_POINT ( 'NONE',  ( -3.815543930780000093, 1414.170066830949963, 206.6642445390390037 ) ) ;
#79981 = CARTESIAN_POINT ( 'NONE',  ( 19.41452480519999924, 1410.952374995430091, 196.0910004049979989 ) ) ;
#79982 = CARTESIAN_POINT ( 'NONE',  ( 12.93811130839999812, 1444.994950788469851, 169.4238961894979809 ) ) ;
#79983 = CARTESIAN_POINT ( 'NONE',  ( 16.16109259539999954, 1409.477418176630181, 225.0245223578980074 ) ) ;
#79984 = CARTESIAN_POINT ( 'NONE',  ( 10.84341014260000158, 1490.334183146890155, 204.2640498865189898 ) ) ;
#79985 = CARTESIAN_POINT ( 'NONE',  ( 4.500000000000000000, 1448.210448412289907, 182.3842140122979743 ) ) ;
#79986 = AXIS2_PLACEMENT_3D ( 'NONE', #47771, #21432, #56726 ) ;
#79987 = CARTESIAN_POINT ( 'NONE',  ( 2.500000000000000000, 1439.114301455650093, 157.7261946041980138 ) ) ;
#79988 = CARTESIAN_POINT ( 'NONE',  ( 1.711311228545000063, 1516.591755933730155, 214.8926661113670207 ) ) ;
#79989 = CARTESIAN_POINT ( 'NONE',  ( 3.261946504277382086, 1524.739563915922190, 241.7746690245087677 ) ) ;
#79990 = ORIENTED_EDGE ( 'NONE', *, *, #93991, .F. ) ;
#79991 = CARTESIAN_POINT ( 'NONE',  ( -17.28305401740000136, 1417.746658045750110, 207.2609050454489932 ) ) ;
#79992 = DIRECTION ( 'NONE',  ( 0.2562858833364869415, 0.008949701426205170993, -0.9665595940483019399 ) ) ;
#79993 = DIRECTION ( 'NONE',  ( 0.4794255386042041156, -2.935634756405673411E-17, -0.8775825618903722036 ) ) ;
#79994 = EDGE_CURVE ( 'NONE', #53103, #88887, #68398, .T. ) ;
#79995 = CARTESIAN_POINT ( 'NONE',  ( 4.380123746805410612, 1517.051697240460271, 201.6648244196679798 ) ) ;
#79996 = CARTESIAN_POINT ( 'NONE',  ( -38.15885483313930138, 1448.679264857810040, 136.3994482979960026 ) ) ;
#79997 = DIRECTION ( 'NONE',  ( 0.002120872317174225027, 0.9999913661844083146, -0.003573437736249155880 ) ) ;
#79998 = CARTESIAN_POINT ( 'NONE',  ( -22.74199305119999792, 1446.314437877210139, 234.3916895697979612 ) ) ;
#79999 = CARTESIAN_POINT ( 'NONE',  ( 17.76546875260000036, 1430.865606781589804, 204.9340536459789917 ) ) ;
#80000 = CARTESIAN_POINT ( 'NONE',  ( 11.59597807620000154, 1433.182955382529826, 151.0968555446979735 ) ) ;
#80001 = ADVANCED_FACE ( 'NONE', ( #10972 ), #55200, .T. ) ;
#80002 = CARTESIAN_POINT ( 'NONE',  ( -2.086158904326180341, 1474.140508472220063, 270.1368012846049851 ) ) ;
#80003 = CARTESIAN_POINT ( 'NONE',  ( 24.69096861020820199, 1440.913060394919967, 214.0095001576269738 ) ) ;
#80004 = CARTESIAN_POINT ( 'NONE',  ( -109.8796183239999920, 1385.344994265080004, 297.0482512251589924 ) ) ;
#80005 = CARTESIAN_POINT ( 'NONE',  ( 11.07831394190110075, 1500.667860359830001, 205.8219701691039916 ) ) ;
#80006 = EDGE_LOOP ( 'NONE', ( #108150, #2978, #61300, #106331 ) ) ;
#80007 = CARTESIAN_POINT ( 'NONE',  ( -105.4653109980351076, 1391.248289814977625, 304.9316009898920470 ) ) ;
#80008 = CARTESIAN_POINT ( 'NONE',  ( 18.89959486413309975, 1416.839692127159879, 210.6687135792209915 ) ) ;
#80009 = CIRCLE ( 'NONE', #8454, 65.59183216034817576 ) ;
#80010 = CARTESIAN_POINT ( 'NONE',  ( -19.31939586139944254, 1485.616822396989619, 189.8190535202998603 ) ) ;
#80011 = CARTESIAN_POINT ( 'NONE',  ( 8.104840167896952607, 1398.153761633497197, 198.9574189372607123 ) ) ;
#80012 = CARTESIAN_POINT ( 'NONE',  ( 2.637616553089999982, 1474.725858340030072, 234.5358300088979888 ) ) ;
#80013 = B_SPLINE_CURVE_WITH_KNOTS ( 'NONE', 3,
 ( #25619, #96156, #61476, #27852, #78247, #68228, #103430 ),
 .UNSPECIFIED., .F., .F.,
 ( 4, 3, 4 ),
 ( -108.0170515669999958, -74.06595527500620335, -37.80268138969999825 ),
 .UNSPECIFIED. ) ;
#80014 = CARTESIAN_POINT ( 'NONE',  ( 24.93139309710000262, 1449.798359900550167, 212.9211815600280033 ) ) ;
#80015 = VECTOR ( 'NONE', #102582, 1000.000000000000000 ) ;
#80016 = CARTESIAN_POINT ( 'NONE',  ( -16.54816711760097547, 1420.093509083089202, 208.5750742618841400 ) ) ;
#80017 = CARTESIAN_POINT ( 'NONE',  ( -14.38163500639999981, 1509.358420488030106, 233.7087952759979999 ) ) ;
#80018 = CARTESIAN_POINT ( 'NONE',  ( -21.83573956349999889, 1383.851617847329862, 221.6010342889879894 ) ) ;
#80019 = CARTESIAN_POINT ( 'NONE',  ( -4.487359966065140426, 1509.034537944679869, 206.0057109289620030 ) ) ;
#80020 = CARTESIAN_POINT ( 'NONE',  ( 6.294750265859999416, 1408.079328832830015, 220.7028845648979711 ) ) ;
#80021 = CARTESIAN_POINT ( 'NONE',  ( -14.87918228200000037, 1415.865102022439942, 212.9009079454490063 ) ) ;
#80022 = DIRECTION ( 'NONE',  ( 0.4794254784390402646, 5.727640580602533849E-10, 0.8775825947587483356 ) ) ;
#80024 = ORIENTED_EDGE ( 'NONE', *, *, #54205, .F. ) ;
#80023 = CARTESIAN_POINT ( 'NONE',  ( -41.65810620650000828, 1443.954352776429914, 135.6863023723980177 ) ) ;
#80025 = CARTESIAN_POINT ( 'NONE',  ( -1.297832609859999931, 1452.391379596130037, 183.7169094889979988 ) ) ;
#80026 = CARTESIAN_POINT ( 'NONE',  ( -3.078458294050000266, 1383.868666969369770, 218.4015365393190109 ) ) ;
#80027 = LINE ( 'NONE', #88429, #54990 ) ;
#80029 = ORIENTED_EDGE ( 'NONE', *, *, #99903, .F. ) ;
#80028 = CARTESIAN_POINT ( 'NONE',  ( 17.15830831501806131, 1512.187213306747481, 209.3391145445731070 ) ) ;
#80030 = CARTESIAN_POINT ( 'NONE',  ( 11.27336394452900059, 1433.557839144309810, 225.8166928899180164 ) ) ;
#80031 = ORIENTED_EDGE ( 'NONE', *, *, #62287, .T. ) ;
#80032 = CARTESIAN_POINT ( 'NONE',  ( -9.309222779429999761, 1389.084088572969904, 217.3257696767689993 ) ) ;
#80033 = LINE ( 'NONE', #36920, #105193 ) ;
#80034 = CARTESIAN_POINT ( 'NONE',  ( 28.34436068694596500, 1509.902867273254287, 202.2339729425384007 ) ) ;
#80035 = CARTESIAN_POINT ( 'NONE',  ( -2.145980225789999807, 1431.918816440389946, 217.3940193458890064 ) ) ;
#80036 = CARTESIAN_POINT ( 'NONE',  ( 20.40004974522683767, 1509.667807812142883, 187.4863181757289681 ) ) ;
#80037 = CIRCLE ( 'NONE', #38857, 33.13701971169416538 ) ;
#80038 = CARTESIAN_POINT ( 'NONE',  ( 13.82144533499180028, 1409.395715893920169, 203.4549396693699919 ) ) ;
#80039 = CARTESIAN_POINT ( 'NONE',  ( -31.23437356469425907, 1511.187213306747708, 222.8968241038848248 ) ) ;
#80040 = CARTESIAN_POINT ( 'NONE',  ( -90.07212409636069594, 1385.192969068609955, 292.6181576655579875 ) ) ;
#80041 = DIRECTION ( 'NONE',  ( -0.4999999999998399058, 0.7071067811867739472, -0.4999999999998399058 ) ) ;
#80042 = CARTESIAN_POINT ( 'NONE',  ( 11.41327087716770095, 1427.619034137559765, 209.6360973194659891 ) ) ;
#80043 = CARTESIAN_POINT ( 'NONE',  ( 13.51610093809999924, 1443.913060387330006, 169.3501091259980171 ) ) ;
#80044 = ORIENTED_EDGE ( 'NONE', *, *, #50922, .T. ) ;
#80045 = ORIENTED_EDGE ( 'NONE', *, *, #107537, .T. ) ;
#80046 = CARTESIAN_POINT ( 'NONE',  ( -11.57234447566209923, 1415.219159636060112, 195.3490233354060308 ) ) ;
#80047 = CARTESIAN_POINT ( 'NONE',  ( -2.075886983448210099, 1496.000771925150048, 196.9582277030409898 ) ) ;
#80048 = CARTESIAN_POINT ( 'NONE',  ( 16.20698216735619468, 1469.058401758687296, 269.3699621073229196 ) ) ;
#80049 = FACE_OUTER_BOUND ( 'NONE', #26768, .T. ) ;
#80050 = CARTESIAN_POINT ( 'NONE',  ( -27.78452750130110260, 1508.000976266860107, 210.4681927182890036 ) ) ;
#80051 = CARTESIAN_POINT ( 'NONE',  ( 32.05521452193837462, 1525.253996226948402, 201.2193335479506118 ) ) ;
#80052 = CARTESIAN_POINT ( 'NONE',  ( -0.1575406214799999760, 1462.356505213130049, 182.8094439125979989 ) ) ;
#80053 = CARTESIAN_POINT ( 'NONE',  ( -11.13778651236117057, 1367.489867554787679, 209.6218459617033432 ) ) ;
#80054 = CARTESIAN_POINT ( 'NONE',  ( -25.77751368618157102, 1436.654609691480573, 137.0719439152050256 ) ) ;
#80055 = CARTESIAN_POINT ( 'NONE',  ( 4.608417506514999928, 1516.691389976299888, 206.6316000176769876 ) ) ;
#80056 = CIRCLE ( 'NONE', #83567, 40.01690241380000401 ) ;
#80057 = CARTESIAN_POINT ( 'NONE',  ( -2.143764089412641738, 1525.848198008145346, 176.8604052475766650 ) ) ;
#80058 = CARTESIAN_POINT ( 'NONE',  ( -8.021592841849999544, 1384.982153790620032, 218.7868050085690186 ) ) ;
#80059 = CARTESIAN_POINT ( 'NONE',  ( 17.17241001986506888, 1512.187213306747481, 238.6251415217915337 ) ) ;
#80060 = CARTESIAN_POINT ( 'NONE',  ( 20.36637623643389716, 1500.297579758999973, 227.4379270215500242 ) ) ;
#80061 = CARTESIAN_POINT ( 'NONE',  ( -2.832179855692609660, 1497.533054541979936, 201.1364361656100073 ) ) ;
#80062 = CARTESIAN_POINT ( 'NONE',  ( -103.6168536339999946, 1379.900079317219934, 303.2097866628589600 ) ) ;
#80063 = ORIENTED_EDGE ( 'NONE', *, *, #100660, .F. ) ;
#80064 = CARTESIAN_POINT ( 'NONE',  ( 11.86100282799569960, 1492.894947744830006, 212.5846961511890072 ) ) ;
#80065 = CARTESIAN_POINT ( 'NONE',  ( -26.30775428199999766, 1469.245646017629952, 207.3898640084980229 ) ) ;
#80067 = CARTESIAN_POINT ( 'NONE',  ( 13.45946769660000086, 1415.628674266529742, 196.7502466371980177 ) ) ;
#80066 = CARTESIAN_POINT ( 'NONE',  ( -11.01735835230000049, 1426.937595289829915, 91.95967800869790665 ) ) ;
#80068 = EDGE_CURVE ( 'NONE', #508, #6446, #3700, .T. ) ;
#80069 = DIRECTION ( 'NONE',  ( -1.000000000000000000, -2.249639673992789970E-32, -1.224646799147350002E-16 ) ) ;
#80070 = CARTESIAN_POINT ( 'NONE',  ( -36.81312563220000555, 1438.597774659029938, 254.5659314777980455 ) ) ;
#80071 = CARTESIAN_POINT ( 'NONE',  ( 3.584503077479999966, 1486.500511906190013, 219.3043361389989911 ) ) ;
#80072 = EDGE_CURVE ( 'NONE', #60488, #41404, #22926, .T. ) ;
#80073 = EDGE_CURVE ( 'NONE', #85994, #80823, #63068, .T. ) ;
#80074 = DIRECTION ( 'NONE',  ( 0.000000000000000000, 0.000000000000000000, 1.000000000000000000 ) ) ;
#80075 = CARTESIAN_POINT ( 'NONE',  ( -22.91555022173351475, 1409.723203468988913, 208.8960394818137161 ) ) ;
#80076 = EDGE_LOOP ( 'NONE', ( #32209, #38456, #61264, #76448 ) ) ;
#80077 = FACE_OUTER_BOUND ( 'NONE', #75237, .T. ) ;
#80078 = CARTESIAN_POINT ( 'NONE',  ( -19.74860284620000073, 1465.132576429690062, 209.4730770639620232 ) ) ;
#80079 = CARTESIAN_POINT ( 'NONE',  ( 5.857737085409999267, 1509.117617073830161, 238.0531267651979874 ) ) ;
#80080 = VERTEX_POINT ( 'NONE', #37739 ) ;
#80081 = ORIENTED_EDGE ( 'NONE', *, *, #11251, .T. ) ;
#80082 = AXIS2_PLACEMENT_3D ( 'NONE', #84006, #8392, #66686 ) ;
#80083 = CARTESIAN_POINT ( 'NONE',  ( 10.50975973408020003, 1452.933536048200040, 210.5056026378560148 ) ) ;
#80084 = CARTESIAN_POINT ( 'NONE',  ( 5.877311519840000997, 1423.581874179079932, 194.6993958404989939 ) ) ;
#80085 = EDGE_LOOP ( 'NONE', ( #1872, #30910, #78799, #58453 ) ) ;
#80086 = CARTESIAN_POINT ( 'NONE',  ( -1.074930184170000080, 1413.843955136130035, 185.1690177555979915 ) ) ;
#80087 = CARTESIAN_POINT ( 'NONE',  ( 5.650554513050000338, 1452.063338381489984, 211.4905750950089782 ) ) ;
#80088 = CARTESIAN_POINT ( 'NONE',  ( -2.361437468280000118, 1479.773351731729917, 235.7524046215980036 ) ) ;
#80089 = CARTESIAN_POINT ( 'NONE',  ( 2.487924132557410406, 1509.038643261319976, 213.6090950281819971 ) ) ;
#80090 = ORIENTED_EDGE ( 'NONE', *, *, #72671, .T. ) ;
#80091 = AXIS2_PLACEMENT_3D ( 'NONE', #93565, #25806, #24694 ) ;
#80092 = FACE_OUTER_BOUND ( 'NONE', #45938, .T. ) ;
#80093 = CARTESIAN_POINT ( 'NONE',  ( -12.77961858748070156, 1414.913057834409983, 220.2176620357280115 ) ) ;
#80094 = CARTESIAN_POINT ( 'NONE',  ( 13.89869200000000049, 1452.835253893030085, 223.8385666725980059 ) ) ;
#80095 = ORIENTED_EDGE ( 'NONE', *, *, #1145, .T. ) ;
#80096 = CARTESIAN_POINT ( 'NONE',  ( -2.294209667535000108, 1516.603620185149794, 203.3509623682169831 ) ) ;
#80097 = ORIENTED_EDGE ( 'NONE', *, *, #37063, .F. ) ;
#80098 = CARTESIAN_POINT ( 'NONE',  ( 11.85300018840249869, 1431.425274647949891, 149.9062840562949930 ) ) ;
#80099 = CARTESIAN_POINT ( 'NONE',  ( 12.69590191108945376, 1445.017070807032269, 186.3645745659958095 ) ) ;
#80100 = VERTEX_POINT ( 'NONE', #26564 ) ;
#80101 = VERTEX_POINT ( 'NONE', #87031 ) ;
#80102 = CARTESIAN_POINT ( 'NONE',  ( 2.456601303385831159, 1523.611961620354123, 175.3003469896238755 ) ) ;
#80103 = CARTESIAN_POINT ( 'NONE',  ( -3.726340750997230167, 1508.413954212639737, 220.4799730696009874 ) ) ;
#80104 = CARTESIAN_POINT ( 'NONE',  ( 7.745985074145769644, 1500.304699407309954, 200.5303357369510024 ) ) ;
#80105 = ADVANCED_FACE ( 'NONE', ( #10320 ), #69354, .T. ) ;
#80106 = CARTESIAN_POINT ( 'NONE',  ( -5.992196956094850258, 1469.346592943629958, 217.7944395441180063 ) ) ;
#80107 = CARTESIAN_POINT ( 'NONE',  ( 23.43477590392700094, 1452.094699979900042, 137.9018702996609989 ) ) ;
#80108 = CARTESIAN_POINT ( 'NONE',  ( 0.4870561706949109726, 1408.236684636520067, 270.3925729436620031 ) ) ;
#80109 = CARTESIAN_POINT ( 'NONE',  ( 5.556349309971470696, 1511.457792576160728, 217.8325609232749969 ) ) ;
#80110 = CARTESIAN_POINT ( 'NONE',  ( -4.818089418980000538, 1474.858188511989965, 199.5909791398490256 ) ) ;
#80111 = CARTESIAN_POINT ( 'NONE',  ( -19.59037083185129546, 1509.615009600280473, 231.2999628551918363 ) ) ;
#80112 = CARTESIAN_POINT ( 'NONE',  ( 8.436189838809218244, 1424.545028496175973, 195.7325651230689232 ) ) ;
#80114 = CARTESIAN_POINT ( 'NONE',  ( 10.14614976752910103, 1469.287792262710127, 204.1824843846119961 ) ) ;
#80113 = CARTESIAN_POINT ( 'NONE',  ( -13.43985408640000045, 1503.346475151690129, 208.6824759411649950 ) ) ;
#80115 = CARTESIAN_POINT ( 'NONE',  ( 11.85624328898539837, 1421.937062395870043, 207.3014288908249796 ) ) ;
#80116 = CARTESIAN_POINT ( 'NONE',  ( 17.64461694360119992, 1412.137575667770079, 224.8446746702369978 ) ) ;
#80117 = CARTESIAN_POINT ( 'NONE',  ( -7.170545816755000246, 1512.974587999889991, 202.0495477424069861 ) ) ;
#80118 = VERTEX_POINT ( 'NONE', #47242 ) ;
#80119 = CARTESIAN_POINT ( 'NONE',  ( 36.99165393039999827, 1427.133824787730191, 268.3665355202980436 ) ) ;
#80120 = DIRECTION ( 'NONE',  ( 0.000000000000000000, 0.07593562622321022026, -0.9971127221483482295 ) ) ;
#80121 = CARTESIAN_POINT ( 'NONE',  ( -76.22128121885890550, 1385.004381994479900, 301.0818327933589558 ) ) ;
#80122 = DIRECTION ( 'NONE',  ( 0.7071067811865475727, -1.473812113707079404E-16, -0.7071067811865475727 ) ) ;
#80123 = CARTESIAN_POINT ( 'NONE',  ( 3.756915432050000003, 1505.735347371189846, 220.9097465364990001 ) ) ;
#80124 =( BOUNDED_SURFACE ( )  B_SPLINE_SURFACE ( 3, 2, ( 
 ( #55683, #66294, #32108 ),
 ( #64083, #13624, #21473 ),
 ( #100410, #98755, #38842 ),
 ( #14190, #14747, #56769 ),
 ( #5251, #83063, #30450 ),
 ( #64634, #23694, #48934 ),
 ( #72474, #57342, #73019 ),
 ( #47263, #108813, #22015 ),
 ( #73583, #65725, #81385 ),
 ( #56213, #91466, #108258 ),
 ( #31547, #22564, #39407 ),
 ( #57879, #15282, #6354 ),
 ( #90343, #74680, #89805 ),
 ( #38294, #106604, #92012 ) ),
 .UNSPECIFIED., .F., .F., .F. ) 
 B_SPLINE_SURFACE_WITH_KNOTS ( ( 4, 2, 2, 2, 2, 2, 4 ),
 ( 3, 3 ),
 ( 7.470152968425125550E-17, 0.0009443072508236408525, 0.001416460876235424091, 0.001888614501647207112, 0.002360768127058990133, 0.002832921752470773588, 0.003777229003294339631 ),
 ( 0.000000000000000000, 1.000000000000000000 ),
 .UNSPECIFIED. ) 
 GEOMETRIC_REPRESENTATION_ITEM ( )  RATIONAL_B_SPLINE_SURFACE ( (
 ( 1.000000000000000000, 0.9376006582765959996, 1.000000000000000000),
 ( 1.000000000000000000, 0.9283977714734229503, 1.000000000000000000),
 ( 1.000000000000000000, 0.9189750060483535821, 1.000000000000000000),
 ( 1.000000000000000000, 0.9042792056125676936, 1.000000000000000000),
 ( 1.000000000000000000, 0.8992469033842545034, 1.000000000000000000),
 ( 1.000000000000000000, 0.8891280264682865919, 1.000000000000000000),
 ( 1.000000000000000000, 0.8840337471676149583, 1.000000000000000000),
 ( 1.000000000000000000, 0.8736395124162725789, 1.000000000000000000),
 ( 1.000000000000000000, 0.8683406746555091260, 1.000000000000000000),
 ( 1.000000000000000000, 0.8573361860705441817, 1.000000000000000000),
 ( 1.000000000000000000, 0.8516508399497870752, 1.000000000000000000),
 ( 1.000000000000000000, 0.8340914917062759448, 1.000000000000000000),
 ( 1.000000000000000000, 0.8215597275864434668, 1.000000000000000000),
 ( 1.000000000000000000, 0.8070209408750140812, 1.000000000000000000) ) ) 
 REPRESENTATION_ITEM ( '' )  SURFACE ( )  );
#80125 = CARTESIAN_POINT ( 'NONE',  ( -15.10167272650000037, 1416.016604972820005, 212.2622663138990049 ) ) ;
#80127 = ORIENTED_EDGE ( 'NONE', *, *, #25225, .F. ) ;
#80126 = CARTESIAN_POINT ( 'NONE',  ( -16.85518942986550073, 1419.928483354570062, 208.4319138966170044 ) ) ;
#80128 = CARTESIAN_POINT ( 'NONE',  ( -17.08097489138819824, 1418.110424922289894, 204.4848448838540094 ) ) ;
#80129 = CARTESIAN_POINT ( 'NONE',  ( -24.89775517959999718, 1442.835547152150184, 210.5176497469579999 ) ) ;
#80130 = CARTESIAN_POINT ( 'NONE',  ( -11.63669227459999966, 1425.864836378729933, 144.1684971660979784 ) ) ;
#80131 = CARTESIAN_POINT ( 'NONE',  ( -11.66658784013729999, 1391.913060387289988, 209.7120188154370339 ) ) ;
#80132 = EDGE_CURVE ( 'NONE', #13404, #100009, #94182, .T. ) ;
#80133 = CARTESIAN_POINT ( 'NONE',  ( 13.59755238133500121, 1512.525301340730039, 224.9104059524669879 ) ) ;
#80134 = CARTESIAN_POINT ( 'NONE',  ( 4.408076783308741753, 1370.458220770605067, 208.8302519701303765 ) ) ;
#80135 = CARTESIAN_POINT ( 'NONE',  ( 13.11760263369310131, 1509.411057675469692, 181.1735613693849984 ) ) ;
#80136 = CARTESIAN_POINT ( 'NONE',  ( 6.992116644224409150, 1458.468605612649981, 201.2966203680600188 ) ) ;
#80137 = CARTESIAN_POINT ( 'NONE',  ( -13.15726448721240160, 1416.851343896870048, 221.9096085506390068 ) ) ;
#80138 = CARTESIAN_POINT ( 'NONE',  ( 13.51135493409999988, 1415.081657033430020, 228.4979249935979908 ) ) ;
#80139 = CARTESIAN_POINT ( 'NONE',  ( -3.410174724169999561, 1476.067642852090103, 219.2827967179989912 ) ) ;
#80141 = CARTESIAN_POINT ( 'NONE',  ( -16.61355167848200054, 1459.966389597419948, 228.4924131504890283 ) ) ;
#80140 = AXIS2_PLACEMENT_3D ( 'NONE', #74685, #16381, #66299 ) ;
#80142 = CARTESIAN_POINT ( 'NONE',  ( 5.770820141135000192, 1516.591755933730155, 207.4105347035570048 ) ) ;
#80143 = CARTESIAN_POINT ( 'NONE',  ( 46.27884742629999693, 1440.913084543189825, 267.5894369069980030 ) ) ;
#80144 = CARTESIAN_POINT ( 'NONE',  ( -18.90483148029999683, 1410.069205653730023, 222.7218158439980016 ) ) ;
#80145 = CARTESIAN_POINT ( 'NONE',  ( 19.01901943839999731, 1435.591100437959767, 145.9747268152980268 ) ) ;
#80146 = CARTESIAN_POINT ( 'NONE',  ( 24.99925640249999859, 1488.577142715929995, 200.8921111725379944 ) ) ;
#80147 = CARTESIAN_POINT ( 'NONE',  ( 29.76859869597256036, 1509.997910412159627, 208.7253019497961475 ) ) ;
#80148 = CARTESIAN_POINT ( 'NONE',  ( -13.57853027955069969, 1379.569703739710121, 207.8817176012079813 ) ) ;
#80149 = CARTESIAN_POINT ( 'NONE',  ( -0.1075775631909999946, 1475.837061347730014, 266.9611530679979978 ) ) ;
#80150 = CARTESIAN_POINT ( 'NONE',  ( -14.80628304904369941, 1417.712450806070137, 203.2308112443149923 ) ) ;
#80151 = CARTESIAN_POINT ( 'NONE',  ( -33.93525073091490185, 1436.160847652960001, 136.3001632569819890 ) ) ;
#80152 = CARTESIAN_POINT ( 'NONE',  ( -13.59572565769999919, 1409.328701682329893, 203.3447866184380075 ) ) ;
#80153 = CARTESIAN_POINT ( 'NONE',  ( -16.76688489720000064, 1417.005534796029906, 207.9255659622089922 ) ) ;
#80154 = CARTESIAN_POINT ( 'NONE',  ( -16.19493240869999795, 1409.478599888930148, 193.4350318414979881 ) ) ;
#80155 = CARTESIAN_POINT ( 'NONE',  ( -7.606524257758859875, 1383.989784261539853, 219.0105849715669990 ) ) ;
#80156 = CARTESIAN_POINT ( 'NONE',  ( 11.87591311449999942, 1433.006404943239886, 146.5967610804979984 ) ) ;
#80157 = CARTESIAN_POINT ( 'NONE',  ( -26.79413260980000189, 1435.433175380389912, 135.2874982680980054 ) ) ;
#80158 = DIRECTION ( 'NONE',  ( 0.000000000000000000, 0.000000000000000000, 1.000000000000000000 ) ) ;
#80159 = ORIENTED_EDGE ( 'NONE', *, *, #73472, .T. ) ;
#80160 = DIRECTION ( 'NONE',  ( 0.3090169943749654369, 2.144236138472418401E-15, 0.9510565162951478690 ) ) ;
#80161 = CARTESIAN_POINT ( 'NONE',  ( 27.93599228869999607, 1442.648988978960006, 137.4365311675980195 ) ) ;
#80162 = CARTESIAN_POINT ( 'NONE',  ( 33.43367350703735497, 1524.397344074318653, 197.7663411554291315 ) ) ;
#80163 = VECTOR ( 'NONE', #31227, 1000.000000000000000 ) ;
#80164 = EDGE_CURVE ( 'NONE', #99465, #77064, #15651, .T. ) ;
#80165 = CARTESIAN_POINT ( 'NONE',  ( -13.30990274189880118, 1508.450031501719877, 209.7671136656329907 ) ) ;
#80166 = CARTESIAN_POINT ( 'NONE',  ( -38.70127719692458612, 1443.913060387331370, 136.9798462687442679 ) ) ;
#80167 = CARTESIAN_POINT ( 'NONE',  ( -26.91513671580000278, 1469.147785373630086, 269.0204381106979667 ) ) ;
#80168 = CARTESIAN_POINT ( 'NONE',  ( -11.83167355530729914, 1481.599286403459928, 209.9607897767780003 ) ) ;
#80169 = VECTOR ( 'NONE', #104144, 1000.000000000000000 ) ;
#80170 = FACE_OUTER_BOUND ( 'NONE', #81658, .T. ) ;
#80171 = EDGE_CURVE ( 'NONE', #35203, #84750, #55117, .T. ) ;
#80172 = CARTESIAN_POINT ( 'NONE',  ( 20.49599333844867033, 1525.960063244516959, 233.8638087104924068 ) ) ;
#80173 = CARTESIAN_POINT ( 'NONE',  ( -91.22755695539819953, 1384.616955451200056, 309.0857609642320085 ) ) ;
#80174 = B_SPLINE_SURFACE_WITH_KNOTS ( 'NONE', 5, 5, ( 
 ( #105071, #37319, #71515, #43519, #103386, #10453 ),
 ( #60889, #78768, #9899, #974, #19385, #69281 ),
 ( #2083, #70397, #61438, #18283, #86605, #27813 ),
 ( #82056, #73696, #63647, #106171, #22681, #89911 ),
 ( #30562, #65290, #46298, #73125, #99403, #46841 ),
 ( #72580, #90459, #80969, #56326, #107822, #13736 ),
 ( #28920, #38404, #105634, #3740, #64752, #21034 ),
 ( #13184, #47920, #98311, #4274, #63111, #48490 ),
 ( #64189, #106708, #12662, #4800, #31110, #29998 ) ),
 .UNSPECIFIED., .F., .F., .F.,
 ( 6, 3, 6 ),
 ( 6, 6 ),
 ( 8.763103464980000368, 19.90566978349999872, 30.47641535120000000 ),
 ( -2.775557561569999727E-17, 2.000000000000000000 ),
 .UNSPECIFIED. ) ;
#80175 = CARTESIAN_POINT ( 'NONE',  ( -29.90545723663199951, 1384.968601192589858, 205.5110789169119982 ) ) ;
#80176 = CARTESIAN_POINT ( 'NONE',  ( -5.364792434415069700, 1374.934204522590107, 214.8728634718659976 ) ) ;
#80177 = CARTESIAN_POINT ( 'NONE',  ( 22.52097504219999990, 1509.699510165530000, 227.8690926855979910 ) ) ;
#80178 = AXIS2_PLACEMENT_3D ( 'NONE', #12133, #90488, #38973 ) ;
#80179 = CARTESIAN_POINT ( 'NONE',  ( -6.446325585610000353, 1432.345375419369930, 154.6647257196979979 ) ) ;
#80180 = CARTESIAN_POINT ( 'NONE',  ( -9.234134023826198856, 1461.205490114660051, 206.1827678865119822 ) ) ;
#80182 = VERTEX_POINT ( 'NONE', #39385 ) ;
#80181 = CARTESIAN_POINT ( 'NONE',  ( 4.328507561560000383, 1515.100736413590084, 208.0459478947190064 ) ) ;
#80183 = CARTESIAN_POINT ( 'NONE',  ( -8.848156404039999146, 1384.935949319609790, 199.9247822318290275 ) ) ;
#80184 = AXIS2_PLACEMENT_3D ( 'NONE', #93706, #68553, #16984 ) ;
#80185 = DIRECTION ( 'NONE',  ( -2.275957200478543654E-15, -0.7071067811865475727, -0.7071067811865475727 ) ) ;
#80186 = CARTESIAN_POINT ( 'NONE',  ( 2.596261494520241353, 1525.907212628473644, 177.4701144822246874 ) ) ;
#80187 = AXIS2_PLACEMENT_3D ( 'NONE', #35299, #17361, #10095 ) ;
#80188 = CARTESIAN_POINT ( 'NONE',  ( -12.33246611440000073, 1415.579607672129896, 195.5076102655979753 ) ) ;
#80189 = DIRECTION ( 'NONE',  ( -0.6736849260863839728, 0.000000000000000000, 0.7390186874254150995 ) ) ;
#80190 = CARTESIAN_POINT ( 'NONE',  ( 22.60280089679999804, 1409.702367587229901, 211.4725249609479931 ) ) ;
#80191 = CARTESIAN_POINT ( 'NONE',  ( -106.5816461138369959, 1391.913060387289988, 305.5142355297590484 ) ) ;
#80192 = CARTESIAN_POINT ( 'NONE',  ( 18.91865458690000068, 1456.348387323389943, 200.2117427500890017 ) ) ;
#80193 = CARTESIAN_POINT ( 'NONE',  ( -15.97230909389999987, 1420.722884146229717, 227.0315162960980047 ) ) ;
#80195 = CARTESIAN_POINT ( 'NONE',  ( -12.46974414340000159, 1379.786009550329936, 205.4121433733889717 ) ) ;
#80194 = CARTESIAN_POINT ( 'NONE',  ( -11.87312849439999951, 1432.864063127479994, 149.9809861782979965 ) ) ;
#80196 = CARTESIAN_POINT ( 'NONE',  ( 1.363639804150000190, 1415.765549334430034, 232.8698634931980109 ) ) ;
#80197 = CARTESIAN_POINT ( 'NONE',  ( -101.1419410403000256, 1375.179104070690528, 307.3518423499588152 ) ) ;
#80198 = CARTESIAN_POINT ( 'NONE',  ( 2201.413669186790685, 11221.53578756870047, -1523.112345774690311 ) ) ;
#80199 = CARTESIAN_POINT ( 'NONE',  ( 5.690155709095000347, 1515.224164712790071, 200.9877428003970010 ) ) ;
#80200 = CARTESIAN_POINT ( 'NONE',  ( 4.261736551907978843, 1515.372048949687269, 206.7917118349798784 ) ) ;
#80201 = CARTESIAN_POINT ( 'NONE',  ( 1.121950743945000051, 1517.123342927159911, 204.1084165760470057 ) ) ;
#80202 = AXIS2_PLACEMENT_3D ( 'NONE', #91374, #108165, #93009 ) ;
#80203 = CARTESIAN_POINT ( 'NONE',  ( -20.58707213139999936, 1427.974737749530050, 223.4007331328979831 ) ) ;
#80204 = EDGE_CURVE ( 'NONE', #104137, #16269, #77694, .T. ) ;
#80205 = CARTESIAN_POINT ( 'NONE',  ( -16.28303581252109922, 1485.105577738389911, 187.8116298709459784 ) ) ;
#80206 = CARTESIAN_POINT ( 'NONE',  ( -13.13304581337124333, 1421.347500487118850, 210.6408966550871185 ) ) ;
#80208 = ORIENTED_EDGE ( 'NONE', *, *, #105810, .F. ) ;
#80207 = CARTESIAN_POINT ( 'NONE',  ( -68.39881485729999611, 1379.747709036749939, 279.9507912016590012 ) ) ;
#80209 = VERTEX_POINT ( 'NONE', #99269 ) ;
#80210 = CARTESIAN_POINT ( 'NONE',  ( 29.42769729879999829, 1509.955660133030051, 212.2907639111579954 ) ) ;
#80211 = ORIENTED_EDGE ( 'NONE', *, *, #66546, .T. ) ;
#80212 = CARTESIAN_POINT ( 'NONE',  ( -19.66678637246580053, 1521.951704408389787, 215.8936635744080093 ) ) ;
#80213 = ADVANCED_FACE ( 'NONE', ( #72459 ), #17422, .T. ) ;
#80214 = CARTESIAN_POINT ( 'NONE',  ( -109.3083906640000009, 1384.947550057740045, 311.2644960252590067 ) ) ;
#80216 = DIRECTION ( 'NONE',  ( -2.028721370088317945E-13, -0.03085824620774639884, 0.9995237709234243706 ) ) ;
#80215 = CARTESIAN_POINT ( 'NONE',  ( 1.525139958810000085, 1427.692446166030095, 112.4493539157979995 ) ) ;
#80217 = CARTESIAN_POINT ( 'NONE',  ( -1.317811661047102012, 1517.051704408389924, 194.7136484256038500 ) ) ;
#80218 = EDGE_CURVE ( 'NONE', #60042, #38113, #44311, .T. ) ;
#80219 = CARTESIAN_POINT ( 'NONE',  ( -24.93976076479000170, 1451.594252318390090, 137.3267138200340014 ) ) ;
#80220 = CARTESIAN_POINT ( 'NONE',  ( 0.8374757675929990208, 1467.465564401289839, 219.8067306195990227 ) ) ;
#80221 = CARTESIAN_POINT ( 'NONE',  ( 10.56558922819999857, 1409.282018893330132, 228.0601045111980056 ) ) ;
#80222 = CARTESIAN_POINT ( 'NONE',  ( 10.18158772832410008, 1482.093709488619879, 212.1941923381180004 ) ) ;
#80223 =( LENGTH_UNIT ( ) NAMED_UNIT ( * ) SI_UNIT ( .MILLI., .METRE. ) );
#80224 = CARTESIAN_POINT ( 'NONE',  ( -7.322105105754999954, 1516.572193931679976, 211.9951753309869957 ) ) ;
#80225 = CARTESIAN_POINT ( 'NONE',  ( 41.66188030070010484, 1443.907795131820194, 134.0999999982419979 ) ) ;
#80226 = EDGE_LOOP ( 'NONE', ( #17739, #29387, #44556 ) ) ;
#80227 = CARTESIAN_POINT ( 'NONE',  ( 18.68390456929999743, 1457.534965338390066, 220.6831945507989872 ) ) ;
#80228 = CARTESIAN_POINT ( 'NONE',  ( -17.19739463999606599, 1525.960063244516959, 236.2603809477411971 ) ) ;
#80229 = ORIENTED_EDGE ( 'NONE', *, *, #73495, .F. ) ;
#80230 = ORIENTED_EDGE ( 'NONE', *, *, #42653, .F. ) ;
#80231 = ORIENTED_EDGE ( 'NONE', *, *, #85761, .F. ) ;
#80232 = ADVANCED_FACE ( 'NONE', ( #56190 ), #13605, .F. ) ;
#80233 = CARTESIAN_POINT ( 'NONE',  ( -5.924854902405000345, 1514.639648807489948, 216.8926256227769898 ) ) ;
#80234 = CARTESIAN_POINT ( 'NONE',  ( 16.09179317404203502, 1514.742486280438925, 194.1160285898321831 ) ) ;
#80235 = CARTESIAN_POINT ( 'NONE',  ( 15.34791040292138220, 1451.140134807847289, 149.4943114245902223 ) ) ;
#80236 = CARTESIAN_POINT ( 'NONE',  ( -7.769424639409999500, 1384.914898569509887, 218.9178468150989829 ) ) ;
#80238 = CARTESIAN_POINT ( 'NONE',  ( 10.90118902510000076, 1461.578585159090153, 210.3785431609790066 ) ) ;
#80237 = B_SPLINE_CURVE_WITH_KNOTS ( 'NONE', 5,
 ( #103271, #42288, #75893, #26011, #69166, #77556 ),
 .UNSPECIFIED., .F., .F.,
 ( 6, 6 ),
 ( 0.000000000000000000, 0.5082988451364722771 ),
 .UNSPECIFIED. ) ;
#80239 = EDGE_CURVE ( 'NONE', #108592, #21237, #48438, .T. ) ;
#80240 = CARTESIAN_POINT ( 'NONE',  ( -13.20210775350000176, 1379.610108467780037, 208.3538038533539805 ) ) ;
#80241 = CARTESIAN_POINT ( 'NONE',  ( -66.84334151430192605, 1379.743858467100608, 276.0920115519006686 ) ) ;
#80242 = CARTESIAN_POINT ( 'NONE',  ( 2.541857501799999586, 1464.337513799189992, 199.6147521953589887 ) ) ;
#80243 = CARTESIAN_POINT ( 'NONE',  ( 0.9304290756690000164, 1507.643508851029765, 237.2595324437979798 ) ) ;
#80244 = EDGE_CURVE ( 'NONE', #39044, #45555, #26396, .T. ) ;
#80245 = ORIENTED_EDGE ( 'NONE', *, *, #7727, .F. ) ;
#80246 = CARTESIAN_POINT ( 'NONE',  ( 7.321169230994999388, 1516.531533746980131, 207.4131249475269954 ) ) ;
#80247 = ORIENTED_EDGE ( 'NONE', *, *, #90605, .T. ) ;
#80248 = CARTESIAN_POINT ( 'NONE',  ( 29.36784481322840179, 1440.913060387330006, 250.7515280202720191 ) ) ;
#80249 = CARTESIAN_POINT ( 'NONE',  ( -15.09049181950000040, 1508.196604722230177, 184.9938367632979919 ) ) ;
#80250 = ORIENTED_EDGE ( 'NONE', *, *, #47520, .T. ) ;
#80251 = CARTESIAN_POINT ( 'NONE',  ( 27.43704247741250057, 1448.208574544649991, 136.8607721885420005 ) ) ;
#80252 = CARTESIAN_POINT ( 'NONE',  ( -14.90953803460000060, 1409.433712928330124, 191.8387206668980127 ) ) ;
#80253 = CARTESIAN_POINT ( 'NONE',  ( -17.96992599225091425, 1508.456902066601742, 211.9348791936326108 ) ) ;
#80254 = EDGE_CURVE ( 'NONE', #30516, #58921, #96098, .T. ) ;
#80256 = CARTESIAN_POINT ( 'NONE',  ( 14.92433369415259925, 1512.160613316490071, 196.7006824897309798 ) ) ;
#80255 = CARTESIAN_POINT ( 'NONE',  ( 8.269201957289999072, 1502.749105916489953, 209.6145118388120068 ) ) ;
#80257 = CARTESIAN_POINT ( 'NONE',  ( 22.50914366684990142, 1410.820172114669958, 206.2042648971080041 ) ) ;
#80258 = CARTESIAN_POINT ( 'NONE',  ( 18.80339018749999980, 1425.953307693130000, 225.0197311690980086 ) ) ;
#80259 = DIRECTION ( 'NONE',  ( 0.9989904502035610312, 0.04492303273871367519, 3.913620833796736061E-05 ) ) ;
#80260 = EDGE_CURVE ( 'NONE', #1077, #87539, #22774, .T. ) ;
#80261 = FACE_OUTER_BOUND ( 'NONE', #100613, .T. ) ;
#80262 = CARTESIAN_POINT ( 'NONE',  ( -15.13342374508840038, 1507.606285602760181, 191.8462590464540085 ) ) ;
#80264 = CARTESIAN_POINT ( 'NONE',  ( -103.8568841305003190, 1379.883889493366269, 304.0042906413861488 ) ) ;
#80263 = CARTESIAN_POINT ( 'NONE',  ( 15.72511249053680160, 1409.739245071985579, 192.0850589048065729 ) ) ;
#80265 = VECTOR ( 'NONE', #102348, 1000.000000000000114 ) ;
#80266 = CARTESIAN_POINT ( 'NONE',  ( 4.036748838804999906, 1516.667393516340098, 216.0582443258770127 ) ) ;
#80267 = AXIS2_PLACEMENT_3D ( 'NONE', #47008, #21754, #23432 ) ;
#80268 = EDGE_CURVE ( 'NONE', #64955, #47444, #49998, .T. ) ;
#80269 = CARTESIAN_POINT ( 'NONE',  ( -32.72607202732667275, 1524.152444737676660, 217.1332748866506108 ) ) ;
#80270 = CARTESIAN_POINT ( 'NONE',  ( 5.384056454772290223, 1511.434805660039956, 217.7741241935190146 ) ) ;
#80271 = VECTOR ( 'NONE', #60880, 1000.000000000000000 ) ;
#80272 = CARTESIAN_POINT ( 'NONE',  ( 17.82490373129249406, 1447.533498047817830, 216.9633381424519030 ) ) ;
#80273 = CARTESIAN_POINT ( 'NONE',  ( 2.299014030735000436, 1516.811292230880099, 211.9858893885470081 ) ) ;
#80274 = CARTESIAN_POINT ( 'NONE',  ( -11.53044373018859758, 1482.676277524829857, 206.1452238863429898 ) ) ;
#80275 = CARTESIAN_POINT ( 'NONE',  ( -2.825231993049800217, 1483.605131848210021, 198.8324855003439779 ) ) ;
#80277 = ORIENTED_EDGE ( 'NONE', *, *, #74664, .T. ) ;
#80276 = CARTESIAN_POINT ( 'NONE',  ( -106.7468999319999909, 1388.280083271419926, 298.2446700897589835 ) ) ;
#80278 = CARTESIAN_POINT ( 'NONE',  ( -16.58908872130532686, 1524.412455883367329, 237.5996433428405794 ) ) ;
#80279 = CARTESIAN_POINT ( 'NONE',  ( 25.42954105229999939, 1453.762068885830104, 238.1443982248979978 ) ) ;
#80280 = CARTESIAN_POINT ( 'NONE',  ( 30.79916350760332833, 1526.104292489136469, 217.1177548920526306 ) ) ;
#80281 = CARTESIAN_POINT ( 'NONE',  ( -25.78156655170059608, 1509.813372604039841, 223.1298223243570078 ) ) ;
#80282 = CARTESIAN_POINT ( 'NONE',  ( 1.983025529729999681, 1411.743863471630220, 232.0748871707980072 ) ) ;
#80283 = CARTESIAN_POINT ( 'NONE',  ( 16.89460221417492036, 1526.348417187221685, 183.3360764755736341 ) ) ;
#80285 = CARTESIAN_POINT ( 'NONE',  ( 2.500000000000000000, 1421.075716575930073, 150.9130928818979953 ) ) ;
#80284 = CARTESIAN_POINT ( 'NONE',  ( -18.89405915729999919, 1457.450104263030198, 227.0059657532979998 ) ) ;
#80286 = CARTESIAN_POINT ( 'NONE',  ( -0.08886200314649998766, 1488.812149332629815, 187.8711066492980137 ) ) ;
#80287 = CARTESIAN_POINT ( 'NONE',  ( -107.1583685770000045, 1380.648470457769918, 309.2260028292590164 ) ) ;
#80288 = AXIS2_PLACEMENT_3D ( 'NONE', #88897, #70477, #37953 ) ;
#80289 = EDGE_LOOP ( 'NONE', ( #86866, #43622, #8165, #32328, #9143 ) ) ;
#80290 = CARTESIAN_POINT ( 'NONE',  ( -5.010423001364999962, 1516.929569650079884, 205.0907035804270038 ) ) ;
#80291 = CARTESIAN_POINT ( 'NONE',  ( 1.757128879749999983, 1406.530468631129906, 269.4976381029979962 ) ) ;
#80292 = CARTESIAN_POINT ( 'NONE',  ( -1.081422847559999845, 1515.099766759590011, 213.4503789145389874 ) ) ;
#80293 = ADVANCED_FACE ( 'NONE', ( #25864 ), #25310, .T. ) ;
#80294 = CARTESIAN_POINT ( 'NONE',  ( 6.382104022434670121, 1471.436293962050058, 269.3346712093340329 ) ) ;
#80295 = EDGE_CURVE ( 'NONE', #62931, #91917, #40484, .T. ) ;
#80296 = CARTESIAN_POINT ( 'NONE',  ( -0.3263425942319403417, 1463.534437392499967, 199.3349841275349945 ) ) ;
#80297 = CARTESIAN_POINT ( 'NONE',  ( 21.10389824529999814, 1496.766845313890144, 207.9755595194390025 ) ) ;
#80298 = CARTESIAN_POINT ( 'NONE',  ( -20.06031067115785760, 1526.189899547014420, 233.0619662239967340 ) ) ;
#80299 = CARTESIAN_POINT ( 'NONE',  ( 3.238872246299508095, 1446.101400423860468, 200.2539368609401151 ) ) ;
#80300 = DIRECTION ( 'NONE',  ( 0.01484500363295476050, 0.5669078173070210003, -0.8236474686073690377 ) ) ;
#80301 = CARTESIAN_POINT ( 'NONE',  ( -15.89684887006662883, 1415.918796183675340, 209.5438883029932242 ) ) ;
#80302 = CARTESIAN_POINT ( 'NONE',  ( 2.039270112060000528, 1507.500700221690067, 220.6757736221989887 ) ) ;
#80303 = CARTESIAN_POINT ( 'NONE',  ( 18.16298593701623076, 1438.550562606129006, 191.5625238809707298 ) ) ;
#80304 = ORIENTED_EDGE ( 'NONE', *, *, #6359, .F. ) ;
#80305 = CARTESIAN_POINT ( 'NONE',  ( -34.97756117570000356, 1432.582706845480061, 262.6648722511980054 ) ) ;
#80306 = EDGE_CURVE ( 'NONE', #59255, #19757, #45598, .T. ) ;
#80307 = CARTESIAN_POINT ( 'NONE',  ( 5.652561691250400422, 1467.010946599490126, 199.8954101620430208 ) ) ;
#80308 = CARTESIAN_POINT ( 'NONE',  ( -0.5589788533730000175, 1476.074308366130026, 267.5370429008980295 ) ) ;
#80309 = CARTESIAN_POINT ( 'NONE',  ( -4.256948536952839923, 1446.548991557320051, 160.0047540042930052 ) ) ;
#80310 = CARTESIAN_POINT ( 'NONE',  ( -33.34040796508471516, 1523.342713519623203, 196.1259889609353877 ) ) ;
#80311 = CARTESIAN_POINT ( 'NONE',  ( -3.622779532894428556, 1448.291314561123500, 184.9376262326799463 ) ) ;
#80312 = CARTESIAN_POINT ( 'NONE',  ( -27.25125854287810157, 1384.838333352839982, 225.4489716181609822 ) ) ;
#80313 = CIRCLE ( 'NONE', #89255, 2.000000000000003553 ) ;
#80314 = B_SPLINE_SURFACE_WITH_KNOTS ( 'NONE', 5, 5, ( 
 ( #20484, #11566, #105635, #104516, #11014, #44628 ),
 ( #37320, #3193, #105072, #46299, #88820, #87736 ),
 ( #95564, #54694, #45185, #80427, #12106, #97212 ),
 ( #28921, #1519, #35652, #86606, #54144, #78769 ),
 ( #79879, #79326, #37872, #61995, #106172, #69842 ),
 ( #96679, #27814, #71516, #2637, #103960, #62559 ),
 ( #29452, #52478, #63648, #18284, #27257, #18834 ),
 ( #19951, #10454, #36213, #96113, #45742, #80970 ),
 ( #31111, #57451, #49042, #99404, #13185, #89371 ),
 ( #97763, #21591, #55796, #74247, #46842, #47374 ),
 ( #31660, #81499, #40068, #108378, #22682, #55238 ),
 ( #39522, #89912, #4801, #56881, #73697, #65840 ),
 ( #12663, #65291, #91011, #38946, #83178, #73126 ),
 ( #107268, #30563, #5362, #40618, #48491, #56327 ),
 ( #64753, #91578, #107823, #98864, #14301, #82630 ),
 ( #22129, #6468, #5922, #4275, #38405, #90460 ),
 ( #13737, #47921, #82057, #72581, #99958, #23252 ),
 ( #14851, #74789, #108931, #29999, #64190, #98312 ),
 ( #106709, #32220, #21035, #1815, #86890, #86338 ),
 ( #18019, #49589, #58540, #43792, #53316, #100520 ),
 ( #10753, #75347, #83721, #57990, #52212, #78504 ),
 ( #92124, #7566, #15400, #87460, #26995, #27541 ),
 ( #84271, #69577, #95845, #44924, #109487, #103695 ),
 ( #94739, #104251, #10185, #44359, #79071, #2376 ),
 ( #24354, #95302, #9623, #32764, #77942, #101056 ),
 ( #61185, #1249, #35952, #70138, #7016, #35389 ),
 ( #92666, #66401, #15943, #18562, #103123, #50144 ) ),
 .UNSPECIFIED., .F., .F., .F.,
 ( 6, 3, 3, 3, 3, 3, 3, 3, 6 ),
 ( 6, 6 ),
 ( 103.3477632230000012, 105.7451336970000000, 107.5792266200000000, 108.1425041709999988, 110.4591985809999954, 112.7758929910000063, 117.4092818109999996, 129.0014047420000054, 142.9189258060000043 ),
 ( 0.000000000000000000, 2.000000000000000000 ),
 .UNSPECIFIED. ) ;
#80315 = CARTESIAN_POINT ( 'NONE',  ( 12.22153682284019993, 1491.665661494050028, 207.6766598159610169 ) ) ;
#80316 = CARTESIAN_POINT ( 'NONE',  ( 11.87502392341400004, 1433.007271648830056, 149.9804723818110119 ) ) ;
#80317 = CARTESIAN_POINT ( 'NONE',  ( 26.46020439838580174, 1436.724525556780009, 136.8114229838039932 ) ) ;
#80318 = CARTESIAN_POINT ( 'NONE',  ( -5.519596238180829673, 1396.105808937369829, 218.6807260319289696 ) ) ;
#80319 = CARTESIAN_POINT ( 'NONE',  ( -14.89476520160000028, 1422.388268083329876, 228.7586242300979791 ) ) ;
#80320 = VECTOR ( 'NONE', #41594, 1000.000000000000000 ) ;
#80321 = EDGE_CURVE ( 'NONE', #44371, #8321, #75049, .T. ) ;
#80322 = CARTESIAN_POINT ( 'NONE',  ( 19.32723965911517183, 1455.838101669217849, 225.3662149856213830 ) ) ;
#80323 = CIRCLE ( 'NONE', #14122, 1.000000000039237946 ) ;
#80324 = VERTEX_POINT ( 'NONE', #51104 ) ;
#80325 = CARTESIAN_POINT ( 'NONE',  ( -11.37608146696432954, 1501.391524824338603, 207.8658177168534564 ) ) ;
#80326 = CARTESIAN_POINT ( 'NONE',  ( 0.8265245808140000427, 1408.941923261729926, 231.1644250952979860 ) ) ;
#80327 = CARTESIAN_POINT ( 'NONE',  ( -7.593205020690000140, 1511.472651697490164, 213.8751816602289750 ) ) ;
#80329 = CARTESIAN_POINT ( 'NONE',  ( -14.66019555306499988, 1513.841826332629807, 192.8214360263669960 ) ) ;
#80328 = CARTESIAN_POINT ( 'NONE',  ( 11.00743345139999896, 1426.053315483930191, 99.60275282069790137 ) ) ;
#80330 = DIRECTION ( 'NONE',  ( 1.835183309750130004E-16, 1.000000000000000000, 1.599799320660000123E-19 ) ) ;
#80331 = EDGE_CURVE ( 'NONE', #94948, #95283, #56407, .T. ) ;
#80332 = CARTESIAN_POINT ( 'NONE',  ( -12.45478753333599720, 1442.762691980110048, 205.2115877711401026 ) ) ;
#80333 = CARTESIAN_POINT ( 'NONE',  ( -3.454119954834999895, 1516.594591938570147, 201.4112355291069889 ) ) ;
#80334 = CARTESIAN_POINT ( 'NONE',  ( 7.768668303840000178, 1424.631498856950202, 211.9127687528989838 ) ) ;
#80335 = CARTESIAN_POINT ( 'NONE',  ( -12.04602610249999906, 1481.198043686990104, 227.9689298191989622 ) ) ;
#80336 = CARTESIAN_POINT ( 'NONE',  ( 3.395856411370000050, 1508.797082644030070, 180.5462404550980011 ) ) ;
#80337 = CARTESIAN_POINT ( 'NONE',  ( 7.625190025545000694, 1512.177707669779920, 206.5800331731570054 ) ) ;
#80338 = CARTESIAN_POINT ( 'NONE',  ( -70.83845563213419894, 1379.712669723569888, 285.7529926274859804 ) ) ;
#80339 = CIRCLE ( 'NONE', #19490, 1.000000000000000888 ) ;
#80340 = CARTESIAN_POINT ( 'NONE',  ( 4.501691961449999724, 1368.956319095359959, 207.6218459616989946 ) ) ;
#80342 = EDGE_LOOP ( 'NONE', ( #59461, #64003, #15332, #47305 ) ) ;
#80341 = CARTESIAN_POINT ( 'NONE',  ( -17.05938549526129577, 1517.051704405600049, 195.1949804090679947 ) ) ;
#80343 = ORIENTED_EDGE ( 'NONE', *, *, #70675, .T. ) ;
#80344 = DIRECTION ( 'NONE',  ( 0.000000000000000000, 0.000000000000000000, -1.000000000000000000 ) ) ;
#80345 = DIRECTION ( 'NONE',  ( 0.000000000000000000, 0.000000000000000000, 1.000000000000000000 ) ) ;
#80346 = CARTESIAN_POINT ( 'NONE',  ( -21.65324558190001980, 1435.253471290908919, 140.9571069649979904 ) ) ;
#80347 = CARTESIAN_POINT ( 'NONE',  ( -8.558300775104999758, 1511.397837225850026, 214.2288200170269761 ) ) ;
#80349 = CARTESIAN_POINT ( 'NONE',  ( -1.367322260308200255, 1418.654931759450164, 185.2513577252690311 ) ) ;
#80348 = CARTESIAN_POINT ( 'NONE',  ( -7.540598407700000116, 1384.733204023860026, 219.0853623458990000 ) ) ;
#80350 = CARTESIAN_POINT ( 'NONE',  ( 1.657366258489999966, 1410.306738087430176, 185.3518365496979925 ) ) ;
#80351 = EDGE_CURVE ( 'NONE', #105626, #66063, #74698, .T. ) ;
#80352 = CARTESIAN_POINT ( 'NONE',  ( -1.551136391885070021, 1463.265703726430047, 199.4650954087569801 ) ) ;
#80353 = CARTESIAN_POINT ( 'NONE',  ( -40.23885053629599895, 1448.346527775979894, 135.0415120907709934 ) ) ;
#80354 =( LENGTH_UNIT ( ) NAMED_UNIT ( * ) SI_UNIT ( .MILLI., .METRE. ) );
#80355 = CARTESIAN_POINT ( 'NONE',  ( -2.500000000000000000, 1448.216394621219933, 167.2095406785390139 ) ) ;
#80356 = DIRECTION ( 'NONE',  ( -0.000000000000000000, -1.000000000000000000, -0.000000000000000000 ) ) ;
#80357 = CARTESIAN_POINT ( 'NONE',  ( 12.33128373348028184, 1390.939237335599955, 208.6028876581396503 ) ) ;
#80358 = CARTESIAN_POINT ( 'NONE',  ( -5.320809690189729935, 1406.488740053329821, 269.2842400656589916 ) ) ;
#80359 = CARTESIAN_POINT ( 'NONE',  ( -19.00254521766261107, 1416.818673809775419, 207.9334427874379116 ) ) ;
#80360 = ORIENTED_EDGE ( 'NONE', *, *, #52198, .T. ) ;
#80361 = CARTESIAN_POINT ( 'NONE',  ( -16.81049281788192218, 1526.143142182265819, 182.6472226615217380 ) ) ;
#80362 = CARTESIAN_POINT ( 'NONE',  ( 21.83181799873717566, 1524.739563915921508, 233.6212106848500412 ) ) ;
#80363 = ORIENTED_EDGE ( 'NONE', *, *, #63184, .T. ) ;
#80364 = VERTEX_POINT ( 'NONE', #24754 ) ;
#80365 = EDGE_CURVE ( 'NONE', #101100, #42035, #76853, .T. ) ;
#80366 = CARTESIAN_POINT ( 'NONE',  ( -3.201475593029999622, 1454.788669051489933, 199.8827623000489666 ) ) ;
#80367 = CARTESIAN_POINT ( 'NONE',  ( 9.704582620010000937, 1366.001145740639913, 207.6218459616989946 ) ) ;
#80368 = AXIS2_PLACEMENT_3D ( 'NONE', #75181, #61008, #44190 ) ;
#80369 = CARTESIAN_POINT ( 'NONE',  ( 2.874588922665000545, 1516.606339319019980, 215.6687976528169770 ) ) ;
#80370 = CARTESIAN_POINT ( 'NONE',  ( 3.432975284724999909, 1511.645462744430006, 217.1388420280169953 ) ) ;
#80371 = EDGE_CURVE ( 'NONE', #23739, #85422, #69432, .T. ) ;
#80372 = ORIENTED_EDGE ( 'NONE', *, *, #57648, .T. ) ;
#80373 = CARTESIAN_POINT ( 'NONE',  ( 0.5624690339869999889, 1416.828040475229955, 190.4759594386979984 ) ) ;
#80374 = CARTESIAN_POINT ( 'NONE',  ( -101.8495347479999964, 1374.485289779690220, 303.2301490391590164 ) ) ;
#80375 = CARTESIAN_POINT ( 'NONE',  ( 0.3443454750360000483, 1415.932840167130053, 226.9638901923979972 ) ) ;
#80376 = CARTESIAN_POINT ( 'NONE',  ( 0.7365611785030020675, 1517.066898074209803, 204.4979538714769944 ) ) ;
#80377 = AXIS2_PLACEMENT_3D ( 'NONE', #85528, #17199, #49760 ) ;
#80378 = DIRECTION ( 'NONE',  ( -0.6736849260149578855, 0.000000000000000000, 0.7390186874905266823 ) ) ;
#80379 = CARTESIAN_POINT ( 'NONE',  ( -98.86936394900000380, 1384.986782500260006, 296.2451545551589902 ) ) ;
#80380 = CARTESIAN_POINT ( 'NONE',  ( -3.314356077729999406, 1409.028800251930079, 230.9273595247980211 ) ) ;
#80381 = ORIENTED_EDGE ( 'NONE', *, *, #78085, .T. ) ;
#80382 = EDGE_CURVE ( 'NONE', #8790, #24414, #72939, .T. ) ;
#80383 = DIRECTION ( 'NONE',  ( 5.980589973904019347E-17, -1.000000000000000000, 1.736889445713099699E-16 ) ) ;
#80384 = CARTESIAN_POINT ( 'NONE',  ( -24.67970723617740347, 1440.913060461539771, 213.9247834336929941 ) ) ;
#80385 = CARTESIAN_POINT ( 'NONE',  ( 20.32791520299490173, 1497.608840033019987, 226.4479123882990166 ) ) ;
#80386 = CARTESIAN_POINT ( 'NONE',  ( 15.68254779764047235, 1506.474306118306004, 224.5749311187954902 ) ) ;
#80387 = CARTESIAN_POINT ( 'NONE',  ( 20.94370973160000204, 1411.258104562529979, 270.0430967323979417 ) ) ;
#80388 = ADVANCED_FACE ( 'NONE', ( #1820 ), #9627, .F. ) ;
#80389 = CARTESIAN_POINT ( 'NONE',  ( -7.710285875814999912, 1516.582197289609894, 212.3822242253069987 ) ) ;
#80390 = AXIS2_PLACEMENT_3D ( 'NONE', #104786, #3450, #71781 ) ;
#80391 = CARTESIAN_POINT ( 'NONE',  ( -65.41912593600000037, 1379.740434417399683, 273.1837229148590609 ) ) ;
#80392 = CARTESIAN_POINT ( 'NONE',  ( 23.96253434680000183, 1410.844299666830011, 208.4004183790169975 ) ) ;
#80393 = CARTESIAN_POINT ( 'NONE',  ( 0.01990864597794416921, 1507.260534525954881, 237.3641690013145649 ) ) ;
#80394 = CARTESIAN_POINT ( 'NONE',  ( 14.53924085489259888, 1427.225259935240274, 198.3454325463169994 ) ) ;
#80395 = CARTESIAN_POINT ( 'NONE',  ( 19.20874097899815780, 1410.945473914794547, 195.6776540737980383 ) ) ;
#80396 = CARTESIAN_POINT ( 'NONE',  ( 6.562094069294999166, 1517.122674412569950, 209.8604508749069737 ) ) ;
#80397 = ORIENTED_EDGE ( 'NONE', *, *, #57560, .F. ) ;
#80398 = CARTESIAN_POINT ( 'NONE',  ( 22.53878404599999641, 1411.058442739730026, 206.1986151668880041 ) ) ;
#80399 = CARTESIAN_POINT ( 'NONE',  ( -8.447610866089998893, 1417.903240752429838, 230.8139735681979801 ) ) ;
#80400 = CARTESIAN_POINT ( 'NONE',  ( -89.65362972180000156, 1384.619809472219913, 308.7387643915590161 ) ) ;
#80401 = ORIENTED_EDGE ( 'NONE', *, *, #4893, .F. ) ;
#80402 = CARTESIAN_POINT ( 'NONE',  ( -24.85901358151489760, 1385.256427123100138, 223.5815164292420150 ) ) ;
#80403 = AXIS2_PLACEMENT_3D ( 'NONE', #73854, #48659, #74414 ) ;
#80404 = CARTESIAN_POINT ( 'NONE',  ( -2.805169331900000174, 1430.372835222990034, 201.2596692449290003 ) ) ;
#80405 = CARTESIAN_POINT ( 'NONE',  ( -2.847678236428970333, 1430.845636561999981, 201.2564352187889938 ) ) ;
#80406 = AXIS2_PLACEMENT_3D ( 'NONE', #53350, #3504, #10782 ) ;
#80407 = CYLINDRICAL_SURFACE ( 'NONE', #83099, 2.000000000000007550 ) ;
#80408 = CARTESIAN_POINT ( 'NONE',  ( -0.3331897858350000297, 1408.924695719030069, 232.1910296785979995 ) ) ;
#80409 = CARTESIAN_POINT ( 'NONE',  ( -0.1423985958509380034, 1420.464637908429950, 182.7409013480950080 ) ) ;
#80410 = B_SPLINE_CURVE_WITH_KNOTS ( 'NONE', 5,
 ( #20190, #26387, #54388, #88521, #94703, #9588 ),
 .UNSPECIFIED., .F., .F.,
 ( 6, 6 ),
 ( 0.000000000000000000, 1.000000000000000000 ),
 .UNSPECIFIED. ) ;
#80412 = FACE_OUTER_BOUND ( 'NONE', #21403, .T. ) ;
#80411 = CARTESIAN_POINT ( 'NONE',  ( -4.613762395014999740, 1516.939574742129935, 214.9064842900469898 ) ) ;
#80413 = CARTESIAN_POINT ( 'NONE',  ( 10.04317674107989156, 1459.686705906630550, 204.8127587888380958 ) ) ;
#80414 = CARTESIAN_POINT ( 'NONE',  ( 10.34497362454819935, 1469.890123644820051, 207.2997660916290101 ) ) ;
#80415 = ORIENTED_EDGE ( 'NONE', *, *, #27617, .F. ) ;
#80416 = CARTESIAN_POINT ( 'NONE',  ( 0.7391219670640019057, 1517.130100026000036, 202.1721425974470208 ) ) ;
#80417 = CARTESIAN_POINT ( 'NONE',  ( 10.02421119480000122, 1480.534221758890226, 205.8829018067289951 ) ) ;
#80418 = EDGE_LOOP ( 'NONE', ( #84104, #26042, #97042, #22362 ) ) ;
#80419 = CIRCLE ( 'NONE', #64285, 1.000000000000000888 ) ;
#80420 = CARTESIAN_POINT ( 'NONE',  ( 4.369470536992099419, 1486.409411101999922, 202.3252857625509762 ) ) ;
#80421 = CARTESIAN_POINT ( 'NONE',  ( -1.729960644012338955, 1451.871857846600051, 184.1618444272322108 ) ) ;
#80422 = CARTESIAN_POINT ( 'NONE',  ( 8.639302646193000257, 1511.681069547209972, 203.0735539262880138 ) ) ;
#80423 = PRODUCT_DEFINITION_CONTEXT ( 'detailed design', #39875, 'design' ) ;
#80424 = CARTESIAN_POINT ( 'NONE',  ( -0.3697322172690010178, 1443.791874737389890, 218.1763052592289966 ) ) ;
#80425 = CARTESIAN_POINT ( 'NONE',  ( -26.53762114791049598, 1508.774119630419818, 201.4667103074619945 ) ) ;
#80426 = CARTESIAN_POINT ( 'NONE',  ( 14.46805569519750101, 1471.430981385289897, 194.8600923975780006 ) ) ;
#80427 = CARTESIAN_POINT ( 'NONE',  ( -17.95690667590000089, 1424.708104102629932, 226.6788193228979935 ) ) ;
#80428 = CARTESIAN_POINT ( 'NONE',  ( -14.28308187130000029, 1434.994876553209906, 148.2389740282980028 ) ) ;
#80429 = CARTESIAN_POINT ( 'NONE',  ( -2.301610763810779670, 1464.951938263800002, 198.3549737183319905 ) ) ;
#80430 = CARTESIAN_POINT ( 'NONE',  ( 19.30519085950000147, 1478.522678847230054, 190.2770777040979908 ) ) ;
#80432 = CARTESIAN_POINT ( 'NONE',  ( 28.45309226149999660, 1509.159855970130138, 209.4524995968540111 ) ) ;
#80431 = CARTESIAN_POINT ( 'NONE',  ( 4.989613516749999533, 1487.671035670790161, 198.1975016566989893 ) ) ;
#80433 = CARTESIAN_POINT ( 'NONE',  ( -10.08152180407089915, 1472.386940315740048, 210.5255569266109887 ) ) ;
#80434 = EDGE_LOOP ( 'NONE', ( #26298, #93429, #62205, #22158 ) ) ;
#80435 = CARTESIAN_POINT ( 'NONE',  ( -103.5847285859999971, 1379.882004272549921, 303.6035322816589996 ) ) ;
#80436 = CARTESIAN_POINT ( 'NONE',  ( -15.33800405639999909, 1508.551704408389924, 214.6490336124689975 ) ) ;
#80437 = CARTESIAN_POINT ( 'NONE',  ( -45.51398236499812811, 1438.090180991398029, 268.9782812080896974 ) ) ;
#80438 = CARTESIAN_POINT ( 'NONE',  ( -24.02573159490000165, 1437.659110011540179, 211.8884722500880002 ) ) ;
#80439 = DIRECTION ( 'NONE',  ( 1.000000000000000000, 0.000000000000000000, 0.000000000000000000 ) ) ;
#80440 = CIRCLE ( 'NONE', #62573, 1.000000000000077494 ) ;
#80441 = CARTESIAN_POINT ( 'NONE',  ( -18.46438761779999993, 1509.557851011129969, 231.7133587053980079 ) ) ;
#80442 = CARTESIAN_POINT ( 'NONE',  ( -3.237065521149570912, 1524.843416604498543, 241.7215981950958223 ) ) ;
#80443 = CARTESIAN_POINT ( 'NONE',  ( 20.26030320659999617, 1497.713060387329961, 217.9272749506380080 ) ) ;
#80444 = B_SPLINE_SURFACE_WITH_KNOTS ( 'NONE', 5, 1, ( 
 ( #26333, #68379 ),
 ( #35864, #60528 ),
 ( #68935, #1726 ),
 ( #94091, #104160 ),
 ( #77860, #50469 ),
 ( #76205, #17362 ),
 ( #7884, #8991 ),
 ( #27446, #78413 ),
 ( #92991, #103608 ) ),
 .UNSPECIFIED., .F., .F., .F.,
 ( 6, 3, 6 ),
 ( 2, 2 ),
 ( -5.179891626739999739E-09, 44.04929316810000017, 84.36259054890000186 ),
 ( 2.018291184700000240, 3.029415486610000041 ),
 .UNSPECIFIED. ) ;
#80445 = CARTESIAN_POINT ( 'NONE',  ( -16.81223226430000039, 1414.913060387329779, 207.5743821216680089 ) ) ;
#80446 = CARTESIAN_POINT ( 'NONE',  ( -1.419022340012153993, 1507.123642348895146, 237.1495897167226587 ) ) ;
#80447 = CARTESIAN_POINT ( 'NONE',  ( -10.22681497006489870, 1488.677241974470007, 215.7752924027969925 ) ) ;
#80448 = CARTESIAN_POINT ( 'NONE',  ( -18.32377916267250129, 1464.077737519419998, 217.4721398674979866 ) ) ;
#80449 = CARTESIAN_POINT ( 'NONE',  ( -83.79005405282170216, 1383.774350621089980, 305.8889031002050274 ) ) ;
#80450 = CARTESIAN_POINT ( 'NONE',  ( -109.8447538101560070, 1383.797388995159963, 311.3561482245430057 ) ) ;
#80451 = CARTESIAN_POINT ( 'NONE',  ( -0.2489082263676290208, 1516.862251239930174, 201.4042270512659911 ) ) ;
#80453 = VERTEX_POINT ( 'NONE', #10189 ) ;
#80452 = DIRECTION ( 'NONE',  ( 0.9455185755993178454, 0.000000000000000000, -0.3255681544571537578 ) ) ;
#80454 = AXIS2_PLACEMENT_3D ( 'NONE', #31282, #31834, #90631 ) ;
#80455 = CARTESIAN_POINT ( 'NONE',  ( -96.58293600380000044, 1381.030388059910138, 308.7257624848589899 ) ) ;
#80456 = CARTESIAN_POINT ( 'NONE',  ( -16.50400130224731754, 1525.907212628473644, 236.2546788475584094 ) ) ;
#80457 = ORIENTED_EDGE ( 'NONE', *, *, #87210, .T. ) ;
#80458 = ORIENTED_EDGE ( 'NONE', *, *, #110361, .T. ) ;
#80459 = CARTESIAN_POINT ( 'NONE',  ( -20.70043371970000123, 1486.933533050689903, 208.1069901901390153 ) ) ;
#80460 = CARTESIAN_POINT ( 'NONE',  ( -109.5358690449999983, 1384.943159195940098, 297.1231912513590032 ) ) ;
#80461 = CARTESIAN_POINT ( 'NONE',  ( 12.55167427646019718, 1442.776442884412745, 169.4734868725398371 ) ) ;
#80463 = CARTESIAN_POINT ( 'NONE',  ( -33.33289073529999769, 1445.199364517940012, 248.0947902359980048 ) ) ;
#80462 = CARTESIAN_POINT ( 'NONE',  ( 29.83023163778732467, 1419.452610179523845, 269.4690072239820324 ) ) ;
#80464 = CARTESIAN_POINT ( 'NONE',  ( -19.29261533819999741, 1484.706083574029890, 189.6393559541980096 ) ) ;
#80465 = CARTESIAN_POINT ( 'NONE',  ( -11.58371378220000025, 1433.785063954710040, 151.2033516465980085 ) ) ;
#80466 = CARTESIAN_POINT ( 'NONE',  ( 26.23319076840000008, 1508.580492117430140, 201.9768647809279969 ) ) ;
#80467 = CARTESIAN_POINT ( 'NONE',  ( -19.46358587980000365, 1485.590242327929900, 189.9720724388979818 ) ) ;
#80468 = CARTESIAN_POINT ( 'NONE',  ( 8.359567452010001176, 1410.137012574430173, 187.7727004011979659 ) ) ;
#80469 = CARTESIAN_POINT ( 'NONE',  ( 4.976421422960000562, 1422.135394151030141, 185.3303333604980025 ) ) ;
#80470 = CARTESIAN_POINT ( 'NONE',  ( -0.08387812424052221161, 1515.158224561690076, 213.4488481431200171 ) ) ;
#80471 = CARTESIAN_POINT ( 'NONE',  ( -107.2899050854710055, 1379.886892357829993, 309.1794776302379546 ) ) ;
#80472 = CARTESIAN_POINT ( 'NONE',  ( 13.08769715623770047, 1428.580231863860035, 223.4460403848140118 ) ) ;
#80473 = CARTESIAN_POINT ( 'NONE',  ( 33.28034951413927445, 1522.382868172863937, 200.8029765415137717 ) ) ;
#80475 = ORIENTED_EDGE ( 'NONE', *, *, #34318, .F. ) ;
#80474 = CARTESIAN_POINT ( 'NONE',  ( 1.099242448648459977E-08, 1409.143622018159931, 260.5448422644799962 ) ) ;
#80476 = ORIENTED_EDGE ( 'NONE', *, *, #40810, .F. ) ;
#80477 = CARTESIAN_POINT ( 'NONE',  ( -11.86456335612260027, 1432.228581043409804, 149.9813182647349947 ) ) ;
#80478 = CARTESIAN_POINT ( 'NONE',  ( -12.04603955804210003, 1481.197944389760096, 227.9689156426159684 ) ) ;
#80479 = CARTESIAN_POINT ( 'NONE',  ( -10.57863510019999964, 1471.118849071129944, 270.0764144472979638 ) ) ;
#80480 = CARTESIAN_POINT ( 'NONE',  ( 7.468327728180000236, 1422.304606718539844, 195.6660984653989885 ) ) ;
#80481 =( BOUNDED_CURVE ( )  B_SPLINE_CURVE ( 3, ( #3123, #98245, #80359, #12597 ),
 .UNSPECIFIED., .F., .F. ) 
 B_SPLINE_CURVE_WITH_KNOTS ( ( 4, 4 ),
 ( 1.036305842674305921, 2.105309002732549839 ),
 .UNSPECIFIED. ) 
 CURVE ( )  GEOMETRIC_REPRESENTATION_ITEM ( )  RATIONAL_B_SPLINE_CURVE ( ( 1.000000000000000000, 0.9070150915768222522, 0.9070150915768222522, 1.000000000000000000 ) ) 
 REPRESENTATION_ITEM ( '' )  );
#80482 = FACE_OUTER_BOUND ( 'NONE', #9725, .T. ) ;
#80483 = DIRECTION ( 'NONE',  ( -0.6736849260863839728, 0.000000000000000000, 0.7390186874254150995 ) ) ;
#80484 = EDGE_CURVE ( 'NONE', #19775, #67049, #49666, .T. ) ;
#80485 = CARTESIAN_POINT ( 'NONE',  ( 0.3570880529365150213, 1450.920097230550027, 181.5564549562909917 ) ) ;
#80486 = EDGE_CURVE ( 'NONE', #109427, #20723, #11312, .T. ) ;
#80487 = CARTESIAN_POINT ( 'NONE',  ( 11.20854089337319870, 1414.996442620860080, 222.5314268542019818 ) ) ;
#80488 = CARTESIAN_POINT ( 'NONE',  ( -29.74901212038058418, 1525.343727714918259, 222.0046262735807829 ) ) ;
#80489 = CARTESIAN_POINT ( 'NONE',  ( -9.519358615130000700, 1460.477013596890174, 210.7621351733390043 ) ) ;
#80490 = B_SPLINE_CURVE_WITH_KNOTS ( 'NONE', 5,
 ( #12064, #54106, #20995, #54654, #2041, #88784 ),
 .UNSPECIFIED., .F., .F.,
 ( 6, 6 ),
 ( -87.06999293180000166, -29.77037674149489987 ),
 .UNSPECIFIED. ) ;
#80491 = CARTESIAN_POINT ( 'NONE',  ( 9.995873456701064086, 1362.519969852305167, 207.6218459616987673 ) ) ;
#80492 = CARTESIAN_POINT ( 'NONE',  ( -45.36837539640040262, 1437.179215847679870, 268.9823049396750321 ) ) ;
#80493 = AXIS2_PLACEMENT_3D ( 'NONE', #36846, #71038, #12747 ) ;
#80494 = VERTEX_POINT ( 'NONE', #28652 ) ;
#80495 = CARTESIAN_POINT ( 'NONE',  ( -3.536362979286669983, 1494.571137096670100, 181.5117196762699905 ) ) ;
#80496 = ORIENTED_EDGE ( 'NONE', *, *, #2116, .F. ) ;
#80497 = ORIENTED_EDGE ( 'NONE', *, *, #52118, .T. ) ;
#80498 = CARTESIAN_POINT ( 'NONE',  ( -0.7352271553329990939, 1516.963431999339946, 210.8369554172870153 ) ) ;
#80499 = DIRECTION ( 'NONE',  ( 0.9510565162951478690, 0.000000000000000000, -0.3090169943749654369 ) ) ;
#80500 = CARTESIAN_POINT ( 'NONE',  ( 17.31001952156929491, 1410.038354363751978, 224.8086568639813834 ) ) ;
#80501 = CARTESIAN_POINT ( 'NONE',  ( -4.111558752199999667, 1410.393682478630126, 186.7772447052980169 ) ) ;
#80502 = VECTOR ( 'NONE', #20559, 1000.000000000000000 ) ;
#80503 = B_SPLINE_CURVE_WITH_KNOTS ( 'NONE', 5,
 ( #46586, #105375, #71814, #86909, #54445, #46035 ),
 .UNSPECIFIED., .F., .F.,
 ( 6, 6 ),
 ( 0.000000000000000000, 1.000000000000000000 ),
 .UNSPECIFIED. ) ;
#80504 = EDGE_CURVE ( 'NONE', #102730, #7200, #41718, .T. ) ;
#80505 = CARTESIAN_POINT ( 'NONE',  ( -0.7302202251785760989, 1496.394952593959943, 221.4547034809050103 ) ) ;
#80506 = ORIENTED_EDGE ( 'NONE', *, *, #11073, .F. ) ;
#80507 = CARTESIAN_POINT ( 'NONE',  ( -7.329925260535000042, 1516.833976295079992, 201.4049670291269933 ) ) ;
#80508 = CARTESIAN_POINT ( 'NONE',  ( 3.118627138969999990, 1507.020746158230168, 237.9289388427980043 ) ) ;
#80509 = CARTESIAN_POINT ( 'NONE',  ( -9.602934085884299975, 1440.348741234980025, 206.2393590046850136 ) ) ;
#80510 = VERTEX_POINT ( 'NONE', #86343 ) ;
#80511 = CARTESIAN_POINT ( 'NONE',  ( -9.504797446096199920, 1411.012292308769702, 269.6245613120399867 ) ) ;
#80512 = CARTESIAN_POINT ( 'NONE',  ( 3.043140677541010142, 1417.779445265420009, 234.3218410894589852 ) ) ;
#80513 = CARTESIAN_POINT ( 'NONE',  ( 8.701161615177460007, 1436.141447764929808, 208.2918654964580014 ) ) ;
#80515 = ORIENTED_EDGE ( 'NONE', *, *, #71499, .T. ) ;
#80514 = CARTESIAN_POINT ( 'NONE',  ( -8.048119939141594514, 1365.119509101891254, 208.3718459617061285 ) ) ;
#80516 = EDGE_LOOP ( 'NONE', ( #27204, #63212, #3732, #91814 ) ) ;
#80517 = CARTESIAN_POINT ( 'NONE',  ( 45.33376732508579465, 1444.887998074412053, 268.9831579371490307 ) ) ;
#80518 = CARTESIAN_POINT ( 'NONE',  ( 2.609390164300539716, 1466.696228754160074, 219.8662591647770057 ) ) ;
#80519 = CARTESIAN_POINT ( 'NONE',  ( -14.02058551345489867, 1436.245318346960175, 150.2233960230930165 ) ) ;
#80520 = AXIS2_PLACEMENT_3D ( 'NONE', #73823, #23927, #73259 ) ;
#80521 = CARTESIAN_POINT ( 'NONE',  ( -0.03713005249742180186, 1409.802211749629805, 185.1324229550240261 ) ) ;
#80522 = EDGE_CURVE ( 'NONE', #42444, #88474, #5498, .T. ) ;
#80523 = CARTESIAN_POINT ( 'NONE',  ( -18.53331733233340017, 1415.778512717889953, 207.5702610487440154 ) ) ;
#80524 = CARTESIAN_POINT ( 'NONE',  ( 5.388168580889999504, 1432.635621093390000, 154.6140392605979912 ) ) ;
#80525 = CARTESIAN_POINT ( 'NONE',  ( -0.0001223106876275270073, 1475.759747512889817, 269.0458114371340343 ) ) ;
#80526 = CARTESIAN_POINT ( 'NONE',  ( 11.58478124470000026, 1415.063410489829948, 222.3466023727980030 ) ) ;
#80527 = CARTESIAN_POINT ( 'NONE',  ( 5.538520585190000567, 1447.740028701229903, 184.7993824163979752 ) ) ;
#80528 = CARTESIAN_POINT ( 'NONE',  ( -0.7576635715699989726, 1516.855632454399938, 206.2537338009369989 ) ) ;
#80529 = ADVANCED_FACE ( 'NONE', ( #54434 ), #76884, .F. ) ;
#80530 = VERTEX_POINT ( 'NONE', #102445 ) ;
#80531 = FACE_OUTER_BOUND ( 'NONE', #16102, .T. ) ;
#80532 = CARTESIAN_POINT ( 'NONE',  ( -21.56756540081639173, 1453.725795844561617, 221.9610449306620126 ) ) ;
#80533 = ORIENTED_EDGE ( 'NONE', *, *, #93180, .F. ) ;
#80535 = CIRCLE ( 'NONE', #32245, 2.000000000000003553 ) ;
#80534 = CARTESIAN_POINT ( 'NONE',  ( 13.42479616400980014, 1453.338203267170002, 224.7140346886050111 ) ) ;
#80536 = CARTESIAN_POINT ( 'NONE',  ( 24.72977296794550028, 1451.893578074279958, 136.8099502904200051 ) ) ;
#80537 = CARTESIAN_POINT ( 'NONE',  ( 10.85845406881951192, 1424.793774302243946, 138.1921923613813590 ) ) ;
#80538 = LINE ( 'NONE', #4386, #71795 ) ;
#80539 = CARTESIAN_POINT ( 'NONE',  ( 20.08164004260000013, 1410.974782856229922, 197.5376054386979945 ) ) ;
#80540 = CARTESIAN_POINT ( 'NONE',  ( 22.50660266490000083, 1409.865199449729971, 207.4947920653180233 ) ) ;
#80541 = CARTESIAN_POINT ( 'NONE',  ( -24.25923418980000079, 1435.344651399380155, 136.2870029874980276 ) ) ;
#80542 = CARTESIAN_POINT ( 'NONE',  ( 10.93233376569999926, 1490.536113732890044, 207.1036721549689901 ) ) ;
#80543 = CARTESIAN_POINT ( 'NONE',  ( 0.8365135405962150772, 1450.872666035589873, 181.3727942470009680 ) ) ;
#80544 = CARTESIAN_POINT ( 'NONE',  ( 2.500000000000000000, 1439.611175471030037, 167.3041001658060054 ) ) ;
#80545 = CARTESIAN_POINT ( 'NONE',  ( 2.292940169014999974, 1516.565291103010168, 215.6678853655270132 ) ) ;
#80546 = DIRECTION ( 'NONE',  ( -1.755985294532469921E-16, 1.000000000000000000, -1.338183447452831989E-16 ) ) ;
#80547 = ORIENTED_EDGE ( 'NONE', *, *, #38495, .T. ) ;
#80548 = CARTESIAN_POINT ( 'NONE',  ( -17.25861218780000073, 1417.514782456119974, 207.1361538078189994 ) ) ;
#80549 = CARTESIAN_POINT ( 'NONE',  ( 4.363122647530000009, 1409.354802298930053, 121.6099336315979969 ) ) ;
#80550 = CARTESIAN_POINT ( 'NONE',  ( 11072.05219664940523, 50.13405481578727318, -8413.031381323531605 ) ) ;
#80551 = CARTESIAN_POINT ( 'NONE',  ( -39.28604983332469658, 1447.310147778509872, 136.5961217192789832 ) ) ;
#80552 = CARTESIAN_POINT ( 'NONE',  ( 18.87853829029999986, 1458.344553362990155, 213.8102309971890236 ) ) ;
#80553 = DIRECTION ( 'NONE',  ( 0.9858563016923833633, 0.000000000000000000, 0.1675928173085483863 ) ) ;
#80554 = VECTOR ( 'NONE', #63203, 1000.000000000000000 ) ;
#80555 = CARTESIAN_POINT ( 'NONE',  ( -2.375604933953470166, 1484.258301715329935, 183.2084465395040240 ) ) ;
#80556 = CARTESIAN_POINT ( 'NONE',  ( 11.58906603029999971, 1433.009685293250186, 151.1019960182979958 ) ) ;
#80557 = LINE ( 'NONE', #2770, #14666 ) ;
#80558 = B_SPLINE_SURFACE_WITH_KNOTS ( 'NONE', 5, 5, ( 
 ( #46356, #80489, #70457, #28425, #78838, #87798 ),
 ( #45249, #104578, #96742, #54752, #27314, #105701 ),
 ( #53089, #97275, #63171, #53653, #105135, #71014 ),
 ( #11625, #88882, #37937, #12166, #9962, #61495 ),
 ( #95625, #54208, #10517, #44691, #27873, #11082 ),
 ( #79936, #62054, #2699, #45803, #36824, #3252 ),
 ( #37379, #48548, #47438, #5423, #106770, #4337 ),
 ( #21647, #98375, #55855, #81562, #98922, #22192 ),
 ( #39581, #82685, #100020, #91073, #83232, #73185 ),
 ( #56390, #14906, #73753, #55299, #4865, #89974 ),
 ( #31716, #90522, #56944, #30626, #64814, #66463 ),
 ( #13248, #65902, #23312, #13798, #107876, #31164 ),
 ( #14356, #74305, #49097, #57505, #6523, #100572 ),
 ( #40675, #65354, #30061, #74849, #39008, #47984 ),
 ( #5975, #38468, #91630, #40120, #82121, #107330 ) ),
 .UNSPECIFIED., .F., .F., .F.,
 ( 6, 3, 3, 3, 6 ),
 ( 6, 6 ),
 ( 13.48959176149999983, 23.65970578370000155, 28.35476274839999888, 30.70229123080000022, 33.04981971320000156 ),
 ( 0.000000000000000000, 2.000000000000000000 ),
 .UNSPECIFIED. ) ;
#80559 = DIRECTION ( 'NONE',  ( -0.06270903725022231034, 1.833354768615425389E-16, 0.9980318515193542517 ) ) ;
#80560 = CARTESIAN_POINT ( 'NONE',  ( -109.8984563230000049, 1385.013959313279884, 297.0294149341589787 ) ) ;
#80561 = CARTESIAN_POINT ( 'NONE',  ( -31.63976464710271941, 1525.343727714918259, 202.0582035741803679 ) ) ;
#80562 = ORIENTED_EDGE ( 'NONE', *, *, #23436, .T. ) ;
#80563 = CARTESIAN_POINT ( 'NONE',  ( 11.23388613411650638, 1442.762691980111640, 150.9272215568491049 ) ) ;
#80564 = CARTESIAN_POINT ( 'NONE',  ( -19.22829456215601240, 1485.595672753383042, 189.7356968105359840 ) ) ;
#80565 = CARTESIAN_POINT ( 'NONE',  ( -2.390047989675008644, 1526.069472839384844, 240.5369618407216024 ) ) ;
#80566 = DIRECTION ( 'NONE',  ( 0.1403878024439506045, 0.9900965937346509760, 0.000000000000000000 ) ) ;
#80567 = AXIS2_PLACEMENT_3D ( 'NONE', #2158, #70465, #62062 ) ;
#80568 = CARTESIAN_POINT ( 'NONE',  ( -16.89460221416782915, 1526.348417187221685, 234.9076154478163687 ) ) ;
#80569 = CARTESIAN_POINT ( 'NONE',  ( -10.16988517760000121, 1507.385799736029867, 234.4102472725979851 ) ) ;
#80570 = CARTESIAN_POINT ( 'NONE',  ( -25.20965598612449909, 1383.847833833380037, 223.6406741977980062 ) ) ;
#80571 = CARTESIAN_POINT ( 'NONE',  ( -18.80014180510890043, 1505.319237130929878, 222.5373109737209916 ) ) ;
#80572 = CARTESIAN_POINT ( 'NONE',  ( 6.244762013140000789, 1407.784308382130121, 220.5925233730980040 ) ) ;
#80573 = DIRECTION ( 'NONE',  ( 1.755985294532469921E-16, -1.000000000000000000, 1.338183447452831989E-16 ) ) ;
#80574 = CARTESIAN_POINT ( 'NONE',  ( 1.679567668810000081, 1466.272168333229956, 234.7591022376979879 ) ) ;
#80576 = ORIENTED_EDGE ( 'NONE', *, *, #50827, .T. ) ;
#80575 = CARTESIAN_POINT ( 'NONE',  ( 32.06031249785753090, 1524.760046179776054, 216.1076607587503133 ) ) ;
#80577 = CARTESIAN_POINT ( 'NONE',  ( -0.8431545162750000433, 1451.883321300629859, 183.2674326525980177 ) ) ;
#80578 = B_SPLINE_CURVE_WITH_KNOTS ( 'NONE', 3,
 ( #91443, #57854, #65150, #14719, #66269, #100386 ),
 .UNSPECIFIED., .F., .F.,
 ( 4, 2, 4 ),
 ( -0.03032162748288879869, -0.01516384315529340117, -1.347308482557360576E-05 ),
 .UNSPECIFIED. ) ;
#80579 = CARTESIAN_POINT ( 'NONE',  ( -20.79832720279999947, 1379.854941608700074, 216.4077191293589806 ) ) ;
#80580 = CARTESIAN_POINT ( 'NONE',  ( 4.836838691807330726, 1508.551704408389924, 205.7765624394519932 ) ) ;
#80582 = ORIENTED_EDGE ( 'NONE', *, *, #97548, .F. ) ;
#80581 = FACE_OUTER_BOUND ( 'NONE', #16093, .T. ) ;
#80583 = CARTESIAN_POINT ( 'NONE',  ( -9.299400257574959028, 1446.922142132390036, 190.6945004022419994 ) ) ;
#80584 = VERTEX_POINT ( 'NONE', #48774 ) ;
#80585 = AXIS2_PLACEMENT_3D ( 'NONE', #15298, #50038, #99856 ) ;
#80586 = CARTESIAN_POINT ( 'NONE',  ( -10.72558049390000079, 1390.998992605100057, 215.2615596033689940 ) ) ;
#80587 = CARTESIAN_POINT ( 'NONE',  ( -10.57298823631211526, 1391.449726738521349, 215.2582967309260766 ) ) ;
#80588 = CARTESIAN_POINT ( 'NONE',  ( -7.613267233414999779, 1512.877204813269827, 211.3708094598169964 ) ) ;
#80589 = CARTESIAN_POINT ( 'NONE',  ( 11.36216713388179933, 1503.110266152410077, 211.0233809544849919 ) ) ;
#80590 = CARTESIAN_POINT ( 'NONE',  ( -2.418973636230000057, 1431.127469431690088, 217.1544448978289950 ) ) ;
#80591 = AXIS2_PLACEMENT_3D ( 'NONE', #65416, #90586, #39072 ) ;
#80592 = CARTESIAN_POINT ( 'NONE',  ( -10.08245609418620070, 1472.804170826050040, 207.2994808592069944 ) ) ;
#80593 = CARTESIAN_POINT ( 'NONE',  ( 14.43827355286400049, 1409.417256009360017, 212.9437002319959902 ) ) ;
#80594 = CARTESIAN_POINT ( 'NONE',  ( -7.000000000000000000, 1418.913060387330006, 172.2701767054979882 ) ) ;
#80595 = CARTESIAN_POINT ( 'NONE',  ( -96.47871924218719641, 1385.211633195850027, 295.4357730181330339 ) ) ;
#80596 = LINE ( 'NONE', #73859, #74776 ) ;
#80597 = CARTESIAN_POINT ( 'NONE',  ( -31.44837959398574867, 1511.187213306747708, 220.9083067115980725 ) ) ;
#80598 = CARTESIAN_POINT ( 'NONE',  ( 10.98558675269530127, 1490.788211858329987, 209.4256117797519892 ) ) ;
#80599 = ORIENTED_EDGE ( 'NONE', *, *, #42824, .F. ) ;
#80600 = ORIENTED_EDGE ( 'NONE', *, *, #91995, .F. ) ;
#80601 = CARTESIAN_POINT ( 'NONE',  ( -7.096077632602200147, 1508.610125823030103, 215.7701981269059957 ) ) ;
#80602 = CARTESIAN_POINT ( 'NONE',  ( -12.21876415543579952, 1416.384967875050052, 194.7139283324180212 ) ) ;
#80603 = CARTESIAN_POINT ( 'NONE',  ( -1.878723365004049795, 1496.058737867240097, 196.9227348079259912 ) ) ;
#80604 = CIRCLE ( 'NONE', #5468, 10.00000000000000000 ) ;
#80605 = CARTESIAN_POINT ( 'NONE',  ( 28.93380231721798523, 1509.926839725682157, 214.7155417130382205 ) ) ;
#80606 = CARTESIAN_POINT ( 'NONE',  ( -20.19390448100880064, 1494.711078886199857, 190.7708293110239879 ) ) ;
#80607 = CARTESIAN_POINT ( 'NONE',  ( 1.233310677790000032, 1396.496404931630195, 221.5848227596979996 ) ) ;
#80608 = CARTESIAN_POINT ( 'NONE',  ( 31.80535162409334049, 1525.137906803776559, 202.0924949887490243 ) ) ;
#80609 = CARTESIAN_POINT ( 'NONE',  ( -0.1493273780539999818, 1457.270727498030055, 183.0267056797979990 ) ) ;
#80610 = CARTESIAN_POINT ( 'NONE',  ( -9.657355732020000971, 1366.083296228050131, 207.6218459616989946 ) ) ;
#80611 = CARTESIAN_POINT ( 'NONE',  ( -21.56441729487620051, 1490.297465683720020, 208.8487828826750103 ) ) ;
#80612 = CARTESIAN_POINT ( 'NONE',  ( 3.232732302729357521, 1524.860077346004800, 176.5310237116080714 ) ) ;
#80613 = B_SPLINE_CURVE_WITH_KNOTS ( 'NONE', 3,
 ( #53414, #70243, #36056, #104906, #97065, #104350, #1347, #87565, #43896, #10280, #3575, #96506, #106018, #35486, #28194, #95951, #29294, #88121, #62380 ),
 .UNSPECIFIED., .F., .F.,
 ( 4, 2, 2, 2, 1, 1, 1, 2, 2, 2, 4 ),
 ( 0.000000000000000000, 0.2500000000062882477, 0.3750000000094199648, 0.4375000000109754983, 0.4687500000117625354, 0.4843750000120938259, 0.4921875000122678534, 0.4960937500122905575, 0.5000000000123132615, 0.7500000000061566308, 1.000000000000000000 ),
 .UNSPECIFIED. ) ;
#80614 = CARTESIAN_POINT ( 'NONE',  ( -2.882326017515000061, 1516.969638403840008, 207.4201161117570109 ) ) ;
#80615 = CARTESIAN_POINT ( 'NONE',  ( -13.25366502360200016, 1435.447908314299866, 150.3196125349689964 ) ) ;
#80616 = CARTESIAN_POINT ( 'NONE',  ( 30.31118248177486052, 1526.186458717538926, 201.5497466985118820 ) ) ;
#80617 = CARTESIAN_POINT ( 'NONE',  ( 1.546869375790000056, 1416.835808384130132, 190.2224234606979962 ) ) ;
#80618 = CARTESIAN_POINT ( 'NONE',  ( 1.791819983609999944, 1496.978182980090196, 196.8421287543990275 ) ) ;
#80619 = CARTESIAN_POINT ( 'NONE',  ( 10.96015508933500016, 1516.551704408390151, 225.0317485278669949 ) ) ;
#80620 = CARTESIAN_POINT ( 'NONE',  ( -106.3258853770000059, 1381.775203003109937, 298.5533487220590132 ) ) ;
#80621 = ORIENTED_EDGE ( 'NONE', *, *, #8529, .F. ) ;
#80622 = EDGE_CURVE ( 'NONE', #2110, #101455, #9178, .T. ) ;
#80623 = CARTESIAN_POINT ( 'NONE',  ( 33.93598468090000608, 1424.339495328229987, 259.3467913669979907 ) ) ;
#80624 = CARTESIAN_POINT ( 'NONE',  ( -26.79586899859999960, 1488.686659795530204, 205.7928254789879929 ) ) ;
#80626 = CARTESIAN_POINT ( 'NONE',  ( 13.28956057169999916, 1415.163755984130148, 197.3206489009980089 ) ) ;
#80625 = CARTESIAN_POINT ( 'NONE',  ( -1.548023937630000013, 1507.264922098230045, 180.7964191004979853 ) ) ;
#80627 = CARTESIAN_POINT ( 'NONE',  ( 19.81028111248627610, 1506.776553286653552, 198.6443937896351031 ) ) ;
#80628 = CARTESIAN_POINT ( 'NONE',  ( -33.60183516099999679, 1440.913060382750018, 248.0844435644980024 ) ) ;
#80629 = CARTESIAN_POINT ( 'NONE',  ( 3.394586495530000025, 1484.752177868989975, 220.4731791295990035 ) ) ;
#80630 = ADVANCED_FACE ( 'NONE', ( #82899 ), #93493, .F. ) ;
#80631 = FACE_OUTER_BOUND ( 'NONE', #55643, .T. ) ;
#80632 = CARTESIAN_POINT ( 'NONE',  ( -11.86982405321553813, 1423.326458348927872, 139.0999999980981556 ) ) ;
#80633 = VERTEX_POINT ( 'NONE', #42009 ) ;
#80634 = CARTESIAN_POINT ( 'NONE',  ( 3.344986830760000363, 1396.029869901429947, 197.7886967553979787 ) ) ;
#80635 = CARTESIAN_POINT ( 'NONE',  ( 12.43458519346858715, 1513.190421807558096, 225.8467871284239834 ) ) ;
#80636 = CARTESIAN_POINT ( 'NONE',  ( 38.57017548136569474, 1443.484401788910191, 137.1611502647569978 ) ) ;
#80637 = ORIENTED_EDGE ( 'NONE', *, *, #105614, .T. ) ;
#80638 = ORIENTED_EDGE ( 'NONE', *, *, #22945, .T. ) ;
#80639 = CARTESIAN_POINT ( 'NONE',  ( 2.405030274568579469E-16, 1384.770513348110171, 199.6218459572590120 ) ) ;
#80640 = CARTESIAN_POINT ( 'NONE',  ( 5.583139218519999503, 1422.549100278879905, 194.7453484342989896 ) ) ;
#80641 = ORIENTED_EDGE ( 'NONE', *, *, #108446, .T. ) ;
#80642 = CARTESIAN_POINT ( 'NONE',  ( 0.4843940562340000033, 1419.324133249529950, 184.6861775234980030 ) ) ;
#80643 = CARTESIAN_POINT ( 'NONE',  ( -3.145950129948163809, 1420.252270208513437, 194.0299402294517392 ) ) ;
#80644 = VECTOR ( 'NONE', #4913, 1000.000000000000000 ) ;
#80645 = CARTESIAN_POINT ( 'NONE',  ( -1.522526128800000045, 1470.485953140730089, 235.5269617602980077 ) ) ;
#80646 = CARTESIAN_POINT ( 'NONE',  ( -8.301987938657498844, 1519.913060387329779, 186.6498241004079262 ) ) ;
#80647 = EDGE_LOOP ( 'NONE', ( #38741, #70286, #13443, #87324, #72416, #21987, #97282, #79028 ) ) ;
#80648 = CARTESIAN_POINT ( 'NONE',  ( 11.43740528939999912, 1425.481182534629852, 144.1672625331979987 ) ) ;
#80649 = CARTESIAN_POINT ( 'NONE',  ( -12.85343379847840062, 1416.225364278609959, 221.8532119807159972 ) ) ;
#80650 = CARTESIAN_POINT ( 'NONE',  ( 0.1144963318970000088, 1419.768049673130008, 184.3728032279979914 ) ) ;
#80651 = ORIENTED_EDGE ( 'NONE', *, *, #97413, .F. ) ;
#80652 = CARTESIAN_POINT ( 'NONE',  ( 2.867803626105000170, 1516.994127245590107, 204.4971090729170271 ) ) ;
#80653 = AXIS2_PLACEMENT_3D ( 'NONE', #37702, #79722, #4117 ) ;
#80654 = EDGE_LOOP ( 'NONE', ( #107772, #84218, #107864, #26807 ) ) ;
#80655 = CARTESIAN_POINT ( 'NONE',  ( 11.86306020403040051, 1432.123576808339976, 149.9782128633559921 ) ) ;
#80656 = CARTESIAN_POINT ( 'NONE',  ( 3.211105652400000121, 1415.841839642130026, 233.8555032973979735 ) ) ;
#80657 = ORIENTED_EDGE ( 'NONE', *, *, #85625, .F. ) ;
#80658 = ORIENTED_EDGE ( 'NONE', *, *, #39236, .T. ) ;
#80659 = CARTESIAN_POINT ( 'NONE',  ( -10.50209100468410028, 1480.194371605160086, 208.4668248273180211 ) ) ;
#80660 = CARTESIAN_POINT ( 'NONE',  ( -2.168256794737599691, 1508.371295004969852, 220.6985498477429815 ) ) ;
#80661 = CARTESIAN_POINT ( 'NONE',  ( 7.937475080669701200, 1499.382778073400004, 200.5719245896989946 ) ) ;
#80662 = CIRCLE ( 'NONE', #62803, 5.868098490439995985 ) ;
#80663 = CARTESIAN_POINT ( 'NONE',  ( -7.723409503819699928, 1470.257994933900136, 215.9036483672630027 ) ) ;
#80664 = CARTESIAN_POINT ( 'NONE',  ( 15.39361870879080030, 1452.375503376769984, 147.5811169514580001 ) ) ;
#80665 = CARTESIAN_POINT ( 'NONE',  ( 12.17174069520000046, 1420.444189216879977, 199.8097663552590006 ) ) ;
#80666 = CARTESIAN_POINT ( 'NONE',  ( 5.716900179066289667, 1511.491070485845285, 217.8701534166750946 ) ) ;
#80667 = CARTESIAN_POINT ( 'NONE',  ( 19.19535387687943029, 1456.080104641030175, 225.8939609127118047 ) ) ;
#80668 = CARTESIAN_POINT ( 'NONE',  ( -19.76905052135469987, 1509.627051507924534, 231.1952065043512619 ) ) ;
#80669 = CARTESIAN_POINT ( 'NONE',  ( 0.002606494515621919725, 1408.913151437613124, 231.8315478586514189 ) ) ;
#80671 = CARTESIAN_POINT ( 'NONE',  ( -106.1577809140989928, 1391.913060435339958, 304.2026313505140251 ) ) ;
#80670 = CARTESIAN_POINT ( 'NONE',  ( -13.52030549040000018, 1503.072261434289885, 208.8037810841129840 ) ) ;
#80672 = CARTESIAN_POINT ( 'NONE',  ( -68.07780588645262299, 1379.747638516087818, 279.5234925689441070 ) ) ;
#80673 = VECTOR ( 'NONE', #66961, 1000.000000000000000 ) ;
#80674 = CARTESIAN_POINT ( 'NONE',  ( -9.637203692943991484, 1440.299518560640081, 206.3693651664740116 ) ) ;
#80675 = CARTESIAN_POINT ( 'NONE',  ( -7.469619929815000781, 1513.342361861110248, 201.3714591891869929 ) ) ;
#80676 = ORIENTED_EDGE ( 'NONE', *, *, #34468, .F. ) ;
#80677 = CARTESIAN_POINT ( 'NONE',  ( 1.088018564129999997E-14, 1422.873164470030133, 234.3916895801979763 ) ) ;
#80678 = CARTESIAN_POINT ( 'NONE',  ( 21.83863730836016614, 1523.580203803270706, 183.2673815773253239 ) ) ;
#80679 = CARTESIAN_POINT ( 'NONE',  ( -88.81082328880501109, 1384.972301615300012, 308.2983196932370333 ) ) ;
#80680 = CARTESIAN_POINT ( 'NONE',  ( 4.151873366180000247, 1507.235155069190114, 220.0634631044989931 ) ) ;
#80681 = CARTESIAN_POINT ( 'NONE',  ( -14.92217863770000008, 1415.738355314559840, 212.2123080183590105 ) ) ;
#80683 = EDGE_LOOP ( 'NONE', ( #1913, #11554, #109785, #249 ) ) ;
#80682 = CARTESIAN_POINT ( 'NONE',  ( -9.806574738260000146, 1463.377913006889912, 203.8363535297289957 ) ) ;
#80684 = CARTESIAN_POINT ( 'NONE',  ( 3.770851430420000039, 1430.288814966790142, 217.3901795606089991 ) ) ;
#80685 = TOROIDAL_SURFACE ( 'NONE', #12661, 2.000000000000000000, 1.000000000000000000 ) ;
#80686 = CARTESIAN_POINT ( 'NONE',  ( 16.66231036550724198, 1523.604703353109699, 237.7554842931445478 ) ) ;
#80687 = CARTESIAN_POINT ( 'NONE',  ( -16.10814125329999769, 1416.492096055970023, 209.3578209456409809 ) ) ;
#80688 = CARTESIAN_POINT ( 'NONE',  ( -19.68223018519999812, 1464.931511052589940, 211.0302758615490006 ) ) ;
#80689 = CARTESIAN_POINT ( 'NONE',  ( 13.19864377693500046, 1513.023086264660151, 225.9744572943669993 ) ) ;
#80690 = CARTESIAN_POINT ( 'NONE',  ( -8.954747414950000817, 1440.423832500330036, 186.6003702932979991 ) ) ;
#80691 = CIRCLE ( 'NONE', #39602, 2.000000000000002220 ) ;
#80692 = CARTESIAN_POINT ( 'NONE',  ( 18.94483675106589970, 1509.587814354350257, 184.9180970421039945 ) ) ;
#80693 = CARTESIAN_POINT ( 'NONE',  ( 2.923521462801879967, 1410.394928839790055, 231.6309329194170061 ) ) ;
#80694 = CARTESIAN_POINT ( 'NONE',  ( -22.75273496409559826, 1512.187213306747481, 234.5707981297189235 ) ) ;
#80695 = CARTESIAN_POINT ( 'NONE',  ( 16.91151655639999518, 1417.432431737429852, 226.6666944154980001 ) ) ;
#80696 = CARTESIAN_POINT ( 'NONE',  ( -4.456636540849999939, 1476.515883157990174, 218.9574462611590207 ) ) ;
#80697 = CARTESIAN_POINT ( 'NONE',  ( -32.85805783624314813, 1523.678648413191695, 201.0453875934059340 ) ) ;
#80698 = CARTESIAN_POINT ( 'NONE',  ( 3.251394362135000105, 1516.757508073510053, 207.4061414411269766 ) ) ;
#80699 = CARTESIAN_POINT ( 'NONE',  ( 46.02997383769999828, 1440.913083148580199, 268.4959101745980092 ) ) ;
#80700 = CARTESIAN_POINT ( 'NONE',  ( -18.31053858800000000, 1410.915397185529855, 224.2400752736980110 ) ) ;
#80701 = CARTESIAN_POINT ( 'NONE',  ( 15.36997192539999979, 1435.038989691999859, 147.5081777520979927 ) ) ;
#80702 = AXIS2_PLACEMENT_3D ( 'NONE', #98185, #47245, #13607 ) ;
#80703 = CARTESIAN_POINT ( 'NONE',  ( 21.43187510470000134, 1508.012749821929901, 191.1662891575980154 ) ) ;
#80704 = CARTESIAN_POINT ( 'NONE',  ( 29.55474026598078652, 1509.961787258783716, 207.3740816649607552 ) ) ;
#80705 = CARTESIAN_POINT ( 'NONE',  ( -14.57206770570000032, 1474.063984277629970, 266.8771244472980015 ) ) ;
#80706 = DIRECTION ( 'NONE',  ( 0.9858563016923833633, 0.000000000000000000, 0.1675928173085483863 ) ) ;
#80707 = CARTESIAN_POINT ( 'NONE',  ( -35.91420678757950213, 1436.070278595480204, 135.9004835983330111 ) ) ;
#80708 = CARTESIAN_POINT ( 'NONE',  ( 0.2144289812932060058, 1454.866627002209952, 183.1733190174600168 ) ) ;
#80709 = CARTESIAN_POINT ( 'NONE',  ( -12.40156580232079975, 1408.024392905250124, 203.8687696987620086 ) ) ;
#80710 = CARTESIAN_POINT ( 'NONE',  ( 1.590050350630178855, 1426.843352158476364, 137.0999999982234385 ) ) ;
#80711 = CARTESIAN_POINT ( 'NONE',  ( -4.045211208830000515, 1515.528099018290050, 207.6335164720289868 ) ) ;
#80712 = LINE ( 'NONE', #37604, #85500 ) ;
#80713 = CARTESIAN_POINT ( 'NONE',  ( 2.779282467552740332, 1456.300107729789943, 219.3762139804350113 ) ) ;
#80714 = CARTESIAN_POINT ( 'NONE',  ( -37.46849106905889926, 1436.652236075829933, 134.0999999968449856 ) ) ;
#80715 = FACE_OUTER_BOUND ( 'NONE', #59665, .T. ) ;
#80716 = ORIENTED_EDGE ( 'NONE', *, *, #16624, .F. ) ;
#80717 = CARTESIAN_POINT ( 'NONE',  ( 6.123056445345035570, 1510.784366248568858, 216.5990792139033942 ) ) ;
#80718 = DIRECTION ( 'NONE',  ( 0.9455185755993178454, 0.000000000000000000, -0.3255681544571537578 ) ) ;
#80719 = DIRECTION ( 'NONE',  ( -0.9455185755993167351, 0.000000000000000000, 0.3255681544571568109 ) ) ;
#80720 = ORIENTED_EDGE ( 'NONE', *, *, #61302, .T. ) ;
#80721 = CARTESIAN_POINT ( 'NONE',  ( -0.5199289187719989824, 1463.450241312990102, 202.1355596697889894 ) ) ;
#80722 = CARTESIAN_POINT ( 'NONE',  ( 15.86904733465020101, 1508.170982057090214, 231.8327019708549983 ) ) ;
#80723 = CARTESIAN_POINT ( 'NONE',  ( -37.32007217949999500, 1461.346032246330196, 269.2040743517979990 ) ) ;
#80724 = CARTESIAN_POINT ( 'NONE',  ( -4.378216884482949212, 1453.707746088449994, 199.6107954155660025 ) ) ;
#80725 = CARTESIAN_POINT ( 'NONE',  ( -17.84054674790860773, 1523.580204110581235, 237.8810931398598143 ) ) ;
#80726 = DIRECTION ( 'NONE',  ( 0.03489949194094554841, 0.9993908271853728653, 4.612811327639278900E-09 ) ) ;
#80727 = CARTESIAN_POINT ( 'NONE',  ( -93.65288495826759174, 1384.612519065399965, 309.7350186990149723 ) ) ;
#80728 = CARTESIAN_POINT ( 'NONE',  ( -44.16285280505819344, 1385.000714628640026, 217.3125100336829973 ) ) ;
#80729 = CARTESIAN_POINT ( 'NONE',  ( -12.12611261273299945, 1490.951129191179916, 207.2692690533270081 ) ) ;
#80730 = CARTESIAN_POINT ( 'NONE',  ( -4.672438357553319932, 1508.551704408389924, 205.4176553271170178 ) ) ;
#80731 = CARTESIAN_POINT ( 'NONE',  ( -28.75826058165200294, 1509.399771098719839, 208.7351958221130133 ) ) ;
#80732 = CARTESIAN_POINT ( 'NONE',  ( -2.470955850358427686, 1523.580204110584191, 175.3687159778811520 ) ) ;
#80734 = ORIENTED_EDGE ( 'NONE', *, *, #96614, .T. ) ;
#80733 = CARTESIAN_POINT ( 'NONE',  ( 0.4970513752842960487, 1415.323890719899964, 184.8574490102490131 ) ) ;
#80735 = CARTESIAN_POINT ( 'NONE',  ( -109.8253217000000035, 1384.908747186490018, 311.3807772092590085 ) ) ;
#80736 = CARTESIAN_POINT ( 'NONE',  ( -23.55538518210000021, 1409.900238766430220, 208.7448397572840122 ) ) ;
#80737 = B_SPLINE_CURVE_WITH_KNOTS ( 'NONE', 3,
 ( #26886, #70027, #104690, #1702 ),
 .UNSPECIFIED., .F., .F.,
 ( 4, 4 ),
 ( 0.000000000000000000, 1.000000000000000000 ),
 .UNSPECIFIED. ) ;
#80738 = VECTOR ( 'NONE', #27479, 1000.000000000000000 ) ;
#80739 = CARTESIAN_POINT ( 'NONE',  ( -5.530579386980000400, 1496.346118937389974, 218.9093369348890121 ) ) ;
#80740 = CARTESIAN_POINT ( 'NONE',  ( -12.26151716610000086, 1416.568813549730066, 194.6723721426980092 ) ) ;
#80741 = LINE ( 'NONE', #106487, #33594 ) ;
#80742 = CARTESIAN_POINT ( 'NONE',  ( 22.27637251949999708, 1409.690968457230156, 211.0033668272880050 ) ) ;
#80743 = CARTESIAN_POINT ( 'NONE',  ( -107.2344095241460025, 1391.913060387289988, 307.1919084200470138 ) ) ;
#80744 = CARTESIAN_POINT ( 'NONE',  ( -18.31098522441029885, 1464.870751162060060, 217.5849428054170005 ) ) ;
#80745 = CARTESIAN_POINT ( 'NONE',  ( -15.03569858740000065, 1422.461940334329938, 228.7610666488980087 ) ) ;
#80747 = CARTESIAN_POINT ( 'NONE',  ( -12.26760366359999921, 1381.106678608419998, 202.8726028786589950 ) ) ;
#80746 = DIRECTION ( 'NONE',  ( 0.000000000000000000, -1.000000000000000000, -0.000000000000000000 ) ) ;
#80748 = CARTESIAN_POINT ( 'NONE',  ( 25.19844959086550062, 1449.936406620129901, 207.7167063678460011 ) ) ;
#80749 = CARTESIAN_POINT ( 'NONE',  ( -120.6713756150341652, 1375.179104070688936, 291.9637869975590547 ) ) ;
#80750 = FACE_OUTER_BOUND ( 'NONE', #56813, .T. ) ;
#80751 = B_SPLINE_CURVE_WITH_KNOTS ( 'NONE', 3,
 ( #6479, #49601, #56894, #39535, #92136, #58002, #40630, #83734, #7029, #101068, #100531, #23811 ),
 .UNSPECIFIED., .F., .F.,
 ( 4, 2, 2, 2, 2, 4 ),
 ( 0.000000000000000000, 0.1249999999998835931, 0.2499999999997671862, 0.4999999999998447908, 0.7499999999999223954, 1.000000000000000000 ),
 .UNSPECIFIED. ) ;
#80752 = CARTESIAN_POINT ( 'NONE',  ( -22.75992841280000079, 1415.999885432929887, 212.0429175107379933 ) ) ;
#80753 = CARTESIAN_POINT ( 'NONE',  ( 9.532517564019999057, 1366.286862064870093, 210.6218459616991936 ) ) ;
#80754 = TOROIDAL_SURFACE ( 'NONE', #73653, 30.13701971169416538, 3.000000000000000000 ) ;
#80755 = CARTESIAN_POINT ( 'NONE',  ( -6.560742263465000335, 1517.028034847769959, 205.0881926677770082 ) ) ;
#80756 = DIRECTION ( 'NONE',  ( 0.000000000000000000, 1.000000000000000000, 0.000000000000000000 ) ) ;
#80757 = VERTEX_POINT ( 'NONE', #34153 ) ;
#80758 = FACE_OUTER_BOUND ( 'NONE', #9331, .T. ) ;
#80759 = CARTESIAN_POINT ( 'NONE',  ( -10.34903246276065758, 1422.477322477220014, 210.6474012835178371 ) ) ;
#80761 = VERTEX_POINT ( 'NONE', #67773 ) ;
#80760 = CARTESIAN_POINT ( 'NONE',  ( -67.83249339340770234, 1379.746683816080122, 279.1961202499749675 ) ) ;
#80762 = VERTEX_POINT ( 'NONE', #57180 ) ;
#80763 = CARTESIAN_POINT ( 'NONE',  ( 27.44017514259999757, 1508.035989681029832, 213.3629512357580325 ) ) ;
#80764 = ORIENTED_EDGE ( 'NONE', *, *, #41271, .F. ) ;
#80765 = CARTESIAN_POINT ( 'NONE',  ( 0.3803298753218480321, 1485.753653569830021, 220.9969941478449869 ) ) ;
#80766 = CARTESIAN_POINT ( 'NONE',  ( -109.6582946740000040, 1384.935989956509957, 311.3230066222590153 ) ) ;
#80768 = CARTESIAN_POINT ( 'NONE',  ( -11.99512490559999911, 1410.769353062130222, 225.2869993423979906 ) ) ;
#80767 = CARTESIAN_POINT ( 'NONE',  ( -15.73553964349176226, 1409.462560401643486, 225.4753464985124367 ) ) ;
#80769 = DIRECTION ( 'NONE',  ( -0.6742693640212139572, -4.521919481779818477E-17, -0.7384854939282339270 ) ) ;
#80771 = B_SPLINE_CURVE_WITH_KNOTS ( 'NONE', 3,
 ( #72548, #45154, #106679, #37289, #47337, #12633, #81465, #29970, #105041, #55208, #37838, #96644, #64162, #105602, #55767, #19913, #63617, #98280, #79847, #10980, #63081, #22095, #38915, #97180, #54662, #3708, #54114, #73097, #46266, #80394, #72024, #106140, #97734, #21005, #89337, #107236, #79294, #2605, #36729, #46810, #6981, #15366, #41132, #84233, #39489, #22642, #92634, #100488, #90422 ),
 .UNSPECIFIED., .F., .F.,
 ( 4, 3, 3, 3, 3, 3, 3, 3, 3, 3, 3, 3, 3, 3, 3, 3, 4 ),
 ( -7.217395425439999457, -6.314159096166340746, -5.426996328170729633, -4.536566390866929588, -3.643034527830809832, -2.730152093685779491, -1.829978413125148862, -0.9107416021879179979, 0.008495208749310201313, 0.9096077358356460252, 1.811265860083839385, 2.713151777285197852, 3.614808793634290751, 4.515455451585719260, 5.414687769663739658, 6.316041597551869557, 7.217395425439999457 ),
 .UNSPECIFIED. ) ;
#80770 = CARTESIAN_POINT ( 'NONE',  ( -25.25207292682919658, 1450.803465017199869, 137.6137618836170020 ) ) ;
#80772 = CARTESIAN_POINT ( 'NONE',  ( -1.231622111079999859, 1468.763012560089919, 219.2115919040990093 ) ) ;
#80773 = CARTESIAN_POINT ( 'NONE',  ( 9.206517179299998688, 1410.169093132829857, 230.1231226820979998 ) ) ;
#80774 = CARTESIAN_POINT ( 'NONE',  ( 10.56018849299529982, 1481.177537964639896, 213.4278321560559846 ) ) ;
#80775 = EDGE_CURVE ( 'NONE', #25916, #65578, #13531, .T. ) ;
#80776 =( NAMED_UNIT ( * ) SI_UNIT ( $, .STERADIAN. ) SOLID_ANGLE_UNIT ( ) );
#80777 = CARTESIAN_POINT ( 'NONE',  ( 40.60962964061170055, 1447.683802590399864, 134.0999999984219926 ) ) ;
#80778 = CARTESIAN_POINT ( 'NONE',  ( -7.179517906949999251, 1480.902174850589972, 207.6226633918490165 ) ) ;
#80779 = ORIENTED_EDGE ( 'NONE', *, *, #92721, .F. ) ;
#80780 = CARTESIAN_POINT ( 'NONE',  ( 14.30278547136329870, 1435.293658520200097, 149.3523124186869779 ) ) ;
#80781 = CARTESIAN_POINT ( 'NONE',  ( -1.173443483158729927, 1431.768907133609900, 200.7987716776540026 ) ) ;
#80782 = ORIENTED_EDGE ( 'NONE', *, *, #89359, .T. ) ;
#80783 = EDGE_LOOP ( 'NONE', ( #17505, #54847, #38195, #14643 ) ) ;
#80784 = ORIENTED_EDGE ( 'NONE', *, *, #6976, .T. ) ;
#80785 = CARTESIAN_POINT ( 'NONE',  ( 8.710226003111458226, 1410.592674012450061, 230.2685501115730915 ) ) ;
#80786 = CARTESIAN_POINT ( 'NONE',  ( 16.26362608049849712, 1514.552098279665415, 194.3450158896016831 ) ) ;
#80787 = DIRECTION ( 'NONE',  ( -1.755985294532469921E-16, 1.000000000000000000, -1.338183447452831989E-16 ) ) ;
#80788 = CARTESIAN_POINT ( 'NONE',  ( -3.054816054689999838, 1485.996906145230014, 182.1538611197979947 ) ) ;
#80789 = CIRCLE ( 'NONE', #68328, 7.500000000000000000 ) ;
#80790 = CARTESIAN_POINT ( 'NONE',  ( -17.78690504666375816, 1447.654120957741043, 217.2684850421684359 ) ) ;
#80791 = CARTESIAN_POINT ( 'NONE',  ( -68.16989581615023042, 1379.746757633565267, 278.7814004105860022 ) ) ;
#80792 = CARTESIAN_POINT ( 'NONE',  ( 9221.844915941721410, 50.28429875041810249, -5636.577220268512065 ) ) ;
#80793 = DIRECTION ( 'NONE',  ( -0.9455185755993166241, 1.675808339056839216E-14, 0.3255681544571569219 ) ) ;
#80794 =( BOUNDED_CURVE ( )  B_SPLINE_CURVE ( 3, ( #82665, #108413, #5956, #66980 ),
 .UNSPECIFIED., .F., .F. ) 
 B_SPLINE_CURVE_WITH_KNOTS ( ( 4, 4 ),
 ( 0.9002477009694567212, 1.144704973640544798 ),
 .UNSPECIFIED. ) 
 CURVE ( )  GEOMETRIC_REPRESENTATION_ITEM ( )  RATIONAL_B_SPLINE_CURVE ( ( 1.000000000000000000, 0.9950262503666102987, 0.9950262503666102987, 1.000000000000000000 ) ) 
 REPRESENTATION_ITEM ( '' )  );
#80795 = CARTESIAN_POINT ( 'NONE',  ( 1.543258704960000172, 1416.522662136229883, 190.2352491560979786 ) ) ;
#80796 = CARTESIAN_POINT ( 'NONE',  ( -66.13828525536300162, 1384.712330930560029, 257.5898851940499981 ) ) ;
#80797 = EDGE_LOOP ( 'NONE', ( #88096, #38938, #20852, #110713, #37327 ) ) ;
#80798 = CARTESIAN_POINT ( 'NONE',  ( -7.725990199955000470, 1517.181921232829836, 206.6366402828969910 ) ) ;
#80799 = VERTEX_POINT ( 'NONE', #110306 ) ;
#80800 = CARTESIAN_POINT ( 'NONE',  ( 25.39713358094629569, 1440.913060387330006, 240.3806062677190027 ) ) ;
#80801 = CARTESIAN_POINT ( 'NONE',  ( 11.51338207723369855, 1478.865430962250002, 206.7896514733459981 ) ) ;
#80802 = ORIENTED_EDGE ( 'NONE', *, *, #35867, .T. ) ;
#80803 = CARTESIAN_POINT ( 'NONE',  ( -17.27380372710149103, 1525.712830164893376, 181.5601675622793039 ) ) ;
#80804 = CARTESIAN_POINT ( 'NONE',  ( -15.88334012139999984, 1409.634352649830134, 191.9077379488980171 ) ) ;
#80805 = CARTESIAN_POINT ( 'NONE',  ( -23.20186796309999977, 1425.882772870329973, 212.0388266195080007 ) ) ;
#80807 = CARTESIAN_POINT ( 'NONE',  ( 7.512750207965000371, 1509.038615934239942, 203.6084103740869864 ) ) ;
#80806 = CARTESIAN_POINT ( 'NONE',  ( -24.39260148680000029, 1440.996668616129909, 211.3370849838079835 ) ) ;
#80808 = CARTESIAN_POINT ( 'NONE',  ( -9.307164086263318481, 1437.573555850379989, 212.3980636621099904 ) ) ;
#80809 = CARTESIAN_POINT ( 'NONE',  ( -5.730039698873020448, 1510.523965798400013, 201.5701372575169898 ) ) ;
#80810 = CARTESIAN_POINT ( 'NONE',  ( 35.72701205430000471, 1418.844138006729963, 266.4694652101980523 ) ) ;
#80811 = CARTESIAN_POINT ( 'NONE',  ( -27.66673063000770227, 1441.266444767720259, 137.2829077538830234 ) ) ;
#80813 = EDGE_CURVE ( 'NONE', #42031, #94989, #108730, .T. ) ;
#80812 = CARTESIAN_POINT ( 'NONE',  ( 14.60161135774977126, 1435.005028810949170, 148.0399020830880659 ) ) ;
#80814 = CARTESIAN_POINT ( 'NONE',  ( 20.71343476517513338, 1522.382868172863937, 179.9059455038194528 ) ) ;
#80815 = CARTESIAN_POINT ( 'NONE',  ( -7.715625241105000143, 1516.786099423779888, 215.6766101314970001 ) ) ;
#80816 = CARTESIAN_POINT ( 'NONE',  ( 11.63669227459999966, 1425.864836378729933, 144.1684971660979784 ) ) ;
#80817 = CARTESIAN_POINT ( 'NONE',  ( -0.1604665283746669890, 1507.146139023270052, 180.9012722249049716 ) ) ;
#80818 = CARTESIAN_POINT ( 'NONE',  ( 19.43120254477782893, 1441.383652375895053, 212.5091604960843767 ) ) ;
#80819 = CARTESIAN_POINT ( 'NONE',  ( -5.771797464315000070, 1516.647618671360078, 211.9976960644470125 ) ) ;
#80820 = CARTESIAN_POINT ( 'NONE',  ( -20.52471789389999657, 1470.812340169729850, 209.0748028894099946 ) ) ;
#80821 = CARTESIAN_POINT ( 'NONE',  ( 0.000000000000000000, 1511.187213306747708, 209.1218459616979999 ) ) ;
#80823 = VERTEX_POINT ( 'NONE', #49866 ) ;
#80822 = CARTESIAN_POINT ( 'NONE',  ( -109.9987472859999968, 1389.231820704839947, 308.7519488593589472 ) ) ;
#80824 = CARTESIAN_POINT ( 'NONE',  ( 15.47923624849999946, 1465.564491349630089, 248.5133305153979961 ) ) ;
#80825 = CARTESIAN_POINT ( 'NONE',  ( -11.86593889309999916, 1432.333689122770011, 150.3973551558979977 ) ) ;
#80826 = CARTESIAN_POINT ( 'NONE',  ( -15.43894024600000137, 1415.776528789690246, 207.8411306001490004 ) ) ;
#80827 = DIRECTION ( 'NONE',  ( 0.9980967576408298347, 0.06164622075854649108, 0.001614265483442069724 ) ) ;
#80828 = CARTESIAN_POINT ( 'NONE',  ( -0.3973340087122340103, 1418.672806152889962, 184.7148007238050127 ) ) ;
#80829 = AXIS2_PLACEMENT_3D ( 'NONE', #10225, #9667, #43839 ) ;
#80831 = CARTESIAN_POINT ( 'NONE',  ( 2.500000000000000000, 1430.041878304429929, 157.3252622477980083 ) ) ;
#80830 = CARTESIAN_POINT ( 'NONE',  ( -18.70316662140000119, 1457.451126846130137, 227.2880144703979965 ) ) ;
#80832 = CARTESIAN_POINT ( 'NONE',  ( 6.594884990749999787, 1463.733222497789939, 209.8009783769319938 ) ) ;
#80833 = CARTESIAN_POINT ( 'NONE',  ( -104.2932360906780076, 1380.188221978170077, 306.6001351807259994 ) ) ;
#80834 = ORIENTED_EDGE ( 'NONE', *, *, #32316, .T. ) ;
#80835 = CARTESIAN_POINT ( 'NONE',  ( -2.877744984375000037, 1516.723920667490120, 204.5127816287269980 ) ) ;
#80836 = CARTESIAN_POINT ( 'NONE',  ( 1.770390159249999984, 1406.013915744430051, 266.9599398126979963 ) ) ;
#80837 = CARTESIAN_POINT ( 'NONE',  ( -1.842962231260000028, 1515.551704408389924, 213.1059277140590211 ) ) ;
#80838 = EDGE_CURVE ( 'NONE', #35962, #79801, #58627, .T. ) ;
#80839 = CARTESIAN_POINT ( 'NONE',  ( 38.28767213281710724, 1455.716104437349941, 270.0147264652339913 ) ) ;
#80840 = ADVANCED_FACE ( 'NONE', ( #33581 ), #41465, .F. ) ;
#80841 = CARTESIAN_POINT ( 'NONE',  ( 3.350338079455601026, 1523.604703353109699, 176.1628856388066708 ) ) ;
#80842 = DIRECTION ( 'NONE',  ( 0.000000000000000000, 0.000000000000000000, -1.000000000000000000 ) ) ;
#80843 = ADVANCED_FACE ( 'NONE', ( #27402 ), #35817, .F. ) ;
#80844 = CIRCLE ( 'NONE', #20009, 15.41148139973879871 ) ;
#80845 = CARTESIAN_POINT ( 'NONE',  ( -6.608531157176709137, 1439.954310736166690, 203.3674198005971618 ) ) ;
#80846 = CARTESIAN_POINT ( 'NONE',  ( -4.963305069829999638, 1458.663087589289944, 218.6479516874489946 ) ) ;
#80847 = CARTESIAN_POINT ( 'NONE',  ( -6.632177051280000235, 1428.092653318189832, 204.0245593685589824 ) ) ;
#80848 = ADVANCED_FACE ( 'NONE', ( #2246 ), #50029, .T. ) ;
#80849 = CARTESIAN_POINT ( 'NONE',  ( 2.310870013312309901, 1449.824111145019970, 154.7919404106129946 ) ) ;
#80850 = EDGE_CURVE ( 'NONE', #56812, #52184, #3260, .T. ) ;
#80851 = CARTESIAN_POINT ( 'NONE',  ( -14.37881581502230155, 1416.259629948920065, 221.3107050206100155 ) ) ;
#80852 = CARTESIAN_POINT ( 'NONE',  ( -4.326992699989999913, 1515.158586642889986, 209.1218459616989946 ) ) ;
#80853 = B_SPLINE_CURVE_WITH_KNOTS ( 'NONE', 3,
 ( #25762, #59961, #94076, #87351, #44255, #68921, #90082, #54324, #3918, #13366, #36933, #4454, #21202 ),
 .UNSPECIFIED., .F., .F.,
 ( 4, 3, 3, 3, 4 ),
 ( -1.727219771889999977, -0.7951722241532679369, 0.1344887764924689311, 1.059669685035710129, 1.727219771889999977 ),
 .UNSPECIFIED. ) ;
#80854 = ORIENTED_EDGE ( 'NONE', *, *, #95674, .F. ) ;
#80855 = CARTESIAN_POINT ( 'NONE',  ( -24.08292308869999943, 1431.749769072390109, 243.9198229650980068 ) ) ;
#80856 = ADVANCED_FACE ( 'NONE', ( #104115 ), #14196, .T. ) ;
#80857 = CARTESIAN_POINT ( 'NONE',  ( 6.489845843996670638, 1466.368330838150086, 201.4744493398009979 ) ) ;
#80858 = CARTESIAN_POINT ( 'NONE',  ( -0.5580518338940000378, 1475.981069911630129, 267.2348423975979586 ) ) ;
#80859 = DIRECTION ( 'NONE',  ( -8.703204010890035850E-06, -3.665990706876905690E-05, 0.9999999992901525969 ) ) ;
#80860 = CARTESIAN_POINT ( 'NONE',  ( -8.697287760260000056, 1440.006335262490211, 206.1599773368889714 ) ) ;
#80861 = CARTESIAN_POINT ( 'NONE',  ( -2.991382624059956807, 1448.269496906028508, 184.4535707602067021 ) ) ;
#80862 = CARTESIAN_POINT ( 'NONE',  ( -30.60972296751670285, 1384.826188984249939, 228.7072743885399859 ) ) ;
#80863 = AXIS2_PLACEMENT_3D ( 'NONE', #38389, #5345, #31091 ) ;
#80864 = CARTESIAN_POINT ( 'NONE',  ( -105.3716458700000089, 1379.306619424940209, 302.1984682570590053 ) ) ;
#80865 = CARTESIAN_POINT ( 'NONE',  ( -11.27425270319999839, 1482.889162177290018, 205.2544580881489935 ) ) ;
#80866 = CARTESIAN_POINT ( 'NONE',  ( 8.152186767047583160, 1511.505229895813500, 205.2575009507046957 ) ) ;
#80867 = CARTESIAN_POINT ( 'NONE',  ( -10.79328541798980012, 1396.289970219479983, 211.5874294395580080 ) ) ;
#80868 = EDGE_CURVE ( 'NONE', #104691, #45986, #25731, .T. ) ;
#80869 = CARTESIAN_POINT ( 'NONE',  ( -15.65995984010000086, 1420.957345113829888, 227.0387551958980055 ) ) ;
#80870 = CARTESIAN_POINT ( 'NONE',  ( 31.64580750758041461, 1523.313115944345327, 196.3083633854960794 ) ) ;
#80871 = VERTEX_POINT ( 'NONE', #78369 ) ;
#80872 = CARTESIAN_POINT ( 'NONE',  ( -11.33324210258937192, 1502.232704771361114, 207.2803833977290253 ) ) ;
#80874 = EDGE_CURVE ( 'NONE', #91565, #108700, #29605, .T. ) ;
#80873 = CARTESIAN_POINT ( 'NONE',  ( 2.445258106880000337, 1408.998450681829809, 230.6876405877980005 ) ) ;
#80875 = CARTESIAN_POINT ( 'NONE',  ( -18.75204458307589661, 1485.356665832905264, 189.3982496731914580 ) ) ;
#80877 = CARTESIAN_POINT ( 'NONE',  ( -11.95959066036500040, 1513.007288725360013, 192.5106861886669947 ) ) ;
#80876 = CARTESIAN_POINT ( 'NONE',  ( 10.14778948840000083, 1425.169760000230099, 103.4485609486980024 ) ) ;
#80878 = DIRECTION ( 'NONE',  ( -0.9510565162951518658, 0.000000000000000000, 0.3090169943749528914 ) ) ;
#80879 = EDGE_CURVE ( 'NONE', #46444, #90450, #5517, .T. ) ;
#80880 = CARTESIAN_POINT ( 'NONE',  ( -11.23388613411650638, 1442.762691980111640, 205.3674499604519212 ) ) ;
#80881 = CARTESIAN_POINT ( 'NONE',  ( 3.453544825624999870, 1517.106845464700200, 201.7850012896870169 ) ) ;
#80882 = CARTESIAN_POINT ( 'NONE',  ( 8.439944554000000210, 1428.238409027789885, 213.1498827361689905 ) ) ;
#80883 = CARTESIAN_POINT ( 'NONE',  ( 4.803837674189999518, 1471.771474222590086, 187.6888395837989947 ) ) ;
#80884 = CARTESIAN_POINT ( 'NONE',  ( 3.240124005049999756, 1507.974159727629967, 181.2795196955979975 ) ) ;
#80885 = CARTESIAN_POINT ( 'NONE',  ( 7.629870545114999736, 1512.332007210709889, 206.5727344848370137 ) ) ;
#80886 = CARTESIAN_POINT ( 'NONE',  ( -60.74530810509999412, 1376.530688957809843, 271.1243785565590088 ) ) ;
#80887 = EDGE_CURVE ( 'NONE', #88321, #72815, #100414, .T. ) ;
#80888 = CARTESIAN_POINT ( 'NONE',  ( 7.637356462754751441, 1365.417503186476779, 209.6218459617148824 ) ) ;
#80889 = ORIENTED_EDGE ( 'NONE', *, *, #82339, .F. ) ;
#80890 = ORIENTED_EDGE ( 'NONE', *, *, #71422, .T. ) ;
#80891 = CARTESIAN_POINT ( 'NONE',  ( -10.60278645200000192, 1398.227574263030192, 200.8859367841879759 ) ) ;
#80892 = CARTESIAN_POINT ( 'NONE',  ( 1.151838181399999828, 1507.064426625830038, 237.0475204680980141 ) ) ;
#80893 = CARTESIAN_POINT ( 'NONE',  ( 0.8073615121260000471, 1466.693077628429819, 235.5175635199979922 ) ) ;
#80894 = CARTESIAN_POINT ( 'NONE',  ( 12.45610846519999981, 1519.913060387329779, 228.8821925242980058 ) ) ;
#80895 = CARTESIAN_POINT ( 'NONE',  ( -7.563688229914999894, 1510.983859056260144, 212.0526840097969909 ) ) ;
#80897 = CARTESIAN_POINT ( 'NONE',  ( -1.359208896535600175, 1412.363887663969990, 185.5179172785579738 ) ) ;
#80896 = CARTESIAN_POINT ( 'NONE',  ( -105.5745580539999935, 1391.578493776289861, 304.2150181189589944 ) ) ;
#80898 = CARTESIAN_POINT ( 'NONE',  ( 4.222593189340000386, 1429.767617791429984, 185.2245064671979833 ) ) ;
#80899 = CARTESIAN_POINT ( 'NONE',  ( -2.289647404633549765, 1464.762954016199956, 198.7769187872700059 ) ) ;
#80900 = CARTESIAN_POINT ( 'NONE',  ( -40.68043012285709636, 1444.654440062869980, 137.0056235015979951 ) ) ;
#80901 =( LENGTH_UNIT ( ) NAMED_UNIT ( * ) SI_UNIT ( .MILLI., .METRE. ) );
#80902 = CARTESIAN_POINT ( 'NONE',  ( 39.39001429889999883, 1440.250354032689984, 136.7508189299979904 ) ) ;
#80903 = CARTESIAN_POINT ( 'NONE',  ( 31.23437356469435144, 1512.187213306747481, 195.3468678195113739 ) ) ;
#80904 = CARTESIAN_POINT ( 'NONE',  ( 33.92729710940290744, 1435.682235881620045, 135.5031028085159903 ) ) ;
#80905 = CARTESIAN_POINT ( 'NONE',  ( 11.84773374989999972, 1431.064121367410053, 149.8383244911979943 ) ) ;
#80906 = B_SPLINE_CURVE_WITH_KNOTS ( 'NONE', 3,
 ( #17862, #104101, #88408, #3332, #37456, #102978, #9486, #3878, #38007, #63776 ),
 .UNSPECIFIED., .F., .F.,
 ( 4, 2, 2, 2, 4 ),
 ( 0.000000000000000000, 0.0007189769279726045429, 0.001437953855945209086, 0.002156930783917813520, 0.002875907711890418172 ),
 .UNSPECIFIED. ) ;
#80907 = DIRECTION ( 'NONE',  ( -0.4999999999998399614, -0.7071067811867740582, -0.4999999999998399614 ) ) ;
#80908 = ORIENTED_EDGE ( 'NONE', *, *, #3502, .F. ) ;
#80909 = CARTESIAN_POINT ( 'NONE',  ( -3.827327206003696247, 1409.546157813740592, 137.0999999980979851 ) ) ;
#80910 = CARTESIAN_POINT ( 'NONE',  ( 20.70484064406385727, 1525.907212628473872, 233.2025904124104443 ) ) ;
#80911 = ORIENTED_EDGE ( 'NONE', *, *, #98162, .T. ) ;
#80912 = ORIENTED_EDGE ( 'NONE', *, *, #21681, .T. ) ;
#80913 = CARTESIAN_POINT ( 'NONE',  ( -19.06375576466449928, 1488.013913749329959, 228.8372936450909947 ) ) ;
#80914 = CARTESIAN_POINT ( 'NONE',  ( -14.33877495950000025, 1460.594445894529827, 230.1573440692980341 ) ) ;
#80915 = CARTESIAN_POINT ( 'NONE',  ( -14.70465418319999884, 1470.816980702929868, 194.9479760845979968 ) ) ;
#80916 = CARTESIAN_POINT ( 'NONE',  ( 1.711311228545000063, 1516.591755933730155, 214.8926661113670207 ) ) ;
#80917 = CARTESIAN_POINT ( 'NONE',  ( -13.09461299200390094, 1380.098038397369919, 209.6821016411979883 ) ) ;
#80918 = EDGE_LOOP ( 'NONE', ( #56466, #62100, #12466, #5523, #42318 ) ) ;
#80919 = CARTESIAN_POINT ( 'NONE',  ( -11.71614241347159968, 1509.388950667939980, 181.5344912488080240 ) ) ;
#80920 = CARTESIAN_POINT ( 'NONE',  ( -50.85477211400000641, 1375.010081756269983, 242.1550097575589859 ) ) ;
#80921 = EDGE_CURVE ( 'NONE', #94111, #101374, #16306, .T. ) ;
#80922 = CARTESIAN_POINT ( 'NONE',  ( 16.61533299009999709, 1414.913060387329779, 212.4682773652579897 ) ) ;
#80923 = CARTESIAN_POINT ( 'NONE',  ( -7.335901033725000353, 1517.068717944079935, 205.0869373723870126 ) ) ;
#80924 = ORIENTED_EDGE ( 'NONE', *, *, #95034, .T. ) ;
#80925 = CARTESIAN_POINT ( 'NONE',  ( -29.35072644275227560, 1526.211528530236592, 220.5206086590065127 ) ) ;
#80926 = CARTESIAN_POINT ( 'NONE',  ( -94.50989921500000435, 1384.972694751829977, 294.8597475345590055 ) ) ;
#80927 = CARTESIAN_POINT ( 'NONE',  ( -2.697248550460000338, 1409.007250382230040, 231.5774121206980283 ) ) ;
#80929 = EDGE_LOOP ( 'NONE', ( #105103, #95463, #108422, #33606 ) ) ;
#80928 = CARTESIAN_POINT ( 'NONE',  ( -6.553899686920000356, 1408.913060387329779, 192.3638312768979972 ) ) ;
#80930 = CARTESIAN_POINT ( 'NONE',  ( -17.17760814124009983, 1517.051704413129983, 195.4929600000709797 ) ) ;
#80931 = CARTESIAN_POINT ( 'NONE',  ( -30.39409183528769987, 1440.913060387249971, 239.5824303925190009 ) ) ;
#80932 = CARTESIAN_POINT ( 'NONE',  ( -13.36052273939999857, 1384.881792980340151, 218.9673617354289945 ) ) ;
#80934 = EDGE_CURVE ( 'NONE', #38761, #87765, #104386, .T. ) ;
#80933 = CARTESIAN_POINT ( 'NONE',  ( 34.68852446352940433, 1501.977400791986611, 199.9946320047950223 ) ) ;
#80935 = CARTESIAN_POINT ( 'NONE',  ( 43.35688237767370623, 1431.798309265539956, 270.1056626526180366 ) ) ;
#80936 = CARTESIAN_POINT ( 'NONE',  ( -0.7355686809059980291, 1517.012231669750008, 212.3888856620870058 ) ) ;
#80937 = CARTESIAN_POINT ( 'NONE',  ( -67.96433663839999895, 1379.748578009009861, 278.4994408155590122 ) ) ;
#80938 = CARTESIAN_POINT ( 'NONE',  ( 23.66578124539999806, 1410.976491880930098, 207.8922445630679761 ) ) ;
#80939 = CARTESIAN_POINT ( 'NONE',  ( -12.08786860576782729, 1428.067598096224174, 223.1528678408886037 ) ) ;
#80940 = CARTESIAN_POINT ( 'NONE',  ( -30.77259778570326176, 1524.972383263453366, 221.6912870679553862 ) ) ;
#80941 = CARTESIAN_POINT ( 'NONE',  ( -7.712670236151770276, 1516.673252337400072, 210.0631823355520282 ) ) ;
#80942 = CARTESIAN_POINT ( 'NONE',  ( 7.339107202615000602, 1517.203017563489766, 210.2473558205170150 ) ) ;
#80943 = CARTESIAN_POINT ( 'NONE',  ( 4.172805552454540212, 1421.497310399080106, 184.9553930896919951 ) ) ;
#80944 = LINE ( 'NONE', #54668, #64554 ) ;
#80945 = CARTESIAN_POINT ( 'NONE',  ( -81.17714880479999806, 1384.872208132610012, 304.9620800596590016 ) ) ;
#80946 = EDGE_LOOP ( 'NONE', ( #7064, #79827, #21581, #102079 ) ) ;
#80948 = B_SPLINE_CURVE_WITH_KNOTS ( 'NONE', 3,
 ( #90424, #46811, #14269, #49009, #89883, #74216, #38917, #13702, #48460, #57419, #63619, #97735, #47890, #21006, #81467, #5330, #55209, #31627, #72550, #73661, #82026, #65260, #22096, #6440, #65805, #73098, #98836, #99371, #99925, #107237, #64720, #83145, #39490, #82598, #29971, #91545, #107793, #89338, #22643, #23219, #80941, #31077, #40585, #4239, #5888, #30528, #38374, #108345, #74757, #21557, #29419, #64163, #12634, #106680, #98281, #13153, #47338, #49558, #68024, #85897, #57957, #15909, #9203, #24860 ),
 .UNSPECIFIED., .F., .F.,
 ( 4, 3, 3, 3, 3, 3, 3, 3, 3, 3, 3, 3, 3, 3, 3, 3, 3, 3, 3, 3, 3, 4 ),
 ( -14.97205243065559976, -14.82652090134419964, -14.54016986210000084, -14.44422471178040013, -14.18616264305039998, -13.96389174838669867, -13.75628582469069983, -13.55954966579430021, -13.48778920245429980, -13.41168693589320071, -13.29682063962729899, -13.03955858623080033, -12.77367974343709989, -12.48589049144669971, -12.17406903241579919, -11.81735513509999969, -11.73764735024779959, -11.37242316392340058, -11.02427058926000036, -10.95328185380470032, -10.66065659679330047, -10.38572052090729869 ),
 .UNSPECIFIED. ) ;
#80947 = CARTESIAN_POINT ( 'NONE',  ( -20.99389299076310067, 1385.272353955699828, 221.3600716116459921 ) ) ;
#80949 = EDGE_CURVE ( 'NONE', #84894, #107129, #91092, .T. ) ;
#80950 = CARTESIAN_POINT ( 'NONE',  ( 18.90776592919999644, 1416.839648759230158, 210.0259814473739937 ) ) ;
#80951 = CARTESIAN_POINT ( 'NONE',  ( -21.06135014068000189, 1509.319523268100056, 228.6460338313929981 ) ) ;
#80952 = EDGE_CURVE ( 'NONE', #104178, #34578, #24242, .T. ) ;
#80953 = CARTESIAN_POINT ( 'NONE',  ( 7.594039249315000184, 1512.142919181319940, 206.8921143228970152 ) ) ;
#80954 = CARTESIAN_POINT ( 'NONE',  ( 12.25490649660000031, 1421.424738529230126, 204.6606925453189945 ) ) ;
#80955 = CARTESIAN_POINT ( 'NONE',  ( -14.94707557629999961, 1464.413060387330006, 223.3779789887979916 ) ) ;
#80956 = CARTESIAN_POINT ( 'NONE',  ( -1.709384611084999950, 1517.224900789629828, 216.4615953054470197 ) ) ;
#80957 = CARTESIAN_POINT ( 'NONE',  ( 0.4151546846821903003, 1511.187213306747708, 243.9330574173806951 ) ) ;
#80958 = CARTESIAN_POINT ( 'NONE',  ( 10.00951688712369858, 1468.852972450649986, 208.4479931420239893 ) ) ;
#80959 = ORIENTED_EDGE ( 'NONE', *, *, #106908, .T. ) ;
#80960 = CARTESIAN_POINT ( 'NONE',  ( -3.260378293205000055, 1516.582197289609894, 201.4115600944169842 ) ) ;
#80961 = CARTESIAN_POINT ( 'NONE',  ( 10.08517028152789941, 1480.579361189179963, 206.0651545076909770 ) ) ;
#80962 = EDGE_LOOP ( 'NONE', ( #13418, #106329, #70149, #34655 ) ) ;
#80963 = CARTESIAN_POINT ( 'NONE',  ( 11.60004869884835621, 1426.501518730301996, 135.6460183129449604 ) ) ;
#80964 = EDGE_CURVE ( 'NONE', #5353, #44905, #99004, .T. ) ;
#80965 = CARTESIAN_POINT ( 'NONE',  ( 9.928347934575134204, 1435.779368277902222, 152.5402617987141696 ) ) ;
#80966 = CARTESIAN_POINT ( 'NONE',  ( 7.926223792202339524, 1423.719494923044977, 195.8478123068922798 ) ) ;
#80967 = CARTESIAN_POINT ( 'NONE',  ( 1.101591607640000081, 1442.758995474489893, 218.3133920886989756 ) ) ;
#80968 = CARTESIAN_POINT ( 'NONE',  ( -26.90301038610129680, 1509.321327670540086, 201.3214349759640243 ) ) ;
#80969 = CARTESIAN_POINT ( 'NONE',  ( -2.705316718739999793, 1447.083576453610021, 165.9366052023979989 ) ) ;
#80971 = ADVANCED_FACE ( 'NONE', ( #21176 ), #39099, .T. ) ;
#80970 = CARTESIAN_POINT ( 'NONE',  ( -19.14726318969999852, 1425.916566196629901, 226.2004032037980039 ) ) ;
#80972 = CARTESIAN_POINT ( 'NONE',  ( -20.53413670659999823, 1435.214474261499845, 143.2474216777980018 ) ) ;
#80973 = CARTESIAN_POINT ( 'NONE',  ( -0.5954300179934969295, 1497.361593313569983, 231.3170566686650034 ) ) ;
#80974 = CARTESIAN_POINT ( 'NONE',  ( 16.10738486569999850, 1509.418797648129839, 185.7100371376980092 ) ) ;
#80976 = CARTESIAN_POINT ( 'NONE',  ( -17.88309616991011453, 1434.908678899640790, 215.0727088695880127 ) ) ;
#80975 = CARTESIAN_POINT ( 'NONE',  ( -106.0221095560000037, 1391.653194082120081, 301.9380359125589735 ) ) ;
#80977 = CYLINDRICAL_SURFACE ( 'NONE', #65372, 2.499999999999989786 ) ;
#80978 = ORIENTED_EDGE ( 'NONE', *, *, #104372, .T. ) ;
#80979 = DIRECTION ( 'NONE',  ( 0.4090087482554204401, 2.838068309914575726E-15, 0.9125304618754019881 ) ) ;
#80980 = CARTESIAN_POINT ( 'NONE',  ( -13.27855961070000212, 1508.487312425190112, 216.9533382897689933 ) ) ;
#80981 = DIRECTION ( 'NONE',  ( -1.836970198721029688E-16, -1.000000000000000000, 0.000000000000000000 ) ) ;
#80982 = ADVANCED_FACE ( 'NONE', ( #73276 ), #46443, .F. ) ;
#80983 = CARTESIAN_POINT ( 'NONE',  ( -17.55396644409012907, 1524.816548299036640, 237.4834937945546187 ) ) ;
#80984 = CARTESIAN_POINT ( 'NONE',  ( -1.726834413310000205, 1484.334256824789918, 198.5613324875990315 ) ) ;
#80985 = DIRECTION ( 'NONE',  ( -5.980589973904019347E-17, 1.000000000000000000, -1.736889445713099699E-16 ) ) ;
#80986 = CARTESIAN_POINT ( 'NONE',  ( -2.968899200039013753, 1425.987603892220477, 185.4310391008963563 ) ) ;
#80987 = CARTESIAN_POINT ( 'NONE',  ( -12.58579218318286053, 1442.781936543507527, 186.0352767261755105 ) ) ;
#80988 = CARTESIAN_POINT ( 'NONE',  ( 13.56949689579999863, 1407.458599673630033, 211.9076660747180085 ) ) ;
#80989 = CARTESIAN_POINT ( 'NONE',  ( 2.461360751019160187, 1493.777257040230097, 219.9857987593770190 ) ) ;
#80990 = EDGE_CURVE ( 'NONE', #66010, #89621, #102023, .T. ) ;
#80991 = CARTESIAN_POINT ( 'NONE',  ( 9.738317565070000015, 1493.400072498489862, 188.2659980885989910 ) ) ;
#80992 = CARTESIAN_POINT ( 'NONE',  ( -15.39283239035830064, 1415.677402202039957, 209.2531991726660294 ) ) ;
#80993 = CARTESIAN_POINT ( 'NONE',  ( -109.5761286768430125, 1384.171525062670071, 311.2610357945890200 ) ) ;
#80994 = CARTESIAN_POINT ( 'NONE',  ( -0.08855571868401390656, 1516.909122020869972, 201.4030000720750024 ) ) ;
#80996 = EDGE_LOOP ( 'NONE', ( #4720, #1909, #53135, #93627 ) ) ;
#80995 = CARTESIAN_POINT ( 'NONE',  ( -18.51973145710680058, 1443.522805491569898, 212.3835520930680048 ) ) ;
#80997 = CARTESIAN_POINT ( 'NONE',  ( 14.75568479846049819, 1513.870294662269998, 224.0700459103859714 ) ) ;
#80998 = ORIENTED_EDGE ( 'NONE', *, *, #29636, .T. ) ;
#80999 = ORIENTED_EDGE ( 'NONE', *, *, #98162, .F. ) ;
#81000 = CARTESIAN_POINT ( 'NONE',  ( 24.96344457455600008, 1444.384464582640021, 207.7241043758569674 ) ) ;
#81001 = FACE_OUTER_BOUND ( 'NONE', #47325, .T. ) ;
#81002 = CARTESIAN_POINT ( 'NONE',  ( 7.294045558785978045, 1423.346842215470815, 213.7896502874405655 ) ) ;
#81004 = CARTESIAN_POINT ( 'NONE',  ( -36.52133863790000134, 1445.557345868840230, 254.5789810496980010 ) ) ;
#81003 = CARTESIAN_POINT ( 'NONE',  ( 16.16460400119147778, 1412.754790776669097, 269.3697747609250541 ) ) ;
#81005 = CARTESIAN_POINT ( 'NONE',  ( -20.47178266730000118, 1503.711780051630058, 190.1944351405979887 ) ) ;
#81006 = CARTESIAN_POINT ( 'NONE',  ( -109.4427638259999895, 1384.881580825830042, 297.1256396965589488 ) ) ;
#81007 = CARTESIAN_POINT ( 'NONE',  ( -1.031155851060000073, 1488.425564119090041, 217.1473006051089669 ) ) ;
#81008 = CARTESIAN_POINT ( 'NONE',  ( 11.62784611939870061, 1426.769117065760156, 136.3672025267389927 ) ) ;
#81009 = DIRECTION ( 'NONE',  ( -0.000000000000000000, -1.000000000000000000, -0.000000000000000000 ) ) ;
#81010 = CARTESIAN_POINT ( 'NONE',  ( -25.18648013920000039, 1436.583765715590062, 137.5280688333979811 ) ) ;
#81012 = EDGE_CURVE ( 'NONE', #49931, #64042, #71200, .T. ) ;
#81011 = CARTESIAN_POINT ( 'NONE',  ( 0.05006135363680530581, 1515.158685764440179, 213.4488360661000002 ) ) ;
#81013 = CARTESIAN_POINT ( 'NONE',  ( -21.41971086555122028, 1511.187213306747708, 185.1638823089581081 ) ) ;
#81014 = CARTESIAN_POINT ( 'NONE',  ( -10.79334919306910123, 1480.196592731939973, 213.7852440063740289 ) ) ;
#81015 = CARTESIAN_POINT ( 'NONE',  ( -3.627397453644670033, 1362.602819439402992, 208.3718459617061285 ) ) ;
#81017 = ORIENTED_EDGE ( 'NONE', *, *, #29171, .T. ) ;
#81016 = CARTESIAN_POINT ( 'NONE',  ( 5.086570735490939355E-09, 1409.986055680089976, 258.6209524227260204 ) ) ;
#81018 = VERTEX_POINT ( 'NONE', #107967 ) ;
#81019 = CARTESIAN_POINT ( 'NONE',  ( -11.36958083090000038, 1503.847187927490268, 207.0750579214790150 ) ) ;
#81020 = CARTESIAN_POINT ( 'NONE',  ( -5.768266513520000416, 1492.234223000290058, 185.8590593905989863 ) ) ;
#81021 = CARTESIAN_POINT ( 'NONE',  ( -13.37958332629999880, 1471.793002122430153, 270.4094488012979696 ) ) ;
#81022 = CARTESIAN_POINT ( 'NONE',  ( 8.028494635650000433, 1421.573180670790180, 196.0255996755989827 ) ) ;
#81023 = CARTESIAN_POINT ( 'NONE',  ( -102.0933291365972053, 1371.894749952189159, 310.3987084017696816 ) ) ;
#81024 = CARTESIAN_POINT ( 'NONE',  ( 14.72577158086200022, 1514.214451999800076, 194.1036973123569851 ) ) ;
#81025 = CARTESIAN_POINT ( 'NONE',  ( 0.2383086145270630063, 1451.487641661899943, 182.6700190730029760 ) ) ;
#81026 = CARTESIAN_POINT ( 'NONE',  ( -14.06463665569999932, 1420.693613352630109, 227.5127406239979848 ) ) ;
#81027 = CARTESIAN_POINT ( 'NONE',  ( 0.9885189933060011258, 1456.680325442589947, 199.2944122769889930 ) ) ;
#81028 = CARTESIAN_POINT ( 'NONE',  ( -4.082704913390346135, 1515.071394843999087, 205.5354683776590434 ) ) ;
#81029 = CARTESIAN_POINT ( 'NONE',  ( 9.093835586142619221, 1363.023136422003972, 210.6218459616991936 ) ) ;
#81030 = CARTESIAN_POINT ( 'NONE',  ( -45.04224761993110349, 1433.697822895979925, 268.5281460005010103 ) ) ;
#81031 = VERTEX_POINT ( 'NONE', #83321 ) ;
#81032 = CARTESIAN_POINT ( 'NONE',  ( -3.542414024086459889, 1500.294088126669976, 181.2680764341660051 ) ) ;
#81033 = EDGE_LOOP ( 'NONE', ( #29521, #85534, #106967, #97450 ) ) ;
#81034 = VERTEX_POINT ( 'NONE', #66556 ) ;
#81035 = CARTESIAN_POINT ( 'NONE',  ( 2.300729626665000360, 1516.923170579120097, 210.8225527465970117 ) ) ;
#81036 = CARTESIAN_POINT ( 'NONE',  ( 4.494990604111427146, 1423.798284629885757, 183.7099184631668720 ) ) ;
#81037 = DIRECTION ( 'NONE',  ( 0.9996573249755569268, 0.02617694830788839730, 1.176140869340470334E-16 ) ) ;
#81038 = CARTESIAN_POINT ( 'NONE',  ( -6.310775319510000259, 1470.460832479730243, 184.4692652257980114 ) ) ;
#81039 = CARTESIAN_POINT ( 'NONE',  ( 5.360207926212690488, 1422.242713656610022, 144.1549664376839814 ) ) ;
#81040 = ORIENTED_EDGE ( 'NONE', *, *, #94766, .T. ) ;
#81041 = CARTESIAN_POINT ( 'NONE',  ( 2.485205649205000089, 1517.181921232829836, 201.3958557702769951 ) ) ;
#81042 = CARTESIAN_POINT ( 'NONE',  ( 6.287349243829999601, 1473.446183115890108, 218.1771757008089878 ) ) ;
#81043 = CARTESIAN_POINT ( 'NONE',  ( -23.72302164034240235, 1384.541713701390108, 202.8184092090419881 ) ) ;
#81044 = VERTEX_POINT ( 'NONE', #14451 ) ;
#81045 = CARTESIAN_POINT ( 'NONE',  ( -22.76371513368420452, 1413.786089238920113, 270.3574169790829842 ) ) ;
#81046 = CARTESIAN_POINT ( 'NONE',  ( -30.19569412050000068, 1435.551785849099815, 135.1818641824980034 ) ) ;
#81047 = CARTESIAN_POINT ( 'NONE',  ( 8.367692836712059545, 1436.613519496920162, 207.0421242491720193 ) ) ;
#81049 = VERTEX_POINT ( 'NONE', #49192 ) ;
#81048 = CARTESIAN_POINT ( 'NONE',  ( -8.000983929430127262, 1364.900167260016815, 209.6218459617148824 ) ) ;
#81050 = EDGE_LOOP ( 'NONE', ( #25453, #38197, #58652, #49266 ) ) ;
#81051 = CARTESIAN_POINT ( 'NONE',  ( 40.87089738971353370, 1456.294579038563143, 269.1063834202503813 ) ) ;
#81052 = CARTESIAN_POINT ( 'NONE',  ( 11.11707036908040003, 1471.687204444999907, 211.7794637602030150 ) ) ;
#81053 = ADVANCED_FACE ( 'NONE', ( #67650 ), #91095, .T. ) ;
#81054 = CARTESIAN_POINT ( 'NONE',  ( -13.95044291110659884, 1436.238062604179959, 150.2632303846619948 ) ) ;
#81055 = CARTESIAN_POINT ( 'NONE',  ( -0.03462643923284049879, 1410.128970406620056, 185.0390004595289781 ) ) ;
#81056 = CARTESIAN_POINT ( 'NONE',  ( -7.710967015764999211, 1516.608208975040043, 210.2506035313070072 ) ) ;
#81057 = CARTESIAN_POINT ( 'NONE',  ( -20.74431189456849722, 1506.539416732394102, 216.6629043160080812 ) ) ;
#81058 = CARTESIAN_POINT ( 'NONE',  ( 6.749186742440000053, 1455.205488045889979, 217.3783194977189908 ) ) ;
#81059 = CARTESIAN_POINT ( 'NONE',  ( -0.0001244928238367220131, 1476.109334953009920, 267.8539258397410094 ) ) ;
#81060 = CARTESIAN_POINT ( 'NONE',  ( 11.76272948489999948, 1415.263254653229978, 222.9123187206980106 ) ) ;
#81061 = CARTESIAN_POINT ( 'NONE',  ( 7.559673304084999934, 1510.830536680500245, 205.9482437802269885 ) ) ;
#81062 = CARTESIAN_POINT ( 'NONE',  ( -4.043366258305000294, 1516.951766529250108, 206.2549880390970145 ) ) ;
#81063 = ORIENTED_EDGE ( 'NONE', *, *, #27517, .T. ) ;
#81064 = CARTESIAN_POINT ( 'NONE',  ( -36.37832872588079169, 1451.642701155429904, 134.7398512091019995 ) ) ;
#81065 = CARTESIAN_POINT ( 'NONE',  ( -23.84299525371533690, 1446.521247574655490, 213.7712371745673465 ) ) ;
#81066 = ORIENTED_EDGE ( 'NONE', *, *, #100084, .T. ) ;
#81067 = CARTESIAN_POINT ( 'NONE',  ( 3.955232551284513232, 1457.450780121971093, 228.4962720231502828 ) ) ;
#81068 = EDGE_CURVE ( 'NONE', #14911, #108882, #19268, .T. ) ;
#81069 = CARTESIAN_POINT ( 'NONE',  ( 24.07258447067579965, 1452.056610454110114, 137.0856313116819933 ) ) ;
#81070 = CARTESIAN_POINT ( 'NONE',  ( 13.91566348329999947, 1415.553739809529816, 196.9408153421979932 ) ) ;
#81071 = CARTESIAN_POINT ( 'NONE',  ( -9.113128543256529213, 1384.565653361969908, 199.9635744024730002 ) ) ;
#81072 = CARTESIAN_POINT ( 'NONE',  ( 22.02260509859999971, 1411.040493132430129, 203.2687847944879991 ) ) ;
#81073 = CARTESIAN_POINT ( 'NONE',  ( -2.572473174660243611, 1447.610664178797833, 170.5280181871044078 ) ) ;
#81074 = CARTESIAN_POINT ( 'NONE',  ( -26.02813552489999793, 1435.406381042510020, 135.3446223067979872 ) ) ;
#81075 = DIRECTION ( 'NONE',  ( -0.000000000000000000, -1.000000000000000000, -0.000000000000000000 ) ) ;
#81076 = CARTESIAN_POINT ( 'NONE',  ( 31.34137657934018506, 1523.382868172864164, 221.9025654077410081 ) ) ;
#81077 = CARTESIAN_POINT ( 'NONE',  ( 0.8897843876074499336, 1451.970290787959811, 183.2052206821309994 ) ) ;
#81078 = CARTESIAN_POINT ( 'NONE',  ( 2.500000000000199840, 1439.253548877449930, 159.5301951678090120 ) ) ;
#81079 = CARTESIAN_POINT ( 'NONE',  ( 2.875850094215000041, 1516.647618671360078, 214.8936433964170192 ) ) ;
#81080 = ORIENTED_EDGE ( 'NONE', *, *, #9797, .T. ) ;
#81081 = CARTESIAN_POINT ( 'NONE',  ( 7.708876326848260518, 1516.528370242520168, 207.0834033919979902 ) ) ;
#81082 = B_SPLINE_SURFACE_WITH_KNOTS ( 'NONE', 5, 4, ( 
 ( #11468, #17615, #87059, #78105, #77020 ),
 ( #10346, #53482, #1982, #9798, #70301 ),
 ( #326, #45089, #34452, #79229, #61893 ),
 ( #43963, #873, #34997, #69177, #103283 ),
 ( #102729, #26590, #95466, #44518, #26023 ),
 ( #18730, #104413, #2538, #60787, #27706 ),
 ( #1406, #60219, #94337, #62449, #36662 ),
 ( #94913, #35547, #69742, #70856, #104967 ),
 ( #103861, #27162, #54591, #88726, #37767 ) ),
 .UNSPECIFIED., .F., .F., .F.,
 ( 6, 3, 6 ),
 ( 5, 5 ),
 ( 0.000000000000000000, 5.782490304330000441, 11.25975508159999983 ),
 ( 40.20365518519999881, 50.26548245740000453 ),
 .UNSPECIFIED. ) ;
#81083 = CARTESIAN_POINT ( 'NONE',  ( -3.152270375085599596, 1474.954422185709745, 198.1306180807430053 ) ) ;
#81084 = CARTESIAN_POINT ( 'NONE',  ( -0.2587093370397540171, 1408.925427049060090, 231.8715964213000120 ) ) ;
#81085 = CARTESIAN_POINT ( 'NONE',  ( -5.684698874817770253, 1422.983442514339913, 101.6537644099010009 ) ) ;
#81086 = CARTESIAN_POINT ( 'NONE',  ( -39.77744193145330343, 1446.343101763050072, 136.7458254679739866 ) ) ;
#81087 = CARTESIAN_POINT ( 'NONE',  ( 11.60004869885203682, 1425.678573708903514, 138.3920037478602012 ) ) ;
#81088 = DIRECTION ( 'NONE',  ( -0.9955685427539349153, -0.04363816682463748930, 0.08330058268098361474 ) ) ;
#81089 = CARTESIAN_POINT ( 'NONE',  ( -2.637143185960590053, 1477.800872778979965, 183.5714675770420001 ) ) ;
#81091 = ADVANCED_FACE ( 'NONE', ( #68211 ), #43540, .T. ) ;
#81090 = CARTESIAN_POINT ( 'NONE',  ( -0.08399573354635679612, 1455.696542369420058, 198.5840329839000162 ) ) ;
#81092 = CARTESIAN_POINT ( 'NONE',  ( -3.276827735968430133, 1474.091273656589919, 270.1354579856779878 ) ) ;
#81093 = CARTESIAN_POINT ( 'NONE',  ( 34.06181652996020404, 1440.913060384559913, 248.9867622432190046 ) ) ;
#81094 = CARTESIAN_POINT ( 'NONE',  ( -1.531858734065989602E-13, 1515.051704408389924, 205.2922258481490303 ) ) ;
#81095 = CARTESIAN_POINT ( 'NONE',  ( -32.31946296792706619, 1524.082582765195411, 202.1440730665343324 ) ) ;
#81096 = EDGE_LOOP ( 'NONE', ( #72497, #98301, #29747, #58882 ) ) ;
#81097 = EDGE_CURVE ( 'NONE', #51752, #38761, #51054, .T. ) ;
#81098 = CARTESIAN_POINT ( 'NONE',  ( -2.487935123034409557, 1508.603735228351297, 213.8522301342857475 ) ) ;
#81099 = ADVANCED_FACE ( 'NONE', ( #34571 ), #57161, .F. ) ;
#81100 = FACE_OUTER_BOUND ( 'NONE', #7234, .T. ) ;
#81101 = CARTESIAN_POINT ( 'NONE',  ( -28.59841874049999788, 1509.911739175030107, 211.5620548042080031 ) ) ;
#81102 = CARTESIAN_POINT ( 'NONE',  ( 12.18686852027619949, 1501.408139047200166, 211.6432815866139947 ) ) ;
#81103 = EDGE_CURVE ( 'NONE', #73081, #23187, #89708, .T. ) ;
#81104 = LINE ( 'NONE', #38546, #21667 ) ;
#81105 = CARTESIAN_POINT ( 'NONE',  ( -13.73919968929999946, 1508.116376860629998, 232.6024638145979964 ) ) ;
#81106 = CARTESIAN_POINT ( 'NONE',  ( -46.55794552509269835, 1383.817606665970061, 254.2825134048519828 ) ) ;
#81107 = CARTESIAN_POINT ( 'NONE',  ( -4.678978663885700051, 1508.551704408389924, 205.0635906264530206 ) ) ;
#81109 =( BOUNDED_CURVE ( )  B_SPLINE_CURVE ( 3, ( #100552, #49076, #72617, #74282 ),
 .UNSPECIFIED., .F., .F. ) 
 B_SPLINE_CURVE_WITH_KNOTS ( ( 4, 4 ),
 ( 4.624801027031749889, 4.863190234949479773 ),
 .UNSPECIFIED. ) 
 CURVE ( )  GEOMETRIC_REPRESENTATION_ITEM ( )  RATIONAL_B_SPLINE_CURVE ( ( 1.000000000000000000, 0.9952698197215197329, 0.9952698197215197329, 1.000000000000000000 ) ) 
 REPRESENTATION_ITEM ( '' )  );
#81108 = DIRECTION ( 'NONE',  ( -0.4544580288560248760, -1.636314548565651616E-16, -0.8907681516580486791 ) ) ;
#81110 = CARTESIAN_POINT ( 'NONE',  ( 1.846023538469999892, 1465.081219559430110, 235.4517473921979729 ) ) ;
#81112 = ORIENTED_EDGE ( 'NONE', *, *, #27754, .T. ) ;
#81111 = CARTESIAN_POINT ( 'NONE',  ( -13.92686555291570194, 1517.051704405520013, 226.1812314194930025 ) ) ;
#81113 = CARTESIAN_POINT ( 'NONE',  ( -0.4298670265450000305, 1452.022084704629833, 183.1235002304979957 ) ) ;
#81114 = CARTESIAN_POINT ( 'NONE',  ( -39.75532303620000363, 1384.581637800209819, 212.4630896483189701 ) ) ;
#81115 = CARTESIAN_POINT ( 'NONE',  ( -3.151263210079999766, 1476.308150043789965, 199.2625576691089861 ) ) ;
#81117 = ORIENTED_EDGE ( 'NONE', *, *, #89477, .T. ) ;
#81116 = CARTESIAN_POINT ( 'NONE',  ( -16.66147553287439820, 1414.913057846380070, 208.2448045594530015 ) ) ;
#81118 = CARTESIAN_POINT ( 'NONE',  ( 18.32583560018409941, 1473.764173505169765, 194.8973815002569836 ) ) ;
#81119 = ORIENTED_EDGE ( 'NONE', *, *, #34965, .F. ) ;
#81120 = CARTESIAN_POINT ( 'NONE',  ( -8.424900129770140467, 1387.809024083920121, 218.2696960641690112 ) ) ;
#81121 = LINE ( 'NONE', #30161, #76564 ) ;
#81122 = DIRECTION ( 'NONE',  ( 0.5450600352768949497, -0.8383970168982891602, 0.000000000000000000 ) ) ;
#81123 = CARTESIAN_POINT ( 'NONE',  ( -5.302704825520000220, 1464.205378554289837, 199.9536502662190003 ) ) ;
#81124 = CARTESIAN_POINT ( 'NONE',  ( -23.59335433665016524, 1521.951704408389787, 209.8811657366738928 ) ) ;
#81125 = CARTESIAN_POINT ( 'NONE',  ( 20.84639163829999831, 1494.459648749690132, 206.0923896281290126 ) ) ;
#81126 = CARTESIAN_POINT ( 'NONE',  ( 5.844095810701279703, 1409.117140709990053, 195.3369297680639818 ) ) ;
#81127 = CARTESIAN_POINT ( 'NONE',  ( 5.992819232552546005, 1413.913060387330006, 220.0916279853276762 ) ) ;
#81128 = CARTESIAN_POINT ( 'NONE',  ( 2.523331955360000212, 1419.463757169429982, 185.1820755668979643 ) ) ;
#81129 = EDGE_CURVE ( 'NONE', #81525, #32285, #96188, .T. ) ;
#81130 = CARTESIAN_POINT ( 'NONE',  ( -18.83305916869999663, 1478.165930216330025, 189.8264731359980146 ) ) ;
#81131 = CARTESIAN_POINT ( 'NONE',  ( -68.75983579849153671, 1379.748052159727195, 280.1905170100664577 ) ) ;
#81132 = AXIS2_PLACEMENT_3D ( 'NONE', #88923, #12209, #105183 ) ;
#81133 = CARTESIAN_POINT ( 'NONE',  ( -3.503066957091310218, 1450.087732454140223, 184.8680753463810049 ) ) ;
#81134 = ORIENTED_EDGE ( 'NONE', *, *, #19899, .F. ) ;
#81135 = ORIENTED_EDGE ( 'NONE', *, *, #50041, .F. ) ;
#81136 = EDGE_CURVE ( 'NONE', #103262, #108726, #87237, .T. ) ;
#81137 = CARTESIAN_POINT ( 'NONE',  ( 18.40343465886353513, 1525.402221411349501, 238.3904617729369306 ) ) ;
#81138 = CARTESIAN_POINT ( 'NONE',  ( -12.13275115633589962, 1416.073666499230058, 194.7976983533769726 ) ) ;
#81139 = CARTESIAN_POINT ( 'NONE',  ( -12.30998824179999929, 1434.241983831289872, 150.0643212511979812 ) ) ;
#81140 = B_SPLINE_CURVE_WITH_KNOTS ( 'NONE', 5,
 ( #25717, #82888, #91835, #101312, #102433, #42541 ),
 .UNSPECIFIED., .F., .F.,
 ( 6, 6 ),
 ( 0.000000000000000000, 1.000000000000000000 ),
 .UNSPECIFIED. ) ;
#81141 = CARTESIAN_POINT ( 'NONE',  ( -7.502908036863889723E-10, 1468.442909337529954, 249.6120660866809828 ) ) ;
#81142 = CARTESIAN_POINT ( 'NONE',  ( -20.56963670059100124, 1506.881352026369996, 190.4177983208670071 ) ) ;
#81143 = CARTESIAN_POINT ( 'NONE',  ( -24.39386434493582811, 1435.492275954125716, 137.6392133633064816 ) ) ;
#81144 = CARTESIAN_POINT ( 'NONE',  ( -109.1320112420000044, 1384.953741877159700, 311.2644403302589353 ) ) ;
#81145 = CARTESIAN_POINT ( 'NONE',  ( -19.15967863205523969, 1486.263174534858535, 189.4699138206827911 ) ) ;
#81146 = CARTESIAN_POINT ( 'NONE',  ( -9.830395177430000686, 1365.769828494180047, 207.6218459616989946 ) ) ;
#81147 = CYLINDRICAL_SURFACE ( 'NONE', #3667, 1.000000000000070166 ) ;
#81148 = CIRCLE ( 'NONE', #104420, 1.999999999999998668 ) ;
#81149 = CARTESIAN_POINT ( 'NONE',  ( 3.350338079455601026, 1523.604703353109699, 176.1628856388066708 ) ) ;
#81150 = B_SPLINE_CURVE_WITH_KNOTS ( 'NONE', 5,
 ( #3120, #72511, #52957, #96042, #53514, #37800, #36692, #29379, #10946, #78698, #106639, #45118 ),
 .UNSPECIFIED., .F., .F.,
 ( 6, 3, 3, 6 ),
 ( 0.000000000000000000, 0.1846806524304075159, 0.5540478659889513935, 1.000000000000000000 ),
 .UNSPECIFIED. ) ;
#81151 = CARTESIAN_POINT ( 'NONE',  ( -0.7559395363919990674, 1516.972341476009888, 207.9998125401569951 ) ) ;
#81152 = CARTESIAN_POINT ( 'NONE',  ( 11.95006413401319989, 1433.524393973229735, 149.8867095871329980 ) ) ;
#81153 = CARTESIAN_POINT ( 'NONE',  ( -13.62029002549420120, 1434.976853200989808, 148.9443457557660224 ) ) ;
#81154 = CARTESIAN_POINT ( 'NONE',  ( -8.299200653989998955, 1385.160822377860086, 218.6946808916390239 ) ) ;
#81155 = CARTESIAN_POINT ( 'NONE',  ( 1.546949757049999929, 1416.828042640230024, 190.2227907535979909 ) ) ;
#81156 = CARTESIAN_POINT ( 'NONE',  ( -8.881784196999999612E-15, 1443.913060387330006, 126.8032249175980155 ) ) ;
#81157 = CARTESIAN_POINT ( 'NONE',  ( -18.74294524797809913, 1488.344793556559807, 199.7614651361420215 ) ) ;
#81158 = ORIENTED_EDGE ( 'NONE', *, *, #11242, .T. ) ;
#81159 = CARTESIAN_POINT ( 'NONE',  ( 11.55307713589999885, 1412.346723009130073, 255.2309128184979556 ) ) ;
#81160 = CARTESIAN_POINT ( 'NONE',  ( -27.78146449870000012, 1508.131230135330043, 206.3146870670979922 ) ) ;
#81162 = CARTESIAN_POINT ( 'NONE',  ( 2.743693168446419660E-14, 1421.936573599349913, 238.0271386588229916 ) ) ;
#81161 = CARTESIAN_POINT ( 'NONE',  ( -10.91009346278590009, 1426.088824854960194, 92.74416427518930561 ) ) ;
#81163 = CARTESIAN_POINT ( 'NONE',  ( -5.000068473801503544, 1407.851922743381010, 270.1322175188799974 ) ) ;
#81164 = CARTESIAN_POINT ( 'NONE',  ( -24.33135486439999795, 1436.015388124420042, 216.3889742816580224 ) ) ;
#81165 = CARTESIAN_POINT ( 'NONE',  ( -0.7156643283900009367, 1487.058471442790051, 220.0700283026990007 ) ) ;
#81166 = CARTESIAN_POINT ( 'NONE',  ( -13.27254556637139338, 1414.941240495243619, 220.1937345174850975 ) ) ;
#81167 = CARTESIAN_POINT ( 'NONE',  ( 27.01382259529999885, 1450.681608749369843, 136.4483196305980073 ) ) ;
#81168 = ORIENTED_EDGE ( 'NONE', *, *, #8381, .F. ) ;
#81169 = CARTESIAN_POINT ( 'NONE',  ( 3.254127503250000331, 1396.026697023729866, 198.1014182944979893 ) ) ;
#81170 = CARTESIAN_POINT ( 'NONE',  ( 10.96015508933500016, 1512.830284628050094, 225.0317485278669949 ) ) ;
#81171 = DIRECTION ( 'NONE',  ( 0.000000000000000000, 0.000000000000000000, 1.000000000000000000 ) ) ;
#81172 = ORIENTED_EDGE ( 'NONE', *, *, #976, .T. ) ;
#81173 = ORIENTED_EDGE ( 'NONE', *, *, #8063, .F. ) ;
#81174 = CARTESIAN_POINT ( 'NONE',  ( -3.078458355159999993, 1384.635588543570066, 199.6791145954990156 ) ) ;
#81175 = CARTESIAN_POINT ( 'NONE',  ( -22.82027165193229834, 1409.709881720489875, 208.9770212787329910 ) ) ;
#81176 = ORIENTED_EDGE ( 'NONE', *, *, #65731, .T. ) ;
#81177 = CARTESIAN_POINT ( 'NONE',  ( 4.678149145594550085, 1508.611352722540005, 205.6342600828810134 ) ) ;
#81178 = CARTESIAN_POINT ( 'NONE',  ( -106.3126565290000087, 1379.599899938080171, 307.8895711306589646 ) ) ;
#81179 = CARTESIAN_POINT ( 'NONE',  ( -2.040341087039999834, 1470.484922564130102, 235.4172632116979855 ) ) ;
#81180 = DIRECTION ( 'NONE',  ( -0.6736849260863839728, 0.000000000000000000, 0.7390186874254150995 ) ) ;
#81181 = ORIENTED_EDGE ( 'NONE', *, *, #43961, .F. ) ;
#81182 = CARTESIAN_POINT ( 'NONE',  ( 11.73645620740000162, 1426.280382981230105, 144.1655706652979632 ) ) ;
#81183 = CARTESIAN_POINT ( 'NONE',  ( -13.15726446870029953, 1414.972329067380088, 220.5265291070639933 ) ) ;
#81184 = CARTESIAN_POINT ( 'NONE',  ( 14.27330718989999880, 1474.742293895330022, 225.2716373713979863 ) ) ;
#81185 = CARTESIAN_POINT ( 'NONE',  ( -2.877113108595000135, 1516.697242742309982, 204.1252037719370094 ) ) ;
#81186 = ORIENTED_EDGE ( 'NONE', *, *, #45621, .T. ) ;
#81187 = FACE_OUTER_BOUND ( 'NONE', #46208, .T. ) ;
#81188 = CARTESIAN_POINT ( 'NONE',  ( -4.500000000000000000, 1448.210448412289907, 183.1418046154980175 ) ) ;
#81189 = ORIENTED_EDGE ( 'NONE', *, *, #60296, .F. ) ;
#81190 = ORIENTED_EDGE ( 'NONE', *, *, #49492, .T. ) ;
#81191 = CARTESIAN_POINT ( 'NONE',  ( 2.314969334973882464, 1525.402221411349956, 174.6257708845645595 ) ) ;
#81192 = CARTESIAN_POINT ( 'NONE',  ( -2.134361597679850231, 1508.551704408389924, 220.0638607491889900 ) ) ;
#81193 = CARTESIAN_POINT ( 'NONE',  ( 12.70677192039999959, 1507.773872374229995, 233.3565881929980037 ) ) ;
#81194 = CARTESIAN_POINT ( 'NONE',  ( -13.13649031037390102, 1512.464953430890091, 193.8649562899759928 ) ) ;
#81195 = CARTESIAN_POINT ( 'NONE',  ( 3.968827103902559550, 1522.051704408389924, 188.7040005461919918 ) ) ;
#81196 = CARTESIAN_POINT ( 'NONE',  ( 8.309581502480000381, 1421.353511227099943, 196.1914330872990035 ) ) ;
#81197 = DIRECTION ( 'NONE',  ( -0.4875821524125462103, 0.8726613282937071281, 0.02694161742381519925 ) ) ;
#81198 = DIRECTION ( 'NONE',  ( 0.9824080081115887930, -2.243614313870717968E-31, 0.1867471702549210744 ) ) ;
#81199 = DIRECTION ( 'NONE',  ( -0.9054006440294158908, 0.3019905698272229433, 0.2984147609059379924 ) ) ;
#81200 = TOROIDAL_SURFACE ( 'NONE', #49025, 8.500000000000000000, 1.500000000000000000 ) ;
#81201 = CARTESIAN_POINT ( 'NONE',  ( 0.02695769203707745407, 1409.103991128304187, 232.4957075236154083 ) ) ;
#81203 = FACE_OUTER_BOUND ( 'NONE', #94820, .T. ) ;
#81202 = CARTESIAN_POINT ( 'NONE',  ( 29.86461515634905695, 1525.960063244517187, 197.2746849027936378 ) ) ;
#81204 = CARTESIAN_POINT ( 'NONE',  ( -52.42853552574362652, 1379.742143312621693, 249.9106425968767553 ) ) ;
#81205 = CARTESIAN_POINT ( 'NONE',  ( -9.758464371257050018, 1440.110776583330107, 206.8639830241129971 ) ) ;
#81206 = CARTESIAN_POINT ( 'NONE',  ( -6.013894009214999947, 1511.644799026709961, 201.1705823216470037 ) ) ;
#81207 = EDGE_LOOP ( 'NONE', ( #46359, #69588, #10724, #75828, #18228 ) ) ;
#81208 = CARTESIAN_POINT ( 'NONE',  ( 5.969073325650000150, 1428.313923095629889, 209.1218459616979999 ) ) ;
#81209 = AXIS2_PLACEMENT_3D ( 'NONE', #80039, #44803, #105808 ) ;
#81210 = CARTESIAN_POINT ( 'NONE',  ( -11.43740528939994405, 1425.481182534629852, 144.1672625331937923 ) ) ;
#81211 = CARTESIAN_POINT ( 'NONE',  ( -99.13733263931901263, 1384.948377550129862, 310.7311109629659427 ) ) ;
#81212 = B_SPLINE_SURFACE_WITH_KNOTS ( 'NONE', 5, 5, ( 
 ( #65138, #99806, #6317, #74639, #100376, #15778 ),
 ( #91433, #57307, #14709, #48898, #90867, #98719 ),
 ( #109344, #23661, #66801, #32625, #100902, #39369 ),
 ( #14155, #57844, #49980, #84117, #90310, #7416 ),
 ( #91971, #72983, #73543, #107121, #21979, #56171 ),
 ( #13588, #47776, #107678, #30963, #99252, #48341 ),
 ( #82480, #16494, #31667, #101065, #49596, #65848 ),
 ( #83728, #84280, #41181, #57998, #42281, #68061 ),
 ( #75355, #32771, #7023, #66955, #93227, #24361 ) ),
 .UNSPECIFIED., .F., .F., .F.,
 ( 6, 3, 6 ),
 ( 6, 6 ),
 ( 11.24104702996040039, 18.80012749189999965, 23.52194917210970004 ),
 ( -0.0001008039396122149963, 2.000000000000000000 ),
 .UNSPECIFIED. ) ;
#81213 = CARTESIAN_POINT ( 'NONE',  ( -10.27296164000000012, 1387.820157591719862, 201.2959240949089974 ) ) ;
#81214 = DIRECTION ( 'NONE',  ( -0.000000000000000000, -1.000000000000000000, 0.000000000000000000 ) ) ;
#81216 = ORIENTED_EDGE ( 'NONE', *, *, #72721, .F. ) ;
#81215 = CARTESIAN_POINT ( 'NONE',  ( -5.976488786809999176, 1464.287555164190053, 199.8460616603990161 ) ) ;
#81217 = CARTESIAN_POINT ( 'NONE',  ( 5.508554876272072853, 1427.333971811663332, 137.0999999980980135 ) ) ;
#81218 = CARTESIAN_POINT ( 'NONE',  ( -0.8327748425420000711, 1442.756953654829886, 150.7628527808980152 ) ) ;
#81219 = CARTESIAN_POINT ( 'NONE',  ( -16.41680482819999654, 1416.781978129459958, 208.2739500234559955 ) ) ;
#81221 = EDGE_CURVE ( 'NONE', #70446, #28737, #96705, .T. ) ;
#81220 = CARTESIAN_POINT ( 'NONE',  ( -1.611085750247870152, 1429.654024655400008, 199.8738294952200079 ) ) ;
#81222 = CARTESIAN_POINT ( 'NONE',  ( 13.50445032983499871, 1512.655881406860090, 224.4988687930670039 ) ) ;
#81223 = CARTESIAN_POINT ( 'NONE',  ( 0.9855760050558128871, 1450.835604561619903, 181.4318144648370037 ) ) ;
#81224 = CARTESIAN_POINT ( 'NONE',  ( -41.15111457195003908, 1443.645559386717878, 136.9181535104192164 ) ) ;
#81225 = CARTESIAN_POINT ( 'NONE',  ( -10.03739716579999808, 1408.913060387329779, 223.8190696839980092 ) ) ;
#81226 = CARTESIAN_POINT ( 'NONE',  ( 15.24121254350000143, 1417.426114801229915, 227.6809794210979874 ) ) ;
#81227 = CARTESIAN_POINT ( 'NONE',  ( -19.63708787179571402, 1526.382868172863937, 234.8228066531185334 ) ) ;
#81228 = CARTESIAN_POINT ( 'NONE',  ( 1.118104729594999958, 1516.965971551240045, 206.8221779662269739 ) ) ;
#81229 = CARTESIAN_POINT ( 'NONE',  ( 45.48736378840000327, 1434.898499431709979, 266.6954231658979779 ) ) ;
#81230 = CARTESIAN_POINT ( 'NONE',  ( -17.72998244229999898, 1409.697166527829950, 224.1509371522980132 ) ) ;
#81231 = CARTESIAN_POINT ( 'NONE',  ( 20.10060672000000181, 1435.200054686760041, 143.0090892206980016 ) ) ;
#81232 = CARTESIAN_POINT ( 'NONE',  ( -1.120901768300000212, 1420.508728649429941, 228.2469200848979938 ) ) ;
#81233 = CARTESIAN_POINT ( 'NONE',  ( 29.75012120190000076, 1509.993914123429931, 209.6841247587719863 ) ) ;
#81234 = ADVANCED_FACE ( 'NONE', ( #55818 ), #74137, .T. ) ;
#81235 = CARTESIAN_POINT ( 'NONE',  ( 12.27010798620000109, 1416.835808399930102, 223.5795575983979973 ) ) ;
#81236 = CARTESIAN_POINT ( 'NONE',  ( -14.38719234011680115, 1417.088620461709979, 203.2501595028660120 ) ) ;
#81237 = CARTESIAN_POINT ( 'NONE',  ( -39.66821287261589646, 1439.813157609439941, 136.6894622735260043 ) ) ;
#81238 = CARTESIAN_POINT ( 'NONE',  ( 0.2164654389101900167, 1453.731855533950011, 183.2219979431039860 ) ) ;
#81239 = CARTESIAN_POINT ( 'NONE',  ( -8.468073032660511146, 1408.680955921970053, 220.2966634368420102 ) ) ;
#81240 = CARTESIAN_POINT ( 'NONE',  ( -0.2357814831160000291, 1418.572813431130044, 184.6863074503980044 ) ) ;
#81241 = CARTESIAN_POINT ( 'NONE',  ( 17.89234610336922771, 1523.611961620354123, 180.3157245011607017 ) ) ;
#81242 = ADVANCED_FACE ( 'NONE', ( #30587 ), #43275, .T. ) ;
#81243 = CARTESIAN_POINT ( 'NONE',  ( 0.8442079999446018279, 1484.559943106105948, 198.4446501219433969 ) ) ;
#81244 = CARTESIAN_POINT ( 'NONE',  ( 11.94131420200000093, 1433.615230264759930, 148.5014726782980006 ) ) ;
#81245 = CARTESIAN_POINT ( 'NONE',  ( -35.32500643234939730, 1435.854286985860199, 134.0999999975889807 ) ) ;
#81246 = CARTESIAN_POINT ( 'NONE',  ( 18.86688640473582268, 1512.187213306747481, 180.7825021045438803 ) ) ;
#81247 = ORIENTED_EDGE ( 'NONE', *, *, #103593, .F. ) ;
#81248 = CARTESIAN_POINT ( 'NONE',  ( 2.115055681410000332, 1476.785742702189964, 198.5761133783990147 ) ) ;
#81249 = CARTESIAN_POINT ( 'NONE',  ( -7.590886950367840669, 1409.178140000780104, 222.0180217246389986 ) ) ;
#81250 = CARTESIAN_POINT ( 'NONE',  ( -11.03560576459999965, 1491.884727983489938, 209.0941458228089971 ) ) ;
#81251 = CARTESIAN_POINT ( 'NONE',  ( 18.05542497264820057, 1416.825784014559986, 208.7596466293869923 ) ) ;
#81252 = CARTESIAN_POINT ( 'NONE',  ( -14.26885700313499861, 1464.825200350059959, 194.0278458552699874 ) ) ;
#81253 = CARTESIAN_POINT ( 'NONE',  ( 26.17821860987093530, 1412.906292311588231, 269.4265852173028861 ) ) ;
#81254 = CARTESIAN_POINT ( 'NONE',  ( 19.76254418480000297, 1434.994542537490133, 210.2414884005780209 ) ) ;
#81255 = CARTESIAN_POINT ( 'NONE',  ( 20.99191417935101711, 1509.583341918330689, 188.7493953713247663 ) ) ;
#81256 = CARTESIAN_POINT ( 'NONE',  ( -92.84358858088950228, 1384.613997830719882, 309.5363385667750435 ) ) ;
#81257 = CARTESIAN_POINT ( 'NONE',  ( -42.51724257030390675, 1384.996239121569943, 215.4468276199860099 ) ) ;
#81258 = CARTESIAN_POINT ( 'NONE',  ( -12.13697616928110001, 1490.926079256330240, 207.3467037448569954 ) ) ;
#81259 = CARTESIAN_POINT ( 'NONE',  ( -9.699660872752350116, 1472.030908259890111, 212.1562907213800031 ) ) ;
#81260 = CARTESIAN_POINT ( 'NONE',  ( -29.09134681210840156, 1509.695701326110111, 208.6729072386179951 ) ) ;
#81261 = CARTESIAN_POINT ( 'NONE',  ( 2.038646110889573038, 1525.960063244516959, 177.0579350083065435 ) ) ;
#81263 = ORIENTED_EDGE ( 'NONE', *, *, #70155, .F. ) ;
#81262 = FACE_OUTER_BOUND ( 'NONE', #70202, .T. ) ;
#81264 = CARTESIAN_POINT ( 'NONE',  ( -109.4837766770000087, 1384.913273580270015, 311.2841394952590122 ) ) ;
#81265 = CARTESIAN_POINT ( 'NONE',  ( 2.745142294599053567, 1419.769955103634175, 137.0999999980979567 ) ) ;
#81266 = ADVANCED_FACE ( 'NONE', ( #13761 ), #75954, .F. ) ;
#81267 = CARTESIAN_POINT ( 'NONE',  ( -11.19681733540000046, 1500.043629866090214, 211.1912691597789831 ) ) ;
#81268 = CARTESIAN_POINT ( 'NONE',  ( -12.37159932449999822, 1415.628674266529742, 195.6623782650979990 ) ) ;
#81269 = DIRECTION ( 'NONE',  ( -1.755985294532469921E-16, 1.000000000000000000, -1.338183447452831989E-16 ) ) ;
#81270 = CARTESIAN_POINT ( 'NONE',  ( 22.93207306500000087, 1410.635252800330136, 213.6236024351379967 ) ) ;
#81271 = CARTESIAN_POINT ( 'NONE',  ( -113.4000000000000057, 1304.231242809270043, 304.2218459572590064 ) ) ;
#81272 = CARTESIAN_POINT ( 'NONE',  ( -16.49003115520000051, 1466.602378028289877, 220.8807112456989898 ) ) ;
#81273 = CARTESIAN_POINT ( 'NONE',  ( -5.383700104412980636, 1431.668365950359885, 154.5770934270130113 ) ) ;
#81275 = CARTESIAN_POINT ( 'NONE',  ( -10.78481250609999975, 1379.886398380170021, 203.0395362228890122 ) ) ;
#81274 = CARTESIAN_POINT ( 'NONE',  ( -11.30340071049999828, 1432.444836995149899, 151.5218617844980145 ) ) ;
#81276 = CARTESIAN_POINT ( 'NONE',  ( 27.69051024323239929, 1508.175440098090121, 207.6659959044340269 ) ) ;
#81277 = CARTESIAN_POINT ( 'NONE',  ( -113.4000000000000057, 1371.894749952190068, 291.3379631701589574 ) ) ;
#81278 = CARTESIAN_POINT ( 'NONE',  ( 25.78167222729700114, 1509.813387082529971, 195.1140727163279962 ) ) ;
#81279 = CARTESIAN_POINT ( 'NONE',  ( -1.846469602520000253, 1415.927399473230025, 233.0908749537980214 ) ) ;
#81280 = AXIS2_PLACEMENT_3D ( 'NONE', #82164, #74350, #64296 ) ;
#81281 = CARTESIAN_POINT ( 'NONE',  ( 9.671060821790000261, 1366.060403940050037, 210.6218459616991936 ) ) ;
#81282 = CARTESIAN_POINT ( 'NONE',  ( -2.878693287274999957, 1516.766397346390022, 205.0941487061870134 ) ) ;
#81283 = CARTESIAN_POINT ( 'NONE',  ( -11.28228388660000014, 1484.392611670030192, 185.3973464570979957 ) ) ;
#81284 = VERTEX_POINT ( 'NONE', #91596 ) ;
#81285 = AXIS2_PLACEMENT_3D ( 'NONE', #10457, #78772, #79883 ) ;
#81286 = CARTESIAN_POINT ( 'NONE',  ( 11.32068957845180002, 1502.651254573290089, 211.1497440136959938 ) ) ;
#81287 = CARTESIAN_POINT ( 'NONE',  ( -4.283151062209100246, 1440.965633392529980, 156.0301116215779871 ) ) ;
#81288 = TOROIDAL_SURFACE ( 'NONE', #75947, 7.499828603750000156, 0.5000000000000000000 ) ;
#81290 = VERTEX_POINT ( 'NONE', #90486 ) ;
#81289 = CARTESIAN_POINT ( 'NONE',  ( -67.64859488819530497, 1379.745247417349901, 278.9922900543069773 ) ) ;
#81291 = ORIENTED_EDGE ( 'NONE', *, *, #61639, .F. ) ;
#81292 = CARTESIAN_POINT ( 'NONE',  ( 28.45308972519999813, 1509.159845678430202, 209.4525048039269848 ) ) ;
#81293 = ORIENTED_EDGE ( 'NONE', *, *, #40526, .F. ) ;
#81294 = CARTESIAN_POINT ( 'NONE',  ( -21.50400446119279962, 1505.467562055609960, 209.6175409707290100 ) ) ;
#81295 = CARTESIAN_POINT ( 'NONE',  ( 12.17073512129999990, 1499.730396594889726, 205.6506568158590085 ) ) ;
#81297 = FACE_OUTER_BOUND ( 'NONE', #68683, .T. ) ;
#81296 = CARTESIAN_POINT ( 'NONE',  ( 15.85018817003589930, 1416.524830770489871, 191.3417815159440067 ) ) ;
#81298 = CARTESIAN_POINT ( 'NONE',  ( -1.119592219845000125, 1516.958737650239982, 210.2577447559170025 ) ) ;
#81299 = CARTESIAN_POINT ( 'NONE',  ( -24.69498610859029952, 1451.810891097460171, 137.2013499168999999 ) ) ;
#81300 = CARTESIAN_POINT ( 'NONE',  ( -107.2277229851110008, 1378.913060387289988, 307.4948507977209715 ) ) ;
#81301 = CARTESIAN_POINT ( 'NONE',  ( 11.95779796459999922, 1409.330635893630188, 227.4564908493979942 ) ) ;
#81302 = CARTESIAN_POINT ( 'NONE',  ( 11.40628762099720106, 1480.472364249699922, 212.2078988420369967 ) ) ;
#81303 = APPLICATION_PROTOCOL_DEFINITION ( 'draft international standard', 'automotive_design', 1998, #93479 ) ;
#81304 = CARTESIAN_POINT ( 'NONE',  ( 40.49955491180480038, 1447.865363690810000, 134.0999999983799853 ) ) ;
#81305 = CARTESIAN_POINT ( 'NONE',  ( -40.17672711025409882, 1442.495956272649892, 136.9880589186049917 ) ) ;
#81306 = ORIENTED_EDGE ( 'NONE', *, *, #29894, .F. ) ;
#81307 = CARTESIAN_POINT ( 'NONE',  ( 13.80540804498470031, 1434.979597930440150, 148.5369051581390067 ) ) ;
#81308 = CARTESIAN_POINT ( 'NONE',  ( -10.81222349729999976, 1391.793768475530214, 204.0084625770589923 ) ) ;
#81309 = EDGE_LOOP ( 'NONE', ( #6386, #515, #85974, #82637 ) ) ;
#81310 = ORIENTED_EDGE ( 'NONE', *, *, #19177, .T. ) ;
#81311 = CARTESIAN_POINT ( 'NONE',  ( -6.834484321545000185, 1513.760531203570054, 216.6429190012370043 ) ) ;
#81312 = CARTESIAN_POINT ( 'NONE',  ( 31.93049531883788816, 1525.394081235439444, 217.0185068061728941 ) ) ;
#81313 = CARTESIAN_POINT ( 'NONE',  ( 0.3919105056819999766, 1450.899374570899909, 181.2708612515980064 ) ) ;
#81314 = CARTESIAN_POINT ( 'NONE',  ( -18.43525369369999822, 1507.707328976990084, 209.4281662339789705 ) ) ;
#81315 = CARTESIAN_POINT ( 'NONE',  ( -15.52964687406499955, 1451.324136384999974, 222.4830579234560162 ) ) ;
#81316 = CARTESIAN_POINT ( 'NONE',  ( -66.36196940094187369, 1379.742730262553778, 275.1157302125421893 ) ) ;
#81317 = DIRECTION ( 'NONE',  ( -5.980589973904019347E-17, 1.000000000000000000, -1.736889445713099699E-16 ) ) ;
#81318 = AXIS2_PLACEMENT_3D ( 'NONE', #89284, #63034, #12029 ) ;
#81319 = CARTESIAN_POINT ( 'NONE',  ( 28.27930517080000072, 1508.150008669530052, 208.9705538469389978 ) ) ;
#81320 = CARTESIAN_POINT ( 'NONE',  ( 1.487492019119999842, 1415.934222461130048, 190.4277445559980038 ) ) ;
#81321 = CARTESIAN_POINT ( 'NONE',  ( -60.61372366948459955, 1384.676785248499982, 245.3352954287460079 ) ) ;
#81322 = ORIENTED_EDGE ( 'NONE', *, *, #30133, .T. ) ;
#81323 = CARTESIAN_POINT ( 'NONE',  ( 4.026614479655000522, 1516.699825673279975, 207.4075116849170115 ) ) ;
#81324 = ORIENTED_EDGE ( 'NONE', *, *, #26072, .F. ) ;
#81325 = CARTESIAN_POINT ( 'NONE',  ( 11.36018337630000019, 1414.996442546230128, 222.2791104318980047 ) ) ;
#81326 = CARTESIAN_POINT ( 'NONE',  ( 19.34465229990000168, 1467.203108048530112, 226.8433508900980087 ) ) ;
#81327 = ORIENTED_EDGE ( 'NONE', *, *, #68470, .F. ) ;
#81328 = CARTESIAN_POINT ( 'NONE',  ( -17.37724426307464753, 1525.394057003702756, 181.1943177926724502 ) ) ;
#81329 = CARTESIAN_POINT ( 'NONE',  ( -15.60376662210000198, 1409.457955924729958, 192.7658650750980200 ) ) ;
#81330 = DIRECTION ( 'NONE',  ( 0.000000000000000000, 0.000000000000000000, -1.000000000000000000 ) ) ;
#81331 = CIRCLE ( 'NONE', #84915, 27.00880975787848470 ) ;
#81332 = CARTESIAN_POINT ( 'NONE',  ( 8.268934410249999090, 1502.576082311989921, 209.2129076204989815 ) ) ;
#81333 = CARTESIAN_POINT ( 'NONE',  ( 22.53878404599999641, 1411.058442739730026, 206.1986151668880041 ) ) ;
#81334 = CARTESIAN_POINT ( 'NONE',  ( -5.972112790866080267, 1511.562335007999991, 200.3290730311999823 ) ) ;
#81335 = CARTESIAN_POINT ( 'NONE',  ( 3.426893344479999826, 1406.086097517129929, 266.9564242903979903 ) ) ;
#81336 = CARTESIAN_POINT ( 'NONE',  ( -11.87576731660000107, 1433.006546870060220, 147.1501944259979950 ) ) ;
#81337 = CARTESIAN_POINT ( 'NONE',  ( 26.73888307210470217, 1505.237121714349769, 206.2308591485389968 ) ) ;
#81339 = CARTESIAN_POINT ( 'NONE',  ( -11.60004869885203682, 1423.633889434096545, 135.8155558197614141 ) ) ;
#81338 = CARTESIAN_POINT ( 'NONE',  ( 15.72885894491134806, 1409.636817080781157, 192.2423624785494951 ) ) ;
#81340 = B_SPLINE_SURFACE_WITH_KNOTS ( 'NONE', 5, 1, ( 
 ( #54315, #87908 ),
 ( #3360, #106878 ),
 ( #89535, #12269 ),
 ( #64359, #11197 ),
 ( #54857, #20123 ),
 ( #71690, #45361 ) ),
 .UNSPECIFIED., .F., .F., .F.,
 ( 6, 6 ),
 ( 2, 2 ),
 ( 0.000000000000000000, 16.10685270580000150 ),
 ( 0.000000000000000000, 14.00000000000000000 ),
 .UNSPECIFIED. ) ;
#81341 = CARTESIAN_POINT ( 'NONE',  ( -4.615017365965000451, 1516.987478262539980, 215.6816440265270103 ) ) ;
#81342 = CYLINDRICAL_SURFACE ( 'NONE', #74839, 2.000000000000003553 ) ;
#81343 = CARTESIAN_POINT ( 'NONE',  ( -0.1321621631135420083, 1507.857770132879978, 180.7250568012690053 ) ) ;
#81344 = CARTESIAN_POINT ( 'NONE',  ( 19.12881724366919300, 1443.878319859672729, 213.6723730806366461 ) ) ;
#81345 = CARTESIAN_POINT ( 'NONE',  ( -6.547881413045000265, 1516.647534046129977, 212.5778533554070293 ) ) ;
#81346 = CARTESIAN_POINT ( 'NONE',  ( -19.13335938739999875, 1434.810047171619999, 208.8572077783250052 ) ) ;
#81347 = CARTESIAN_POINT ( 'NONE',  ( 29.30029655192936033, 1525.907212628473644, 221.3719603026171967 ) ) ;
#81349 = ORIENTED_EDGE ( 'NONE', *, *, #30231, .F. ) ;
#81348 = DIRECTION ( 'NONE',  ( 3.828568698926945491E-16, 0.000000000000000000, -1.000000000000000000 ) ) ;
#81350 = CARTESIAN_POINT ( 'NONE',  ( -19.97269067359999895, 1507.847566760029849, 229.1287437625980203 ) ) ;
#81351 = CARTESIAN_POINT ( 'NONE',  ( 3.965904004230000002, 1461.348673275530018, 221.5631610770980160 ) ) ;
#81352 = CARTESIAN_POINT ( 'NONE',  ( -11.75013601680000086, 1430.854277466529766, 150.6431448726979738 ) ) ;
#81353 = CARTESIAN_POINT ( 'NONE',  ( -20.69303424980000372, 1486.764600954290017, 209.1218459616989946 ) ) ;
#81354 = CARTESIAN_POINT ( 'NONE',  ( 2.668065388650000092, 1415.928191210829937, 231.9156402769980048 ) ) ;
#81355 = DIRECTION ( 'NONE',  ( -0.6736849260863841948, 0.000000000000000000, 0.7390186874254148774 ) ) ;
#81356 = B_SPLINE_CURVE_WITH_KNOTS ( 'NONE', 3,
 ( #40634, #23814, #7032, #75362, #25464, #23269, #83737, #76441, #33880, #24904 ),
 .UNSPECIFIED., .F., .F.,
 ( 4, 2, 2, 2, 4 ),
 ( 0.000000000000000000, 0.0007189769279725903399, 0.001437953855945180680, 0.002156930783917771020, 0.002875907711890361360 ),
 .UNSPECIFIED. ) ;
#81357 = CIRCLE ( 'NONE', #109994, 2.000000000000001776 ) ;
#81358 = FACE_OUTER_BOUND ( 'NONE', #78391, .T. ) ;
#81360 = CARTESIAN_POINT ( 'NONE',  ( 5.376760986923570407, 1429.759527328420063, 154.2914800372689967 ) ) ;
#81359 = CARTESIAN_POINT ( 'NONE',  ( -21.38271991759999935, 1444.798061961909980, 221.4370072385979995 ) ) ;
#81361 = DIRECTION ( 'NONE',  ( -0.8090169943749467851, 5.613683090426285025E-15, -0.5877852522924740253 ) ) ;
#81362 = ORIENTED_EDGE ( 'NONE', *, *, #13060, .T. ) ;
#81363 = CARTESIAN_POINT ( 'NONE',  ( 7.711550677984999602, 1516.630499592039996, 205.0863552195469879 ) ) ;
#81364 = CARTESIAN_POINT ( 'NONE',  ( 0.7690095136829999678, 1406.511333993930066, 269.4984834021980191 ) ) ;
#81365 = AXIS2_PLACEMENT_3D ( 'NONE', #48215, #109220, #14024 ) ;
#81366 = CARTESIAN_POINT ( 'NONE',  ( -1.454938208119999965, 1515.064792882589927, 213.4512947377390049 ) ) ;
#81367 = CARTESIAN_POINT ( 'NONE',  ( 22.31666139102123481, 1430.631687695787832, 217.4689210016930474 ) ) ;
#81368 = CARTESIAN_POINT ( 'NONE',  ( -26.33484430150000222, 1451.993449299329768, 134.9650937070979921 ) ) ;
#81369 = CARTESIAN_POINT ( 'NONE',  ( 11.60004869885203682, 1425.163358000256721, 137.9635521539829313 ) ) ;
#81370 = CARTESIAN_POINT ( 'NONE',  ( -2.501005686574460096, 1448.957422176130194, 154.2481697560310181 ) ) ;
#81371 = CARTESIAN_POINT ( 'NONE',  ( -12.42723113640000143, 1446.757544803429937, 187.7007663958980004 ) ) ;
#81372 = CARTESIAN_POINT ( 'NONE',  ( -16.75801468479999912, 1408.913060387329779, 215.6757456486180047 ) ) ;
#81373 = CARTESIAN_POINT ( 'NONE',  ( -2.137141269540000277, 1508.158423200389961, 220.7965104394990021 ) ) ;
#81374 = CARTESIAN_POINT ( 'NONE',  ( -4.274333237420000486, 1515.341807516890185, 210.5964949952889924 ) ) ;
#81375 = CARTESIAN_POINT ( 'NONE',  ( -27.19819525569999996, 1434.390360740969982, 248.0989693098979956 ) ) ;
#81376 = DIRECTION ( 'NONE',  ( -6.922360974429999144E-17, -1.000000000000000000, 2.302693041820029802E-16 ) ) ;
#81377 = CARTESIAN_POINT ( 'NONE',  ( 2.500000000000000000, 1439.447172965609980, 162.2861354707980013 ) ) ;
#81378 = CARTESIAN_POINT ( 'NONE',  ( -6.194945185159999923, 1475.672627291929984, 267.2191845881980043 ) ) ;
#81379 = DIRECTION ( 'NONE',  ( -0.000000000000000000, -1.000000000000000000, -0.000000000000000000 ) ) ;
#81380 = CARTESIAN_POINT ( 'NONE',  ( 0.000000000000000000, 1524.340287715038357, 209.1218459616979999 ) ) ;
#81381 = DIRECTION ( 'NONE',  ( -0.9125304618754029873, 0.000000000000000000, -0.4090087482554177756 ) ) ;
#81382 = CARTESIAN_POINT ( 'NONE',  ( -36.40840158213870126, 1384.803230251859986, 236.2568994546979866 ) ) ;
#81383 = CARTESIAN_POINT ( 'NONE',  ( -4.095224926770001161, 1416.176064121729951, 162.4091932246979866 ) ) ;
#81384 = CARTESIAN_POINT ( 'NONE',  ( -105.3073167809999973, 1379.015836308379903, 304.0377958964590448 ) ) ;
#81385 = CARTESIAN_POINT ( 'NONE',  ( 32.35368859299575206, 1524.871836253796118, 217.0491380271198807 ) ) ;
#81386 = CARTESIAN_POINT ( 'NONE',  ( 8.609269427741782721, 1511.418041552835120, 203.8636807336108063 ) ) ;
#81387 = CIRCLE ( 'NONE', #51045, 0.4999999999999449329 ) ;
#81388 = CARTESIAN_POINT ( 'NONE',  ( -9.624269588760540728, 1396.249147287179994, 214.5727258578990018 ) ) ;
#81389 = CARTESIAN_POINT ( 'NONE',  ( -15.20173261459999914, 1421.117185528429900, 227.1213815240980125 ) ) ;
#81390 = CARTESIAN_POINT ( 'NONE',  ( 19.71200401973678140, 1455.391961128802677, 226.0432321991784477 ) ) ;
#81391 = VERTEX_POINT ( 'NONE', #77421 ) ;
#81392 = DIRECTION ( 'NONE',  ( 0.000000000000000000, -1.000000000000000000, 0.000000000000000000 ) ) ;
#81393 = CARTESIAN_POINT ( 'NONE',  ( -13.58621515471660146, 1508.473582053489963, 209.9518858487339799 ) ) ;
#81394 = AXIS2_PLACEMENT_3D ( 'NONE', #71351, #79177, #10285 ) ;
#81395 = FACE_OUTER_BOUND ( 'NONE', #42704, .T. ) ;
#81397 = CARTESIAN_POINT ( 'NONE',  ( -12.49293100206499929, 1511.939906524110256, 193.6511072290670086 ) ) ;
#81396 = CARTESIAN_POINT ( 'NONE',  ( 10.59099531070000033, 1425.359974359930220, 108.0493016666979855 ) ) ;
#81398 = DIRECTION ( 'NONE',  ( 0.000000000000000000, 1.000000000000000000, 0.000000000000000000 ) ) ;
#81399 = CARTESIAN_POINT ( 'NONE',  ( -5.183066490639999913, 1453.381677452690155, 200.4630107504189880 ) ) ;
#81400 = CARTESIAN_POINT ( 'NONE',  ( -6.943602691585000208, 1516.858069504249897, 202.1807456543569685 ) ) ;
#81401 = CARTESIAN_POINT ( 'NONE',  ( 8.051697842710000330, 1428.206416439490113, 213.2401734540090104 ) ) ;
#81402 = CARTESIAN_POINT ( 'NONE',  ( 22.24401329409999661, 1475.958617299990010, 209.7631870919539949 ) ) ;
#81403 = CARTESIAN_POINT ( 'NONE',  ( 3.220346732419999913, 1507.711646624130026, 181.3860254081980088 ) ) ;
#81404 = CARTESIAN_POINT ( 'NONE',  ( -20.14820771579280034, 1418.607677447980222, 207.2578463169909924 ) ) ;
#81405 = CARTESIAN_POINT ( 'NONE',  ( -61.17467505917599624, 1379.375923620560116, 270.9160354019339820 ) ) ;
#81406 = CARTESIAN_POINT ( 'NONE',  ( 7.721792848913118235, 1365.509929565264883, 208.3718459617061285 ) ) ;
#81408 = ORIENTED_EDGE ( 'NONE', *, *, #55623, .T. ) ;
#81407 = CARTESIAN_POINT ( 'NONE',  ( 8.810583203269999331, 1453.517925901990111, 213.4503995737389914 ) ) ;
#81409 = VERTEX_POINT ( 'NONE', #47945 ) ;
#81410 = CARTESIAN_POINT ( 'NONE',  ( -11.60590866750000139, 1396.839197833930029, 203.5249495555179919 ) ) ;
#81411 = CARTESIAN_POINT ( 'NONE',  ( -3.487592467065000257, 1509.038615934169911, 213.6090957241370063 ) ) ;
#81412 = DIRECTION ( 'NONE',  ( 0.000000000000000000, 1.000000000000000000, 0.000000000000000000 ) ) ;
#81413 = CARTESIAN_POINT ( 'NONE',  ( -12.54683716722921893, 1445.050387070945590, 169.4738468618211016 ) ) ;
#81414 = CARTESIAN_POINT ( 'NONE',  ( -15.20522052231627441, 1435.028466183189721, 147.6080187111736279 ) ) ;
#81415 = CARTESIAN_POINT ( 'NONE',  ( -14.93718008229999938, 1416.181292664740113, 212.9156384192889959 ) ) ;
#81416 =( BOUNDED_SURFACE ( )  B_SPLINE_SURFACE ( 3, 2, ( 
 ( #62704, #53169, #88410 ),
 ( #80565, #45876, #106310 ),
 ( #20624, #78356, #27953 ),
 ( #95707, #70539, #44213 ),
 ( #29594, #87880, #45330 ),
 ( #87311, #1665, #37458 ) ),
 .UNSPECIFIED., .F., .F., .F. ) 
 B_SPLINE_SURFACE_WITH_KNOTS ( ( 4, 2, 4 ),
 ( 3, 3 ),
 ( -5.095750210681870840E-17, 0.001312027981647294166, 0.002624055963294639506 ),
 ( 0.000000000000000000, 1.000000000000000000 ),
 .UNSPECIFIED. ) 
 GEOMETRIC_REPRESENTATION_ITEM ( )  RATIONAL_B_SPLINE_SURFACE ( (
 ( 1.000000000000000000, 0.9376006582765910036, 1.000000000000000000),
 ( 1.000000000000000000, 0.9569320108024047533, 1.000000000000000000),
 ( 1.000000000000000000, 0.9725743441616951923, 1.000000000000000000),
 ( 1.000000000000000000, 0.9942095667137571535, 1.000000000000000000),
 ( 1.000000000000000000, 1.000043666450562752, 1.000000000000000000),
 ( 1.000000000000000000, 1.000000000000000000, 1.000000000000000000) ) ) 
 REPRESENTATION_ITEM ( '' )  SURFACE ( )  );
#81418 = CARTESIAN_POINT ( 'NONE',  ( -1.360143013212020024, 1413.075073688769862, 185.4878003428050022 ) ) ;
#81417 = CARTESIAN_POINT ( 'NONE',  ( -8.860690249450000167, 1384.665722157209984, 218.6783682169690053 ) ) ;
#81419 = CARTESIAN_POINT ( 'NONE',  ( -30.31052258194605642, 1523.604703353109699, 195.7506062427372058 ) ) ;
#81420 = CARTESIAN_POINT ( 'NONE',  ( 13.15671565689999944, 1428.802034784529951, 222.6511392629980151 ) ) ;
#81421 = CARTESIAN_POINT ( 'NONE',  ( -40.61865684678500088, 1445.110985547599967, 136.9289262089600072 ) ) ;
#81422 = CARTESIAN_POINT ( 'NONE',  ( 9.293729047804200505, 1396.237604587079886, 203.1225184155669865 ) ) ;
#81423 = DIRECTION ( 'NONE',  ( -1.000000000000000000, 0.000000000000000000, 0.000000000000000000 ) ) ;
#81424 = CARTESIAN_POINT ( 'NONE',  ( 11.85151536849999943, 1431.322505881100142, 149.8924761066980125 ) ) ;
#81425 = FACE_OUTER_BOUND ( 'NONE', #94290, .T. ) ;
#81426 = VERTEX_POINT ( 'NONE', #58561 ) ;
#81427 = CARTESIAN_POINT ( 'NONE',  ( 3.970410702060000130, 1424.721377522129842, 185.1344166264979947 ) ) ;
#81428 = CARTESIAN_POINT ( 'NONE',  ( 12.88731009049999976, 1442.860943865789977, 187.0020155325980227 ) ) ;
#81429 = VERTEX_POINT ( 'NONE', #15419 ) ;
#81430 = EDGE_LOOP ( 'NONE', ( #11115, #95229, #17616, #7122 ) ) ;
#81431 = CARTESIAN_POINT ( 'NONE',  ( -18.78802005810790021, 1468.166114262229939, 227.9520744910329881 ) ) ;
#81432 = CARTESIAN_POINT ( 'NONE',  ( 9.231361398829999843, 1366.659448741839924, 207.6218459616989946 ) ) ;
#81433 = CARTESIAN_POINT ( 'NONE',  ( -14.45344520480000128, 1470.804162801829989, 194.2860277952979970 ) ) ;
#81434 = DIRECTION ( 'NONE',  ( -0.6736849260863841948, 0.000000000000000000, 0.7390186874254148774 ) ) ;
#81435 = CARTESIAN_POINT ( 'NONE',  ( -0.7376675409259989546, 1517.104497701820037, 214.9086937099069985 ) ) ;
#81436 = CARTESIAN_POINT ( 'NONE',  ( -22.75273496409615603, 1511.187213306747708, 183.6728937936775310 ) ) ;
#81437 = B_SPLINE_CURVE_WITH_KNOTS ( 'NONE', 5,
 ( #21646, #70044, #55854, #60522, #13247, #19021 ),
 .UNSPECIFIED., .F., .F.,
 ( 6, 6 ),
 ( 0.000000000000000000, 1.000000000000000000 ),
 .UNSPECIFIED. ) ;
#81438 = VERTEX_POINT ( 'NONE', #31681 ) ;
#81439 = CARTESIAN_POINT ( 'NONE',  ( -17.61823560201790073, 1508.551704408389924, 211.7175350862160315 ) ) ;
#81440 = CARTESIAN_POINT ( 'NONE',  ( -11.75444382587980030, 1509.419601378840071, 181.4412948336569968 ) ) ;
#81441 = CARTESIAN_POINT ( 'NONE',  ( -57.85314987360000316, 1379.895658628149931, 259.2190729278590311 ) ) ;
#81442 = ADVANCED_FACE ( 'NONE', ( #92689 ), #24055, .F. ) ;
#81443 = CONICAL_SURFACE ( 'NONE', #40287, 0.9999999999999857891, 0.7853981633970000820 ) ;
#81444 = EDGE_CURVE ( 'NONE', #59426, #48271, #17497, .T. ) ;
#81445 = CARTESIAN_POINT ( 'NONE',  ( 18.34777493720000408, 1415.426952350729835, 210.5090058238380095 ) ) ;
#81446 = CARTESIAN_POINT ( 'NONE',  ( 3.448206878685000198, 1516.904492006980036, 205.0794281543969646 ) ) ;
#81447 = ORIENTED_EDGE ( 'NONE', *, *, #53107, .F. ) ;
#81448 = CARTESIAN_POINT ( 'NONE',  ( -19.97269067359999895, 1507.847566760029849, 229.1287437625980203 ) ) ;
#81449 = ADVANCED_FACE ( 'NONE', ( #88589 ), #53911, .F. ) ;
#81450 = B_SPLINE_SURFACE_WITH_KNOTS ( 'NONE', 5, 5, ( 
 ( #110610, #52388, #69747, #44523, #27166, #1987 ),
 ( #51256, #17620, #18192, #9263, #77572, #61898 ),
 ( #85389, #84837, #34457, #26595, #86508, #18736 ),
 ( #43969, #33892, #879, #68633, #52931, #68088 ),
 ( #87065, #1411, #35003, #51824, #35552, #36122 ),
 ( #26028, #60792, #42866, #85963, #60224, #69182 ),
 ( #103866, #61350, #102200, #70306, #25480, #93782 ),
 ( #8685, #88731, #80328, #45094, #106074, #37221 ),
 ( #29354, #13088, #4174, #104972, #79234, #36668 ),
 ( #63019, #45648, #2543, #11473, #70861, #80876 ),
 ( #20394, #79788, #107168, #30460, #81396, #10919 ),
 ( #3644, #28261, #62455, #4708, #54054, #64645 ),
 ( #72485, #55695, #55147, #89268, #19286, #63555 ),
 ( #96578, #73030, #97670, #54598, #97125, #47273 ),
 ( #19850, #46745, #88181, #3093, #53487, #38851 ),
 ( #28822, #20942, #71418, #87631, #105533, #89816 ),
 ( #12014, #46194, #29900, #12564, #38304, #37773 ),
 ( #71964, #106614, #64092, #98214, #21482, #15296 ),
 ( #65735, #92025, #74141, #32119, #23149, #48943 ),
 ( #91477, #56224, #14756, #99300, #99854, #90916 ),
 ( #90355, #13633, #57352, #83074, #107723, #75242 ),
 ( #75780, #6909, #41065, #24253, #23705, #57889 ),
 ( #66304, #39965, #65188, #41626, #100422, #6367 ),
 ( #15831, #56778, #5263, #49488, #14201, #73594 ) ),
 .UNSPECIFIED., .F., .F., .F.,
 ( 6, 3, 3, 3, 3, 3, 3, 6 ),
 ( 6, 6 ),
 ( 14.55918620569999966, 19.99492494029999889, 25.43066367479999812, 36.30214114399999659, 58.04509608220000416, 73.63322306669999762, 84.29463333639999689, 89.22135005120000528 ),
 ( 0.000000000000000000, 2.069352078150000107 ),
 .UNSPECIFIED. ) ;
#81452 = EDGE_CURVE ( 'NONE', #36309, #76907, #44384, .T. ) ;
#81451 = CARTESIAN_POINT ( 'NONE',  ( -39.02150397496387768, 1429.577995707119726, 269.5933091914920396 ) ) ;
#81453 = CARTESIAN_POINT ( 'NONE',  ( -0.5238648979389999294, 1409.870336987230075, 233.1507188881979857 ) ) ;
#81455 = ORIENTED_EDGE ( 'NONE', *, *, #76651, .T. ) ;
#81454 = CARTESIAN_POINT ( 'NONE',  ( -10.22570915140000025, 1431.113060387329824, 192.7293421165980192 ) ) ;
#81456 = CARTESIAN_POINT ( 'NONE',  ( 2.500000000000000000, 1432.279053890430077, 157.4932346246980046 ) ) ;
#81457 = CARTESIAN_POINT ( 'NONE',  ( -32.01195192850000382, 1440.913060389299972, 244.1429064932979998 ) ) ;
#81458 = CARTESIAN_POINT ( 'NONE',  ( -59.24835266110000020, 1384.395332261929980, 279.9182260145590249 ) ) ;
#81459 = CARTESIAN_POINT ( 'NONE',  ( -0.2199937827443219918, 1465.432054623820250, 236.3155471839449717 ) ) ;
#81460 = CARTESIAN_POINT ( 'NONE',  ( 25.76377174109999757, 1414.047232564129899, 270.2932678871979988 ) ) ;
#81461 = CARTESIAN_POINT ( 'NONE',  ( -6.935133418554999096, 1516.613881697390070, 212.3834819030570031 ) ) ;
#81462 = CARTESIAN_POINT ( 'NONE',  ( -54.39340494969999895, 1379.701756400480008, 248.9505162619590237 ) ) ;
#81463 = CARTESIAN_POINT ( 'NONE',  ( 23.41495040159999874, 1410.123695770630093, 208.2164741116880009 ) ) ;
#81464 = CARTESIAN_POINT ( 'NONE',  ( 16.14386229810000017, 1410.940818424630152, 209.1133554891810036 ) ) ;
#81465 = CARTESIAN_POINT ( 'NONE',  ( 7.600903732925440082, 1425.252121065440178, 192.7969948842710153 ) ) ;
#81467 = CARTESIAN_POINT ( 'NONE',  ( -7.708852918845599866, 1516.527474870850256, 211.2226130665349899 ) ) ;
#81466 = CONICAL_SURFACE ( 'NONE', #35044, 26.99999999999999645, 0.2186689458740001812 ) ;
#81468 = CARTESIAN_POINT ( 'NONE',  ( -0.7374509209069979310, 1516.978425811520083, 210.2554991112269818 ) ) ;
#81469 = CARTESIAN_POINT ( 'NONE',  ( 4.384104894483219717, 1420.229028528550089, 185.7135937214090120 ) ) ;
#81471 = EDGE_CURVE ( 'NONE', #105885, #48821, #20291, .T. ) ;
#81470 = CARTESIAN_POINT ( 'NONE',  ( -0.6386371946080000583, 1415.383004098129959, 233.3563721401980047 ) ) ;
#81472 = CARTESIAN_POINT ( 'NONE',  ( -106.4197298790000019, 1384.588767362379940, 311.3121942672589739 ) ) ;
#81473 = ORIENTED_EDGE ( 'NONE', *, *, #107044, .F. ) ;
#81474 = CARTESIAN_POINT ( 'NONE',  ( -26.15713872745329738, 1385.250841378830046, 224.5366954647260229 ) ) ;
#81475 = CARTESIAN_POINT ( 'NONE',  ( 18.64618908219999938, 1416.835809767629826, 209.6841500801740210 ) ) ;
#81476 = CARTESIAN_POINT ( 'NONE',  ( 0.4646427325219999460, 1417.292090517329825, 234.8189226518980206 ) ) ;
#81477 = EDGE_CURVE ( 'NONE', #3936, #42483, #91324, .T. ) ;
#81478 = TOROIDAL_SURFACE ( 'NONE', #33209, 11.26398391340000060, 1.000000000000000000 ) ;
#81479 = CARTESIAN_POINT ( 'NONE',  ( 4.832616806509603791, 1508.551704408389924, 206.6339108634079196 ) ) ;
#81480 = CARTESIAN_POINT ( 'NONE',  ( 7.563688191785000292, 1510.983859056260144, 206.1910078925270113 ) ) ;
#81481 = EDGE_CURVE ( 'NONE', #508, #18362, #60375, .T. ) ;
#81482 = CARTESIAN_POINT ( 'NONE',  ( 11.09438297129999995, 1422.716151225649810, 205.9069650321689835 ) ) ;
#81483 = CARTESIAN_POINT ( 'NONE',  ( -3.202919937201420097, 1497.488146467896513, 198.3026830809020566 ) ) ;
#81485 = CARTESIAN_POINT ( 'NONE',  ( 18.10358820054819873, 1416.830086716310007, 209.0369172249700114 ) ) ;
#81484 = CARTESIAN_POINT ( 'NONE',  ( -2.290886304614999869, 1517.184383877180153, 216.4605998004670084 ) ) ;
#81486 = CARTESIAN_POINT ( 'NONE',  ( -11.00301372470000061, 1492.094802143589959, 210.0154403701209844 ) ) ;
#81487 = CARTESIAN_POINT ( 'NONE',  ( -11.28506483534210147, 1425.468559411955994, 139.1360102533408565 ) ) ;
#81488 = ORIENTED_EDGE ( 'NONE', *, *, #5135, .T. ) ;
#81489 = CARTESIAN_POINT ( 'NONE',  ( -1.708092304294999808, 1516.523379810429788, 201.4131002843170108 ) ) ;
#81490 = CARTESIAN_POINT ( 'NONE',  ( 10.37204961533650049, 1480.880553692909871, 207.1848069682540086 ) ) ;
#81491 = ORIENTED_EDGE ( 'NONE', *, *, #105655, .F. ) ;
#81492 = CARTESIAN_POINT ( 'NONE',  ( -15.87603345926501675, 1512.359593911809952, 220.1461273412669755 ) ) ;
#81493 = CARTESIAN_POINT ( 'NONE',  ( 23.11298832950000204, 1449.418514959970025, 217.9321843291079972 ) ) ;
#81494 = CARTESIAN_POINT ( 'NONE',  ( 10.95226140456819941, 1461.055140320559985, 208.9723413537100214 ) ) ;
#81495 = CARTESIAN_POINT ( 'NONE',  ( 8.637116716612862177, 1424.696483988998125, 195.7776412112969808 ) ) ;
#81496 = CARTESIAN_POINT ( 'NONE',  ( 1.940446769709999852, 1443.740569421090186, 217.8448552839390118 ) ) ;
#81497 = CARTESIAN_POINT ( 'NONE',  ( -28.08690426975079646, 1509.893876697129826, 200.8665688467620214 ) ) ;
#81498 = CARTESIAN_POINT ( 'NONE',  ( 5.580754349969999417, 1425.065972486529972, 185.9108535249980036 ) ) ;
#81499 = CARTESIAN_POINT ( 'NONE',  ( -18.82636944589999928, 1425.197040939629915, 224.5568828730980329 ) ) ;
#81500 = CARTESIAN_POINT ( 'NONE',  ( -31.48330081542915337, 1465.654837984586266, 269.3264367229945151 ) ) ;
#81501 = CARTESIAN_POINT ( 'NONE',  ( -107.6645298440000005, 1388.788267583639936, 298.6282682945589499 ) ) ;
#81502 = CARTESIAN_POINT ( 'NONE',  ( 18.91741685370000070, 1507.874522288630033, 188.5215471660979745 ) ) ;
#81504 = CARTESIAN_POINT ( 'NONE',  ( 29.28982057039999987, 1509.872724133429983, 209.1311963767199700 ) ) ;
#81503 = CARTESIAN_POINT ( 'NONE',  ( -0.004423692707904589884, 1409.421459607170164, 233.0174416772929931 ) ) ;
#81505 = CARTESIAN_POINT ( 'NONE',  ( -10.15838176937289994, 1472.546283077140060, 209.8695213180610040 ) ) ;
#81506 = EDGE_LOOP ( 'NONE', ( #38213, #65107, #69632, #44292 ) ) ;
#81507 =( NAMED_UNIT ( * ) PLANE_ANGLE_UNIT ( ) SI_UNIT ( $, .RADIAN. ) );
#81508 = CARTESIAN_POINT ( 'NONE',  ( -8.809401951759999960, 1508.551704408389924, 218.7286899463289842 ) ) ;
#81509 = CARTESIAN_POINT ( 'NONE',  ( 0.000000000000000000, 1414.421228241719973, 209.1218459616989946 ) ) ;
#81510 = CARTESIAN_POINT ( 'NONE',  ( 11.37384798555710042, 1470.779892333479893, 208.4801607157270098 ) ) ;
#81511 = CARTESIAN_POINT ( 'NONE',  ( -4.561655832029999580, 1453.313060387329870, 228.9334036006980000 ) ) ;
#81512 = CARTESIAN_POINT ( 'NONE',  ( 1.466938223877110037, 1489.323189782810005, 181.8892042488770073 ) ) ;
#81513 = CARTESIAN_POINT ( 'NONE',  ( 0.1439970023041980962, 1408.918088873463375, 231.7716143890593230 ) ) ;
#81514 = CARTESIAN_POINT ( 'NONE',  ( -13.21516149639446525, 1444.692096246350502, 186.6006968847816836 ) ) ;
#81515 = CARTESIAN_POINT ( 'NONE',  ( -3.286480964850000408, 1456.341185808290220, 218.0120306903490075 ) ) ;
#81516 = CARTESIAN_POINT ( 'NONE',  ( 5.312683756866860563, 1493.059111247549936, 218.8466363622630126 ) ) ;
#81517 = B_SPLINE_CURVE_WITH_KNOTS ( 'NONE', 5,
 ( #35722, #87803, #69910, #78843, #2154, #36829, #104583, #45807, #26200, #62059, #19459, #53659 ),
 .UNSPECIFIED., .F., .F.,
 ( 6, 3, 3, 6 ),
 ( 0.000000000000000000, 0.3019449542239004969, 0.7424883509937331150, 1.000000000000000000 ),
 .UNSPECIFIED. ) ;
#81518 = CARTESIAN_POINT ( 'NONE',  ( -8.888758267720000106, 1385.314821192629779, 218.6605176881890031 ) ) ;
#81519 = AXIS2_PLACEMENT_3D ( 'NONE', #28876, #89326, #44580 ) ;
#81520 = CARTESIAN_POINT ( 'NONE',  ( 17.60627569411529691, 1410.895669416499913, 224.1775087544040161 ) ) ;
#81521 = CIRCLE ( 'NONE', #83294, 1.999999999999998890 ) ;
#81522 = CARTESIAN_POINT ( 'NONE',  ( 17.85863899644585473, 1424.390786367949886, 228.2669348674518517 ) ) ;
#81523 = CARTESIAN_POINT ( 'NONE',  ( -0.9413364034040100359, 1516.673252337410077, 201.4091757340799802 ) ) ;
#81525 = VERTEX_POINT ( 'NONE', #22995 ) ;
#81524 = CARTESIAN_POINT ( 'NONE',  ( 22.78821502090000095, 1509.414782074829873, 192.0681064721979965 ) ) ;
#81526 = CARTESIAN_POINT ( 'NONE',  ( -109.9987473139999992, 1380.796323439529942, 299.4245717883589464 ) ) ;
#81527 = CARTESIAN_POINT ( 'NONE',  ( 12.42116344234460001, 1512.160613316490071, 224.0461796643650132 ) ) ;
#81528 = EDGE_LOOP ( 'NONE', ( #103176, #68004, #58863, #29525, #56619 ) ) ;
#81529 = EDGE_LOOP ( 'NONE', ( #6903, #3106, #46429, #64970 ) ) ;
#81530 = CARTESIAN_POINT ( 'NONE',  ( 17.78809123684730054, 1415.431750870129918, 209.6300319562920151 ) ) ;
#81531 = CARTESIAN_POINT ( 'NONE',  ( -109.8947179409999961, 1384.912517356189937, 297.0284612775590176 ) ) ;
#81532 = CARTESIAN_POINT ( 'NONE',  ( 17.69507376876702764, 1517.051704408389924, 202.0148427140983358 ) ) ;
#81534 = CARTESIAN_POINT ( 'NONE',  ( -10.53938673230000056, 1467.231892117930101, 248.5638781414980087 ) ) ;
#81533 = CARTESIAN_POINT ( 'NONE',  ( 37.96159890643052393, 1427.824381202910672, 269.5756791377570494 ) ) ;
#81535 = DIRECTION ( 'NONE',  ( 0.4090087482554383147, 0.000000000000000000, 0.9125304618753937724 ) ) ;
#81536 = CARTESIAN_POINT ( 'NONE',  ( -11.79562278360000072, 1433.595085838450132, 150.7745987806980281 ) ) ;
#81537 = EDGE_CURVE ( 'NONE', #56028, #96209, #55036, .T. ) ;
#81538 = CYLINDRICAL_SURFACE ( 'NONE', #8775, 1.999999999999999556 ) ;
#81539 = CARTESIAN_POINT ( 'NONE',  ( 11.68880576114610115, 1426.727712291149828, 140.7201426135219720 ) ) ;
#81540 = CARTESIAN_POINT ( 'NONE',  ( 26.04969316654200284, 1456.961035536420013, 209.5000640554989957 ) ) ;
#81541 = EDGE_CURVE ( 'NONE', #33454, #54701, #105581, .T. ) ;
#81542 = CARTESIAN_POINT ( 'NONE',  ( -25.77702438540000074, 1439.619448183560053, 137.8626266291980187 ) ) ;
#81543 = CARTESIAN_POINT ( 'NONE',  ( 0.7597457875069780764, 1515.127202858759802, 213.4496604749319886 ) ) ;
#81544 = CARTESIAN_POINT ( 'NONE',  ( 6.267127390599999792, 1440.453901950489808, 154.5142010626979925 ) ) ;
#81545 = CARTESIAN_POINT ( 'NONE',  ( -10.54669675879670088, 1479.991597968870110, 214.2917569529570017 ) ) ;
#81546 = CARTESIAN_POINT ( 'NONE',  ( -3.982247585420000124, 1360.759224656429978, 207.6218459616989946 ) ) ;
#81547 = CARTESIAN_POINT ( 'NONE',  ( 33.23421991949613385, 1522.906363951597314, 200.8294566360694660 ) ) ;
#81548 = AXIS2_PLACEMENT_3D ( 'NONE', #96248, #7142, #82746 ) ;
#81550 = ORIENTED_EDGE ( 'NONE', *, *, #52057, .F. ) ;
#81549 = CARTESIAN_POINT ( 'NONE',  ( 1.559404887145759819E-08, 1408.124151547700194, 262.7415101742070078 ) ) ;
#81551 = VERTEX_POINT ( 'NONE', #22429 ) ;
#81552 = CARTESIAN_POINT ( 'NONE',  ( -13.31088003390000019, 1503.456607311290099, 208.6977490917149964 ) ) ;
#81553 = CARTESIAN_POINT ( 'NONE',  ( 19.49044434509999846, 1499.602757397389723, 221.7314651344989898 ) ) ;
#81554 = CARTESIAN_POINT ( 'NONE',  ( -33.26587534239999400, 1460.596492508030224, 269.9719372418979901 ) ) ;
#81555 = CARTESIAN_POINT ( 'NONE',  ( -1.552659050370000182, 1415.628674276829770, 227.5866819053980237 ) ) ;
#81556 = FACE_OUTER_BOUND ( 'NONE', #23996, .T. ) ;
#81557 = CARTESIAN_POINT ( 'NONE',  ( -6.647330431358690284, 1517.051704408389924, 184.4413780136169976 ) ) ;
#81558 = ADVANCED_FACE ( 'NONE', ( #56631 ), #74915, .T. ) ;
#81559 = CARTESIAN_POINT ( 'NONE',  ( 0.2936830235118059740, 1451.092918877540114, 182.1143685304440112 ) ) ;
#81560 = CARTESIAN_POINT ( 'NONE',  ( -13.99060315449999869, 1420.944189322230159, 227.6471180683980151 ) ) ;
#81561 = CARTESIAN_POINT ( 'NONE',  ( 22.52609270013210008, 1509.699688878029974, 227.6602567939980020 ) ) ;
#81562 = CARTESIAN_POINT ( 'NONE',  ( -5.584473570009999221, 1458.593347104090071, 217.4064612629990165 ) ) ;
#81563 = CARTESIAN_POINT ( 'NONE',  ( 9.943976501839999926, 1365.461622992600041, 207.6218459616989946 ) ) ;
#81564 = CARTESIAN_POINT ( 'NONE',  ( -27.08062899747210039, 1413.352696219579911, 269.4117077479539830 ) ) ;
#81565 = ORIENTED_EDGE ( 'NONE', *, *, #102982, .T. ) ;
#81566 = CARTESIAN_POINT ( 'NONE',  ( -24.34268787264259970, 1442.549328851149994, 212.2035684885649687 ) ) ;
#81567 = ORIENTED_EDGE ( 'NONE', *, *, #29645, .F. ) ;
#81568 = ORIENTED_EDGE ( 'NONE', *, *, #45962, .T. ) ;
#81569 = CARTESIAN_POINT ( 'NONE',  ( 7.727327114725000001, 1517.232977404109988, 210.8318586907270173 ) ) ;
#81570 = CARTESIAN_POINT ( 'NONE',  ( 4.794874430321680592, 1423.553857172505786, 184.0667277509072903 ) ) ;
#81571 = EDGE_CURVE ( 'NONE', #94948, #59250, #70902, .T. ) ;
#81573 = CARTESIAN_POINT ( 'NONE',  ( -17.64146421497870065, 1419.304501645640130, 207.1873797621490212 ) ) ;
#81572 = CARTESIAN_POINT ( 'NONE',  ( 4.042729802795000715, 1516.919782530640077, 212.3762473738369749 ) ) ;
#81574 = CARTESIAN_POINT ( 'NONE',  ( -17.21788923599999777, 1425.427158435330057, 191.3819988649980246 ) ) ;
#81575 = CARTESIAN_POINT ( 'NONE',  ( -2.131094719222661027, 1450.051764141119293, 182.8883510409370956 ) ) ;
#81576 = ORIENTED_EDGE ( 'NONE', *, *, #102818, .T. ) ;
#81577 = CARTESIAN_POINT ( 'NONE',  ( -26.81198143800000011, 1435.984767782220160, 136.4831820118980090 ) ) ;
#81578 = EDGE_CURVE ( 'NONE', #108323, #60994, #90885, .T. ) ;
#81579 = EDGE_CURVE ( 'NONE', #97968, #101207, #53774, .T. ) ;
#81580 = CARTESIAN_POINT ( 'NONE',  ( 0.7396922377450010355, 1517.135701590510052, 201.7845486201169933 ) ) ;
#81581 = CARTESIAN_POINT ( 'NONE',  ( 10.70463268489999997, 1472.030523703590006, 213.2176825260490034 ) ) ;
#81582 = CARTESIAN_POINT ( 'NONE',  ( -10.02843955878900140, 1522.051704408389924, 185.3723613107750054 ) ) ;
#81583 = CARTESIAN_POINT ( 'NONE',  ( -42.06230555778069657, 1440.913045005490176, 269.6487386043370407 ) ) ;
#81584 = CARTESIAN_POINT ( 'NONE',  ( -17.30126322264655769, 1523.462669333492613, 180.8506073315049605 ) ) ;
#81585 = CARTESIAN_POINT ( 'NONE',  ( 0.08248930346060000252, 1397.911842041330146, 196.1221076645980190 ) ) ;
#81587 = ORIENTED_EDGE ( 'NONE', *, *, #108446, .F. ) ;
#81586 = CARTESIAN_POINT ( 'NONE',  ( -9.830395177430000686, 1365.769828494180047, 207.6218459616989946 ) ) ;
#81588 = EDGE_LOOP ( 'NONE', ( #66842, #75144, #62777, #55841 ) ) ;
#81589 = CARTESIAN_POINT ( 'NONE',  ( 45.63742906433166269, 1440.984662832818231, 268.9747442027135094 ) ) ;
#81590 = EDGE_CURVE ( 'NONE', #64454, #59255, #20078, .T. ) ;
#81591 = CARTESIAN_POINT ( 'NONE',  ( -1.272696501052200002, 1467.775668680739955, 220.1607310847500116 ) ) ;
#81592 = CARTESIAN_POINT ( 'NONE',  ( -2.499989269620250809, 1419.524750234567819, 137.1000002976804808 ) ) ;
#81593 = CARTESIAN_POINT ( 'NONE',  ( -2.446860876200000146, 1485.861696305629948, 182.3251189419979994 ) ) ;
#81594 = CARTESIAN_POINT ( 'NONE',  ( -0.7352271553329990939, 1516.963431999339946, 210.8369554172870153 ) ) ;
#81595 = ADVANCED_FACE ( 'NONE', ( #27980 ), #109016, .F. ) ;
#81596 = CARTESIAN_POINT ( 'NONE',  ( -68.77833046130001549, 1379.747972053160083, 280.2623328013589799 ) ) ;
#81597 = CARTESIAN_POINT ( 'NONE',  ( -18.17797837000000172, 1430.799045000430169, 226.0673535798979970 ) ) ;
#81598 = CARTESIAN_POINT ( 'NONE',  ( 6.202679998688561014, 1439.658092082629764, 216.9645777206339972 ) ) ;
#81599 = CARTESIAN_POINT ( 'NONE',  ( 11.95789827870000011, 1415.263254644630024, 222.5852371437979969 ) ) ;
#81600 = CARTESIAN_POINT ( 'NONE',  ( 8.016996057795001462, 1511.645462744430006, 205.6888706473769730 ) ) ;
#81601 = VERTEX_POINT ( 'NONE', #73299 ) ;
#81602 = CARTESIAN_POINT ( 'NONE',  ( 4.608417506514999928, 1516.691389976299888, 206.6316000176769876 ) ) ;
#81603 = EDGE_LOOP ( 'NONE', ( #26803, #27821 ) ) ;
#81604 = CARTESIAN_POINT ( 'NONE',  ( -36.37832870497099691, 1435.767865672210064, 135.0584844266200264 ) ) ;
#81605 = CARTESIAN_POINT ( 'NONE',  ( -22.86910817896174208, 1450.559972649895826, 218.2799029533455553 ) ) ;
#81606 = EDGE_LOOP ( 'NONE', ( #85202, #77686, #5004, #64607 ) ) ;
#81607 = CARTESIAN_POINT ( 'NONE',  ( 7.944299862241802401, 1456.350524190856049, 227.3938853663973987 ) ) ;
#81608 = B_SPLINE_CURVE_WITH_KNOTS ( 'NONE', 5,
 ( #24394, #15984, #14340, #101095, #33345, #22722 ),
 .UNSPECIFIED., .F., .F.,
 ( 6, 6 ),
 ( -1.455169987240000129, -1.489991576120175409E-06 ),
 .UNSPECIFIED. ) ;
#81609 = CARTESIAN_POINT ( 'NONE',  ( -2.813822098188480059, 1367.641464703512383, 209.1220808600859300 ) ) ;
#81610 = CARTESIAN_POINT ( 'NONE',  ( -4.094010558034039349, 1440.293265212250844, 185.3665320917685904 ) ) ;
#81611 = CARTESIAN_POINT ( 'NONE',  ( 2.424063131930000115, 1427.257651041929876, 147.9020499575979954 ) ) ;
#81612 = CARTESIAN_POINT ( 'NONE',  ( 22.31986392519999995, 1411.050752918829858, 204.7278403729679894 ) ) ;
#81613 = CARTESIAN_POINT ( 'NONE',  ( 16.57641946659999732, 1409.993768443630188, 226.3203854516980300 ) ) ;
#81614 = CARTESIAN_POINT ( 'NONE',  ( 32.23393008313274066, 1523.382868172864391, 201.4036600223104756 ) ) ;
#81615 = ADVANCED_FACE ( 'NONE', ( #90632 ), #13910, .T. ) ;
#81616 = DIRECTION ( 'NONE',  ( -0.3090169943749382919, 0.000000000000000000, 0.9510565162951565288 ) ) ;
#81617 = CARTESIAN_POINT ( 'NONE',  ( 24.56874431706803819, 1443.565273634055075, 213.1861617392668791 ) ) ;
#81618 = LINE ( 'NONE', #5477, #31638 ) ;
#81619 = CARTESIAN_POINT ( 'NONE',  ( 3.457266605394999637, 1516.691414181030041, 214.8945738789770132 ) ) ;
#81620 = EDGE_CURVE ( 'NONE', #47514, #93315, #76513, .T. ) ;
#81621 = ORIENTED_EDGE ( 'NONE', *, *, #86568, .T. ) ;
#81622 = CARTESIAN_POINT ( 'NONE',  ( -17.73273491259999801, 1417.940993905429877, 206.5463141675389807 ) ) ;
#81623 = DIRECTION ( 'NONE',  ( -1.755985294532469921E-16, 1.000000000000000000, -1.338183447452831989E-16 ) ) ;
#81624 = EDGE_CURVE ( 'NONE', #104774, #5353, #80596, .T. ) ;
#81625 = DIRECTION ( 'NONE',  ( 4.465978680329379737E-17, 1.000000000000000000, -2.349386720892264891E-16 ) ) ;
#81626 = CARTESIAN_POINT ( 'NONE',  ( -11.58690340151069798, 1425.690683090560015, 133.5559456973340104 ) ) ;
#81627 = CARTESIAN_POINT ( 'NONE',  ( -39.43671781166209911, 1447.053669326719955, 136.6351060954069965 ) ) ;
#81628 = CARTESIAN_POINT ( 'NONE',  ( 11.60004869885203682, 1426.038537708185913, 137.7598684020179007 ) ) ;
#81629 = CARTESIAN_POINT ( 'NONE',  ( 2.647161304830442319, 1417.760379040673342, 233.9115002235340626 ) ) ;
#81630 = CARTESIAN_POINT ( 'NONE',  ( -2.500000000000000000, 1420.232870451130111, 149.2693594355980053 ) ) ;
#81631 = CARTESIAN_POINT ( 'NONE',  ( -1.315889753809829976, 1455.200739381179801, 198.6907887078860142 ) ) ;
#81632 = CARTESIAN_POINT ( 'NONE',  ( -3.829620113550000315, 1515.551704408389924, 207.0352977830190184 ) ) ;
#81633 = CARTESIAN_POINT ( 'NONE',  ( 36.81295551165820257, 1440.913060387279984, 254.3033511140860412 ) ) ;
#81634 = CARTESIAN_POINT ( 'NONE',  ( -9.702020572793150777, 1471.556206313400025, 212.0789205537989801 ) ) ;
#81635 = CARTESIAN_POINT ( 'NONE',  ( -1.600048698852036821, 1411.254281879943164, 137.0999999980979851 ) ) ;
#81636 = ORIENTED_EDGE ( 'NONE', *, *, #6329, .F. ) ;
#81637 = ORIENTED_EDGE ( 'NONE', *, *, #20758, .F. ) ;
#81638 = CARTESIAN_POINT ( 'NONE',  ( 10.52836328796560039, 1481.199420803890007, 208.2605164816220054 ) ) ;
#81639 = CARTESIAN_POINT ( 'NONE',  ( -19.08349653902698506, 1485.503699954400417, 189.6259701294393949 ) ) ;
#81640 = CARTESIAN_POINT ( 'NONE',  ( -1.780534836129999965, 1443.660695742489906, 199.9945852240089721 ) ) ;
#81641 = CARTESIAN_POINT ( 'NONE',  ( 18.46871732690730283, 1509.558002197609767, 190.5444645169020248 ) ) ;
#81642 = CARTESIAN_POINT ( 'NONE',  ( 15.05358515032119904, 1410.831827804430077, 191.5175411757069810 ) ) ;
#81643 = EDGE_CURVE ( 'NONE', #7882, #94821, #106964, .T. ) ;
#81644 = CARTESIAN_POINT ( 'NONE',  ( -1.109176384893529876, 1508.551704408389924, 220.0791009952889965 ) ) ;
#81645 = CARTESIAN_POINT ( 'NONE',  ( -51.45124350130279822, 1383.809539065679928, 264.3240461168200000 ) ) ;
#81646 = CARTESIAN_POINT ( 'NONE',  ( -14.69331829855070026, 1452.091493848030041, 222.9975758587799817 ) ) ;
#81647 = CARTESIAN_POINT ( 'NONE',  ( -12.84591856360000151, 1434.996842492640098, 194.0990980877979837 ) ) ;
#81648 = CARTESIAN_POINT ( 'NONE',  ( -11.86289009182950061, 1502.090840157799903, 208.8788401476599859 ) ) ;
#81649 = CARTESIAN_POINT ( 'NONE',  ( 1.713204752390000252, 1465.618698357430276, 235.0090078382979755 ) ) ;
#81651 = VERTEX_POINT ( 'NONE', #21751 ) ;
#81650 = CARTESIAN_POINT ( 'NONE',  ( -41.66135440509999910, 1443.796918820770088, 135.6885369501979994 ) ) ;
#81652 = CARTESIAN_POINT ( 'NONE',  ( -0.5934080169919999648, 1450.964169822730128, 181.9620993427980125 ) ) ;
#81653 = CARTESIAN_POINT ( 'NONE',  ( -16.29753011569999899, 1382.961179775240225, 200.7913250421689781 ) ) ;
#81654 = CARTESIAN_POINT ( 'NONE',  ( 3.466266129261410089, 1508.551704408389924, 204.3328199221159878 ) ) ;
#81656 = EDGE_LOOP ( 'NONE', ( #50097, #4169, #13544, #64242, #42933, #41009, #29148, #55690 ) ) ;
#81655 = CARTESIAN_POINT ( 'NONE',  ( 9.225907677606098645, 1517.051704408389924, 198.5805875773771731 ) ) ;
#81657 = CARTESIAN_POINT ( 'NONE',  ( -17.66148560826829694, 1440.150327659670211, 218.7822435725309731 ) ) ;
#81658 = EDGE_LOOP ( 'NONE', ( #50744, #63052, #49215, #106110 ) ) ;
#81659 = CARTESIAN_POINT ( 'NONE',  ( -11.02704084530000017, 1390.246027334430210, 215.0626141722390230 ) ) ;
#81660 = CARTESIAN_POINT ( 'NONE',  ( -3.982959079219469789, 1515.551843419029865, 206.2722837986890170 ) ) ;
#81661 = CARTESIAN_POINT ( 'NONE',  ( -4.798573010642852132, 1474.699596436941647, 199.5387037236716594 ) ) ;
#81662 = CARTESIAN_POINT ( 'NONE',  ( -4.748707946720000628, 1463.075555322190212, 200.5806829759990251 ) ) ;
#81663 = ADVANCED_FACE ( 'NONE', ( #72751 ), #64361, .T. ) ;
#81664 = CARTESIAN_POINT ( 'NONE',  ( 1.336801414591168413, 1526.382868172864164, 178.6745493585861482 ) ) ;
#81665 = CARTESIAN_POINT ( 'NONE',  ( -10.06325851941720018, 1473.086862127829818, 207.3770336094819982 ) ) ;
#81666 = CARTESIAN_POINT ( 'NONE',  ( 11.49168982355860003, 1409.314359038739894, 199.5648683907749898 ) ) ;
#81667 = CARTESIAN_POINT ( 'NONE',  ( 18.52259598965499876, 1425.592173059454126, 225.5497999757189973 ) ) ;
#81668 = CARTESIAN_POINT ( 'NONE',  ( 15.69795926444620271, 1519.551704408389924, 222.7678737639049871 ) ) ;
#81669 = CARTESIAN_POINT ( 'NONE',  ( 20.20959865099471031, 1512.187213306747481, 182.0120230947219966 ) ) ;
#81670 = CARTESIAN_POINT ( 'NONE',  ( -67.40081635460001053, 1379.748791505480085, 277.3949072269590488 ) ) ;
#81671 = CIRCLE ( 'NONE', #106783, 1.999999961249164571 ) ;
#81672 = CARTESIAN_POINT ( 'NONE',  ( -3.766451722194359863, 1450.184391830480081, 184.9593740939260158 ) ) ;
#81673 = EDGE_LOOP ( 'NONE', ( #35264, #97438, #81473, #29614 ) ) ;
#81674 = ORIENTED_EDGE ( 'NONE', *, *, #31669, .F. ) ;
#81675 = CARTESIAN_POINT ( 'NONE',  ( 20.17436656406300699, 1524.841055067849766, 237.7389007707603241 ) ) ;
#81676 = CARTESIAN_POINT ( 'NONE',  ( -12.20493293955300196, 1416.321686235030029, 194.7273820060790115 ) ) ;
#81677 = CARTESIAN_POINT ( 'NONE',  ( -12.58535514000000077, 1434.516889947230084, 149.4256401672980132 ) ) ;
#81678 = EDGE_CURVE ( 'NONE', #83932, #64568, #66021, .T. ) ;
#81679 = CARTESIAN_POINT ( 'NONE',  ( 22.75273496409577945, 1512.187213306747481, 183.6728937936772184 ) ) ;
#81680 = CARTESIAN_POINT ( 'NONE',  ( -20.03609527204229934, 1489.599509856700024, 190.9186466828699906 ) ) ;
#81681 = CARTESIAN_POINT ( 'NONE',  ( -15.15615661080000187, 1420.466168034640077, 211.8568737882690129 ) ) ;
#81682 = CARTESIAN_POINT ( 'NONE',  ( -109.3508372059999942, 1385.551281695979924, 311.2426504422589915 ) ) ;
#81683 = CARTESIAN_POINT ( 'NONE',  ( -7.482857926667088933, 1511.023286695659863, 215.2724589492860048 ) ) ;
#81684 = CARTESIAN_POINT ( 'NONE',  ( -10.51561482155124772, 1366.597316028666000, 207.6218459616987673 ) ) ;
#81685 = CARTESIAN_POINT ( 'NONE',  ( -46.05257396074449616, 1440.913065467579827, 266.6769880795539507 ) ) ;
#81686 = B_SPLINE_CURVE_WITH_KNOTS ( 'NONE', 3,
 ( #18652, #45009, #247, #10267, #52301, #53972, #86426, #61814, #35473, #9716, #68547, #78587, #102647, #44443, #27627, #51740, #60707, #69664, #25947, #60142, #76936, #95937, #19197, #79154, #1903, #36041, #42776, #86978, #43882, #9176, #43341, #78026, #62365, #52851, #96490, #2463, #1333, #103787, #77489, #27088, #61272, #70229, #53399, #95387, #88104, #87549, #789, #10838, #34374, #104334, #28180, #94262, #26510, #17538, #36579, #70777, #104889, #85874, #34918, #69104, #103205, #22489, #46659, #56133, #105445, #4631, #107636, #3560, #11931, #28733, #47736, #71887, #90267, #106002, #65098, #13005, #13550, #30370, #107081, #64011, #56690, #98122, #11393, #46110, #79704, #62939, #97590, #81316, #29278, #55607, #80241, #81871, #89731, #63471, #20862, #89183, #106535, #97050, #29824, #99210, #45563, #55057, #54518, #5172, #37682, #12477, #80791, #20313, #21397, #4098, #38222, #38769, #3009, #30919, #37132, #88653, #72404, #47191, #72943, #64559, #98678 ),
 .UNSPECIFIED., .F., .F.,
 ( 4, 2, 2, 2, 2, 2, 1, 1, 1, 1, 1, 2, 2, 2, 2, 2, 2, 2, 1, 1, 1, 1, 1, 2, 2, 2, 2, 2, 2, 2, 1, 1, 1, 1, 1, 1, 2, 2, 2, 2, 2, 1, 1, 1, 1, 1, 1, 2, 2, 2, 2, 1, 1, 1, 1, 1, 1, 2, 2, 2, 1, 1, 1, 1, 1, 2, 2, 2, 2, 2, 1, 1, 1, 1, 2, 2, 1, 1, 2, 4 ),
 ( 0.000000000000000000, 0.06250000000015401569, 0.1250000000003080314, 0.1875000000004620471, 0.2187500000005390688, 0.2343750000005775658, 0.2421875000005963841, 0.2460937500006055434, 0.2480468750006098733, 0.2490234375006122602, 0.2495117187506134815, 0.2497558593756140644, 0.2500000000006146750, 0.3125000000006831757, 0.3750000000007517320, 0.4375000000008202328, 0.4687500000008548717, 0.4843750000008721912, 0.4921875000008812950, 0.4960937500008858470, 0.4980468750008876788, 0.4990234375008891221, 0.4995117187508901768, 0.4997558593758907319, 0.5000000000008912870, 0.5625000000010081935, 0.6250000000011251000, 0.6875000000012428947, 0.7187500000013026247, 0.7343750000013316015, 0.7421875000013461454, 0.7460937500013532508, 0.7480468750013579138, 0.7490234375013611334, 0.7495117187513627988, 0.7497558593763636869, 0.7498779296888640200, 0.7500000000013644641, 0.8125000000014666046, 0.8437500000015185631, 0.8593750000015447643, 0.8671875000015588641, 0.8710937500015667467, 0.8730468750015695223, 0.8740234375015699664, 0.8745117187515702994, 0.8747558593765693002, 0.8748779296890687451, 0.8750000000015680790, 0.9062500000013085089, 0.9218750000011778356, 0.9296875000011124435, 0.9335937500010798029, 0.9355468750010625945, 0.9365234375010541568, 0.9370117187510489387, 0.9372558593760461632, 0.9373779296885438317, 0.9375000000010415002, 0.9531250000007589485, 0.9609375000006168399, 0.9648437500005457856, 0.9667968750005112577, 0.9677734375004941603, 0.9682617187504866108, 0.9685058593754828360, 0.9687500000004790612, 0.9765625000003641532, 0.9804687500003066436, 0.9814453125002918776, 0.9824218750002771117, 0.9843750000002472467, 0.9882812500001895151, 0.9885253906251861844, 0.9886474609376846301, 0.9887695312501830758, 0.9892578125001750822, 0.9902343750001582068, 0.9921875000001258993, 1.000000000000000000 ),
 .UNSPECIFIED. ) ;
#81687 = EDGE_CURVE ( 'NONE', #73608, #49951, #2660, .T. ) ;
#81688 = CARTESIAN_POINT ( 'NONE',  ( 3.141363374988426660, 1525.159177407155767, 176.7077309898103010 ) ) ;
#81689 = CARTESIAN_POINT ( 'NONE',  ( 7.323390407215000231, 1516.613712827999962, 207.9924597298270044 ) ) ;
#81690 = CARTESIAN_POINT ( 'NONE',  ( -8.747074744635460419, 1447.713388414080100, 212.1118496456160187 ) ) ;
#81691 = CARTESIAN_POINT ( 'NONE',  ( 2.658320287279529737, 1408.468079325770077, 222.5002190481939977 ) ) ;
#81692 = CARTESIAN_POINT ( 'NONE',  ( -14.08843079593609993, 1436.001885614380171, 150.1056882708590194 ) ) ;
#81693 = CIRCLE ( 'NONE', #108565, 2.000000000000001776 ) ;
#81694 = CARTESIAN_POINT ( 'NONE',  ( -8.578981978779999906, 1385.024532827439998, 218.6678019865190095 ) ) ;
#81695 = CARTESIAN_POINT ( 'NONE',  ( 6.772449311907529967, 1425.395680090955921, 226.3226949956692522 ) ) ;
#81696 = CARTESIAN_POINT ( 'NONE',  ( 7.105712853721669831, 1424.913842867449830, 213.0229688049089702 ) ) ;
#81697 = VERTEX_POINT ( 'NONE', #102337 ) ;
#81698 = CARTESIAN_POINT ( 'NONE',  ( 15.89627787559999916, 1415.668893200830098, 250.4785789370980069 ) ) ;
#81699 = CARTESIAN_POINT ( 'NONE',  ( -0.8266050234419367593, 1416.818673806272272, 228.0313514088118723 ) ) ;
#81701 = CARTESIAN_POINT ( 'NONE',  ( -16.26032719119999825, 1409.480883525030094, 194.9505595544979997 ) ) ;
#81700 = CARTESIAN_POINT ( 'NONE',  ( -11.82672846260030042, 1491.252350426499788, 206.7221554372329990 ) ) ;
#81702 = CARTESIAN_POINT ( 'NONE',  ( -13.59642666202369199, 1409.123926534358816, 270.0979380971739943 ) ) ;
#81703 = CARTESIAN_POINT ( 'NONE',  ( -3.933791733460000106, 1420.650940111930140, 220.7242732661979971 ) ) ;
#81704 = CARTESIAN_POINT ( 'NONE',  ( -4.637746460722021347, 1378.072810476678342, 214.3830454900369205 ) ) ;
#81705 = EDGE_CURVE ( 'NONE', #102491, #52007, #55640, .T. ) ;
#81706 = CARTESIAN_POINT ( 'NONE',  ( -2.467066344142949674, 1452.826908532200150, 152.4293883740839988 ) ) ;
#81707 = CARTESIAN_POINT ( 'NONE',  ( 27.42695472179999783, 1451.955572177629847, 134.9063961680979844 ) ) ;
#81708 = VERTEX_POINT ( 'NONE', #7196 ) ;
#81709 = CARTESIAN_POINT ( 'NONE',  ( -2.500000000000000000, 1419.649642134729902, 147.2763244958979953 ) ) ;
#81710 = DIRECTION ( 'NONE',  ( 0.000000000000000000, 1.000000000000000000, 0.000000000000000000 ) ) ;
#81711 = FACE_OUTER_BOUND ( 'NONE', #3276, .T. ) ;
#81712 = ORIENTED_EDGE ( 'NONE', *, *, #58207, .T. ) ;
#81713 = ORIENTED_EDGE ( 'NONE', *, *, #106862, .T. ) ;
#81714 = CARTESIAN_POINT ( 'NONE',  ( -16.32897964160000370, 1384.525298249519892, 200.5993092285889929 ) ) ;
#81715 = CARTESIAN_POINT ( 'NONE',  ( -24.09604921521779985, 1410.858796070480139, 208.7909344980870117 ) ) ;
#81716 = EDGE_CURVE ( 'NONE', #53542, #110638, #14057, .T. ) ;
#81717 = ORIENTED_EDGE ( 'NONE', *, *, #11089, .T. ) ;
#81718 = CARTESIAN_POINT ( 'NONE',  ( 3.861663294462490015, 1508.610718243669908, 204.4420517555579977 ) ) ;
#81719 = CIRCLE ( 'NONE', #53147, 33.13701971169416538 ) ;
#81720 = LINE ( 'NONE', #39172, #29488 ) ;
#81721 = ADVANCED_FACE ( 'NONE', ( #8274 ), #26841, .T. ) ;
#81722 = CARTESIAN_POINT ( 'NONE',  ( -0.5993188596290000003, 1479.776975780129987, 236.1040631272980193 ) ) ;
#81723 = CARTESIAN_POINT ( 'NONE',  ( -3.968827103576990201, 1522.051704408389924, 229.5396913781519856 ) ) ;
#81724 = ORIENTED_EDGE ( 'NONE', *, *, #104372, .F. ) ;
#81725 = CARTESIAN_POINT ( 'NONE',  ( 46.02990395988660310, 1441.850884208020034, 268.4960837853089970 ) ) ;
#81726 = CARTESIAN_POINT ( 'NONE',  ( -3.487585001777260274, 1508.551704408610021, 204.2892321445339689 ) ) ;
#81727 = CARTESIAN_POINT ( 'NONE',  ( 0.05691672067130000567, 1419.745815343030017, 184.3817560464979977 ) ) ;
#81728 = CARTESIAN_POINT ( 'NONE',  ( -4.621267922064999922, 1516.830644417779922, 204.1223895416970038 ) ) ;
#81729 = ORIENTED_EDGE ( 'NONE', *, *, #17484, .F. ) ;
#81730 = CARTESIAN_POINT ( 'NONE',  ( 7.150985165824430112, 1483.211489592900080, 218.5460388441480006 ) ) ;
#81731 = CARTESIAN_POINT ( 'NONE',  ( 13.10446631662097694, 1443.028365240957783, 187.3795884430450371 ) ) ;
#81732 = ORIENTED_EDGE ( 'NONE', *, *, #21536, .T. ) ;
#81733 = ORIENTED_EDGE ( 'NONE', *, *, #38623, .T. ) ;
#81734 = CARTESIAN_POINT ( 'NONE',  ( -10.70175718777040075, 1481.110708145740091, 208.7148072333299922 ) ) ;
#81735 = CARTESIAN_POINT ( 'NONE',  ( -3.208441210349299855, 1508.400043147619954, 220.5739096555420247 ) ) ;
#81736 = CARTESIAN_POINT ( 'NONE',  ( 3.240951521948889802, 1499.214374350819980, 198.1680990744349913 ) ) ;
#81737 = CARTESIAN_POINT ( 'NONE',  ( -14.69525445759580151, 1513.799047785590119, 194.1342753316129688 ) ) ;
#81738 = CARTESIAN_POINT ( 'NONE',  ( 22.23919608084329980, 1452.136450547310005, 140.1164325590560225 ) ) ;
#81739 = CARTESIAN_POINT ( 'NONE',  ( -1.700037425840850145E-05, 1408.561147966129965, 270.4290818598980195 ) ) ;
#81740 = EDGE_CURVE ( 'NONE', #64216, #45216, #6794, .T. ) ;
#81741 = CARTESIAN_POINT ( 'NONE',  ( -3.132370430190279720, 1476.360346537520172, 220.1606225241589812 ) ) ;
#81742 = CARTESIAN_POINT ( 'NONE',  ( -8.219322315134521162, 1493.760598851730037, 199.9648169300360223 ) ) ;
#81743 = CARTESIAN_POINT ( 'NONE',  ( -10.97066968179730040, 1432.419134699010101, 151.7701069147389887 ) ) ;
#81744 = CARTESIAN_POINT ( 'NONE',  ( 0.02210936670623420836, 1409.026086586376778, 232.3383378967181727 ) ) ;
#81746 = CARTESIAN_POINT ( 'NONE',  ( -3.527569048119670203, 1486.518325592330029, 181.8541486797999767 ) ) ;
#81745 = CARTESIAN_POINT ( 'NONE',  ( -16.81906092389080243, 1415.724267959580175, 191.6016362877150243 ) ) ;
#81747 = VECTOR ( 'NONE', #75062, 1000.000000000000114 ) ;
#81748 = CARTESIAN_POINT ( 'NONE',  ( 12.03043414124249999, 1426.848548796940122, 206.5778447381370029 ) ) ;
#81749 = CARTESIAN_POINT ( 'NONE',  ( -25.19698811078400169, 1509.685706755500178, 222.8649656611040086 ) ) ;
#81750 = EDGE_CURVE ( 'NONE', #69697, #7138, #469, .T. ) ;
#81751 = FACE_OUTER_BOUND ( 'NONE', #4381, .T. ) ;
#81752 = ORIENTED_EDGE ( 'NONE', *, *, #86662, .T. ) ;
#81753 = CARTESIAN_POINT ( 'NONE',  ( 3.858955742690000079, 1472.030406003990038, 215.5337125726789793 ) ) ;
#81754 = CARTESIAN_POINT ( 'NONE',  ( -11.73709356416840066, 1426.695943276110029, 144.1748013770919954 ) ) ;
#81755 = AXIS2_PLACEMENT_3D ( 'NONE', #91187, #7191, #49207 ) ;
#81756 = CARTESIAN_POINT ( 'NONE',  ( -97.79264536580190281, 1384.951517786579871, 310.5502822603710342 ) ) ;
#81757 = CARTESIAN_POINT ( 'NONE',  ( -8.049886528540000086, 1385.314864400589840, 199.5718903080289977 ) ) ;
#81758 = ADVANCED_FACE ( 'NONE', ( #79370 ), #59912, .F. ) ;
#81759 = CARTESIAN_POINT ( 'NONE',  ( 10.30455700085379966, 1426.851391274549997, 209.1700833811410121 ) ) ;
#81760 =( BOUNDED_CURVE ( )  B_SPLINE_CURVE ( 3, ( #72847, #106981, #56041, #30269 ),
 .UNSPECIFIED., .F., .T. ) 
 B_SPLINE_CURVE_WITH_KNOTS ( ( 4, 4 ),
 ( 1.570952385993269473, 3.141745504670674816 ),
 .UNSPECIFIED. ) 
 CURVE ( )  GEOMETRIC_REPRESENTATION_ITEM ( )  RATIONAL_B_SPLINE_CURVE ( ( 1.000000000000000000, 0.8047386102843028244, 0.8047386102843028244, 1.000000000000000000 ) ) 
 REPRESENTATION_ITEM ( '' )  );
#81762 = ORIENTED_EDGE ( 'NONE', *, *, #30221, .F. ) ;
#81761 = CARTESIAN_POINT ( 'NONE',  ( -16.08636396047539918, 1420.123211618729783, 209.9761059327369992 ) ) ;
#81763 = CARTESIAN_POINT ( 'NONE',  ( 2.885753653580000133, 1430.267042387290076, 217.3699626952389963 ) ) ;
#81764 = CARTESIAN_POINT ( 'NONE',  ( -0.8197920095480000224, 1434.541746329560056, 150.4759714514979976 ) ) ;
#81765 = CARTESIAN_POINT ( 'NONE',  ( -14.45760372979999886, 1416.831925145830155, 221.3918073827979924 ) ) ;
#81766 = CARTESIAN_POINT ( 'NONE',  ( -12.51099982459209947, 1416.825784013739849, 222.1450729932890056 ) ) ;
#81767 = CARTESIAN_POINT ( 'NONE',  ( 11.65415823093499981, 1512.679339245399888, 225.6053821474669974 ) ) ;
#81768 = CARTESIAN_POINT ( 'NONE',  ( 13.15726444150010011, 1415.434635989099888, 196.8996500771419846 ) ) ;
#81769 = CARTESIAN_POINT ( 'NONE',  ( 8.701316397187270013, 1436.141094936039735, 208.2917281785899775 ) ) ;
#81770 = CARTESIAN_POINT ( 'NONE',  ( -30.31940284292398857, 1523.382868172864164, 222.4933038710547919 ) ) ;
#81771 = CARTESIAN_POINT ( 'NONE',  ( 11.93521150820000010, 1422.099766630330123, 229.5825812192979924 ) ) ;
#81772 = B_SPLINE_CURVE_WITH_KNOTS ( 'NONE', 5,
 ( #33407, #41828, #109593, #65956, #24455, #93324, #82732, #42375, #109050 ),
 .UNSPECIFIED., .F., .F.,
 ( 6, 3, 6 ),
 ( -5.629877540799999913, -0.1526127635309997288, 5.629877540799999913 ),
 .UNSPECIFIED. ) ;
#81773 = CARTESIAN_POINT ( 'NONE',  ( -22.52214966618477376, 1524.244163922423695, 236.5012798002454701 ) ) ;
#81774 = CARTESIAN_POINT ( 'NONE',  ( 2.463155222774959796, 1474.677674756690067, 220.2738971877009817 ) ) ;
#81775 = CARTESIAN_POINT ( 'NONE',  ( -18.03030449919999612, 1409.542692494829907, 222.7095495660980191 ) ) ;
#81776 = AXIS2_PLACEMENT_3D ( 'NONE', #61993, #45183, #44626 ) ;
#81777 = CARTESIAN_POINT ( 'NONE',  ( -0.1664554869000815507, 1508.975239299347777, 238.8734868107800366 ) ) ;
#81778 = CARTESIAN_POINT ( 'NONE',  ( 5.389719913101400195, 1440.971386073809981, 154.8246291173960003 ) ) ;
#81779 = CARTESIAN_POINT ( 'NONE',  ( -26.53449174420000034, 1450.861614052709911, 136.4341869045979934 ) ) ;
#81780 = CARTESIAN_POINT ( 'NONE',  ( 5.360207926212690488, 1422.242713656610022, 144.1549664376839814 ) ) ;
#81781 = CARTESIAN_POINT ( 'NONE',  ( 1.106162138419999996, 1515.349603040190004, 204.8392668440190221 ) ) ;
#81782 = CARTESIAN_POINT ( 'NONE',  ( 12.49318908552830010, 1427.060670871449929, 206.4845319198009861 ) ) ;
#81783 = CARTESIAN_POINT ( 'NONE',  ( -34.74032776987759519, 1437.042396455660082, 136.5358758002960258 ) ) ;
#81784 = CARTESIAN_POINT ( 'NONE',  ( -5.808538649209999960, 1415.087797054229895, 225.3799766708980030 ) ) ;
#81785 = LINE ( 'NONE', #107551, #95791 ) ;
#81786 = CARTESIAN_POINT ( 'NONE',  ( -14.66707320740000142, 1409.366313021530004, 207.8310585063279916 ) ) ;
#81787 = DIRECTION ( 'NONE',  ( 0.7071067811865490160, 0.000000000000000000, -0.7071067811865460184 ) ) ;
#81788 = FACE_OUTER_BOUND ( 'NONE', #38760, .T. ) ;
#81789 = CARTESIAN_POINT ( 'NONE',  ( 2.856819527319533147, 1485.195369544046798, 198.7387337485362480 ) ) ;
#81790 = CARTESIAN_POINT ( 'NONE',  ( 11.94121320300000022, 1433.615332063370033, 149.0256580470980055 ) ) ;
#81791 = CARTESIAN_POINT ( 'NONE',  ( -27.70450820019999938, 1435.944202404889893, 136.4829434803980064 ) ) ;
#81792 = CARTESIAN_POINT ( 'NONE',  ( 12.53380499169999851, 1442.773887286369927, 186.4115750671979868 ) ) ;
#81793 = VERTEX_POINT ( 'NONE', #20532 ) ;
#81794 = B_SPLINE_CURVE_WITH_KNOTS ( 'NONE', 3,
 ( #36439, #44313, #28596, #35343, #54379, #12331 ),
 .UNSPECIFIED., .F., .F.,
 ( 4, 2, 4 ),
 ( 0.000000000000000000, 0.5000000000000000000, 1.000000000000000000 ),
 .UNSPECIFIED. ) ;
#81795 = CARTESIAN_POINT ( 'NONE',  ( -1.337327472479999946, 1485.289799181490025, 198.0623755896990019 ) ) ;
#81796 = CARTESIAN_POINT ( 'NONE',  ( 8.960243246639999271, 1478.398532434489880, 202.8149044888089918 ) ) ;
#81797 = CARTESIAN_POINT ( 'NONE',  ( -11.29853220753019905, 1409.307613826159923, 218.9138666963339972 ) ) ;
#81798 = CARTESIAN_POINT ( 'NONE',  ( -11.33289292689999961, 1491.456575546390013, 207.4739972654290057 ) ) ;
#81799 = CARTESIAN_POINT ( 'NONE',  ( -0.6637618131060000204, 1452.913539784329942, 183.3365650660979895 ) ) ;
#81800 = CARTESIAN_POINT ( 'NONE',  ( 14.37827720497629969, 1508.124459880479890, 232.6080666346479973 ) ) ;
#81801 = AXIS2_PLACEMENT_3D ( 'NONE', #83517, #33117, #101400 ) ;
#81802 = CARTESIAN_POINT ( 'NONE',  ( 43.01611365321106462, 1429.412580181660815, 269.0481421394022732 ) ) ;
#81803 = CARTESIAN_POINT ( 'NONE',  ( 20.56075711880000156, 1453.152003547730146, 210.2400806596079974 ) ) ;
#81804 = CARTESIAN_POINT ( 'NONE',  ( -12.29457997419999948, 1378.306942845010099, 210.0158913818380029 ) ) ;
#81805 = CARTESIAN_POINT ( 'NONE',  ( -104.5732689346720008, 1384.592179270920042, 311.1645418064740056 ) ) ;
#81806 = CARTESIAN_POINT ( 'NONE',  ( -62.90092488694899941, 1385.075852493079992, 250.3550165034500026 ) ) ;
#81807 = CARTESIAN_POINT ( 'NONE',  ( -12.03082246793990073, 1491.135896161340042, 206.7151464320039906 ) ) ;
#81808 = CARTESIAN_POINT ( 'NONE',  ( -4.421996589226610652, 1508.551704408389924, 205.0496395602209816 ) ) ;
#81809 = CARTESIAN_POINT ( 'NONE',  ( 16.53242905777655025, 1526.073429442291854, 182.3092717672457184 ) ) ;
#81810 = CARTESIAN_POINT ( 'NONE',  ( 1.590879946460525218, 1526.333389947941669, 178.3980910637225463 ) ) ;
#81811 = CARTESIAN_POINT ( 'NONE',  ( -16.19826984269869996, 1409.504006194269778, 225.4340666559009776 ) ) ;
#81813 = ORIENTED_EDGE ( 'NONE', *, *, #27503, .T. ) ;
#81812 = CARTESIAN_POINT ( 'NONE',  ( 0.4868008580694940246, 1418.555763684930071, 184.7190794935820293 ) ) ;
#81814 = CARTESIAN_POINT ( 'NONE',  ( -13.70773370810000102, 1507.648153709230201, 184.2587369236979953 ) ) ;
#81815 = CARTESIAN_POINT ( 'NONE',  ( 10.08617654595050084, 1470.665958206250025, 210.9901929890509962 ) ) ;
#81816 = CARTESIAN_POINT ( 'NONE',  ( 5.649719750514999639, 1514.216922324319739, 200.4731542066570000 ) ) ;
#81817 = CARTESIAN_POINT ( 'NONE',  ( -109.6501487310000016, 1384.584076603700169, 311.3100189002590241 ) ) ;
#81818 = CARTESIAN_POINT ( 'NONE',  ( 2.038847259689231084, 1522.382868172863937, 173.3106345060153046 ) ) ;
#81819 = CARTESIAN_POINT ( 'NONE',  ( -1.302966447159999985, 1421.690229046850163, 193.6084558154989850 ) ) ;
#81820 = CARTESIAN_POINT ( 'NONE',  ( 22.17406007969999848, 1409.851833609830010, 214.1807298746780077 ) ) ;
#81821 = CARTESIAN_POINT ( 'NONE',  ( -2.671470825897180212, 1410.370364388000098, 186.5763473022349785 ) ) ;
#81822 = CARTESIAN_POINT ( 'NONE',  ( -18.54887138051830320, 1467.029277636209827, 200.9622475402150030 ) ) ;
#81823 = CARTESIAN_POINT ( 'NONE',  ( -18.26676158009999895, 1424.840347090229898, 227.6848214930980134 ) ) ;
#81825 = CARTESIAN_POINT ( 'NONE',  ( 0.4151546846821903003, 1501.977400791986611, 244.9330574173806951 ) ) ;
#81824 = CARTESIAN_POINT ( 'NONE',  ( -3.605950197753253761, 1511.586636682142625, 201.0506624174682315 ) ) ;
#81826 = CARTESIAN_POINT ( 'NONE',  ( 23.83757722819380120, 1411.098961242099904, 208.0515134900099952 ) ) ;
#81827 = CARTESIAN_POINT ( 'NONE',  ( -107.9538559792320740, 1348.229899472569059, 307.1970880689542582 ) ) ;
#81828 = CARTESIAN_POINT ( 'NONE',  ( 16.71509328322861521, 1526.382868172863937, 234.3620852791651146 ) ) ;
#81829 = CARTESIAN_POINT ( 'NONE',  ( -13.93400296699999963, 1503.656733194990011, 208.7363982927060135 ) ) ;
#81830 = VECTOR ( 'NONE', #87473, 1000.000000000000000 ) ;
#81831 = CARTESIAN_POINT ( 'NONE',  ( -8.622403150220000256, 1362.632156860360055, 210.6218459616991936 ) ) ;
#81832 = CARTESIAN_POINT ( 'NONE',  ( -1.134358008724999811, 1516.744381837270112, 205.0932347109869909 ) ) ;
#81833 = CARTESIAN_POINT ( 'NONE',  ( -6.438481900084330078, 1485.523881333330110, 183.4856451987570267 ) ) ;
#81834 = FACE_OUTER_BOUND ( 'NONE', #9472, .T. ) ;
#81835 = CARTESIAN_POINT ( 'NONE',  ( -4.221673790220910050, 1441.603346299159966, 168.4332526023039804 ) ) ;
#81838 = ORIENTED_EDGE ( 'NONE', *, *, #39427, .T. ) ;
#81837 = CARTESIAN_POINT ( 'NONE',  ( -67.79781760454831385, 1379.745846262460191, 279.2210569798610322 ) ) ;
#81836 = AXIS2_PLACEMENT_3D ( 'NONE', #46616, #104291, #53926 ) ;
#81839 = ORIENTED_EDGE ( 'NONE', *, *, #57111, .T. ) ;
#81840 = CARTESIAN_POINT ( 'NONE',  ( 29.68011212880000116, 1509.981399006330093, 210.4260893018980312 ) ) ;
#81841 = EDGE_LOOP ( 'NONE', ( #90691, #33652, #80600, #1424 ) ) ;
#81842 = AXIS2_PLACEMENT_3D ( 'NONE', #14071, #90228, #41912 ) ;
#81843 = CARTESIAN_POINT ( 'NONE',  ( 1.868158843242359923, 1485.292041900309869, 220.8373525465659668 ) ) ;
#81844 = CARTESIAN_POINT ( 'NONE',  ( 11.15670367650000117, 1501.329131309490094, 206.5574276672290068 ) ) ;
#81846 = CARTESIAN_POINT ( 'NONE',  ( 15.68538546202029949, 1410.854151051389863, 191.5168454177849924 ) ) ;
#81845 = CARTESIAN_POINT ( 'NONE',  ( -11.69488816318309965, 1426.307070945479836, 141.1954652412310054 ) ) ;
#81847 = CARTESIAN_POINT ( 'NONE',  ( -4.031168805994999715, 1516.805675336850072, 209.8787446699039947 ) ) ;
#81848 = EDGE_CURVE ( 'NONE', #66063, #105626, #105143, .T. ) ;
#81849 = CARTESIAN_POINT ( 'NONE',  ( -24.80300324625899933, 1451.983833449960002, 136.3302103276260198 ) ) ;
#81850 = CARTESIAN_POINT ( 'NONE',  ( -11.73704819359999973, 1426.695975325029849, 144.1715469091980140 ) ) ;
#81851 = CARTESIAN_POINT ( 'NONE',  ( 9.159401628690000408, 1409.736190099430132, 229.9419424971980277 ) ) ;
#81853 = EDGE_CURVE ( 'NONE', #98070, #18384, #13781, .T. ) ;
#81852 = CARTESIAN_POINT ( 'NONE',  ( 6.445592309133529874, 1483.538731108610136, 219.1440388116969871 ) ) ;
#81854 = PRODUCT_CONTEXT ( 'NONE', #45628, 'mechanical' ) ;
#81855 = CARTESIAN_POINT ( 'NONE',  ( 41.31139259158630495, 1441.358669516819873, 134.0999999980719792 ) ) ;
#81856 = B_SPLINE_CURVE_WITH_KNOTS ( 'NONE', 3,
 ( #29428, #79856, #44600, #3167, #2059, #98290 ),
 .UNSPECIFIED., .F., .F.,
 ( 4, 2, 4 ),
 ( 0.000000000000000000, 0.5000000000000000000, 1.000000000000000000 ),
 .UNSPECIFIED. ) ;
#81857 = CARTESIAN_POINT ( 'NONE',  ( -26.45259676378333324, 1507.993351259675364, 215.5777749561062819 ) ) ;
#81858 = ORIENTED_EDGE ( 'NONE', *, *, #12447, .F. ) ;
#81859 = CARTESIAN_POINT ( 'NONE',  ( 18.38166056949999927, 1428.164368492389940, 201.4944003551989908 ) ) ;
#81860 = CARTESIAN_POINT ( 'NONE',  ( -2.847678236428970333, 1430.845636561999981, 201.2564352187889938 ) ) ;
#81861 = ORIENTED_EDGE ( 'NONE', *, *, #48019, .T. ) ;
#81862 = ORIENTED_EDGE ( 'NONE', *, *, #108310, .T. ) ;
#81863 = CARTESIAN_POINT ( 'NONE',  ( -6.059489674125000391, 1514.830240247470101, 217.0841925463570021 ) ) ;
#81864 = CARTESIAN_POINT ( 'NONE',  ( 16.78391007505477361, 1513.564960623365778, 195.8729266718472672 ) ) ;
#81865 = CARTESIAN_POINT ( 'NONE',  ( 0.3125228751849999931, 1450.902146847709901, 181.9094755473980172 ) ) ;
#81866 = CARTESIAN_POINT ( 'NONE',  ( -3.324976118279999948, 1484.702107398830094, 183.3515308503979782 ) ) ;
#81867 = CARTESIAN_POINT ( 'NONE',  ( -2.500000000000000000, 1439.604493174010031, 166.9187913690360006 ) ) ;
#81868 = B_SPLINE_CURVE_WITH_KNOTS ( 'NONE', 5,
 ( #74965, #55952, #90074, #23429, #32395, #13356, #23964, #47548, #30170 ),
 .UNSPECIFIED., .F., .F.,
 ( 6, 3, 6 ),
 ( 0.000000000000000000, 0.2526770774007812692, 1.000000000000000000 ),
 .UNSPECIFIED. ) ;
#81869 = CARTESIAN_POINT ( 'NONE',  ( -41.65407148426780282, 1444.067059942649848, 136.1145735031259960 ) ) ;
#81870 = ADVANCED_FACE ( 'NONE', ( #89415 ), #55285, .F. ) ;
#81871 = CARTESIAN_POINT ( 'NONE',  ( -67.16270863874164831, 1379.744581544945504, 276.7363381173806829 ) ) ;
#81872 = CARTESIAN_POINT ( 'NONE',  ( 1.907321127619999945, 1465.438333563990000, 199.0325445061990024 ) ) ;
#81873 = CARTESIAN_POINT ( 'NONE',  ( -17.43675326300159867, 1417.688629928019964, 206.2161178420579972 ) ) ;
#81874 = CARTESIAN_POINT ( 'NONE',  ( 1.387159858850000038, 1415.426952350729835, 190.7740710235979975 ) ) ;
#81875 = CARTESIAN_POINT ( 'NONE',  ( -68.09224033998870595, 1384.725039953799978, 261.8692284254199762 ) ) ;
#81876 = EDGE_LOOP ( 'NONE', ( #78886, #75905, #14929 ) ) ;
#81877 = DIRECTION ( 'NONE',  ( -0.6736849260863839728, 0.000000000000000000, 0.7390186874254150995 ) ) ;
#81878 = CARTESIAN_POINT ( 'NONE',  ( -6.951517170504999399, 1517.194816588360027, 207.9969518818670053 ) ) ;
#81879 = ORIENTED_EDGE ( 'NONE', *, *, #21247, .T. ) ;
#81880 = FACE_OUTER_BOUND ( 'NONE', #55305, .T. ) ;
#81881 = CARTESIAN_POINT ( 'NONE',  ( -0.0002459590164598172003, 1452.612215934647338, 153.4544582660230674 ) ) ;
#81882 = EDGE_LOOP ( 'NONE', ( #21948, #41710 ) ) ;
#81883 = CARTESIAN_POINT ( 'NONE',  ( 0.06979897883669991532, 1450.915497821400095, 181.2403767522520184 ) ) ;
#81884 = CARTESIAN_POINT ( 'NONE',  ( -16.17524367689999920, 1409.477912330530216, 192.6004206005979711 ) ) ;
#81885 = FACE_OUTER_BOUND ( 'NONE', #89246, .T. ) ;
#81886 = CARTESIAN_POINT ( 'NONE',  ( -10.31423480426190054, 1462.747221160460185, 206.6676018887629880 ) ) ;
#81887 = CARTESIAN_POINT ( 'NONE',  ( 22.42329670567509936, 1410.541750806409937, 206.2184894776289923 ) ) ;
#81888 = CARTESIAN_POINT ( 'NONE',  ( -5.912728008667049728, 1510.598356033839991, 201.5879984038760142 ) ) ;
#81889 = CARTESIAN_POINT ( 'NONE',  ( -2.875659706749999600, 1507.251074149530041, 180.8868938410979865 ) ) ;
#81890 = CARTESIAN_POINT ( 'NONE',  ( -5.929777071639043662, 1510.642476712295547, 201.6026015433274381 ) ) ;
#81891 = CARTESIAN_POINT ( 'NONE',  ( 26.58595117206280278, 1501.797944955920002, 206.2299323259489938 ) ) ;
#81893 = CARTESIAN_POINT ( 'NONE',  ( -11.60004869885203682, 1423.119248846121991, 136.9990639856974894 ) ) ;
#81892 = CARTESIAN_POINT ( 'NONE',  ( 15.40417916130000009, 1460.637496422029926, 229.9378244178980140 ) ) ;
#81894 = EDGE_CURVE ( 'NONE', #46650, #108404, #73666, .T. ) ;
#81895 = CARTESIAN_POINT ( 'NONE',  ( -2.484577695354999616, 1517.170512887980067, 216.4602579296269766 ) ) ;
#81896 = CARTESIAN_POINT ( 'NONE',  ( 0.1595995995380000143, 1486.508831850330125, 181.8147405652979671 ) ) ;
#81897 = CARTESIAN_POINT ( 'NONE',  ( -10.44855943793014319, 1480.411207778927064, 207.8053790864071289 ) ) ;
#81898 = CARTESIAN_POINT ( 'NONE',  ( 19.03234955206701073, 1444.324475315276004, 213.9789776947724249 ) ) ;
#81899 = CARTESIAN_POINT ( 'NONE',  ( 7.336844642415000450, 1517.106845464700200, 212.5753907958570039 ) ) ;
#81900 = B_SPLINE_CURVE_WITH_KNOTS ( 'NONE', 3,
 ( #26848, #102980, #85631, #101313, #34142, #69430, #75615, #77264, #61036, #94039, #50414, #8931, #51498, #95157, #34689, #33027, #24605, #52064, #16211, #93480, #16750, #85083, #68879, #60468, #9488, #8372, #68326, #102434, #25718, #59919, #94585, #17865, #43654, #77806, #104103, #3334, #18973, #80011, #54829, #12244, #10604, #36347, #44775, #71093, #97355, #11170, #11703, #96261, #19537, #21167, #2779, #53744 ),
 .UNSPECIFIED., .F., .F.,
 ( 4, 2, 2, 2, 1, 1, 1, 1, 2, 2, 2, 2, 2, 1, 1, 1, 2, 2, 2, 2, 2, 1, 1, 1, 1, 1, 2, 2, 2, 2, 2, 4 ),
 ( 0.000000000000000000, 0.1250000000000079381, 0.1875000000000119071, 0.2187500000000126843, 0.2343750000000130451, 0.2421875000000132672, 0.2460937500000133782, 0.2480468750000134892, 0.2490234375000133782, 0.2500000000000132672, 0.3750000000002221001, 0.4375000000003265721, 0.4687500000003787526, 0.4843750000004061196, 0.4921875000004198863, 0.4960937500004268808, 0.4980468750004303224, 0.5000000000004337641, 0.6250000000005224710, 0.6875000000005676570, 0.7187500000005903056, 0.7343750000006006307, 0.7421875000006051826, 0.7460937500006078471, 0.7480468750006094014, 0.7490234375006091794, 0.7495117187506087353, 0.7500000000006081802, 0.8125000000004561906, 0.8750000000003042011, 0.9375000000001521006, 1.000000000000000000 ),
 .UNSPECIFIED. ) ;
#81901 = CARTESIAN_POINT ( 'NONE',  ( 18.61766193520000101, 1509.563203467730091, 187.1480463371979965 ) ) ;
#81902 = EDGE_CURVE ( 'NONE', #65447, #43851, #89063, .T. ) ;
#81903 = DIRECTION ( 'NONE',  ( 8.881784197001252323E-15, 0.000000000000000000, 1.000000000000000000 ) ) ;
#81905 = ORIENTED_EDGE ( 'NONE', *, *, #62608, .T. ) ;
#81904 = CARTESIAN_POINT ( 'NONE',  ( -106.7715504409999880, 1386.777196091089991, 297.2705617508589739 ) ) ;
#81906 = CARTESIAN_POINT ( 'NONE',  ( -7.966035888499998663, 1384.903651512129727, 199.4892911144889922 ) ) ;
#81907 = CARTESIAN_POINT ( 'NONE',  ( 3.209791212160000295, 1508.551704408389924, 219.6807919779989788 ) ) ;
#81908 = CARTESIAN_POINT ( 'NONE',  ( -11.30117475489999990, 1432.296176012079741, 151.5220922668979995 ) ) ;
#81909 = DIRECTION ( 'NONE',  ( 1.755985294532464991E-16, -1.000000000000000000, 1.338183447452830017E-16 ) ) ;
#81910 = CARTESIAN_POINT ( 'NONE',  ( -109.6086345746109885, 1383.178240054900016, 311.2147542219479988 ) ) ;
#81911 = CARTESIAN_POINT ( 'NONE',  ( 27.02053748618845574, 1451.952524399011281, 135.1690508283753900 ) ) ;
#81912 = CARTESIAN_POINT ( 'NONE',  ( -19.21579922906590099, 1443.315308456250023, 209.4908471617739849 ) ) ;
#81913 = VECTOR ( 'NONE', #22113, 1000.000000000000227 ) ;
#81914 = CARTESIAN_POINT ( 'NONE',  ( 12.50982346350000007, 1445.295918751409999, 187.3223261910979716 ) ) ;
#81916 = CARTESIAN_POINT ( 'NONE',  ( -5.347953505379625661, 1422.377634548564401, 137.0999999978673998 ) ) ;
#81915 = CARTESIAN_POINT ( 'NONE',  ( -24.42891514760000149, 1457.437613031330102, 213.4851266144380020 ) ) ;
#81917 = CARTESIAN_POINT ( 'NONE',  ( 0.1620123089799999916, 1416.817366564930126, 190.8766898493980193 ) ) ;
#81918 = EDGE_LOOP ( 'NONE', ( #64684, #39595, #11182 ) ) ;
#81920 = CIRCLE ( 'NONE', #96238, 2.000010725851112170 ) ;
#81919 = CARTESIAN_POINT ( 'NONE',  ( -1.713317447804999949, 1516.660388280709867, 204.5138242629670060 ) ) ;
#81921 = CARTESIAN_POINT ( 'NONE',  ( 7.052473882389999282, 1406.463605886129926, 269.0260246300979361 ) ) ;
#81922 = CARTESIAN_POINT ( 'NONE',  ( -32.86802468363524099, 1523.481610118014487, 217.2040256692613980 ) ) ;
#81923 = AXIS2_PLACEMENT_3D ( 'NONE', #94731, #59496, #84120 ) ;
#81924 = CARTESIAN_POINT ( 'NONE',  ( 18.53883420589999886, 1410.877181416130043, 194.4121139098979825 ) ) ;
#81925 = CIRCLE ( 'NONE', #89130, 0.9999999999999970024 ) ;
#81926 = CARTESIAN_POINT ( 'NONE',  ( 23.64215237190858332, 1434.207970953952781, 214.6801654245506370 ) ) ;
#81927 = CARTESIAN_POINT ( 'NONE',  ( -1.151960966433035471, 1463.347226664416667, 199.4035414042922980 ) ) ;
#81928 = CARTESIAN_POINT ( 'NONE',  ( 21.12368589899999805, 1496.824149423590143, 208.3574563239919826 ) ) ;
#81929 = CARTESIAN_POINT ( 'NONE',  ( 1.984413551915469975, 1517.051704408389924, 198.9129232538419956 ) ) ;
#81930 = CARTESIAN_POINT ( 'NONE',  ( -0.5703798177140180226, 1450.893142285190152, 154.7888451936129854 ) ) ;
#81931 = CARTESIAN_POINT ( 'NONE',  ( -1.729960644012338955, 1451.871857846600051, 184.1618444272322108 ) ) ;
#81932 = CARTESIAN_POINT ( 'NONE',  ( 2.441038204699999881, 1449.508741055270093, 155.6080914322980107 ) ) ;
#81933 = CARTESIAN_POINT ( 'NONE',  ( 7.499999999999998224, 1374.913060387289988, 209.1218459572589836 ) ) ;
#81934 = CARTESIAN_POINT ( 'NONE',  ( -4.329448813750000014, 1515.064791442790010, 210.5737697173989886 ) ) ;
#81935 = CARTESIAN_POINT ( 'NONE',  ( -36.06124927489999976, 1440.913060387330006, 262.6648722463980334 ) ) ;
#81936 = CARTESIAN_POINT ( 'NONE',  ( -27.11938936275100076, 1507.995193792530017, 211.2322906163280152 ) ) ;
#81937 = CARTESIAN_POINT ( 'NONE',  ( 2.712833823950000056, 1440.235308908170055, 157.0900337514979981 ) ) ;
#81938 = CARTESIAN_POINT ( 'NONE',  ( -4.995145369879999464, 1475.912100276329966, 267.8435508500979836 ) ) ;
#81940 = AXIS2_PLACEMENT_3D ( 'NONE', #76900, #103169, #94791 ) ;
#81939 = DIRECTION ( 'NONE',  ( -0.9455185755993178454, 0.000000000000000000, 0.3255681544571537578 ) ) ;
#81941 = CARTESIAN_POINT ( 'NONE',  ( -109.9698195215979979, 1384.452562162210143, 311.4357956501490321 ) ) ;
#81942 = CARTESIAN_POINT ( 'NONE',  ( -17.71193100849139768, 1519.551704408389924, 221.5709757781449980 ) ) ;
#81943 = CARTESIAN_POINT ( 'NONE',  ( -29.04272165705700459, 1384.831948739079962, 227.0851056154090202 ) ) ;
#81944 = LINE ( 'NONE', #14186, #71543 ) ;
#81945 = CARTESIAN_POINT ( 'NONE',  ( -4.075310406729379942, 1517.051704406860154, 216.1877156734769869 ) ) ;
#81946 = CARTESIAN_POINT ( 'NONE',  ( 12.31857963777959952, 1491.958284206870076, 208.7100351509869824 ) ) ;
#81947 = CARTESIAN_POINT ( 'NONE',  ( 4.987078442593329441, 1508.551704408389924, 206.6339108768089829 ) ) ;
#81948 = CARTESIAN_POINT ( 'NONE',  ( 8.431940979592114971, 1511.395336166478046, 204.3955032846177460 ) ) ;
#81949 = CARTESIAN_POINT ( 'NONE',  ( -21.78142531070000132, 1409.673684521329960, 204.2523482604379694 ) ) ;
#81950 = CARTESIAN_POINT ( 'NONE',  ( -15.06420487680200004, 1422.389038249511941, 229.4662359065569888 ) ) ;
#81951 = CARTESIAN_POINT ( 'NONE',  ( -43.65584475269999842, 1432.560345650309955, 269.7151603323979998 ) ) ;
#81952 = VERTEX_POINT ( 'NONE', #46887 ) ;
#81953 = CARTESIAN_POINT ( 'NONE',  ( -11.90018169985392760, 1410.698182860651514, 228.4914053468817201 ) ) ;
#81954 = CARTESIAN_POINT ( 'NONE',  ( 21.62164173326539895, 1519.551704408389924, 208.0273405521070060 ) ) ;
#81955 = CARTESIAN_POINT ( 'NONE',  ( 18.99432372851790163, 1459.501274160539879, 220.3864141097060099 ) ) ;
#81957 = CARTESIAN_POINT ( 'NONE',  ( -10.96771875526499862, 1512.594959757389915, 193.2043797466670014 ) ) ;
#81956 = FACE_OUTER_BOUND ( 'NONE', #39828, .T. ) ;
#81958 = CARTESIAN_POINT ( 'NONE',  ( -0.5000000000076130213, 1448.894380913990062, 155.6080925171820013 ) ) ;
#81959 = CARTESIAN_POINT ( 'NONE',  ( -5.616639813079999932, 1453.118421927689951, 200.7460651932889846 ) ) ;
#81960 = CARTESIAN_POINT ( 'NONE',  ( 5.002593359325000044, 1516.960844870249957, 202.5626772953570196 ) ) ;
#81961 = CARTESIAN_POINT ( 'NONE',  ( 7.671698190030000752, 1427.928538830389925, 213.1259091499790088 ) ) ;
#81962 = CARTESIAN_POINT ( 'NONE',  ( -0.03315926146910300187, 1502.038558776489936, 233.2541124319990047 ) ) ;
#81963 = CARTESIAN_POINT ( 'NONE',  ( 16.22329229643499815, 1513.248517198770060, 194.7967040231669955 ) ) ;
#81964 = FACE_BOUND ( 'NONE', #50428, .T. ) ;
#81965 = CARTESIAN_POINT ( 'NONE',  ( -67.87968102602539489, 1379.746884770850102, 281.0430582061820246 ) ) ;
#81966 = CARTESIAN_POINT ( 'NONE',  ( 8.251048879689999893, 1367.474174444410210, 207.6218459616989946 ) ) ;
#81968 = VERTEX_POINT ( 'NONE', #90503 ) ;
#81967 = CARTESIAN_POINT ( 'NONE',  ( 9.196765935889999355, 1453.799101180989965, 213.5670157982789874 ) ) ;
#81969 = ORIENTED_EDGE ( 'NONE', *, *, #105576, .F. ) ;
#81970 = CARTESIAN_POINT ( 'NONE',  ( -9.292968016810000620, 1396.237577981529967, 201.9577587458279879 ) ) ;
#81971 = CARTESIAN_POINT ( 'NONE',  ( -19.78018474210000122, 1409.768243630330062, 220.0095457091979938 ) ) ;
#81972 = CARTESIAN_POINT ( 'NONE',  ( -1.499137190340000148, 1414.988017874730076, 226.5174424890980163 ) ) ;
#81973 = CARTESIAN_POINT ( 'NONE',  ( -13.26789768477497233, 1444.630613151548005, 169.3822729539114107 ) ) ;
#81974 = CARTESIAN_POINT ( 'NONE',  ( -10.26338073471560008, 1519.551704408389924, 184.6900425920350131 ) ) ;
#81975 = CARTESIAN_POINT ( 'NONE',  ( -19.66678637246580053, 1517.051704408389924, 215.8936635744080093 ) ) ;
#81977 = CARTESIAN_POINT ( 'NONE',  ( 17.68836376279999811, 1413.554570832630134, 224.8857514005979965 ) ) ;
#81976 = CARTESIAN_POINT ( 'NONE',  ( -7.647431551520000426, 1383.749817281759988, 218.9711582107190111 ) ) ;
#81978 = CARTESIAN_POINT ( 'NONE',  ( 3.793927053430000473, 1429.768419767629894, 185.0899286004980127 ) ) ;
#81979 = CARTESIAN_POINT ( 'NONE',  ( -33.28034951413935971, 1522.382868172863937, 200.8029765415142549 ) ) ;
#81980 = CARTESIAN_POINT ( 'NONE',  ( -38.43251260839529948, 1449.162497472070072, 136.3062348396100276 ) ) ;
#81981 =( LENGTH_UNIT ( ) NAMED_UNIT ( * ) SI_UNIT ( .MILLI., .METRE. ) );
#81982 = CARTESIAN_POINT ( 'NONE',  ( 6.667638404474650393, 1396.145899509130004, 200.3161284921849870 ) ) ;
#81983 = CARTESIAN_POINT ( 'NONE',  ( 1.547930050009999947, 1416.311719782429918, 190.2897677825980054 ) ) ;
#81984 = CARTESIAN_POINT ( 'NONE',  ( 11.75041584140000062, 1430.875550170730094, 150.6471352439980080 ) ) ;
#81985 = CARTESIAN_POINT ( 'NONE',  ( 7.449529084515000399, 1511.198876514819858, 202.8590003749670245 ) ) ;
#81986 = VERTEX_POINT ( 'NONE', #81013 ) ;
#81987 = CARTESIAN_POINT ( 'NONE',  ( -16.89460221417084895, 1526.348417187220775, 183.3360764755740604 ) ) ;
#81988 = CARTESIAN_POINT ( 'NONE',  ( 21.80586122363390800, 1523.954914175592421, 234.9031843411586635 ) ) ;
#81989 = ORIENTED_EDGE ( 'NONE', *, *, #44202, .F. ) ;
#81990 = ORIENTED_EDGE ( 'NONE', *, *, #47932, .F. ) ;
#81991 = FACE_OUTER_BOUND ( 'NONE', #69488, .T. ) ;
#81992 = CARTESIAN_POINT ( 'NONE',  ( 21.04904418909999819, 1494.916427559390058, 209.1218459616989946 ) ) ;
#81993 = AXIS2_PLACEMENT_3D ( 'NONE', #2694, #63165, #71008 ) ;
#81994 = CARTESIAN_POINT ( 'NONE',  ( -109.9496004110956449, 1385.529525279795052, 311.4216302621462660 ) ) ;
#81995 = CARTESIAN_POINT ( 'NONE',  ( -28.27139721233049485, 1526.382868172864164, 198.6830693683576499 ) ) ;
#81996 = CARTESIAN_POINT ( 'NONE',  ( -5.002593397454999646, 1516.960844870249957, 215.6810146069769871 ) ) ;
#81997 = FACE_OUTER_BOUND ( 'NONE', #20983, .T. ) ;
#81998 = AXIS2_PLACEMENT_3D ( 'NONE', #64364, #64916, #55955 ) ;
#81999 = EDGE_LOOP ( 'NONE', ( #35131, #88214, #31594, #28765, #62696 ) ) ;
#82000 = FACE_OUTER_BOUND ( 'NONE', #8096, .T. ) ;
#82001 = CARTESIAN_POINT ( 'NONE',  ( -5.994742217816120267, 1509.255429174939991, 179.4820970290749926 ) ) ;
#82002 = CARTESIAN_POINT ( 'NONE',  ( -37.47102956639999860, 1376.102040661649880, 218.9879198341890003 ) ) ;
#82003 = EDGE_CURVE ( 'NONE', #69834, #21185, #82959, .T. ) ;
#82004 = CIRCLE ( 'NONE', #55262, 1.999999999999999556 ) ;
#82005 = CARTESIAN_POINT ( 'NONE',  ( 4.912414298609999896, 1414.913060387329779, 224.8486248791979847 ) ) ;
#82006 = CARTESIAN_POINT ( 'NONE',  ( 5.772727908745000747, 1516.691414181030041, 205.6645793267070133 ) ) ;
#82007 = EDGE_LOOP ( 'NONE', ( #40776, #91645, #69210, #90637, #26700 ) ) ;
#82008 = CARTESIAN_POINT ( 'NONE',  ( -4.623892098755000291, 1517.066898074209803, 208.3852847535989952 ) ) ;
#82009 = CARTESIAN_POINT ( 'NONE',  ( -20.35503715340000142, 1509.384884516829743, 229.8737127907980096 ) ) ;
#82010 = EDGE_CURVE ( 'NONE', #14771, #50836, #44408, .T. ) ;
#82011 = CARTESIAN_POINT ( 'NONE',  ( -35.04504030444321216, 1424.100410869143616, 269.5321305596128809 ) ) ;
#82012 = CARTESIAN_POINT ( 'NONE',  ( 7.101217468594999360, 1512.693483295329997, 217.4300948872370043 ) ) ;
#82014 = VERTEX_POINT ( 'NONE', #46342 ) ;
#82013 = CARTESIAN_POINT ( 'NONE',  ( -1.910180902340000111E-10, 1431.113060387329824, 190.4145386866979948 ) ) ;
#82015 = CARTESIAN_POINT ( 'NONE',  ( 5.513435558210308507, 1508.551704408385376, 216.2892291545065291 ) ) ;
#82016 = CARTESIAN_POINT ( 'NONE',  ( -30.01782267245550173, 1440.913060386890038, 238.4060211167299883 ) ) ;
#82017 = CARTESIAN_POINT ( 'NONE',  ( -89.68054741670000851, 1384.049504871620229, 308.6620857943589726 ) ) ;
#82018 = CARTESIAN_POINT ( 'NONE',  ( -0.1948764052599220031, 1466.762775982959965, 235.6169484919890067 ) ) ;
#82019 = VECTOR ( 'NONE', #72661, 1000.000000000000000 ) ;
#82020 = CARTESIAN_POINT ( 'NONE',  ( 5.207738542198760534, 1410.011340619670136, 270.0726153996189964 ) ) ;
#82021 = CARTESIAN_POINT ( 'NONE',  ( -6.547556969464999987, 1516.633288330999903, 212.3841106205370011 ) ) ;
#82022 = CARTESIAN_POINT ( 'NONE',  ( -62.19530719199999425, 1379.731596365480073, 266.2974022992590335 ) ) ;
#82023 = CARTESIAN_POINT ( 'NONE',  ( 23.26324602400000074, 1409.830269578829984, 208.8206324519090060 ) ) ;
#82024 = CARTESIAN_POINT ( 'NONE',  ( 29.36007807473302123, 1526.208281990539263, 197.7147929784462121 ) ) ;
#82025 = CARTESIAN_POINT ( 'NONE',  ( -1.003913049989999973, 1443.013031698689929, 219.0745052372589896 ) ) ;
#82026 = CARTESIAN_POINT ( 'NONE',  ( -7.709135228525060057, 1516.538255842549916, 210.9323641728119867 ) ) ;
#82027 = CARTESIAN_POINT ( 'NONE',  ( -2.477975353594999763, 1516.839862955080207, 210.2583935552169976 ) ) ;
#82028 = LINE ( 'NONE', #5332, #56283 ) ;
#82029 = CARTESIAN_POINT ( 'NONE',  ( -0.4151546846821903003, 1511.187213306747708, 174.3106345060153046 ) ) ;
#82030 = CARTESIAN_POINT ( 'NONE',  ( -106.4194572870000002, 1384.702728600540013, 311.3224507522589306 ) ) ;
#82032 = ORIENTED_EDGE ( 'NONE', *, *, #72558, .F. ) ;
#82031 = CARTESIAN_POINT ( 'NONE',  ( -32.24223533869999869, 1386.864980676749838, 229.8438144294590018 ) ) ;
#82033 = CARTESIAN_POINT ( 'NONE',  ( -54.44628037483680316, 1385.095773140109941, 270.7265002573269612 ) ) ;
#82034 = CARTESIAN_POINT ( 'NONE',  ( -10.10004869885203682, 1422.222932908413441, 135.5999999980979851 ) ) ;
#82035 = CARTESIAN_POINT ( 'NONE',  ( 0.8788404816429999933, 1417.051259547929931, 234.0243021844979978 ) ) ;
#82036 = DIRECTION ( 'NONE',  ( 0.000000000000000000, -0.7071067811865467956, 0.7071067811865481278 ) ) ;
#82037 = CARTESIAN_POINT ( 'NONE',  ( -30.44527832718667071, 1526.211523310372058, 217.1519757128520212 ) ) ;
#82038 = CARTESIAN_POINT ( 'NONE',  ( 12.61062062610000112, 1426.965819617340003, 205.9085298951989671 ) ) ;
#82039 = CARTESIAN_POINT ( 'NONE',  ( 0.9741480355934977187, 1498.705209631067646, 197.8347779590515358 ) ) ;
#82040 =( REPRESENTATION_RELATIONSHIP ('NONE','NONE', #14372, #105979 ) REPRESENTATION_RELATIONSHIP_WITH_TRANSFORMATION ( #24679 )SHAPE_REPRESENTATION_RELATIONSHIP( ) );
#82042 = CARTESIAN_POINT ( 'NONE',  ( 26.35471571933159751, 1507.985750330240080, 216.6976075425179999 ) ) ;
#82041 = CARTESIAN_POINT ( 'NONE',  ( -3.259101837015000225, 1517.102359858469754, 216.0714209178769920 ) ) ;
#82043 = CARTESIAN_POINT ( 'NONE',  ( -21.56891552722479943, 1409.666264158969852, 211.8934869078800034 ) ) ;
#82044 = CARTESIAN_POINT ( 'NONE',  ( -3.347801439296144377, 1523.456872492435195, 176.1543725841967500 ) ) ;
#82045 = VERTEX_POINT ( 'NONE', #13232 ) ;
#82046 = CARTESIAN_POINT ( 'NONE',  ( -7.329925260535000042, 1516.833976295079992, 201.4049670291269933 ) ) ;
#82047 = CARTESIAN_POINT ( 'NONE',  ( -18.89959486414000267, 1416.839692127460012, 207.5749783441650038 ) ) ;
#82048 = VERTEX_POINT ( 'NONE', #47962 ) ;
#82049 = AXIS2_PLACEMENT_3D ( 'NONE', #49326, #50979, #60492 ) ;
#82050 = CARTESIAN_POINT ( 'NONE',  ( 16.73628186595838940, 1526.382868172863937, 234.1845039693043589 ) ) ;
#82051 = CARTESIAN_POINT ( 'NONE',  ( 10.88378871588750130, 1461.622812891039985, 210.4881833553409933 ) ) ;
#82052 = CARTESIAN_POINT ( 'NONE',  ( 8.953637812627370351, 1424.991390415354317, 195.6949955708311109 ) ) ;
#82053 = CARTESIAN_POINT ( 'NONE',  ( 2.589115358950000001, 1442.050439910990008, 217.9721093094690048 ) ) ;
#82054 = CARTESIAN_POINT ( 'NONE',  ( 16.30864140254039896, 1421.541993608423809, 227.2433116674564815 ) ) ;
#82055 = AXIS2_PLACEMENT_3D ( 'NONE', #49348, #6768, #106490 ) ;
#82056 = CARTESIAN_POINT ( 'NONE',  ( -2.500000000000000000, 1448.555988483530200, 159.6014995286979854 ) ) ;
#82057 = CARTESIAN_POINT ( 'NONE',  ( -19.81820729400000403, 1426.896038699130031, 223.1116520403979848 ) ) ;
#82058 = CARTESIAN_POINT ( 'NONE',  ( -27.08407403294973292, 1468.437741058713527, 269.4108308351487722 ) ) ;
#82059 = CARTESIAN_POINT ( 'NONE',  ( -105.9703572220000041, 1389.071254289390254, 299.6216621737590344 ) ) ;
#82060 = CARTESIAN_POINT ( 'NONE',  ( 19.93327782750000310, 1507.860201549930025, 189.0376985353979933 ) ) ;
#82062 = CARTESIAN_POINT ( 'NONE',  ( -18.44338626690686667, 1436.494772525281178, 212.9881102422318975 ) ) ;
#82061 = LINE ( 'NONE', #65295, #89461 ) ;
#82063 = CARTESIAN_POINT ( 'NONE',  ( -16.10306942921122797, 1469.090033419330666, 269.3694949584788674 ) ) ;
#82064 = ORIENTED_EDGE ( 'NONE', *, *, #22282, .F. ) ;
#82065 = CARTESIAN_POINT ( 'NONE',  ( -105.5164974550000068, 1378.552361626299898, 303.6894019292590201 ) ) ;
#82066 = CARTESIAN_POINT ( 'NONE',  ( 28.77730036989999718, 1509.917985860129875, 206.0039977793879871 ) ) ;
#82067 = DIRECTION ( 'NONE',  ( 0.9996573249755689172, 0.02617694830742899742, -1.602875797806941134E-18 ) ) ;
#82068 = CARTESIAN_POINT ( 'NONE',  ( -24.20882931179999886, 1435.739118266630157, 210.8967388383280195 ) ) ;
#82069 = CARTESIAN_POINT ( 'NONE',  ( 10.24015526565915124, 1427.983981843523225, 211.5553936737110519 ) ) ;
#82070 = VECTOR ( 'NONE', #65299, 1000.000000000000000 ) ;
#82071 = CARTESIAN_POINT ( 'NONE',  ( 1.455449434017229926, 1500.378593733119942, 181.4070823815799827 ) ) ;
#82072 = CARTESIAN_POINT ( 'NONE',  ( 11.60004869885203682, 1428.983126981193436, 134.0999999980966777 ) ) ;
#82073 = CARTESIAN_POINT ( 'NONE',  ( -13.33896809004436790, 1444.529557431482772, 186.7949707955224312 ) ) ;
#82074 = DIRECTION ( 'NONE',  ( 0.000000000000000000, -1.000000000000000000, 0.000000000000000000 ) ) ;
#82075 = DIRECTION ( 'NONE',  ( 0.000000000000000000, 1.000000000000000000, 0.000000000000000000 ) ) ;
#82076 = AXIS2_PLACEMENT_3D ( 'NONE', #44755, #20603, #27374 ) ;
#82077 = CARTESIAN_POINT ( 'NONE',  ( -4.161595075237580765, 1448.982995846620042, 185.0801961897900298 ) ) ;
#82078 = CARTESIAN_POINT ( 'NONE',  ( -105.8349242470570033, 1383.760197502439951, 311.0348730228309932 ) ) ;
#82079 = AXIS2_PLACEMENT_3D ( 'NONE', #9647, #43822, #3495 ) ;
#82080 = EDGE_CURVE ( 'NONE', #105138, #102452, #41518, .T. ) ;
#82081 = CARTESIAN_POINT ( 'NONE',  ( -9.579393573437259946, 1460.145585854909996, 210.2509438530599937 ) ) ;
#82082 =( BOUNDED_CURVE ( )  B_SPLINE_CURVE ( 3, ( #54709, #81513, #97228, #53605 ),
 .UNSPECIFIED., .F., .T. ) 
 B_SPLINE_CURVE_WITH_KNOTS ( ( 4, 4 ),
 ( 3.325826778622074986, 4.046911212262204849 ),
 .UNSPECIFIED. ) 
 CURVE ( )  GEOMETRIC_REPRESENTATION_ITEM ( )  RATIONAL_B_SPLINE_CURVE ( ( 1.000000000000000000, 0.9571371180642251897, 0.9571371180642251897, 1.000000000000000000 ) ) 
 REPRESENTATION_ITEM ( '' )  );
#82083 = CARTESIAN_POINT ( 'NONE',  ( 0.1763907685423009852, 1516.984411380839902, 201.4010288749069844 ) ) ;
#82085 = ORIENTED_EDGE ( 'NONE', *, *, #34316, .F. ) ;
#82084 = CARTESIAN_POINT ( 'NONE',  ( -14.12346018160000050, 1409.573557975030099, 226.3109121399980097 ) ) ;
#82086 = CARTESIAN_POINT ( 'NONE',  ( -89.71137825399999599, 1383.770488589559818, 308.5740051020589476 ) ) ;
#82087 = EDGE_CURVE ( 'NONE', #20697, #37122, #101591, .T. ) ;
#82088 = CARTESIAN_POINT ( 'NONE',  ( 14.81380078118680110, 1513.941944658630064, 224.0275431902680054 ) ) ;
#82089 = ORIENTED_EDGE ( 'NONE', *, *, #63343, .T. ) ;
#82090 = ORIENTED_EDGE ( 'NONE', *, *, #11205, .T. ) ;
#82091 = ADVANCED_FACE ( 'NONE', ( #42311 ), #41214, .F. ) ;
#82092 = CARTESIAN_POINT ( 'NONE',  ( 17.98384814369790163, 1416.218865267220053, 208.9184880541960183 ) ) ;
#82093 = CARTESIAN_POINT ( 'NONE',  ( 5.421019186268996037, 1516.848040087860227, 203.8236974790748945 ) ) ;
#82095 = CARTESIAN_POINT ( 'NONE',  ( -33.66409354910000218, 1447.474031025510158, 250.0355534335980110 ) ) ;
#82094 = CARTESIAN_POINT ( 'NONE',  ( 2.966112986920000250, 1454.352909205089873, 218.0484514319589948 ) ) ;
#82096 = CARTESIAN_POINT ( 'NONE',  ( -20.00014847029999743, 1494.489802793330000, 189.8466569891980100 ) ) ;
#82097 = CARTESIAN_POINT ( 'NONE',  ( -11.16957869839999873, 1433.751945839420159, 151.6334640592980065 ) ) ;
#82098 = B_SPLINE_CURVE_WITH_KNOTS ( 'NONE', 3,
 ( #19984, #45221, #80461, #63144, #3225, #71551, #36798, #105106, #46331, #70990, #55275, #3774, #61470, #97245, #95596, #28397, #89405, #37907, #18865, #20520, #53062, #87199, #79912, #10491, #2673, #45777, #62597, #54178, #103991, #78803, #54727, #53627, #79359, #12139, #96147, #96714, #37352, #105672, #88855, #12693, #44662, #2118, #72089, #4309, #87769, #36244, #88306, #104550, #106203, #11050 ),
 .UNSPECIFIED., .F., .F.,
 ( 4, 2, 2, 2, 2, 1, 2, 2, 2, 1, 1, 1, 2, 2, 2, 2, 1, 1, 2, 2, 2, 2, 2, 1, 1, 2, 2, 2, 4 ),
 ( 0.000000000000000000, 0.06250000000146122003, 0.09375000000219183005, 0.1250000000029224401, 0.1875000000044818871, 0.2187500000051815496, 0.2343750000056289418, 0.2500000000060763061, 0.3125000000082249763, 0.3437500000092993391, 0.3593750000099265596, 0.3671875000101492703, 0.3710937500102622910, 0.3750000000103753672, 0.4375000000113411502, 0.4687500000119324550, 0.4843750000122225008, 0.4921875000121107568, 0.4960937500120483068, 0.5000000000119858568, 0.5625000000117040821, 0.6250000000114224186, 0.6875000000111406440, 0.7187500000109988685, 0.7343750000110760290, 0.7421875000109645626, 0.7500000000108530962, 0.8750000000054265481, 1.000000000000000000 ),
 .UNSPECIFIED. ) ;
#82099 = DIRECTION ( 'NONE',  ( 1.000000000000000000, 0.000000000000000000, 0.000000000000000000 ) ) ;
#82100 = CARTESIAN_POINT ( 'NONE',  ( 11.73700276280139931, 1426.696010850159837, 144.1682878426319974 ) ) ;
#82101 = AXIS2_PLACEMENT_3D ( 'NONE', #812, #24321, #60733 ) ;
#82102 = CARTESIAN_POINT ( 'NONE',  ( 9.420227998632439537, 1464.385042586709915, 211.9321054643539810 ) ) ;
#82103 = CARTESIAN_POINT ( 'NONE',  ( -26.91513731259999886, 1437.386455222429959, 136.8516220636979881 ) ) ;
#82104 = CARTESIAN_POINT ( 'NONE',  ( 1.037000659087049748, 1515.105800736289893, 213.4502209092399880 ) ) ;
#82105 = CARTESIAN_POINT ( 'NONE',  ( -20.06033034266364368, 1526.189892541618974, 185.1817216005363491 ) ) ;
#82106 = CARTESIAN_POINT ( 'NONE',  ( 13.15094574255949844, 1428.684587356050088, 223.1532025252389815 ) ) ;
#82107 = CARTESIAN_POINT ( 'NONE',  ( -2.380813228430795903, 1360.502616939869995, 210.6218459616987957 ) ) ;
#82108 = CARTESIAN_POINT ( 'NONE',  ( -11.21381126459350419, 1509.429652529044688, 236.9473696240944776 ) ) ;
#82110 = ORIENTED_EDGE ( 'NONE', *, *, #65263, .T. ) ;
#82109 = CARTESIAN_POINT ( 'NONE',  ( 1.547888423906569751E-08, 1407.594100959480102, 263.8350914467960138 ) ) ;
#82111 = ORIENTED_EDGE ( 'NONE', *, *, #60512, .F. ) ;
#82112 = CARTESIAN_POINT ( 'NONE',  ( -11.86023832827350155, 1431.926758601109896, 149.9669891830439781 ) ) ;
#82113 = CARTESIAN_POINT ( 'NONE',  ( 13.81351351143439921, 1499.702438827800052, 227.7632555812340058 ) ) ;
#82114 = CARTESIAN_POINT ( 'NONE',  ( -13.22859606919999997, 1471.163352849629973, 270.3663863922980681 ) ) ;
#82115 = CARTESIAN_POINT ( 'NONE',  ( -0.3246279079737399709, 1473.616300012054353, 219.3513874934918420 ) ) ;
#82116 = CARTESIAN_POINT ( 'NONE',  ( -124.5778210737999956, 1377.418846546390114, 304.2218459572590064 ) ) ;
#82117 = CARTESIAN_POINT ( 'NONE',  ( 35.94911020107750232, 1451.437441929419947, 135.1301813102820120 ) ) ;
#82118 = CARTESIAN_POINT ( 'NONE',  ( 0.2184868517783540021, 1451.777963835670107, 182.9107317036869915 ) ) ;
#82119 = CARTESIAN_POINT ( 'NONE',  ( -19.97968237250000101, 1483.906011188890034, 214.0068283976289933 ) ) ;
#82120 = CARTESIAN_POINT ( 'NONE',  ( 17.76546875260000036, 1430.865606781589804, 204.9340536459789917 ) ) ;
#82121 = CARTESIAN_POINT ( 'NONE',  ( -3.094819429390000209, 1457.827881892290179, 218.9172904726289914 ) ) ;
#82122 = CARTESIAN_POINT ( 'NONE',  ( 10.02176186330000007, 1364.879735892739973, 207.6218459616989946 ) ) ;
#82123 = CARTESIAN_POINT ( 'NONE',  ( -41.97207030135130168, 1426.354619028159959, 266.5340502157400238 ) ) ;
#82124 = ORIENTED_EDGE ( 'NONE', *, *, #105655, .T. ) ;
#82125 = CARTESIAN_POINT ( 'NONE',  ( -24.44537314746287393, 1442.730589020610978, 210.9654079490763650 ) ) ;
#82126 = B_SPLINE_CURVE_WITH_KNOTS ( 'NONE', 3,
 ( #1712, #95199, #37497, #27992, #105254, #35852, #18460, #36936, #2817, #62177, #28548, #62747, #45913, #45373, #79513, #2277, #53216, #35289, #71133 ),
 .UNSPECIFIED., .F., .F.,
 ( 4, 3, 3, 3, 3, 3, 4 ),
 ( -8.078122936479999794, -7.682761468106989788, -6.749878609470029822, -5.846755267555650448, -4.962182452275140321, -4.110507351632660011, -3.282019784874940171 ),
 .UNSPECIFIED. ) ;
#82127 = ORIENTED_EDGE ( 'NONE', *, *, #104887, .F. ) ;
#82128 = ORIENTED_EDGE ( 'NONE', *, *, #23951, .T. ) ;
#82129 = CARTESIAN_POINT ( 'NONE',  ( 1.136814033864999907, 1516.854133554269993, 211.4058994415870245 ) ) ;
#82130 = CARTESIAN_POINT ( 'NONE',  ( 4.906730394725735245, 1423.390749761640336, 184.2167557326281440 ) ) ;
#82132 = DIRECTION ( 'NONE',  ( 0.000000000000000000, 0.000000000000000000, 1.000000000000000000 ) ) ;
#82131 = CARTESIAN_POINT ( 'NONE',  ( 6.560742225334999844, 1517.028034847769959, 213.1554992345569701 ) ) ;
#82133 = CARTESIAN_POINT ( 'NONE',  ( -15.67917309240000279, 1455.451896433330148, 188.9440702688980025 ) ) ;
#82134 = AXIS2_PLACEMENT_3D ( 'NONE', #101018, #24316, #89204 ) ;
#82135 = CARTESIAN_POINT ( 'NONE',  ( -18.26532265589999682, 1415.628674266529742, 208.3526068587169959 ) ) ;
#82136 = B_SPLINE_SURFACE_WITH_KNOTS ( 'NONE', 5, 1, ( 
 ( #85206, #42668 ),
 ( #76824, #139 ),
 ( #44903, #10731 ),
 ( #79051, #97479 ),
 ( #20208, #63364 ),
 ( #37574, #2353 ),
 ( #38118, #71211 ),
 ( #29715, #2898 ),
 ( #54945, #89072 ) ),
 .UNSPECIFIED., .F., .F., .F.,
 ( 6, 3, 6 ),
 ( 2, 2 ),
 ( -1.085177091614590055E-05, 35.35713585580000284, 84.36278594678920228 ),
 ( 2.018291180219999870, 3.029423978413739782 ),
 .UNSPECIFIED. ) ;
#82137 = EDGE_LOOP ( 'NONE', ( #99081, #79158 ) ) ;
#82138 = CARTESIAN_POINT ( 'NONE',  ( -26.80348844950000142, 1436.439654078439844, 136.7215874007980005 ) ) ;
#82139 = CARTESIAN_POINT ( 'NONE',  ( -4.036119682645000317, 1516.647924054489977, 201.7978713257969900 ) ) ;
#82140 = AXIS2_PLACEMENT_3D ( 'NONE', #83861, #107959, #49730 ) ;
#82141 = EDGE_CURVE ( 'NONE', #19394, #97755, #21452, .T. ) ;
#82142 = DIRECTION ( 'NONE',  ( -0.4978433412588781914, 0.000000000000000000, -0.8672669759446606230 ) ) ;
#82143 = CARTESIAN_POINT ( 'NONE',  ( -9.721399282128558639, 1384.510033814309963, 200.0150085476490176 ) ) ;
#82144 = CARTESIAN_POINT ( 'NONE',  ( -35.38898509910070089, 1419.603228493539973, 269.8627298453310459 ) ) ;
#82145 = CARTESIAN_POINT ( 'NONE',  ( -17.84054674790984052, 1523.580204110583281, 180.3625987835359581 ) ) ;
#82146 = CARTESIAN_POINT ( 'NONE',  ( -3.841870597909999852, 1398.027800385929822, 196.5971685358980210 ) ) ;
#82148 = ORIENTED_EDGE ( 'NONE', *, *, #76837, .F. ) ;
#82147 = CARTESIAN_POINT ( 'NONE',  ( -9.832966357676340863, 1364.062280235945991, 210.6218459616987957 ) ) ;
#82149 = ORIENTED_EDGE ( 'NONE', *, *, #8708, .T. ) ;
#82150 = CARTESIAN_POINT ( 'NONE',  ( 0.3919059719699999889, 1450.899374729219971, 181.2708615468980042 ) ) ;
#82151 = CARTESIAN_POINT ( 'NONE',  ( 17.17241001986506888, 1518.913060387330006, 237.6251415217915337 ) ) ;
#82152 = CARTESIAN_POINT ( 'NONE',  ( 0.6257610854233279785, 1425.690485377240066, 191.1046958424169873 ) ) ;
#82153 = CARTESIAN_POINT ( 'NONE',  ( -13.28075528932130212, 1436.102060238340073, 150.6141327710369922 ) ) ;
#82154 = CARTESIAN_POINT ( 'NONE',  ( -0.03626856688976699827, 1409.963246368600039, 185.0759526402830204 ) ) ;
#82156 = CARTESIAN_POINT ( 'NONE',  ( 5.013429356055000063, 1517.123342927159911, 210.2437967141769946 ) ) ;
#82155 = AXIS2_PLACEMENT_3D ( 'NONE', #31101, #79871, #98306 ) ;
#82157 = CARTESIAN_POINT ( 'NONE',  ( -68.75569806500000425, 1379.747887185579884, 280.1327824861590443 ) ) ;
#82158 = CARTESIAN_POINT ( 'NONE',  ( -18.20274223739999897, 1435.778903725820101, 226.4112149876980027 ) ) ;
#82159 = DIRECTION ( 'NONE',  ( 0.000000000000000000, 0.000000000000000000, 1.000000000000000000 ) ) ;
#82160 = CARTESIAN_POINT ( 'NONE',  ( 2.589235753919999445E-16, 1524.551704408390151, 209.1218459616989946 ) ) ;
#82161 = CARTESIAN_POINT ( 'NONE',  ( 8.245978508674999929, 1511.399604276809896, 204.0113757433670116 ) ) ;
#82162 = CARTESIAN_POINT ( 'NONE',  ( 5.772978278544999675, 1516.659138130710289, 207.9900491214870044 ) ) ;
#82163 = EDGE_LOOP ( 'NONE', ( #40592, #102197, #26557, #71174 ) ) ;
#82164 = CARTESIAN_POINT ( 'NONE',  ( 9.833393186232889605, 1517.151704408390060, 205.7359371553449989 ) ) ;
#82165 = CARTESIAN_POINT ( 'NONE',  ( -11.59417537721629898, 1428.981093291590014, 133.6116858579929954 ) ) ;
#82166 = CARTESIAN_POINT ( 'NONE',  ( -23.74203090515832315, 1447.138914774234763, 214.4317863515268527 ) ) ;
#82167 = ORIENTED_EDGE ( 'NONE', *, *, #9021, .F. ) ;
#82168 = CARTESIAN_POINT ( 'NONE',  ( 9.932046507237075161, 1455.482931264669332, 226.5863170123957957 ) ) ;
#82169 = CARTESIAN_POINT ( 'NONE',  ( -5.261498365895931784, 1483.803119626035141, 199.8297041156830858 ) ) ;
#82170 = CARTESIAN_POINT ( 'NONE',  ( -4.127455358014529452, 1439.932934338472933, 185.4683297619992288 ) ) ;
#82171 = CARTESIAN_POINT ( 'NONE',  ( -2.920887357330470113, 1416.480278474030001, 186.3404578197399815 ) ) ;
#82172 = CARTESIAN_POINT ( 'NONE',  ( 21.06805239210000380, 1409.648772995130003, 203.5068327927779990 ) ) ;
#82173 = CARTESIAN_POINT ( 'NONE',  ( 6.372167600494999640, 1511.069621805459974, 216.5183910133270047 ) ) ;
#82174 = CARTESIAN_POINT ( 'NONE',  ( -14.07280436816861169, 1379.603689006211425, 211.7284150537196865 ) ) ;
#82175 = CARTESIAN_POINT ( 'NONE',  ( -3.996325623589930043, 1476.488318328419837, 199.5621885948499710 ) ) ;
#82176 = CARTESIAN_POINT ( 'NONE',  ( 4.248370253470151070, 1441.364699327820063, 161.3861545211829878 ) ) ;
#82177 = ADVANCED_FACE ( 'NONE', ( #108416, #65882, #14889, #40104, #66983, #31700, #100003, #23836, #74831, #23291, #50185, #108974, #41757, #31148, #49628, #83215, #66440, #100556, #109523, #92163, #75386, #7059, #15436, #101094, #24393, #92706, #15983, #84311, #7603, #75916, #33344, #67539, #93260, #16524, #65336, #22721, #77032, #61906, #886, #59680, #70313, #10926, #94349, #68096, #9811, #9269, #19295, #26603, #95477, #96024 ), #52938, .F. ) ;
#82178 = AXIS2_PLACEMENT_3D ( 'NONE', #40637, #72602, #47943 ) ;
#82179 = DIRECTION ( 'NONE',  ( 0.000000000000000000, 1.000000000000000000, 0.000000000000000000 ) ) ;
#82180 = CARTESIAN_POINT ( 'NONE',  ( -3.955028505459999653E-16, 1420.349145488430167, 170.8340916043979973 ) ) ;
#82181 = CARTESIAN_POINT ( 'NONE',  ( 1.708720984574999768, 1516.531533746980131, 216.4430152012269843 ) ) ;
#82182 = ORIENTED_EDGE ( 'NONE', *, *, #17853, .F. ) ;
#82183 = CARTESIAN_POINT ( 'NONE',  ( 7.717523752519699798, 1516.858602105719910, 208.8606392115019901 ) ) ;
#82184 = LINE ( 'NONE', #30120, #62392 ) ;
#82185 = DIRECTION ( 'NONE',  ( 0.07713599384728295205, -0.9969860201949398704, 0.008301444997532481801 ) ) ;
#82186 = CARTESIAN_POINT ( 'NONE',  ( 1.931781262533000117E-14, 1421.852997280460158, 133.5964121027310227 ) ) ;
#82187 = CARTESIAN_POINT ( 'NONE',  ( -0.05388807208240130320, 1474.848271548789853, 219.8071399965990054 ) ) ;
#82188 = CARTESIAN_POINT ( 'NONE',  ( 11.60004869885203682, 1426.444849425687153, 138.8727431505155323 ) ) ;
#82189 = AXIS2_PLACEMENT_3D ( 'NONE', #64631, #105095, #10480 ) ;
#82190 = CARTESIAN_POINT ( 'NONE',  ( -2.146337792930170352, 1464.869601414239924, 183.9517861855029821 ) ) ;
#82191 = CARTESIAN_POINT ( 'NONE',  ( 1.222622250163819757, 1456.171658986630064, 198.6221278460869826 ) ) ;
#82192 = CARTESIAN_POINT ( 'NONE',  ( 31.68651911954009748, 1440.913060383499896, 243.2846231541469990 ) ) ;
#82193 = FACE_OUTER_BOUND ( 'NONE', #19281, .T. ) ;
#82194 = CARTESIAN_POINT ( 'NONE',  ( 10.15366035715699944, 1499.165878262429942, 202.2600268113060054 ) ) ;
#82195 = EDGE_LOOP ( 'NONE', ( #73758, #3417, #15176, #66680 ) ) ;
#82196 = ORIENTED_EDGE ( 'NONE', *, *, #63454, .T. ) ;
#82197 = CARTESIAN_POINT ( 'NONE',  ( -5.513435911474870110, 1508.551704408389924, 202.1089243664339961 ) ) ;
#82198 = CARTESIAN_POINT ( 'NONE',  ( 2.038847259689231084, 1501.977400791986611, 173.3106345060153046 ) ) ;
#82199 = B_SPLINE_CURVE_WITH_KNOTS ( 'NONE', 3,
 ( #91595, #66966, #82650, #5941, #14871, #66423, #49062, #75900, #6486, #108397, #75367, #8129, #40087, #40638, #7038, #107841, #83742, #74810, #24910, #41196, #109506, #67521, #92688, #59119, #31680, #93242, #101076, #15965, #31130, #32242, #65862, #16508, #100538, #65312, #23818, #99425, #26587, #61342, #96007, #68078, #43413, #87055, #18725, #86498, #42857, #78102, #70298, #102191, #69174, #27704 ),
 .UNSPECIFIED., .F., .F.,
 ( 4, 2, 2, 2, 2, 1, 2, 2, 2, 1, 1, 1, 2, 2, 2, 2, 1, 1, 2, 2, 2, 2, 2, 1, 1, 2, 2, 2, 4 ),
 ( 0.000000000000000000, 0.06249999999685171281, 0.09374999999528567385, 0.1249999999937196349, 0.1874999999906944714, 0.2187499999891768243, 0.2343749999883256441, 0.2499999999874744638, 0.3124999999842543175, 0.3437499999827312580, 0.3593749999820591845, 0.3671874999817218432, 0.3710937499815532004, 0.3749999999813845020, 0.4374999999794075278, 0.4687499999785326721, 0.4843749999780995186, 0.4921874999781875037, 0.4960937499782315796, 0.4999999999782755999, 0.5624999999801301165, 0.6249999999819845220, 0.6874999999838390385, 0.7187499999849091825, 0.7343749999852986488, 0.7421874999854947141, 0.7499999999856906685, 0.8749999999928452787, 1.000000000000000000 ),
 .UNSPECIFIED. ) ;
#82200 = CARTESIAN_POINT ( 'NONE',  ( -4.545411974820000367, 1442.929234760589907, 200.6103434261889902 ) ) ;
#82201 = CARTESIAN_POINT ( 'NONE',  ( 11.63908763273079927, 1501.958057524839887, 211.3995250518869966 ) ) ;
#82202 = CARTESIAN_POINT ( 'NONE',  ( -5.864566082395450408, 1517.151704408390060, 192.0899093523580063 ) ) ;
#82203 = CARTESIAN_POINT ( 'NONE',  ( -10.48189203859999985, 1491.372288729389993, 212.4833772739189897 ) ) ;
#82204 = CARTESIAN_POINT ( 'NONE',  ( -1.754297334879579839, 1508.551704408389924, 220.0788184290720153 ) ) ;
#82205 = CARTESIAN_POINT ( 'NONE',  ( -44.03378961160060356, 1383.821754830599957, 249.2544531064709759 ) ) ;
#82206 = EDGE_CURVE ( 'NONE', #83491, #9501, #90899, .T. ) ;
#82207 = CARTESIAN_POINT ( 'NONE',  ( -4.832611099234620511, 1508.551704408389924, 206.6339241720520192 ) ) ;
#82208 = EDGE_CURVE ( 'NONE', #60200, #12639, #93792, .T. ) ;
#82209 = CARTESIAN_POINT ( 'NONE',  ( -14.56367227959999866, 1489.468502498129965, 192.4084369560980008 ) ) ;
#82210 = CARTESIAN_POINT ( 'NONE',  ( -8.998910544736714812, 1424.786834349990158, 213.7129700835037909 ) ) ;
#82211 = CARTESIAN_POINT ( 'NONE',  ( 1.412514030800000153, 1466.019513801129960, 235.1197556243980102 ) ) ;
#82212 = EDGE_CURVE ( 'NONE', #71731, #41473, #27719, .T. ) ;
#82214 = ORIENTED_EDGE ( 'NONE', *, *, #82993, .T. ) ;
#82213 = CARTESIAN_POINT ( 'NONE',  ( 9.218508161488790265, 1451.411218699900019, 210.0414266177820082 ) ) ;
#82215 = CARTESIAN_POINT ( 'NONE',  ( -0.6413666067069999643, 1451.453725705629950, 182.8474195845979864 ) ) ;
#82216 = AXIS2_PLACEMENT_3D ( 'NONE', #14845, #108922, #22122 ) ;
#82217 = CARTESIAN_POINT ( 'NONE',  ( -16.11330378180000267, 1381.436043544759968, 201.9289277945890149 ) ) ;
#82218 = EDGE_CURVE ( 'NONE', #23166, #51438, #37548, .T. ) ;
#82219 = CARTESIAN_POINT ( 'NONE',  ( 3.274413360505469939, 1508.551704408389924, 204.2617222807819815 ) ) ;
#82221 = ORIENTED_EDGE ( 'NONE', *, *, #66087, .F. ) ;
#82220 = CARTESIAN_POINT ( 'NONE',  ( -16.93235272047269646, 1414.913060387399810, 207.4470167978099937 ) ) ;
#82222 = CARTESIAN_POINT ( 'NONE',  ( -19.86464697889580222, 1441.435563530799982, 212.6459098933489997 ) ) ;
#82223 = EDGE_LOOP ( 'NONE', ( #26335, #94532, #82149 ) ) ;
#82224 = EDGE_CURVE ( 'NONE', #110603, #70446, #5416, .T. ) ;
#82225 = PRODUCT ( 'Threaded Lock Nut', 'Threaded Lock Nut', '', ( #48282 ) ) ;
#82226 =( BOUNDED_SURFACE ( )  B_SPLINE_SURFACE ( 3, 2, ( 
 ( #4213, #38343, #5302 ),
 ( #104593, #107763, #73070 ),
 ( #27888, #22615, #53671 ),
 ( #98806, #11101, #78857 ),
 ( #22067, #55736, #56264 ),
 ( #13671, #2166, #81995 ) ),
 .UNSPECIFIED., .F., .F., .T. ) 
 B_SPLINE_SURFACE_WITH_KNOTS ( ( 4, 2, 4 ),
 ( 3, 3 ),
 ( 5.009014036883030485E-17, 0.001312027981647231282, 0.002624055963294412257 ),
 ( 0.000000000000000000, 1.000000000000000000 ),
 .UNSPECIFIED. ) 
 GEOMETRIC_REPRESENTATION_ITEM ( )  RATIONAL_B_SPLINE_SURFACE ( (
 ( 1.000000000000000000, 0.9376006582765964437, 1.000000000000000000),
 ( 1.000000000000000000, 0.9569320108028295246, 1.000000000000000000),
 ( 1.000000000000000000, 0.9725743441611425233, 1.000000000000000000),
 ( 1.000000000000000000, 0.9942095667143253657, 1.000000000000000000),
 ( 1.000000000000000000, 1.000043666450136204, 1.000000000000000000),
 ( 1.000000000000000000, 1.000000000000000000, 1.000000000000000000) ) ) 
 REPRESENTATION_ITEM ( '' )  SURFACE ( )  );
#82227 = CARTESIAN_POINT ( 'NONE',  ( -8.802958355110462207, 1385.645181018859830, 218.6119752371670018 ) ) ;
#82228 = CARTESIAN_POINT ( 'NONE',  ( -3.829222805975319943, 1515.551704203360032, 206.3208022964049917 ) ) ;
#82229 = DIRECTION ( 'NONE',  ( -0.02344842167732799632, -0.9996113240391217847, 0.01507887176138064667 ) ) ;
#82230 = VECTOR ( 'NONE', #28854, 1000.000000000000000 ) ;
#82232 = ADVANCED_FACE ( 'NONE', ( #52395 ), #60839, .F. ) ;
#82231 = CARTESIAN_POINT ( 'NONE',  ( -5.077892150579999431, 1463.916894568290218, 200.2638495158990111 ) ) ;
#82233 = CARTESIAN_POINT ( 'NONE',  ( -104.2256462149999976, 1380.095225975270068, 301.7641063316589793 ) ) ;
#82234 = CARTESIAN_POINT ( 'NONE',  ( -15.18835168660036139, 1420.045948940616654, 212.3480784272774713 ) ) ;
#82235 = CARTESIAN_POINT ( 'NONE',  ( 20.61516490012983027, 1509.679647908174275, 187.6627224229067394 ) ) ;
#82236 = CARTESIAN_POINT ( 'NONE',  ( 8.791545081663338479, 1409.220067906589748, 197.0144757566580154 ) ) ;
#82237 = CARTESIAN_POINT ( 'NONE',  ( 18.12291530770000136, 1425.086651382430091, 225.0935702407979875 ) ) ;
#82238 = CARTESIAN_POINT ( 'NONE',  ( 0.8259447189419999447, 1418.827400219930041, 184.7842358559980198 ) ) ;
#82239 = CARTESIAN_POINT ( 'NONE',  ( -19.59136418880000008, 1478.168253370030016, 190.6957923982980105 ) ) ;
#82240 = CARTESIAN_POINT ( 'NONE',  ( -68.73088892949999718, 1379.748097453069931, 280.1074355248589995 ) ) ;
#82241 = CIRCLE ( 'NONE', #57261, 1.000000000000000888 ) ;
#82242 = CARTESIAN_POINT ( 'NONE',  ( -2.468912052060390216, 1449.613523094110178, 183.5976281201020015 ) ) ;
#82243 = ORIENTED_EDGE ( 'NONE', *, *, #76153, .T. ) ;
#82244 = VERTEX_POINT ( 'NONE', #64654 ) ;
#82246 = ADVANCED_FACE ( 'NONE', ( #79242 ), #40143, .T. ) ;
#82245 = CARTESIAN_POINT ( 'NONE',  ( 20.71343476517535009, 1522.382868172863937, 238.3377464195763764 ) ) ;
#82247 = CARTESIAN_POINT ( 'NONE',  ( 19.76289411957749564, 1455.644449270149835, 227.1109336957369749 ) ) ;
#82248 = CARTESIAN_POINT ( 'NONE',  ( -12.68266539220000055, 1434.593723365520191, 149.3604887061979696 ) ) ;
#82249 = PLANE ( 'NONE',  #100146 ) ;
#82250 = CARTESIAN_POINT ( 'NONE',  ( -20.30854934916089860, 1498.424519700439987, 190.6632691037499967 ) ) ;
#82251 = LINE ( 'NONE', #6647, #26836 ) ;
#82252 = CARTESIAN_POINT ( 'NONE',  ( -109.2617005650000124, 1385.525553972230000, 311.2346411152590235 ) ) ;
#82253 = EDGE_CURVE ( 'NONE', #54360, #2110, #25501, .T. ) ;
#82254 = CARTESIAN_POINT ( 'NONE',  ( -8.642118163667179331, 1511.774552108250191, 215.2838205174969630 ) ) ;
#82255 = CARTESIAN_POINT ( 'NONE',  ( -7.592149787962600094, 1361.964468435472099, 210.6218459616991936 ) ) ;
#82256 = CARTESIAN_POINT ( 'NONE',  ( -46.15241011806139682, 1440.697464424330065, 268.2044778594760146 ) ) ;
#82257 = CARTESIAN_POINT ( 'NONE',  ( -18.96495392289999771, 1425.684290752429888, 226.5179610041979856 ) ) ;
#82258 = DIRECTION ( 'NONE',  ( 0.4978433412588651463, 0.000000000000000000, -0.8672669759446679505 ) ) ;
#82259 = EDGE_CURVE ( 'NONE', #714, #12462, #6888, .T. ) ;
#82260 = CARTESIAN_POINT ( 'NONE',  ( 2.865636809105000182, 1516.815173273089840, 207.9858416580370033 ) ) ;
#82261 = CARTESIAN_POINT ( 'NONE',  ( -9.241015495411470937, 1447.557127742399871, 211.4327840398769922 ) ) ;
#82262 = CARTESIAN_POINT ( 'NONE',  ( 1.286193012929579993, 1407.887988129029736, 222.3093619251160362 ) ) ;
#82263 = CARTESIAN_POINT ( 'NONE',  ( -13.42438607818310103, 1436.022353700810072, 150.5143652916869996 ) ) ;
#82264 = CYLINDRICAL_SURFACE ( 'NONE', #14042, 2.000000000000003109 ) ;
#82265 = B_SPLINE_SURFACE_WITH_KNOTS ( 'NONE', 4, 5, ( 
 ( #47471, #81593, #108467, #106264, #55883, #6005 ),
 ( #31200, #56979, #4897, #97848, #98950, #55329 ),
 ( #64284, #31750, #22224, #89462, #14387, #74339 ),
 ( #57537, #98406, #91661, #46388, #37965, #110118 ),
 ( #40709, #109574, #33390, #26523, #7653, #36054 ) ),
 .UNSPECIFIED., .F., .F., .F.,
 ( 5, 5 ),
 ( 6, 6 ),
 ( 1.756953143920000127, 12.62047352739999972 ),
 ( 0.000000000000000000, 2.000000106069999894 ),
 .UNSPECIFIED. ) ;
#82266 = CARTESIAN_POINT ( 'NONE',  ( 2.755131347899999916, 1422.216165794629887, 90.98709265669789659 ) ) ;
#82267 = CARTESIAN_POINT ( 'NONE',  ( 7.018957632036970651, 1424.891662419710201, 213.1748363253989851 ) ) ;
#82268 = EDGE_CURVE ( 'NONE', #31591, #23879, #65913, .T. ) ;
#82269 = ORIENTED_EDGE ( 'NONE', *, *, #17844, .F. ) ;
#82270 = CARTESIAN_POINT ( 'NONE',  ( 15.47923624419999911, 1416.261629425730007, 248.5133305092979867 ) ) ;
#82271 = CARTESIAN_POINT ( 'NONE',  ( -24.29269244670000205, 1508.123907548630086, 196.8922397913979978 ) ) ;
#82273 = DIRECTION ( 'NONE',  ( 1.000000000000000000, 0.000000000000000000, 0.000000000000000000 ) ) ;
#82272 = CARTESIAN_POINT ( 'NONE',  ( -0.4682527189540000023, 1458.406866031629988, 182.9037998423980014 ) ) ;
#82274 = CARTESIAN_POINT ( 'NONE',  ( 17.27558691658489920, 1507.606285602530079, 193.9884222186300065 ) ) ;
#82275 = TOROIDAL_SURFACE ( 'NONE', #53705, 3.000000000000000000, 0.5000000000000000000 ) ;
#82276 = CARTESIAN_POINT ( 'NONE',  ( -24.57380889490000087, 1432.446761552710086, 225.2495674893980038 ) ) ;
#82277 = CARTESIAN_POINT ( 'NONE',  ( -29.51415835736623450, 1509.963286984361730, 206.5299505428056932 ) ) ;
#82278 = CARTESIAN_POINT ( 'NONE',  ( -0.02516806119179999801, 1415.404723302029879, 233.4400559027980080 ) ) ;
#82279 = CARTESIAN_POINT ( 'NONE',  ( 27.84003805790000285, 1450.652436793030120, 136.4235866663979948 ) ) ;
#82280 = ORIENTED_EDGE ( 'NONE', *, *, #57744, .F. ) ;
#82281 = CARTESIAN_POINT ( 'NONE',  ( -32.78250617288050961, 1512.187213306747481, 199.9357095655695957 ) ) ;
#82282 = FACE_OUTER_BOUND ( 'NONE', #11591, .T. ) ;
#82283 = CARTESIAN_POINT ( 'NONE',  ( 13.18359814959999987, 1420.070066474529995, 228.9875191970980097 ) ) ;
#82284 = CARTESIAN_POINT ( 'NONE',  ( -5.144873395449999443, 1502.885538352589947, 229.8910404859989853 ) ) ;
#82285 = VERTEX_POINT ( 'NONE', #67964 ) ;
#82286 = ORIENTED_EDGE ( 'NONE', *, *, #20296, .F. ) ;
#82287 = CARTESIAN_POINT ( 'NONE',  ( -25.91586689989999925, 1384.961148014880109, 203.4475886829490037 ) ) ;
#82288 = CARTESIAN_POINT ( 'NONE',  ( -23.60926278007800150, 1410.014349673999959, 209.1215866734690110 ) ) ;
#82289 = ORIENTED_EDGE ( 'NONE', *, *, #12720, .F. ) ;
#82290 = CARTESIAN_POINT ( 'NONE',  ( 3.487584386345879750, 1508.551704408389924, 204.1347675156980017 ) ) ;
#82291 = DIRECTION ( 'NONE',  ( 0.9455185755993178454, 0.000000000000000000, -0.3255681544571537578 ) ) ;
#82292 = CARTESIAN_POINT ( 'NONE',  ( -22.29678302319670280, 1436.505994161930857, 142.6647499578515976 ) ) ;
#82293 = ADVANCED_FACE ( 'NONE', ( #102073 ), #16396, .T. ) ;
#82294 = LINE ( 'NONE', #97979, #63628 ) ;
#82295 = ORIENTED_EDGE ( 'NONE', *, *, #35229, .F. ) ;
#82296 = CARTESIAN_POINT ( 'NONE',  ( 44.76515501619800119, 1450.021284846529852, 267.6430847853379760 ) ) ;
#82297 = CARTESIAN_POINT ( 'NONE',  ( -12.48769551256209986, 1414.971717244350202, 220.5819595087910159 ) ) ;
#82298 = ADVANCED_FACE ( 'NONE', ( #8020 ), #18068, .F. ) ;
#82299 = CARTESIAN_POINT ( 'NONE',  ( -0.06475640353809999916, 1420.445361017130153, 182.6808671977979941 ) ) ;
#82300 = CARTESIAN_POINT ( 'NONE',  ( 2.478306819944999795, 1516.938330505699923, 205.6592251139969960 ) ) ;
#82301 = EDGE_LOOP ( 'NONE', ( #84434, #63731, #19610, #11940 ) ) ;
#82302 = CARTESIAN_POINT ( 'NONE',  ( 7.599032816436460003, 1483.004653252710114, 218.1850191645339976 ) ) ;
#82303 = AXIS2_PLACEMENT_3D ( 'NONE', #88524, #56572, #45978 ) ;
#82304 = CARTESIAN_POINT ( 'NONE',  ( 13.44976921669219649, 1443.526213651251965, 187.9650672106725722 ) ) ;
#82305 = ORIENTED_EDGE ( 'NONE', *, *, #102675, .F. ) ;
#82306 = ORIENTED_EDGE ( 'NONE', *, *, #9979, .F. ) ;
#82307 = CARTESIAN_POINT ( 'NONE',  ( -10.53021734699250089, 1480.655658436720159, 208.5952819463930155 ) ) ;
#82308 = CARTESIAN_POINT ( 'NONE',  ( -30.60906614450610874, 1526.073434386619510, 216.5595830063403753 ) ) ;
#82309 = CARTESIAN_POINT ( 'NONE',  ( -13.03156812829710098, 1512.406412988020065, 193.8931400537850038 ) ) ;
#82310 = CARTESIAN_POINT ( 'NONE',  ( 7.678176981006109791, 1452.644932538870080, 151.4245570955009725 ) ) ;
#82311 = CARTESIAN_POINT ( 'NONE',  ( 11.26371720470000071, 1420.479700322569897, 198.6834109214989894 ) ) ;
#82312 = CARTESIAN_POINT ( 'NONE',  ( -0.4261653818286619821, 1475.450763992409975, 220.5443349783510314 ) ) ;
#82313 = CARTESIAN_POINT ( 'NONE',  ( -109.6853916682353969, 1383.138375255104620, 297.1883635206749545 ) ) ;
#82314 = CARTESIAN_POINT ( 'NONE',  ( -5.117938804930000529, 1495.139203109789833, 198.3557955832989990 ) ) ;
#82315 = CYLINDRICAL_SURFACE ( 'NONE', #23134, 0.9999999999999985567 ) ;
#82317 = CARTESIAN_POINT ( 'NONE',  ( 15.86840223659999616, 1489.480617680030036, 194.0918035215979955 ) ) ;
#82316 = CARTESIAN_POINT ( 'NONE',  ( 29.30029655192925730, 1525.907212628473872, 196.8717316207785757 ) ) ;
#82318 = CARTESIAN_POINT ( 'NONE',  ( 10.85780712524829994, 1423.231738543280017, 206.8437564243029954 ) ) ;
#82319 = EDGE_CURVE ( 'NONE', #17543, #38227, #42631, .T. ) ;
#82320 = CARTESIAN_POINT ( 'NONE',  ( -9.576991855994098302, 1440.376714694789825, 206.1621517401989934 ) ) ;
#82321 = CARTESIAN_POINT ( 'NONE',  ( 7.235185706049999332, 1427.271387135730038, 145.8323558008980001 ) ) ;
#82322 = VERTEX_POINT ( 'NONE', #25355 ) ;
#82323 = CARTESIAN_POINT ( 'NONE',  ( -16.16632277704817611, 1511.187213306747708, 181.3470724465437627 ) ) ;
#82324 = AXIS2_PLACEMENT_3D ( 'NONE', #8174, #74864, #33933 ) ;
#82325 = DIRECTION ( 'NONE',  ( 0.000000000000000000, 0.000000000000000000, -1.000000000000000000 ) ) ;
#82326 = CARTESIAN_POINT ( 'NONE',  ( -79.98142976928239989, 1384.994008373050065, 303.8518676267449905 ) ) ;
#82327 = CARTESIAN_POINT ( 'NONE',  ( -8.884967209949998335, 1388.039969697709921, 200.4370767659389969 ) ) ;
#82328 = CARTESIAN_POINT ( 'NONE',  ( -15.85633924839999942, 1415.845391443659992, 209.7260009560399965 ) ) ;
#82330 = ORIENTED_EDGE ( 'NONE', *, *, #83792, .F. ) ;
#82329 = CARTESIAN_POINT ( 'NONE',  ( 10.94394802638720066, 1423.896183310979950, 203.1971050292789869 ) ) ;
#82331 = CARTESIAN_POINT ( 'NONE',  ( 3.040651188259999582, 1428.791177441289847, 216.8297566844390190 ) ) ;
#82332 = CARTESIAN_POINT ( 'NONE',  ( 16.54106930751544269, 1524.860077346004800, 237.3885273948277188 ) ) ;
#82333 = EDGE_CURVE ( 'NONE', #109428, #70222, #34759, .T. ) ;
#82334 = CARTESIAN_POINT ( 'NONE',  ( -16.81730075879999831, 1417.162083013060055, 207.4277520661289884 ) ) ;
#82335 = CARTESIAN_POINT ( 'NONE',  ( 11.93269758809999992, 1433.544831721110086, 150.2289606549979908 ) ) ;
#82336 = CARTESIAN_POINT ( 'NONE',  ( 13.66603629819999810, 1471.441739209529942, 271.1218459616979999 ) ) ;
#82337 = CARTESIAN_POINT ( 'NONE',  ( 0.7971436909562600315, 1450.873242978859935, 181.3626938088150098 ) ) ;
#82338 = MANIFOLD_SOLID_BREP ( 'Stock-MAS-682-1', #5599 ) ;
#82339 = EDGE_CURVE ( 'NONE', #78966, #365, #56954, .T. ) ;
#82340 = CARTESIAN_POINT ( 'NONE',  ( 29.00779973304137371, 1526.382868172863937, 217.2942086403122914 ) ) ;
#82341 = CARTESIAN_POINT ( 'NONE',  ( -15.96958168569999970, 1519.913060387329779, 225.0914276473980067 ) ) ;
#82342 = CARTESIAN_POINT ( 'NONE',  ( 16.53726887470000051, 1419.770721813829823, 227.0156051753980080 ) ) ;
#82343 = CARTESIAN_POINT ( 'NONE',  ( -31.34491295179425663, 1525.848198008145346, 201.1913533246503789 ) ) ;
#82344 = VECTOR ( 'NONE', #61854, 1000.000000000000227 ) ;
#82345 = DIRECTION ( 'NONE',  ( 0.000000000000000000, 0.000000000000000000, 1.000000000000000000 ) ) ;
#82346 = CARTESIAN_POINT ( 'NONE',  ( -16.85751496860000032, 1409.501737783529961, 224.7669409504980251 ) ) ;
#82347 = CARTESIAN_POINT ( 'NONE',  ( -12.03392632030000087, 1501.178862756489934, 213.6370645969589930 ) ) ;
#82348 = CARTESIAN_POINT ( 'NONE',  ( -0.5656601615979999220, 1424.194575837329921, 228.0927458394980079 ) ) ;
#82349 = CARTESIAN_POINT ( 'NONE',  ( 12.55412049360000104, 1453.847845034990087, 193.6240741990989989 ) ) ;
#82350 = FACE_OUTER_BOUND ( 'NONE', #46468, .T. ) ;
#82351 = CARTESIAN_POINT ( 'NONE',  ( 12.72965180529999962, 1416.819760301830001, 223.1305968146979808 ) ) ;
#82352 = CARTESIAN_POINT ( 'NONE',  ( -14.57244604748959915, 1417.419309545480019, 203.2554935970629799 ) ) ;
#82353 = EDGE_CURVE ( 'NONE', #20210, #72801, #8643, .T. ) ;
#82354 = CARTESIAN_POINT ( 'NONE',  ( -7.758455216056949766, 1432.346375745089972, 153.7650376895189765 ) ) ;
#82355 = CARTESIAN_POINT ( 'NONE',  ( -3.949231543599999394, 1416.520322351229879, 227.3109020079980098 ) ) ;
#82356 = CARTESIAN_POINT ( 'NONE',  ( 0.2159072697397970142, 1454.042348015329935, 183.2086788371790078 ) ) ;
#82357 = CARTESIAN_POINT ( 'NONE',  ( -13.37628687016149875, 1408.062381179059912, 207.9480605954729810 ) ) ;
#82358 = CARTESIAN_POINT ( 'NONE',  ( -15.98493104980000190, 1416.216252248729916, 200.6524258963880243 ) ) ;
#82359 = AXIS2_PLACEMENT_3D ( 'NONE', #8211, #76532, #53570 ) ;
#82360 = EDGE_CURVE ( 'NONE', #78070, #75164, #33555, .T. ) ;
#82361 = CARTESIAN_POINT ( 'NONE',  ( -0.5006798747275272854, 1484.181444057518320, 198.4395552954152038 ) ) ;
#82362 = CARTESIAN_POINT ( 'NONE',  ( 13.50126846350000065, 1434.968978322849807, 147.6247934473980195 ) ) ;
#82363 = CARTESIAN_POINT ( 'NONE',  ( -35.92423077455959657, 1436.007692230529983, 134.0999999972619889 ) ) ;
#82364 = CARTESIAN_POINT ( 'NONE',  ( 1.126960914759999932, 1451.194794027190028, 189.8794982769989872 ) ) ;
#82365 = VERTEX_POINT ( 'NONE', #79117 ) ;
#82366 = CARTESIAN_POINT ( 'NONE',  ( -17.24701803732119743, 1523.844789899205125, 180.8504343893186501 ) ) ;
#82367 = CARTESIAN_POINT ( 'NONE',  ( 8.555072664789999948, 1479.287826498589993, 202.9093910877689950 ) ) ;
#82368 = CARTESIAN_POINT ( 'NONE',  ( -105.2215450167301611, 1381.056857365499354, 308.6470483461520189 ) ) ;
#82369 = CARTESIAN_POINT ( 'NONE',  ( -11.15057513110000009, 1491.593586447790130, 208.4267869613440212 ) ) ;
#82371 = EDGE_CURVE ( 'NONE', #45409, #21233, #60170, .T. ) ;
#82370 = CARTESIAN_POINT ( 'NONE',  ( -9.361471622734621079, 1438.259801222220176, 210.6624890962389998 ) ) ;
#82372 = CARTESIAN_POINT ( 'NONE',  ( 13.87457611739909957, 1508.109622702359957, 232.8490349609430154 ) ) ;
#82373 = CARTESIAN_POINT ( 'NONE',  ( 40.50178695588397204, 1425.153962140106159, 269.1155952481692566 ) ) ;
#82374 = CARTESIAN_POINT ( 'NONE',  ( -18.89419841210175122, 1483.154679543993097, 218.3089908767800580 ) ) ;
#82375 = CARTESIAN_POINT ( 'NONE',  ( 18.66420869458052323, 1526.382868172864164, 232.7837831374276902 ) ) ;
#82376 = CARTESIAN_POINT ( 'NONE',  ( 3.418717339140000089, 1426.008825657230091, 185.1440916679979978 ) ) ;
#82377 = CARTESIAN_POINT ( 'NONE',  ( -66.36738586336869616, 1385.093736160859862, 258.0857209453200198 ) ) ;
#82378 = CARTESIAN_POINT ( 'NONE',  ( -17.43739734485555459, 1526.178928173328131, 237.5162751070486422 ) ) ;
#82379 = CARTESIAN_POINT ( 'NONE',  ( -3.965129847697639764, 1508.551704408389924, 204.6168180214280028 ) ) ;
#82380 = CARTESIAN_POINT ( 'NONE',  ( -27.77560428830000205, 1450.655010635179906, 136.4259719682980005 ) ) ;
#82381 = ADVANCED_FACE ( 'NONE', ( #88069 ), #31298, .F. ) ;
#82382 = EDGE_CURVE ( 'NONE', #28184, #28853, #1459, .T. ) ;
#82383 = CARTESIAN_POINT ( 'NONE',  ( -16.02269354968879966, 1410.117710933159969, 226.4951371525800141 ) ) ;
#82385 = ORIENTED_EDGE ( 'NONE', *, *, #110402, .F. ) ;
#82384 = CARTESIAN_POINT ( 'NONE',  ( 0.4957976563827369842, 1415.716230218539977, 184.8406531014170184 ) ) ;
#82386 = CARTESIAN_POINT ( 'NONE',  ( 8.337034337958543873, 1374.413060387289988, 213.6763885784389174 ) ) ;
#82387 = CARTESIAN_POINT ( 'NONE',  ( 10.30586371983499916, 1471.203633962730009, 211.4644565147510207 ) ) ;
#82388 = CARTESIAN_POINT ( 'NONE',  ( 10.92857032808210072, 1460.888924644350027, 208.5047758900509791 ) ) ;
#82389 = CARTESIAN_POINT ( 'NONE',  ( -109.9698191200000110, 1384.452558329679960, 311.4357953482589778 ) ) ;
#82390 = CARTESIAN_POINT ( 'NONE',  ( -0.2309819874101929904, 1419.229592309189911, 184.5617884385680156 ) ) ;
#82391 = AXIS2_PLACEMENT_3D ( 'NONE', #40124, #13802, #38472 ) ;
#82392 = CARTESIAN_POINT ( 'NONE',  ( 0.2895612746910000146, 1465.119060462830021, 238.1348910625980011 ) ) ;
#82393 = CARTESIAN_POINT ( 'NONE',  ( 21.39553055000000015, 1411.020667844629997, 217.4763728266080136 ) ) ;
#82394 = B_SPLINE_SURFACE_WITH_KNOTS ( 'NONE', 5, 5, ( 
 ( #20792, #12405, #55536, #46590, #4033, #38161 ),
 ( #89661, #12947, #81254, #4569, #72879, #30304 ),
 ( #64495, #47674, #81803, #73434, #107567, #65029 ),
 ( #22425, #100802, #68353, #109778, #36, #40357 ),
 ( #58827, #24092, #58280, #92965, #14602, #74538 ),
 ( #76174, #42572, #16237, #82914, #7315, #25746 ) ),
 .UNSPECIFIED., .F., .F., .F.,
 ( 6, 6 ),
 ( 6, 6 ),
 ( 29.52656374800000094, 158.0439293190000001 ),
 ( -2.775557561569999727E-17, 1.000000000000000000 ),
 .UNSPECIFIED. ) ;
#82395 = CARTESIAN_POINT ( 'NONE',  ( 0.5105443137851592983, 1450.895231787036892, 181.2859576932934829 ) ) ;
#82396 = CARTESIAN_POINT ( 'NONE',  ( -18.27580183039999895, 1467.051542642389904, 217.8951514484589893 ) ) ;
#82397 = CARTESIAN_POINT ( 'NONE',  ( -16.17440652799999867, 1423.017051802529977, 229.3744292183979780 ) ) ;
#82399 = CARTESIAN_POINT ( 'NONE',  ( 3.835404308830561160, 1412.913060387329779, 216.1425064568153687 ) ) ;
#82398 = CARTESIAN_POINT ( 'NONE',  ( -3.849878380766676766, 1511.509050022477140, 200.9742446617588314 ) ) ;
#82400 = CARTESIAN_POINT ( 'NONE',  ( 24.91361133721389720, 1430.502641194839725, 209.5701750418959932 ) ) ;
#82401 = CARTESIAN_POINT ( 'NONE',  ( -121.2688967968579448, 1320.102705746890251, 290.9564879300592679 ) ) ;
#82402 = CARTESIAN_POINT ( 'NONE',  ( 14.45750538832999865, 1416.828039266780024, 196.8520486936070029 ) ) ;
#82403 = EDGE_CURVE ( 'NONE', #23969, #103706, #99003, .T. ) ;
#82404 = CARTESIAN_POINT ( 'NONE',  ( -15.17885259120000008, 1504.055100336790019, 208.8134705691849717 ) ) ;
#82405 = CARTESIAN_POINT ( 'NONE',  ( -5.511153256349429874, 1374.913063729909936, 203.3075733038869828 ) ) ;
#82406 = CARTESIAN_POINT ( 'NONE',  ( 4.609996581545000360, 1516.769879638719885, 205.6626893540170329 ) ) ;
#82407 = FACE_OUTER_BOUND ( 'NONE', #91636, .T. ) ;
#82408 = ORIENTED_EDGE ( 'NONE', *, *, #65942, .T. ) ;
#82409 = EDGE_CURVE ( 'NONE', #107214, #83466, #68253, .T. ) ;
#82410 = CIRCLE ( 'NONE', #16265, 0.9999999999999481526 ) ;
#82411 = CARTESIAN_POINT ( 'NONE',  ( -32.31945039880162085, 1524.082740465118604, 216.0996078590375475 ) ) ;
#82412 = CARTESIAN_POINT ( 'NONE',  ( -4.222081761889490359, 1441.600097058339998, 170.2277829678710077 ) ) ;
#82414 = ORIENTED_EDGE ( 'NONE', *, *, #19428, .F. ) ;
#82413 = CARTESIAN_POINT ( 'NONE',  ( -68.49931456876349500, 1379.747368005260114, 280.0909653425130159 ) ) ;
#82415 = ORIENTED_EDGE ( 'NONE', *, *, #95243, .T. ) ;
#82416 = CARTESIAN_POINT ( 'NONE',  ( -17.52552833341350080, 1417.778948467160035, 206.7855603744410189 ) ) ;
#82417 = ORIENTED_EDGE ( 'NONE', *, *, #67354, .T. ) ;
#82418 = DIRECTION ( 'NONE',  ( -0.9125304618754022101, 0.000000000000000000, -0.4090087482554195519 ) ) ;
#82419 = CARTESIAN_POINT ( 'NONE',  ( 12.26025649039999976, 1499.789859244890067, 205.9458331038790107 ) ) ;
#82421 = CARTESIAN_POINT ( 'NONE',  ( 15.91660703430019730, 1409.850593835830068, 191.9602275961530040 ) ) ;
#82420 = CARTESIAN_POINT ( 'NONE',  ( -11.74440294555880193, 1426.691427119352511, 144.6990483903438758 ) ) ;
#82422 = CARTESIAN_POINT ( 'NONE',  ( -6.935801299664999142, 1516.621991115350056, 210.2518484644969874 ) ) ;
#82423 = CARTESIAN_POINT ( 'NONE',  ( -106.4040135799809974, 1378.913060387319774, 306.2480672476809787 ) ) ;
#82424 = CARTESIAN_POINT ( 'NONE',  ( 2.935740384309999840, 1409.954265578529885, 231.6094181485979959 ) ) ;
#82425 = CARTESIAN_POINT ( 'NONE',  ( 12.45168873679009991, 1501.262350266580142, 211.7052737702659897 ) ) ;
#82426 = APPLICATION_PROTOCOL_DEFINITION ( 'draft international standard', 'automotive_design', 1998, #97107 ) ;
#82427 = CARTESIAN_POINT ( 'NONE',  ( 39.19204896952249584, 1449.501219045310108, 134.0999999980739688 ) ) ;
#82428 = AXIS2_PLACEMENT_3D ( 'NONE', #60335, #102307, #85499 ) ;
#82429 = CARTESIAN_POINT ( 'NONE',  ( -39.59829837890580251, 1440.706476837099899, 136.7973020598680023 ) ) ;
#82430 = CARTESIAN_POINT ( 'NONE',  ( -13.90059962640000180, 1502.276548577589892, 227.4029734405989984 ) ) ;
#82431 = CARTESIAN_POINT ( 'NONE',  ( -18.12714478550000052, 1457.846702312930120, 228.5127547687980041 ) ) ;
#82432 = ORIENTED_EDGE ( 'NONE', *, *, #40680, .F. ) ;
#82433 = ORIENTED_EDGE ( 'NONE', *, *, #42172, .T. ) ;
#82434 = CARTESIAN_POINT ( 'NONE',  ( -6.648850802594999720, 1513.600111798349872, 216.5887361369370012 ) ) ;
#82435 = CARTESIAN_POINT ( 'NONE',  ( 16.61266722949974195, 1514.059034352515937, 195.0269839839985480 ) ) ;
#82436 = CARTESIAN_POINT ( 'NONE',  ( 12.17073519972539941, 1499.730396604210000, 205.6506567772970016 ) ) ;
#82437 = CARTESIAN_POINT ( 'NONE',  ( -3.174083179560000190, 1485.815246478130121, 182.5712446315979776 ) ) ;
#82438 = CARTESIAN_POINT ( 'NONE',  ( -2.500000000000000000, 1439.559074768590108, 165.1937480901340223 ) ) ;
#82439 = CARTESIAN_POINT ( 'NONE',  ( -27.56049296109999958, 1508.045672656129909, 205.3679835307079884 ) ) ;
#82440 = CARTESIAN_POINT ( 'NONE',  ( 33.91369111058539687, 1435.681798630800131, 135.0591074393149711 ) ) ;
#82441 = LINE ( 'NONE', #56134, #93953 ) ;
#82442 = CARTESIAN_POINT ( 'NONE',  ( 29.52630424919045637, 1525.661275128776197, 221.7199234082868884 ) ) ;
#82443 = CARTESIAN_POINT ( 'NONE',  ( 1.075905130380000019, 1414.913060387329779, 191.8484598369979892 ) ) ;
#82444 = CARTESIAN_POINT ( 'NONE',  ( -68.46546297202630171, 1384.727450216739953, 262.6729272380309794 ) ) ;
#82445 = VERTEX_POINT ( 'NONE', #100160 ) ;
#82446 =( BOUNDED_CURVE ( )  B_SPLINE_CURVE ( 3, ( #40879, #59365, #31926, #93475 ),
 .UNSPECIFIED., .F., .T. ) 
 B_SPLINE_CURVE_WITH_KNOTS ( ( 4, 4 ),
 ( 3.142686768074915094, 3.147761099832099951 ),
 .UNSPECIFIED. ) 
 CURVE ( )  GEOMETRIC_REPRESENTATION_ITEM ( )  RATIONAL_B_SPLINE_CURVE ( ( 1.000000000000000000, 0.9999978542642524726, 0.9999978542642524726, 1.000000000000000000 ) ) 
 REPRESENTATION_ITEM ( '' )  );
#82447 = CARTESIAN_POINT ( 'NONE',  ( 2.872836622524999939, 1517.158319634930194, 201.3964737998670103 ) ) ;
#82448 = CARTESIAN_POINT ( 'NONE',  ( 1.122033391945000069, 1516.972341476009888, 208.3659064338399673 ) ) ;
#82449 = ORIENTED_EDGE ( 'NONE', *, *, #57709, .T. ) ;
#82450 = CARTESIAN_POINT ( 'NONE',  ( 34.63479025869150263, 1440.913060387330006, 260.2959212809009841 ) ) ;
#82451 = AXIS2_PLACEMENT_3D ( 'NONE', #11297, #71221, #95834 ) ;
#82452 = CARTESIAN_POINT ( 'NONE',  ( -0.001699438796131666181, 1451.847275359585637, 154.0281730256439232 ) ) ;
#82453 = ORIENTED_EDGE ( 'NONE', *, *, #4984, .T. ) ;
#82454 = CARTESIAN_POINT ( 'NONE',  ( 0.009324443903248720578, 1452.355234467360106, 183.2662222589769954 ) ) ;
#82455 = CARTESIAN_POINT ( 'NONE',  ( 8.441193709969130765, 1428.373632909889920, 213.4378653404860131 ) ) ;
#82456 = LINE ( 'NONE', #39895, #104662 ) ;
#82457 = CARTESIAN_POINT ( 'NONE',  ( -9.607526321970940586, 1460.797498750790055, 207.9656065552430277 ) ) ;
#82458 = CARTESIAN_POINT ( 'NONE',  ( -13.02607830360000030, 1426.053423478829927, 222.2684508982979992 ) ) ;
#82459 = CARTESIAN_POINT ( 'NONE',  ( -20.15452302159999931, 1507.845791376729949, 228.9024215066979764 ) ) ;
#82460 = CARTESIAN_POINT ( 'NONE',  ( -1.493215638020000124, 1507.691765935529929, 180.8029183418980210 ) ) ;
#82461 = CARTESIAN_POINT ( 'NONE',  ( -11.87968386989999914, 1433.311128018820000, 147.1501983835979956 ) ) ;
#82462 = FACE_OUTER_BOUND ( 'NONE', #54066, .T. ) ;
#82464 = CARTESIAN_POINT ( 'NONE',  ( -10.47364140659463949, 1423.539562070946204, 137.3343660864095170 ) ) ;
#82463 = CARTESIAN_POINT ( 'NONE',  ( 12.53348523240000034, 1462.451547715029847, 231.4893851574979919 ) ) ;
#82465 = CARTESIAN_POINT ( 'NONE',  ( 6.690593169671610774, 1474.175173204296698, 270.1377431963427966 ) ) ;
#82466 = CARTESIAN_POINT ( 'NONE',  ( -4.616899872884999922, 1517.050041317280147, 216.8443827349270236 ) ) ;
#82467 = ORIENTED_EDGE ( 'NONE', *, *, #52467, .F. ) ;
#82468 = CARTESIAN_POINT ( 'NONE',  ( -0.5206041912694210350, 1486.385752493620203, 181.7753473960027577 ) ) ;
#82469 = CARTESIAN_POINT ( 'NONE',  ( -0.1467532245951940206, 1507.559297430280139, 180.8320577633109849 ) ) ;
#82470 = CARTESIAN_POINT ( 'NONE',  ( 19.12310882341182250, 1443.904899534319838, 213.6905610154896635 ) ) ;
#82471 = CARTESIAN_POINT ( 'NONE',  ( -2.865911554774999814, 1516.906233342200039, 212.5838411289170153 ) ) ;
#82472 = CARTESIAN_POINT ( 'NONE',  ( 18.58455362259999788, 1509.562047300529912, 186.5314039206980112 ) ) ;
#82473 = CARTESIAN_POINT ( 'NONE',  ( -0.4151546846821903003, 1511.187213306747708, 243.9330574173806951 ) ) ;
#82475 = ORIENTED_EDGE ( 'NONE', *, *, #26821, .F. ) ;
#82474 = CARTESIAN_POINT ( 'NONE',  ( 3.801724372608250135, 1509.034524880150002, 213.6092044083339943 ) ) ;
#82476 = FACE_OUTER_BOUND ( 'NONE', #103458, .T. ) ;
#82477 = CARTESIAN_POINT ( 'NONE',  ( 2.407821901370000184, 1507.916632424389945, 220.5940247002990020 ) ) ;
#82478 = CARTESIAN_POINT ( 'NONE',  ( -11.28505919290000037, 1431.090797829909889, 151.4130702670979929 ) ) ;
#82479 = CARTESIAN_POINT ( 'NONE',  ( -4.660393612750000081, 1436.848553822789881, 227.0391165213990234 ) ) ;
#82480 = CARTESIAN_POINT ( 'NONE',  ( -7.749229762881280514, 1439.121665196640151, 205.0683262884020337 ) ) ;
#82481 = CARTESIAN_POINT ( 'NONE',  ( -7.105422403163559973E-15, 1425.409940805969882, 153.8890955463500063 ) ) ;
#82482 = CARTESIAN_POINT ( 'NONE',  ( -109.2286396907909989, 1384.893028202680171, 295.1336651452069759 ) ) ;
#82483 = CARTESIAN_POINT ( 'NONE',  ( 12.77839545800000032, 1445.090219591050072, 187.3316831286979891 ) ) ;
#82485 = CARTESIAN_POINT ( 'NONE',  ( -10.45474545596770000, 1481.736993775309884, 206.6726633622900238 ) ) ;
#82484 = CARTESIAN_POINT ( 'NONE',  ( -19.02423469520000054, 1444.806343971380102, 225.8304661078979905 ) ) ;
#82486 = CARTESIAN_POINT ( 'NONE',  ( 0.04536310491940000189, 1416.820969729830040, 190.9583658068980014 ) ) ;
#82487 = ORIENTED_EDGE ( 'NONE', *, *, #74901, .F. ) ;
#82488 = CARTESIAN_POINT ( 'NONE',  ( -1.134358008724999811, 1516.744381837270112, 205.0932347109869909 ) ) ;
#82489 = CARTESIAN_POINT ( 'NONE',  ( 9.928099361890000196, 1406.542887612530194, 268.4433879007979726 ) ) ;
#82490 =( GEOMETRIC_REPRESENTATION_CONTEXT ( 3 ) GLOBAL_UNCERTAINTY_ASSIGNED_CONTEXT ( ( #102831 ) ) GLOBAL_UNIT_ASSIGNED_CONTEXT ( ( #80354, #29928, #98241 ) ) REPRESENTATION_CONTEXT ( 'NONE', 'WORKASPACE' ) );
#82491 = CARTESIAN_POINT ( 'NONE',  ( 0.4960545405569999899, 1409.436441302029834, 185.2773262721979961 ) ) ;
#82492 = CARTESIAN_POINT ( 'NONE',  ( 17.94874957400000071, 1410.880404130830129, 193.3864771145979944 ) ) ;
#82493 = CARTESIAN_POINT ( 'NONE',  ( 22.42926025653192923, 1430.882581194299291, 217.2517530083725603 ) ) ;
#82494 = CARTESIAN_POINT ( 'NONE',  ( -24.00529210049999662, 1452.074773682930072, 136.6368758670979844 ) ) ;
#82495 = CARTESIAN_POINT ( 'NONE',  ( 28.07231212390000152, 1508.101920094730076, 210.4687657402579930 ) ) ;
#82496 = CARTESIAN_POINT ( 'NONE',  ( -8.106555885276549134, 1438.741351455190170, 205.9368832915250209 ) ) ;
#82497 = CARTESIAN_POINT ( 'NONE',  ( -2.496316867461920275, 1449.223786180559955, 155.0643152763460080 ) ) ;
#82498 = CARTESIAN_POINT ( 'NONE',  ( -12.50186341110000043, 1445.154755434839899, 186.4456158379979911 ) ) ;
#82499 = ADVANCED_FACE ( 'NONE', ( #101235 ), #17856, .T. ) ;
#82500 = CARTESIAN_POINT ( 'NONE',  ( -19.79527383844874677, 1485.865817549667554, 190.3272490650382451 ) ) ;
#82501 = CARTESIAN_POINT ( 'NONE',  ( -14.39446395563320102, 1416.321686235100060, 221.3267789012660103 ) ) ;
#82502 = CARTESIAN_POINT ( 'NONE',  ( -11.27301341819999969, 1500.749601584090215, 213.2292196792290042 ) ) ;
#82503 = EDGE_CURVE ( 'NONE', #40664, #23280, #78442, .T. ) ;
#82504 = B_SPLINE_CURVE_WITH_KNOTS ( 'NONE', 3,
 ( #63426, #104843, #10791, #35991 ),
 .UNSPECIFIED., .F., .F.,
 ( 4, 4 ),
 ( 0.000000000000000000, 1.000000000000000000 ),
 .UNSPECIFIED. ) ;
#82505 = CARTESIAN_POINT ( 'NONE',  ( -5.498048942630000546, 1436.980437978990039, 209.3664492523469960 ) ) ;
#82507 = EDGE_CURVE ( 'NONE', #94989, #97932, #76595, .T. ) ;
#82506 = CARTESIAN_POINT ( 'NONE',  ( 20.53373630228941593, 1507.794800605937780, 228.2241611779419088 ) ) ;
#82508 = CARTESIAN_POINT ( 'NONE',  ( 3.659274215279999964, 1441.479476129459954, 165.0935548642979995 ) ) ;
#82509 = AXIS2_PLACEMENT_3D ( 'NONE', #18435, #60489, #50435 ) ;
#82510 = CARTESIAN_POINT ( 'NONE',  ( -1.775122301699999960, 1475.958576172530002, 267.2336942637979860 ) ) ;
#82511 = CARTESIAN_POINT ( 'NONE',  ( -10.73010380666730690, 1424.980364244693419, 138.6337414485319641 ) ) ;
#82512 = CARTESIAN_POINT ( 'NONE',  ( 22.96901158543816734, 1522.051704408389924, 206.5493031772561778 ) ) ;
#82513 = DIRECTION ( 'NONE',  ( 0.000000000000000000, 0.000000000000000000, 1.000000000000000000 ) ) ;
#82514 = CARTESIAN_POINT ( 'NONE',  ( -50.29015339553740205, 1384.738658365939955, 262.3372466638650167 ) ) ;
#82515 = CARTESIAN_POINT ( 'NONE',  ( -106.5621319268489913, 1391.913060387289988, 302.9116844650990288 ) ) ;
#82516 = CARTESIAN_POINT ( 'NONE',  ( 4.487357238568115747, 1509.034509761477011, 212.2379806275817486 ) ) ;
#82517 = B_SPLINE_CURVE_WITH_KNOTS ( 'NONE', 3,
 ( #81353, #72982, #106574, #2497, #98718, #71369 ),
 .UNSPECIFIED., .F., .F.,
 ( 4, 2, 4 ),
 ( 0.000000000000000000, 0.2566448165338969800, 0.5131331537284539168 ),
 .UNSPECIFIED. ) ;
#82518 = EDGE_CURVE ( 'NONE', #66989, #43462, #103457, .T. ) ;
#82519 = CARTESIAN_POINT ( 'NONE',  ( -105.1828009239999915, 1379.114047142900063, 303.4308355331590406 ) ) ;
#82520 = CARTESIAN_POINT ( 'NONE',  ( -20.39893125377176730, 1526.069472839383252, 185.1113182959119001 ) ) ;
#82521 = CARTESIAN_POINT ( 'NONE',  ( 0.1968062131348075061, 1420.483348320591176, 182.7518766831598214 ) ) ;
#82522 = CARTESIAN_POINT ( 'NONE',  ( -1.530945675004649953, 1395.966522188359932, 220.0244024312320050 ) ) ;
#82523 = CARTESIAN_POINT ( 'NONE',  ( -15.06561728630400054, 1422.389775765796230, 229.4662607246160064 ) ) ;
#82524 = CARTESIAN_POINT ( 'NONE',  ( 10.03307217725760125, 1480.064660596370004, 205.9773996988400029 ) ) ;
#82525 = ORIENTED_EDGE ( 'NONE', *, *, #3187, .T. ) ;
#82526 = CARTESIAN_POINT ( 'NONE',  ( -2.413323989047310381, 1410.375482399494103, 232.6928827166564133 ) ) ;
#82527 = CARTESIAN_POINT ( 'NONE',  ( -7.396545081224999763, 1511.069621805459974, 215.4940135707269917 ) ) ;
#82528 = CARTESIAN_POINT ( 'NONE',  ( 0.5708672982295059928, 1460.784242391739781, 230.4191149236459921 ) ) ;
#82529 = CIRCLE ( 'NONE', #34244, 2.000000000000003553 ) ;
#82531 = CARTESIAN_POINT ( 'NONE',  ( -12.20553011617109895, 1378.355942198320008, 210.8952815345800218 ) ) ;
#82530 = CARTESIAN_POINT ( 'NONE',  ( -16.36727155057150185, 1416.861723988390168, 208.8581010215799836 ) ) ;
#82532 = CARTESIAN_POINT ( 'NONE',  ( 16.48400375141593344, 1525.790287071782359, 236.4799654700566975 ) ) ;
#82533 = CARTESIAN_POINT ( 'NONE',  ( 10.71141203040000001, 1409.287111137730108, 190.6699416860979852 ) ) ;
#82534 = DIRECTION ( 'NONE',  ( -0.9455185755993178454, 0.000000000000000000, 0.3255681544571537578 ) ) ;
#82535 = B_SPLINE_CURVE_WITH_KNOTS ( 'NONE', 3,
 ( #50277, #24479, #17160, #94440, #51353, #77127, #433, #84406, #50809, #109074 ),
 .UNSPECIFIED., .F., .F.,
 ( 4, 2, 2, 2, 4 ),
 ( 0.000000000000000000, 0.07144792451131930233, 0.1124765170753259935, 0.1725353800366839774, 0.2229999168759839723 ),
 .UNSPECIFIED. ) ;
#82536 = CARTESIAN_POINT ( 'NONE',  ( 7.328676169885000036, 1516.833844030519913, 202.1788723028969912 ) ) ;
#82537 = CARTESIAN_POINT ( 'NONE',  ( 8.136848112800000976, 1426.803698133580156, 211.7678967111889961 ) ) ;
#82538 = CARTESIAN_POINT ( 'NONE',  ( -12.66923305982695958, 1398.288632557894289, 212.0380595282034619 ) ) ;
#82539 = CARTESIAN_POINT ( 'NONE',  ( 16.10875976033500123, 1511.961073825299991, 196.9868955663669965 ) ) ;
#82540 = CARTESIAN_POINT ( 'NONE',  ( -18.43993559601290144, 1419.439711405959997, 205.9910018360060064 ) ) ;
#82541 = CARTESIAN_POINT ( 'NONE',  ( 7.644361507415789768E-14, 1380.413087040579967, 210.0680626132329962 ) ) ;
#82543 = ADVANCED_FACE ( 'NONE', ( #51982 ), #44694, .F. ) ;
#82542 = EDGE_CURVE ( 'NONE', #58839, #52413, #44136, .T. ) ;
#82544 = CARTESIAN_POINT ( 'NONE',  ( 19.85685705864179695, 1508.846415979930043, 229.4817442290339784 ) ) ;
#82546 = EDGE_LOOP ( 'NONE', ( #86542, #69743, #41941 ) ) ;
#82545 = CARTESIAN_POINT ( 'NONE',  ( 8.476386806709999888, 1453.731993414189901, 214.0848624316990083 ) ) ;
#82547 = ORIENTED_EDGE ( 'NONE', *, *, #42389, .T. ) ;
#82548 = CARTESIAN_POINT ( 'NONE',  ( -5.247863634239999797, 1396.629037141330173, 220.9040508069979865 ) ) ;
#82549 = CARTESIAN_POINT ( 'NONE',  ( -20.05397710889999630, 1410.534994038629975, 220.7224924335979779 ) ) ;
#82550 = ORIENTED_EDGE ( 'NONE', *, *, #45616, .T. ) ;
#82551 = CARTESIAN_POINT ( 'NONE',  ( -12.96259728057930793, 1444.899188585709453, 169.4271164727056771 ) ) ;
#82552 = CARTESIAN_POINT ( 'NONE',  ( 0.3621993315900440269, 1416.825784014750070, 227.1772709241249970 ) ) ;
#82553 = CARTESIAN_POINT ( 'NONE',  ( -7.893411120225001021, 1512.020737142380085, 212.1186310024369845 ) ) ;
#82556 = EDGE_CURVE ( 'NONE', #47989, #39456, #78841, .T. ) ;
#82555 = CARTESIAN_POINT ( 'NONE',  ( 32.86802468386284914, 1501.977400791986611, 201.0396662540042030 ) ) ;
#82554 = CARTESIAN_POINT ( 'NONE',  ( 2.251242965029999876, 1445.013527181690051, 200.2860235718189870 ) ) ;
#82557 = B_SPLINE_CURVE_WITH_KNOTS ( 'NONE', 3,
 ( #39248, #30844, #31949, #22981 ),
 .UNSPECIFIED., .F., .F.,
 ( 4, 4 ),
 ( 0.000000000000000000, 1.000000000000000000 ),
 .UNSPECIFIED. ) ;
#82558 = CARTESIAN_POINT ( 'NONE',  ( 5.279034537639999414, 1410.298216193129974, 186.4795294922980133 ) ) ;
#82559 = CARTESIAN_POINT ( 'NONE',  ( -4.836107688109999359, 1414.913060387329779, 193.6922375078979996 ) ) ;
#82560 = CARTESIAN_POINT ( 'NONE',  ( 5.440512190109999757, 1424.738065781850082, 191.9794586101990319 ) ) ;
#82561 = CARTESIAN_POINT ( 'NONE',  ( 6.002018859382760141, 1396.122655539619927, 199.8546179732479970 ) ) ;
#82562 = CARTESIAN_POINT ( 'NONE',  ( 1.556370157619999972, 1414.996444526030018, 191.7142053706980107 ) ) ;
#82563 = CARTESIAN_POINT ( 'NONE',  ( 11.15490121449999883, 1425.160561550830153, 144.1688093938980160 ) ) ;
#82564 = CARTESIAN_POINT ( 'NONE',  ( 8.232567722344999339, 1512.371207877099778, 202.4629285007669921 ) ) ;
#82565 = ORIENTED_EDGE ( 'NONE', *, *, #85786, .F. ) ;
#82566 = CARTESIAN_POINT ( 'NONE',  ( 13.19362647665400168, 1435.060500567780082, 149.8921243419820257 ) ) ;
#82567 = DIRECTION ( 'NONE',  ( 2.491197269910784929E-47, 1.000000000000000000, -1.836970198721029688E-16 ) ) ;
#82568 = ORIENTED_EDGE ( 'NONE', *, *, #62285, .T. ) ;
#82569 = VERTEX_POINT ( 'NONE', #45253 ) ;
#82570 = DIRECTION ( 'NONE',  ( -0.000000000000000000, -1.000000000000000000, -0.000000000000000000 ) ) ;
#82571 = CARTESIAN_POINT ( 'NONE',  ( -14.50827198289999842, 1461.594363702429746, 229.4507344440980035 ) ) ;
#82572 = CARTESIAN_POINT ( 'NONE',  ( -109.9089029649868081, 1385.746877553887089, 311.3956508573958786 ) ) ;
#82573 = CARTESIAN_POINT ( 'NONE',  ( -5.003220765204999587, 1516.983995446890049, 216.0685944891870065 ) ) ;
#82574 = CARTESIAN_POINT ( 'NONE',  ( -12.34620125349839803, 1378.802061108420048, 209.1451513645090188 ) ) ;
#82575 = PRESENTATION_LAYER_ASSIGNMENT (  '', '', ( #39642 ) ) ;
#82576 = ORIENTED_EDGE ( 'NONE', *, *, #65887, .F. ) ;
#82577 = CARTESIAN_POINT ( 'NONE',  ( -12.80491917260000001, 1502.810374455390047, 208.8309748505670029 ) ) ;
#82578 = CARTESIAN_POINT ( 'NONE',  ( -14.42137577593229913, 1509.529401687109839, 182.8435569880860214 ) ) ;
#82579 = CARTESIAN_POINT ( 'NONE',  ( -43.21650806019999891, 1379.188238639419978, 226.3493147681589903 ) ) ;
#82580 = CARTESIAN_POINT ( 'NONE',  ( 1.119717716265000051, 1517.038650117239968, 205.6590103047369951 ) ) ;
#82581 = VERTEX_POINT ( 'NONE', #79388 ) ;
#82582 = CARTESIAN_POINT ( 'NONE',  ( -2.868112169295000236, 1516.855632454399938, 209.8795095036720113 ) ) ;
#82583 = CARTESIAN_POINT ( 'NONE',  ( -8.212845905083440812, 1452.462047389940153, 204.7396385917020041 ) ) ;
#82584 = CARTESIAN_POINT ( 'NONE',  ( -29.85762690982718937, 1419.472691627382119, 269.4692931743723534 ) ) ;
#82585 = CARTESIAN_POINT ( 'NONE',  ( -1.439448805189999847, 1408.963327047329813, 231.9239705684979924 ) ) ;
#82587 = ORIENTED_EDGE ( 'NONE', *, *, #43482, .T. ) ;
#82586 = CARTESIAN_POINT ( 'NONE',  ( -4.255689356150000435, 1519.913060387329779, 186.6761948862979921 ) ) ;
#82588 = CARTESIAN_POINT ( 'NONE',  ( 5.513435558014999849, 1508.551704408389924, 216.1347675157070114 ) ) ;
#82589 = CARTESIAN_POINT ( 'NONE',  ( -29.20316173986769925, 1440.913060386999859, 235.6859508697740182 ) ) ;
#82590 = CARTESIAN_POINT ( 'NONE',  ( -62.13634214319999671, 1384.087241931920062, 284.7267046562590167 ) ) ;
#82591 = CARTESIAN_POINT ( 'NONE',  ( -12.53380499169999851, 1445.052233488290085, 169.4755105685979970 ) ) ;
#82592 = AXIS2_PLACEMENT_3D ( 'NONE', #32101, #23131, #40497 ) ;
#82593 = CARTESIAN_POINT ( 'NONE',  ( 5.012278525919999339, 1408.134067213729850, 270.2879168813980186 ) ) ;
#82594 = CARTESIAN_POINT ( 'NONE',  ( -1.120543735785000106, 1517.073005577650065, 213.1661658574570026 ) ) ;
#82595 = CARTESIAN_POINT ( 'NONE',  ( 24.02131707860000276, 1410.844657319930093, 208.5571756898100091 ) ) ;
#82596 = DIRECTION ( 'NONE',  ( 0.4090087482554183862, 0.000000000000000000, -0.9125304618754026542 ) ) ;
#82597 = CARTESIAN_POINT ( 'NONE',  ( 1.042629999269999885, 1442.250188905790083, 219.0243665098589929 ) ) ;
#82598 = CARTESIAN_POINT ( 'NONE',  ( -7.710327657623590625, 1516.583792872650065, 210.5203955415310020 ) ) ;
#82599 = CARTESIAN_POINT ( 'NONE',  ( 2.299667965875000331, 1516.965971551240045, 210.2399506998270056 ) ) ;
#82600 = CARTESIAN_POINT ( 'NONE',  ( -4.046419768304757802, 1446.994263467394603, 154.8289802513601785 ) ) ;
#82601 = FACE_OUTER_BOUND ( 'NONE', #71320, .T. ) ;
#82602 = CARTESIAN_POINT ( 'NONE',  ( -15.00246656865998496, 1486.068585992124554, 186.3294758681441863 ) ) ;
#82604 = ORIENTED_EDGE ( 'NONE', *, *, #4861, .F. ) ;
#82603 = CARTESIAN_POINT ( 'NONE',  ( -37.56150324949999941, 1389.587769209160115, 214.8459643147290024 ) ) ;
#82606 = AXIS2_PLACEMENT_3D ( 'NONE', #60890, #68731, #59771 ) ;
#82605 = CARTESIAN_POINT ( 'NONE',  ( -51.77010361138839301, 1385.111386686199921, 265.3579611613769771 ) ) ;
#82607 = CARTESIAN_POINT ( 'NONE',  ( 16.95307557376462171, 1410.872489480477498, 226.3250901887366240 ) ) ;
#82608 = DIRECTION ( 'NONE',  ( 0.07512831038525372152, 0.9801898970571882863, 0.1832580221591280645 ) ) ;
#82609 = CARTESIAN_POINT ( 'NONE',  ( -3.805396659119999914, 1495.647976226690162, 219.6495707272989932 ) ) ;
#82610 = CARTESIAN_POINT ( 'NONE',  ( -5.386185223340929973, 1432.347042777500064, 154.6076275972019971 ) ) ;
#82611 = CARTESIAN_POINT ( 'NONE',  ( 11.52427477660000044, 1425.777060552559988, 203.2852374282489905 ) ) ;
#82612 = DIRECTION ( 'NONE',  ( -1.000000000000000000, 0.000000000000000000, 0.000000000000000000 ) ) ;
#82614 = CARTESIAN_POINT ( 'NONE',  ( 4.038582018629999659, 1515.598601288590089, 209.1218459616989946 ) ) ;
#82613 = CARTESIAN_POINT ( 'NONE',  ( -2.872208748294999836, 1517.145312756229941, 216.4596396827270155 ) ) ;
#82615 = CARTESIAN_POINT ( 'NONE',  ( -22.33897147115630233, 1410.187224944829950, 212.0108098745100165 ) ) ;
#82616 = CARTESIAN_POINT ( 'NONE',  ( 31.69312280309836183, 1525.713797967456685, 221.9404206525572931 ) ) ;
#82617 = EDGE_LOOP ( 'NONE', ( #86769, #69195, #4979, #57699 ) ) ;
#82618 = CARTESIAN_POINT ( 'NONE',  ( 7.328676169885000036, 1516.833844030519913, 202.1788723028969912 ) ) ;
#82619 = FACE_OUTER_BOUND ( 'NONE', #42993, .T. ) ;
#82620 = ORIENTED_EDGE ( 'NONE', *, *, #32954, .F. ) ;
#82621 = AXIS2_PLACEMENT_3D ( 'NONE', #70141, #68466, #59508 ) ;
#82622 = CARTESIAN_POINT ( 'NONE',  ( 7.512705394560745376, 1509.036904579576458, 214.8970114893355117 ) ) ;
#82623 = CARTESIAN_POINT ( 'NONE',  ( 24.34559517319999955, 1444.819512104510068, 214.6978151758279978 ) ) ;
#82624 = CARTESIAN_POINT ( 'NONE',  ( 7.886710164585208460, 1438.222028729959902, 153.7402925291054316 ) ) ;
#82625 = CARTESIAN_POINT ( 'NONE',  ( 8.512085479599107884, 1424.558304799583993, 195.8049112898494855 ) ) ;
#82626 = CIRCLE ( 'NONE', #43318, 11.34254167809999991 ) ;
#82627 = CARTESIAN_POINT ( 'NONE',  ( 0.1504078502939990014, 1443.159176389090135, 218.4019229827389950 ) ) ;
#82628 = CARTESIAN_POINT ( 'NONE',  ( -21.01415622427471774, 1522.051704408389924, 217.3717009491090835 ) ) ;
#82629 = CARTESIAN_POINT ( 'NONE',  ( 31.81407709660769001, 1501.977400791986611, 196.2902540610627682 ) ) ;
#82630 = CARTESIAN_POINT ( 'NONE',  ( -19.98479248519999985, 1427.060832424730052, 224.6412401930980138 ) ) ;
#82631 = CARTESIAN_POINT ( 'NONE',  ( -20.02799630220000182, 1485.574563381989947, 204.1280247810589970 ) ) ;
#82632 = CARTESIAN_POINT ( 'NONE',  ( -103.8748163430000062, 1389.962982481139989, 303.0082707663589758 ) ) ;
#82633 = ADVANCED_FACE ( 'NONE', ( #2702 ), #16928, .T. ) ;
#82634 = CARTESIAN_POINT ( 'NONE',  ( 17.56771607889999842, 1461.948909412230023, 189.9394063172979941 ) ) ;
#82635 = CARTESIAN_POINT ( 'NONE',  ( -105.6555295450000074, 1391.469163183259980, 302.6449347093590063 ) ) ;
#82636 = CARTESIAN_POINT ( 'NONE',  ( -12.91577053000571240, 1469.952397743109032, 269.3566365841412562 ) ) ;
#82637 = ORIENTED_EDGE ( 'NONE', *, *, #90599, .F. ) ;
#82638 = CARTESIAN_POINT ( 'NONE',  ( -105.5440549909999959, 1378.571989651840113, 303.3348456324590074 ) ) ;
#82639 = CARTESIAN_POINT ( 'NONE',  ( 9.840689968320072367, 1506.501081259705870, 189.3968735791325742 ) ) ;
#82640 = CARTESIAN_POINT ( 'NONE',  ( 11.25045121061179998, 1470.461340873429890, 207.4716941246359738 ) ) ;
#82641 = CARTESIAN_POINT ( 'NONE',  ( 1.956220388341530114, 1452.619890567819994, 181.5372545095350176 ) ) ;
#82642 = FACE_OUTER_BOUND ( 'NONE', #83448, .T. ) ;
#82643 = CARTESIAN_POINT ( 'NONE',  ( -13.48104552572402781, 1444.198070212794846, 187.0427700716132620 ) ) ;
#82644 = CARTESIAN_POINT ( 'NONE',  ( -8.311290134334250013, 1511.035127054690065, 215.8965699024140008 ) ) ;
#82645 = CARTESIAN_POINT ( 'NONE',  ( -4.987078460856490203, 1508.551704408389924, 212.6094383991630252 ) ) ;
#82646 = DIRECTION ( 'NONE',  ( 0.000000000000000000, 0.000000000000000000, -1.000000000000000000 ) ) ;
#82648 = ADVANCED_FACE ( 'NONE', ( #3121 ), #58067, .T. ) ;
#82647 = CARTESIAN_POINT ( 'NONE',  ( -14.89895980123599983, 1415.677402202029953, 206.9852695848109931 ) ) ;
#82649 = CARTESIAN_POINT ( 'NONE',  ( 25.00975353569999626, 1436.598045313000057, 137.9330155572980061 ) ) ;
#82650 = CARTESIAN_POINT ( 'NONE',  ( -12.55177817982819555, 1442.776457442548690, 169.4734774201230323 ) ) ;
#82652 = ORIENTED_EDGE ( 'NONE', *, *, #45505, .F. ) ;
#82651 = CARTESIAN_POINT ( 'NONE',  ( -13.79685521319999886, 1409.394857187929802, 225.4822212544980289 ) ) ;
#82653 = CARTESIAN_POINT ( 'NONE',  ( -113.4000000000000057, 1384.913060387289988, 297.2218459572590064 ) ) ;
#82654 = CARTESIAN_POINT ( 'NONE',  ( 14.15402810059180005, 1513.231391185909843, 224.3576605340919912 ) ) ;
#82655 = ADVANCED_FACE ( 'NONE', ( #47299 ), #71447, .F. ) ;
#82656 = ORIENTED_EDGE ( 'NONE', *, *, #37091, .T. ) ;
#82657 = ORIENTED_EDGE ( 'NONE', *, *, #15837, .F. ) ;
#82658 = CARTESIAN_POINT ( 'NONE',  ( -11.84702048589999812, 1501.805044540989911, 210.3943432492690135 ) ) ;
#82659 = DIRECTION ( 'NONE',  ( -0.9942586961433756976, -0.000000000000000000, -0.1070030146457317671 ) ) ;
#82661 = CARTESIAN_POINT ( 'NONE',  ( 1.875671004969999833, 1456.514200624189925, 219.5762891113990065 ) ) ;
#82660 = CARTESIAN_POINT ( 'NONE',  ( 4.974027067470000674, 1455.144349094690142, 217.5915564868190017 ) ) ;
#82662 = CARTESIAN_POINT ( 'NONE',  ( -9.410069260120000223, 1446.992726302889878, 212.1327064560190081 ) ) ;
#82663 = CARTESIAN_POINT ( 'NONE',  ( -11.87145374459999836, 1433.215786360830180, 150.2634173165980087 ) ) ;
#82664 = CARTESIAN_POINT ( 'NONE',  ( -2.487935123034410001, 1509.038615930399828, 213.6090957347729784 ) ) ;
#82665 = CARTESIAN_POINT ( 'NONE',  ( 13.62888593203049936, 1517.051704413129983, 191.9442378289920157 ) ) ;
#82666 = DIRECTION ( 'NONE',  ( -1.000000000000000000, 0.000000000000000000, -1.989567262110869994E-13 ) ) ;
#82667 = CARTESIAN_POINT ( 'NONE',  ( -11.36018337610000195, 1414.996442546130083, 195.9645814914979951 ) ) ;
#82668 = CARTESIAN_POINT ( 'NONE',  ( -4.500000000000000000, 1448.210448412289907, 183.1418046154980175 ) ) ;
#82669 = CARTESIAN_POINT ( 'NONE',  ( -0.2350516018847411404, 1467.133467089303167, 235.6301535849441962 ) ) ;
#82670 = CARTESIAN_POINT ( 'NONE',  ( 0.05571536906665219835, 1361.391559110059688, 207.6218459616988241 ) ) ;
#82671 = CARTESIAN_POINT ( 'NONE',  ( -11.07653839470680346, 1509.424964076853257, 237.0021322192719424 ) ) ;
#82673 = ORIENTED_EDGE ( 'NONE', *, *, #85806, .T. ) ;
#82672 = CARTESIAN_POINT ( 'NONE',  ( 1.575643331409844361, 1473.864451249795366, 219.2446589862094868 ) ) ;
#82674 = ORIENTED_EDGE ( 'NONE', *, *, #82218, .T. ) ;
#82675 = CARTESIAN_POINT ( 'NONE',  ( -11.86538321653400097, 1432.285882802679907, 149.9821595126069838 ) ) ;
#82676 = CARTESIAN_POINT ( 'NONE',  ( -18.87649402730879800, 1504.135318570910158, 222.3338261055430110 ) ) ;
#82677 = CARTESIAN_POINT ( 'NONE',  ( -7.984658461500000470, 1471.246104330929938, 269.8705384494979853 ) ) ;
#82678 = FACE_OUTER_BOUND ( 'NONE', #57909, .T. ) ;
#82680 = ADVANCED_FACE ( 'NONE', ( #12041 ), #37283, .F. ) ;
#82679 = CARTESIAN_POINT ( 'NONE',  ( -113.4000000000000057, 1378.528619065190014, 314.5328508192589538 ) ) ;
#82681 = CARTESIAN_POINT ( 'NONE',  ( 35.55994568960879576, 1450.202733143109981, 136.2282289233990014 ) ) ;
#82682 = CARTESIAN_POINT ( 'NONE',  ( 0.2730310470048849525, 1451.200684518790013, 182.3105317300910144 ) ) ;
#82683 = CARTESIAN_POINT ( 'NONE',  ( -8.605915169659999364, 1384.661630203050208, 199.8779420664789939 ) ) ;
#82684 = CARTESIAN_POINT ( 'NONE',  ( -2.470955845399089856, 1523.580203803270933, 175.3687159542604377 ) ) ;
#82685 = CARTESIAN_POINT ( 'NONE',  ( -4.919805416270000009, 1457.514044444589899, 217.2895299339490123 ) ) ;
#82686 = CARTESIAN_POINT ( 'NONE',  ( 10.72817992001798970, 1363.601820912770791, 207.6218459616987673 ) ) ;
#82687 = CARTESIAN_POINT ( 'NONE',  ( -42.01580735148260004, 1426.337994121050087, 268.6260313102509940 ) ) ;
#82688 = ORIENTED_EDGE ( 'NONE', *, *, #69676, .F. ) ;
#82689 = CARTESIAN_POINT ( 'NONE',  ( -3.549608351769999892, 1507.276797637930031, 180.9704965309979912 ) ) ;
#82690 = ORIENTED_EDGE ( 'NONE', *, *, #71407, .T. ) ;
#82691 = VERTEX_POINT ( 'NONE', #107200 ) ;
#82692 = CARTESIAN_POINT ( 'NONE',  ( -4.608417544644999531, 1516.691389976299888, 211.6120918846570191 ) ) ;
#82693 = CARTESIAN_POINT ( 'NONE',  ( 4.563532145992947875, 1423.757224567328194, 183.7871458247886380 ) ) ;
#82694 = CARTESIAN_POINT ( 'NONE',  ( -2.500000000000000000, 1431.404049859629822, 183.8987783686980038 ) ) ;
#82696 = CARTESIAN_POINT ( 'NONE',  ( 3.968827103902559550, 1519.551704408389924, 188.7040005461919918 ) ) ;
#82695 = CARTESIAN_POINT ( 'NONE',  ( -6.935133418554999096, 1516.613881697390070, 212.3834819030570031 ) ) ;
#82697 = CARTESIAN_POINT ( 'NONE',  ( -17.07773618619999922, 1455.454993475929996, 189.7981302288980032 ) ) ;
#82698 = AXIS2_PLACEMENT_3D ( 'NONE', #76672, #26255, #42513 ) ;
#82699 = CARTESIAN_POINT ( 'NONE',  ( -2.342714119161724451, 1449.671868188517237, 182.9885556723570517 ) ) ;
#82700 = ORIENTED_EDGE ( 'NONE', *, *, #32223, .T. ) ;
#82701 = CARTESIAN_POINT ( 'NONE',  ( -26.24539357829999631, 1435.712694766920094, 136.2621512218979944 ) ) ;
#82702 = CARTESIAN_POINT ( 'NONE',  ( -7.718763544034999313, 1516.905946377369901, 202.1794916586869988 ) ) ;
#82703 = DIRECTION ( 'NONE',  ( -0.9786619618251632957, 0.000000000000000000, 0.2054769195713296581 ) ) ;
#82704 = CARTESIAN_POINT ( 'NONE',  ( -23.30935844142160107, 1384.540784663000068, 202.6730237965640242 ) ) ;
#82705 = CARTESIAN_POINT ( 'NONE',  ( -42.06230369252700285, 1436.187529677659768, 269.6487418071969842 ) ) ;
#82706 = CARTESIAN_POINT ( 'NONE',  ( -17.84338787552430006, 1523.481610118012895, 180.3600277898067930 ) ) ;
#82707 = CARTESIAN_POINT ( 'NONE',  ( -1.249934943059999970, 1397.324122628329860, 196.1772859776979772 ) ) ;
#82709 = ORIENTED_EDGE ( 'NONE', *, *, #81103, .T. ) ;
#82708 = CARTESIAN_POINT ( 'NONE',  ( -8.627444824590488892, 1365.466472467317772, 210.6218459617142003 ) ) ;
#82710 = ORIENTED_EDGE ( 'NONE', *, *, #18889, .F. ) ;
#82711 = DIRECTION ( 'NONE',  ( 0.000000000000000000, 1.000000000000000000, 0.000000000000000000 ) ) ;
#82712 = CARTESIAN_POINT ( 'NONE',  ( -29.61692403810246077, 1526.104292489126692, 220.7563138442914408 ) ) ;
#82713 = CARTESIAN_POINT ( 'NONE',  ( 10.92543524466419846, 1460.873421187279973, 208.4607498083740040 ) ) ;
#82714 = CARTESIAN_POINT ( 'NONE',  ( 18.81609481059999922, 1456.479165729590022, 204.5196734937790097 ) ) ;
#82715 = DIRECTION ( 'NONE',  ( 0.4090087482554363163, 0.000000000000000000, 0.9125304618753946606 ) ) ;
#82716 = CARTESIAN_POINT ( 'NONE',  ( -2.476450702264999748, 1516.843453247299749, 211.4215022863270121 ) ) ;
#82717 = CARTESIAN_POINT ( 'NONE',  ( 7.661183502175981985, 1460.828108340008612, 203.1978207858394967 ) ) ;
#82718 = CARTESIAN_POINT ( 'NONE',  ( 31.23437356469435144, 1512.187213306747481, 195.3468678195113739 ) ) ;
#82719 = CARTESIAN_POINT ( 'NONE',  ( 8.282106953172229780, 1438.168376036569953, 212.2658014659700143 ) ) ;
#82720 = CARTESIAN_POINT ( 'NONE',  ( -13.40958072599999973, 1414.996442553830093, 220.3303866892979954 ) ) ;
#82721 = CARTESIAN_POINT ( 'NONE',  ( 7.550503323924999677, 1510.480349266450048, 203.5706572581269995 ) ) ;
#82722 = CARTESIAN_POINT ( 'NONE',  ( 4.608021669135000664, 1516.660388280709867, 207.4085285224269910 ) ) ;
#82723 = ORIENTED_EDGE ( 'NONE', *, *, #54309, .F. ) ;
#82724 = CARTESIAN_POINT ( 'NONE',  ( -38.81202642568450045, 1436.797832264140197, 135.0584845260209761 ) ) ;
#82725 = CARTESIAN_POINT ( 'NONE',  ( -10.38017169539999962, 1471.876108169690042, 207.0077970564690020 ) ) ;
#82726 = CARTESIAN_POINT ( 'NONE',  ( -23.87523795545963168, 1446.306127926221507, 213.5443193811669857 ) ) ;
#82727 = ORIENTED_EDGE ( 'NONE', *, *, #93262, .T. ) ;
#82728 = CARTESIAN_POINT ( 'NONE',  ( 0.000000000000000000, 1515.551704408389924, 209.1218459616989946 ) ) ;
#82729 = CARTESIAN_POINT ( 'NONE',  ( 12.63077516952419899, 1434.551872175529979, 149.3944923939809826 ) ) ;
#82730 = CARTESIAN_POINT ( 'NONE',  ( 13.56558276610000036, 1415.128105759529944, 197.4687002248980150 ) ) ;
#82731 = CARTESIAN_POINT ( 'NONE',  ( -2.875659595060000129, 1507.251074144529866, 180.8868938330980143 ) ) ;
#82732 = CARTESIAN_POINT ( 'NONE',  ( 2.488082932330000219, 1441.600846913620217, 150.5962877614979902 ) ) ;
#82733 = CARTESIAN_POINT ( 'NONE',  ( 16.17523438889999809, 1409.477912219330165, 225.6432943882979885 ) ) ;
#82734 = CARTESIAN_POINT ( 'NONE',  ( 5.531434274799999606, 1486.727690549889758, 199.8330512247090098 ) ) ;
#82735 = CARTESIAN_POINT ( 'NONE',  ( -3.747504258231699747, 1476.575485711930014, 199.4578548330160004 ) ) ;
#82736 = CARTESIAN_POINT ( 'NONE',  ( 4.280208222382819727, 1441.004501108590148, 156.4771712661509753 ) ) ;
#82737 = CARTESIAN_POINT ( 'NONE',  ( -13.59512407998240135, 1507.703338069740084, 209.3532897553030239 ) ) ;
#82738 = CARTESIAN_POINT ( 'NONE',  ( 16.66094735743510213, 1410.867388111209948, 226.5061907891179942 ) ) ;
#82739 = CARTESIAN_POINT ( 'NONE',  ( -1.125509888415000104, 1517.203017563489766, 216.4609531728469847 ) ) ;
#82740 = ORIENTED_EDGE ( 'NONE', *, *, #58388, .T. ) ;
#82741 = CARTESIAN_POINT ( 'NONE',  ( -17.38831264790000120, 1417.589637829370076, 206.5146517552989849 ) ) ;
#82742 = CARTESIAN_POINT ( 'NONE',  ( -5.932239102140000497, 1391.913060387289988, 203.1292509007990077 ) ) ;
#82743 = CARTESIAN_POINT ( 'NONE',  ( 2.113759566260000167, 1420.502650363029943, 184.8096912009980031 ) ) ;
#82744 = CARTESIAN_POINT ( 'NONE',  ( -15.13389074177019999, 1508.450542589140241, 215.3798312893059972 ) ) ;
#82745 =( BOUNDED_CURVE ( )  B_SPLINE_CURVE ( 3, ( #102113, #25392, #6417, #23749 ),
 .UNSPECIFIED., .F., .F. ) 
 B_SPLINE_CURVE_WITH_KNOTS ( ( 4, 4 ),
 ( 1.282549416709988011, 2.438195290911524982 ),
 .UNSPECIFIED. ) 
 CURVE ( )  GEOMETRIC_REPRESENTATION_ITEM ( )  RATIONAL_B_SPLINE_CURVE ( ( 1.000000000000000000, 0.8917691662025382104, 0.8917691662025382104, 1.000000000000000000 ) ) 
 REPRESENTATION_ITEM ( '' )  );
#82746 = DIRECTION ( 'NONE',  ( 0.9510565162951561957, 0.000000000000000000, 0.3090169943749392911 ) ) ;
#82747 = CARTESIAN_POINT ( 'NONE',  ( -0.04640499230476000103, 1508.911437368330098, 179.6947746304720113 ) ) ;
#82748 = CARTESIAN_POINT ( 'NONE',  ( 11.60004869885214518, 1425.158469683133717, 137.9573055125791541 ) ) ;
#82749 = CARTESIAN_POINT ( 'NONE',  ( -0.5890887500919901321, 1526.382868172863937, 174.9674887555077021 ) ) ;
#82750 = B_SPLINE_CURVE_WITH_KNOTS ( 'NONE', 5,
 ( #108226, #100381, #65144, #7421, #41587, #48904, #47781, #58940, #39928, #75742, #99257, #24742 ),
 .UNSPECIFIED., .F., .F.,
 ( 6, 3, 3, 6 ),
 ( -19.23936229089999728, -13.68355489660000046, -9.538385084389998880, -6.352442800617261298 ),
 .UNSPECIFIED. ) ;
#82751 = CARTESIAN_POINT ( 'NONE',  ( 18.01599769506526272, 1424.260621041340301, 225.3203408571521038 ) ) ;
#82752 = CARTESIAN_POINT ( 'NONE',  ( -12.31942453897649870, 1378.266144378809940, 209.5228905148699994 ) ) ;
#82753 = CARTESIAN_POINT ( 'NONE',  ( -4.041733614507550032E-07, 1407.244919736519932, 222.1486585491760195 ) ) ;
#82754 = CARTESIAN_POINT ( 'NONE',  ( 32.83529528479970594, 1440.913060383310039, 246.2013942643669964 ) ) ;
#82756 = CARTESIAN_POINT ( 'NONE',  ( 9.607334135293850608, 1470.026661626050100, 212.1640507808000109 ) ) ;
#82755 = CARTESIAN_POINT ( 'NONE',  ( -9.980609342266690831, 1471.167102018479909, 211.5702527342239989 ) ) ;
#82757 = DIRECTION ( 'NONE',  ( 1.755985294532464991E-16, -1.000000000000000000, 1.338183447452830017E-16 ) ) ;
#82758 = ORIENTED_EDGE ( 'NONE', *, *, #21376, .T. ) ;
#82759 = ORIENTED_EDGE ( 'NONE', *, *, #20066, .F. ) ;
#82760 = CARTESIAN_POINT ( 'NONE',  ( 10.94662241205340081, 1479.920664513949987, 208.8401849076869894 ) ) ;
#82761 = CARTESIAN_POINT ( 'NONE',  ( 17.13513247068420497, 1410.030456530622814, 192.6342742787495865 ) ) ;
#82762 = CARTESIAN_POINT ( 'NONE',  ( -4.792996137980000348, 1442.435460035689857, 201.1994128016890215 ) ) ;
#82763 = CARTESIAN_POINT ( 'NONE',  ( 7.571421872719999335, 1423.019346856819993, 195.7264222406990086 ) ) ;
#82764 = CARTESIAN_POINT ( 'NONE',  ( -2.500000000000000000, 1411.429641636929773, 137.0999999980979851 ) ) ;
#82765 = CARTESIAN_POINT ( 'NONE',  ( 10.39912873559759987, 1422.379202795500078, 211.6466214762630216 ) ) ;
#82766 = DIRECTION ( 'NONE',  ( 0.000000000000000000, 1.000000000000000000, 0.000000000000000000 ) ) ;
#82767 = CARTESIAN_POINT ( 'NONE',  ( -46.90474178049270648, 1383.817032368400078, 254.9874098474779771 ) ) ;
#82768 = CARTESIAN_POINT ( 'NONE',  ( -5.496430559424999807, 1510.805212328559946, 201.5628357695169939 ) ) ;
#82769 = DIRECTION ( 'NONE',  ( -1.000000000000000000, 0.000000000000000000, 0.000000000000000000 ) ) ;
#82770 = PLANE ( 'NONE',  #30788 ) ;
#82771 = CARTESIAN_POINT ( 'NONE',  ( 11.86058708272519979, 1492.120471498190000, 209.8867464431719725 ) ) ;
#82773 = EDGE_LOOP ( 'NONE', ( #79569, #37576, #22672 ) ) ;
#82772 = DIRECTION ( 'NONE',  ( -0.000000000000000000, -1.000000000000000000, -0.000000000000000000 ) ) ;
#82774 = CARTESIAN_POINT ( 'NONE',  ( -4.992349863779999453, 1391.620913471789891, 214.4361776263990009 ) ) ;
#82775 = CARTESIAN_POINT ( 'NONE',  ( -22.59757997700000232, 1381.457731642620047, 203.6687691534690146 ) ) ;
#82776 = CARTESIAN_POINT ( 'NONE',  ( 4.650616333322320273, 1508.551704408389924, 205.3792392240669926 ) ) ;
#82777 = VERTEX_POINT ( 'NONE', #54625 ) ;
#82778 = ORIENTED_EDGE ( 'NONE', *, *, #32954, .T. ) ;
#82779 = CARTESIAN_POINT ( 'NONE',  ( -7.952410203839279212, 1386.346058257690174, 218.7420460867409986 ) ) ;
#82780 = CARTESIAN_POINT ( 'NONE',  ( -4.020407408646379466, 1515.375307573260216, 205.5795248161299753 ) ) ;
#82782 = CARTESIAN_POINT ( 'NONE',  ( -10.93162616829999934, 1470.132888108789984, 212.2376404388290041 ) ) ;
#82781 = CARTESIAN_POINT ( 'NONE',  ( -11.52810963750000006, 1441.751267666019885, 147.8533156590980013 ) ) ;
#82783 = CARTESIAN_POINT ( 'NONE',  ( -5.284442937980000643, 1463.440241038189924, 200.7106537499089711 ) ) ;
#82784 = CARTESIAN_POINT ( 'NONE',  ( -105.7905112890000083, 1378.790852282349988, 301.9387464688589944 ) ) ;
#82785 = CARTESIAN_POINT ( 'NONE',  ( 3.500000000000000000, 1421.663060387330006, 172.2701767054979882 ) ) ;
#82786 = CARTESIAN_POINT ( 'NONE',  ( 9.850348957860671106, 1409.257042152700024, 197.8655441185040047 ) ) ;
#82787 = B_SPLINE_CURVE_WITH_KNOTS ( 'NONE', 5,
 ( #16913, #102039, #67382, #93097, #7992, #25326, #42713, #76867, #34300 ),
 .UNSPECIFIED., .F., .F.,
 ( 6, 3, 6 ),
 ( 0.000000000000000000, 0.5465110906119712286, 1.000000000000000000 ),
 .UNSPECIFIED. ) ;
#82788 = CARTESIAN_POINT ( 'NONE',  ( 18.02214392489999994, 1424.365982604130068, 225.0542928084979906 ) ) ;
#82789 = CARTESIAN_POINT ( 'NONE',  ( -108.0420188247079949, 1385.240018349089951, 297.1067560861690708 ) ) ;
#82790 = CARTESIAN_POINT ( 'NONE',  ( 1.662820216281789998, 1431.604432834220006, 200.5143882900920005 ) ) ;
#82791 = CARTESIAN_POINT ( 'NONE',  ( 18.02257621027597523, 1526.382868172863937, 235.3484976865586873 ) ) ;
#82792 = CARTESIAN_POINT ( 'NONE',  ( -10.79382269979189957, 1414.913060387349788, 196.1395788316550011 ) ) ;
#82793 = VERTEX_POINT ( 'NONE', #54082 ) ;
#82794 = CARTESIAN_POINT ( 'NONE',  ( -21.44520247467892204, 1525.343727714918259, 184.8098521824372540 ) ) ;
#82795 = CARTESIAN_POINT ( 'NONE',  ( -11.60004869885203682, 1428.983126981193436, 134.0999999980979851 ) ) ;
#82796 = CARTESIAN_POINT ( 'NONE',  ( -12.24435440740000125, 1434.149509971349971, 149.6614242918979869 ) ) ;
#82797 = CARTESIAN_POINT ( 'NONE',  ( -4.184817693673509801E-10, 1466.841376965610152, 244.4596446984610054 ) ) ;
#82798 = CARTESIAN_POINT ( 'NONE',  ( -33.42844755917176514, 1522.382868172863937, 222.1271778627170761 ) ) ;
#82799 = DIRECTION ( 'NONE',  ( -0.03489949670252247976, -0.9993908270190688947, -2.284588939963739914E-07 ) ) ;
#82800 = CARTESIAN_POINT ( 'NONE',  ( -108.8468125590000000, 1386.218237515659894, 311.0462259532590110 ) ) ;
#82801 = CARTESIAN_POINT ( 'NONE',  ( 0.1623851794880000199, 1484.828409465129880, 181.8869582818979893 ) ) ;
#82802 = CARTESIAN_POINT ( 'NONE',  ( -10.52246697409539422, 1361.794959946351355, 208.3718459617010978 ) ) ;
#82803 = CARTESIAN_POINT ( 'NONE',  ( 20.45347777980000004, 1495.695647834889996, 214.2365953844490036 ) ) ;
#82804 = CARTESIAN_POINT ( 'NONE',  ( -19.14726318969999852, 1425.916566196629901, 226.2004032037980039 ) ) ;
#82805 = DIRECTION ( 'NONE',  ( -1.836970198721029688E-16, -1.000000000000000000, 0.000000000000000000 ) ) ;
#82806 = EDGE_CURVE ( 'NONE', #74455, #7609, #96263, .T. ) ;
#82807 = CARTESIAN_POINT ( 'NONE',  ( -1.717139122245000094, 1516.949031626070109, 208.0040058453670042 ) ) ;
#82808 = CARTESIAN_POINT ( 'NONE',  ( 7.121584085660000341, 1409.161751583630121, 222.2855843900980233 ) ) ;
#82809 = PRESENTATION_STYLE_ASSIGNMENT (( #73879 ) ) ;
#82810 = CARTESIAN_POINT ( 'NONE',  ( 8.492686941340000573, 1424.222007991629880, 101.6998295726980075 ) ) ;
#82811 = CARTESIAN_POINT ( 'NONE',  ( 7.393437199623040357, 1425.120646642689962, 212.4672936276909923 ) ) ;
#82812 = VERTEX_POINT ( 'NONE', #80357 ) ;
#82813 = CARTESIAN_POINT ( 'NONE',  ( 29.81189561119999709, 1423.440805375829996, 254.8364577152979962 ) ) ;
#82814 = DIRECTION ( 'NONE',  ( 0.000000000000000000, 1.836970198721029688E-16, 1.000000000000000000 ) ) ;
#82816 = CARTESIAN_POINT ( 'NONE',  ( -17.60618190530000149, 1410.892634225830079, 194.3214822148979977 ) ) ;
#82815 = CARTESIAN_POINT ( 'NONE',  ( 0.5325504066310000617, 1458.410320103429967, 183.0292182426980219 ) ) ;
#82817 = DIRECTION ( 'NONE',  ( -6.123233995736769734E-17, -1.000000000000000000, -1.124819836996399911E-32 ) ) ;
#82818 = CARTESIAN_POINT ( 'NONE',  ( -29.63060408680000180, 1437.055400001079988, 238.0637331587980157 ) ) ;
#82819 = CARTESIAN_POINT ( 'NONE',  ( 7.487063056100070391, 1517.051702153270071, 209.5621714086410066 ) ) ;
#82820 = CARTESIAN_POINT ( 'NONE',  ( 0.7313901380009910635, 1415.506039114428177, 233.2853349926991200 ) ) ;
#82821 = CARTESIAN_POINT ( 'NONE',  ( 30.24883931639999801, 1451.704266439629919, 135.6947013027980233 ) ) ;
#82822 = ORIENTED_EDGE ( 'NONE', *, *, #72103, .T. ) ;
#82823 = DIRECTION ( 'NONE',  ( 0.4978433412588624818, 0.000000000000000000, -0.8672669759446693938 ) ) ;
#82824 = CARTESIAN_POINT ( 'NONE',  ( 11.35976097320000022, 1500.240390108989914, 205.8138550405789999 ) ) ;
#82825 = CARTESIAN_POINT ( 'NONE',  ( 14.42573317639249986, 1420.832147603980047, 228.3843187111120017 ) ) ;
#82826 = CARTESIAN_POINT ( 'NONE',  ( 9.783037280509999434, 1463.178299378289921, 209.2268572133950215 ) ) ;
#82827 = EDGE_LOOP ( 'NONE', ( #102386, #5096, #18448, #44935, #77095 ) ) ;
#82828 = ORIENTED_EDGE ( 'NONE', *, *, #48129, .F. ) ;
#82829 = CARTESIAN_POINT ( 'NONE',  ( -37.21348786970000333, 1384.710338601940066, 210.1738723234790029 ) ) ;
#82830 = CARTESIAN_POINT ( 'NONE',  ( -22.70354091851470102, 1409.705854860960017, 209.2041153040200072 ) ) ;
#82831 = CARTESIAN_POINT ( 'NONE',  ( -3.939734656090000176, 1425.432672367729992, 186.1013744347979753 ) ) ;
#82832 = CARTESIAN_POINT ( 'NONE',  ( 4.679794195664990220, 1508.610718263850003, 205.2601949082799990 ) ) ;
#82833 = CARTESIAN_POINT ( 'NONE',  ( 8.627556093114659319, 1519.551704408389924, 234.1780882150808907 ) ) ;
#82834 = CARTESIAN_POINT ( 'NONE',  ( -0.2986054180299999583, 1498.355349864329810, 236.9494477147979978 ) ) ;
#82835 = CARTESIAN_POINT ( 'NONE',  ( 4.240947575409800052, 1509.032041868229953, 212.8661569781619960 ) ) ;
#82836 = ORIENTED_EDGE ( 'NONE', *, *, #5486, .F. ) ;
#82837 = EDGE_CURVE ( 'NONE', #76524, #46346, #49835, .T. ) ;
#82838 = CARTESIAN_POINT ( 'NONE',  ( 42.05291394628070378, 1455.559135556939964, 267.1115876222309566 ) ) ;
#82839 = ADVANCED_FACE ( 'NONE', ( #46773 ), #17232, .F. ) ;
#82840 = CARTESIAN_POINT ( 'NONE',  ( -1.543833121739990100, 1424.175334750540060, 228.3471663839470125 ) ) ;
#82841 = CARTESIAN_POINT ( 'NONE',  ( -0.07944575511320001171, 1419.763150379130138, 184.3780574224979887 ) ) ;
#82842 = CARTESIAN_POINT ( 'NONE',  ( -3.459156616214999591, 1516.769879638719885, 204.5118493505569859 ) ) ;
#82843 = ORIENTED_EDGE ( 'NONE', *, *, #96197, .T. ) ;
#82845 = EDGE_CURVE ( 'NONE', #85844, #11858, #73447, .T. ) ;
#82844 = CARTESIAN_POINT ( 'NONE',  ( 8.631805628161151489, 1482.492055270540050, 217.1926854337019961 ) ) ;
#82846 = CARTESIAN_POINT ( 'NONE',  ( 15.00007757067209901, 1512.191474810040063, 196.5897778920760288 ) ) ;
#82847 = CARTESIAN_POINT ( 'NONE',  ( 12.74884836167065671, 1442.825961663651242, 186.7702961919069082 ) ) ;
#82848 = ORIENTED_EDGE ( 'NONE', *, *, #34397, .T. ) ;
#82849 = EDGE_LOOP ( 'NONE', ( #36836, #98509, #8660, #25381 ) ) ;
#82850 = CARTESIAN_POINT ( 'NONE',  ( -11.27660745936439923, 1481.154147052749977, 210.7583899964359944 ) ) ;
#82851 = EDGE_CURVE ( 'NONE', #56464, #75143, #91508, .T. ) ;
#82852 = CARTESIAN_POINT ( 'NONE',  ( 17.12015336051587511, 1526.107876515966382, 235.9348256314145829 ) ) ;
#82853 = CARTESIAN_POINT ( 'NONE',  ( -10.50233093623509895, 1470.323195244420049, 212.1312216483660222 ) ) ;
#82854 = CARTESIAN_POINT ( 'NONE',  ( 10.57795761202480200, 1502.789340137210047, 216.2109890099079905 ) ) ;
#82855 = CARTESIAN_POINT ( 'NONE',  ( 12.40160733289999939, 1420.584110886950157, 200.5244703085189997 ) ) ;
#82856 = CARTESIAN_POINT ( 'NONE',  ( 16.56432441049999937, 1409.491499342829911, 193.0008963472980099 ) ) ;
#82857 = CARTESIAN_POINT ( 'NONE',  ( -3.411025239260000230, 1429.511272153089976, 201.4092281563090125 ) ) ;
#82858 = CARTESIAN_POINT ( 'NONE',  ( -4.932281309879999576, 1495.209075895590104, 198.2667700775990056 ) ) ;
#82859 = CARTESIAN_POINT ( 'NONE',  ( 0.03196084884758292749, 1409.231241321286234, 232.6875248013703867 ) ) ;
#82861 = CARTESIAN_POINT ( 'NONE',  ( -106.0073915721780082, 1391.832578719599951, 305.5439016709390216 ) ) ;
#82860 = CARTESIAN_POINT ( 'NONE',  ( -16.76374941339440028, 1414.024291605689996, 191.6492321041440050 ) ) ;
#82862 = CARTESIAN_POINT ( 'NONE',  ( 10.68184976760720062, 1424.590726042679989, 206.5862489259359904 ) ) ;
#82863 = CARTESIAN_POINT ( 'NONE',  ( -25.78156655170059608, 1509.813372604039841, 223.1298223243570078 ) ) ;
#82864 = CARTESIAN_POINT ( 'NONE',  ( 4.823778297959999684, 1426.859560269130043, 144.1938086916980239 ) ) ;
#82865 = ORIENTED_EDGE ( 'NONE', *, *, #37742, .F. ) ;
#82866 = CARTESIAN_POINT ( 'NONE',  ( 4.218847493579999853E-15, 1426.979439823029907, 214.3676144195279676 ) ) ;
#82867 = DIRECTION ( 'NONE',  ( -9.439841191556039654E-47, 1.000000000000000000, -1.836970198721029688E-16 ) ) ;
#82868 = CARTESIAN_POINT ( 'NONE',  ( -84.84319801522730131, 1384.981735787840080, 306.6237177180889830 ) ) ;
#82869 = CARTESIAN_POINT ( 'NONE',  ( -8.875238279790000462, 1385.500419937470042, 199.9517188858189911 ) ) ;
#82870 = CARTESIAN_POINT ( 'NONE',  ( 9.650233255823788880, 1426.324557352379998, 209.5560370033680044 ) ) ;
#82871 = EDGE_CURVE ( 'NONE', #98399, #63715, #61368, .T. ) ;
#82873 = ORIENTED_EDGE ( 'NONE', *, *, #80486, .T. ) ;
#82872 = CARTESIAN_POINT ( 'NONE',  ( 10.94714963045309908, 1423.994054955890078, 203.1837039224479895 ) ) ;
#82874 = CARTESIAN_POINT ( 'NONE',  ( 1.988090766190000025, 1430.930902329289893, 217.9995054648290136 ) ) ;
#82875 = CARTESIAN_POINT ( 'NONE',  ( -2.482344662330000062, 1440.444625599219989, 150.5580151863979950 ) ) ;
#82876 = CARTESIAN_POINT ( 'NONE',  ( -6.673722543209559710, 1476.318849632387128, 217.0466873364883611 ) ) ;
#82877 = CARTESIAN_POINT ( 'NONE',  ( 11.27096283070000027, 1433.884051265439894, 151.5488804711980038 ) ) ;
#82878 = CARTESIAN_POINT ( 'NONE',  ( 39.48812356970000081, 1450.238330950499858, 268.3665355199980240 ) ) ;
#82879 = CARTESIAN_POINT ( 'NONE',  ( 0.7331802501534880889, 1450.881784651950056, 181.3416385694490032 ) ) ;
#82880 = EDGE_CURVE ( 'NONE', #65905, #23724, #29395, .T. ) ;
#82881 =( BOUNDED_SURFACE ( )  B_SPLINE_SURFACE ( 3, 2, ( 
 ( #14242, #79402, #29942 ),
 ( #48431, #72522, #94900 ),
 ( #102181, #3483, #42845 ),
 ( #19699, #63401, #34985 ),
 ( #69165, #11321, #9246 ),
 ( #62868, #12399, #77007 ),
 ( #80162, #68613, #313 ),
 ( #53902, #68069, #37054 ),
 ( #85945, #25461, #26578 ),
 ( #28663, #2937, #79633 ) ),
 .UNSPECIFIED., .F., .F., .F. ) 
 B_SPLINE_SURFACE_WITH_KNOTS ( ( 4, 2, 2, 2, 4 ),
 ( 3, 3 ),
 ( 1.570796326794896558, 1.963495408493620697, 2.356194490192344837, 2.748893571891068976, 3.141592653589793116 ),
 ( 0.000000000000000000, 1.000000000000000000 ),
 .UNSPECIFIED. ) 
 GEOMETRIC_REPRESENTATION_ITEM ( )  RATIONAL_B_SPLINE_SURFACE ( (
 ( 1.000000000000000000, 0.7071067811865869857, 1.000000000000000000),
 ( 1.000000000000000000, 0.7166207884823135865, 1.000000000000000000),
 ( 1.000000000000000000, 0.7259222650905752250, 1.000000000000000000),
 ( 1.000000000000000000, 0.7428408967931670048, 1.000000000000000000),
 ( 1.000000000000000000, 0.7504512394537760089, 1.000000000000000000),
 ( 1.000000000000000000, 0.7630177051937124810, 1.000000000000000000),
 ( 1.000000000000000000, 0.7679730451971344962, 1.000000000000000000),
 ( 1.000000000000000000, 0.7746454561798989946, 1.000000000000000000),
 ( 1.000000000000000000, 0.7763684247033887376, 1.000000000000000000),
 ( 1.000000000000000000, 0.7763623250684346111, 1.000000000000000000) ) ) 
 REPRESENTATION_ITEM ( '' )  SURFACE ( )  );
#82882 = CARTESIAN_POINT ( 'NONE',  ( -16.87694756293090137, 1420.409301044890071, 203.4763756665570327 ) ) ;
#82883 = CARTESIAN_POINT ( 'NONE',  ( 9.636272919195080888, 1459.879703458749873, 204.9556293222869954 ) ) ;
#82884 = CARTESIAN_POINT ( 'NONE',  ( 7.306949285421709739, 1422.442428900340019, 195.7985199449469746 ) ) ;
#82885 = ADVANCED_FACE ( 'NONE', ( #86961 ), #1561, .T. ) ;
#82886 = CIRCLE ( 'NONE', #47183, 1.000000000000000888 ) ;
#82887 = FACE_OUTER_BOUND ( 'NONE', #44436, .T. ) ;
#82888 = CARTESIAN_POINT ( 'NONE',  ( 23.10251669230000360, 1410.654477903330189, 207.3358591529579940 ) ) ;
#82889 = CARTESIAN_POINT ( 'NONE',  ( 31.23437356469435144, 1511.187213306747708, 197.3468678195113739 ) ) ;
#82890 = CARTESIAN_POINT ( 'NONE',  ( -17.47308017059999941, 1410.448094988030107, 225.6071494025980257 ) ) ;
#82891 = CARTESIAN_POINT ( 'NONE',  ( -7.717961373019999627, 1491.908876820690011, 210.2849100519189847 ) ) ;
#82892 = CARTESIAN_POINT ( 'NONE',  ( -5.080289282479999002, 1480.093209919690253, 228.8812397303989883 ) ) ;
#82893 = CARTESIAN_POINT ( 'NONE',  ( 21.32681782946750104, 1525.211473355384669, 183.8595827939377898 ) ) ;
#82894 = CARTESIAN_POINT ( 'NONE',  ( 1.477486471849999816, 1515.342042115489903, 204.8476099990489843 ) ) ;
#82895 = CARTESIAN_POINT ( 'NONE',  ( 7.799999999999998934, 1392.213060387289943, 209.1218459616989946 ) ) ;
#82896 = CARTESIAN_POINT ( 'NONE',  ( -2.130922739460000326, 1467.954349356489956, 220.0452206896989935 ) ) ;
#82897 = CARTESIAN_POINT ( 'NONE',  ( -6.288099047490000260, 1416.823872462329973, 226.3732097004979948 ) ) ;
#82898 = CARTESIAN_POINT ( 'NONE',  ( 8.432239102140002274, 1391.413060387289988, 209.1218459572589836 ) ) ;
#82900 = VERTEX_POINT ( 'NONE', #42762 ) ;
#82899 = FACE_OUTER_BOUND ( 'NONE', #95046, .T. ) ;
#82901 = CARTESIAN_POINT ( 'NONE',  ( -13.74428069829999899, 1415.087818611729972, 199.1627811320679768 ) ) ;
#82902 = DIRECTION ( 'NONE',  ( -0.6736849260863841948, 0.000000000000000000, 0.7390186874254148774 ) ) ;
#82903 = CARTESIAN_POINT ( 'NONE',  ( 13.80559114949999966, 1434.979605424110105, 147.9458860626980083 ) ) ;
#82904 = CARTESIAN_POINT ( 'NONE',  ( -41.62352936867430486, 1444.515901151979961, 134.0999999983539794 ) ) ;
#82905 = CARTESIAN_POINT ( 'NONE',  ( 7.452717793499999743, 1442.053991537899947, 184.4597269369980097 ) ) ;
#82906 = EDGE_LOOP ( 'NONE', ( #44515, #94339, #7738, #12620 ) ) ;
#82907 = B_SPLINE_SURFACE_WITH_KNOTS ( 'NONE', 5, 5, ( 
 ( #66775, #24708, #15216, #42648, #42101, #51057 ),
 ( #93578, #16853, #117, #110397, #7932, #51606 ),
 ( #100874, #17409, #74612, #41552, #85188, #75708 ),
 ( #58356, #101980, #83532, #33132, #92480, #33677 ),
 ( #59468, #23635, #67320, #40986, #49407, #84634 ),
 ( #76249, #85740, #8474, #76802, #109855, #34240 ),
 ( #94138, #101418, #58906, #93037, #6826, #75165 ),
 ( #100347, #57817, #49952, #91942, #109313, #68425 ),
 ( #32598, #102527, #25266, #16310, #24166, #9038 ) ),
 .UNSPECIFIED., .F., .F., .F.,
 ( 6, 3, 6 ),
 ( 6, 6 ),
 ( 0.7655572723410000169, 2.316155491860000026, 3.835724788389999862 ),
 ( 0.000000000000000000, 1.000000000000000000 ),
 .UNSPECIFIED. ) ;
#82908 = CARTESIAN_POINT ( 'NONE',  ( -2.069830134539999644, 1485.439312381189893, 197.8250538963989982 ) ) ;
#82909 = FACE_OUTER_BOUND ( 'NONE', #54247, .T. ) ;
#82910 = CARTESIAN_POINT ( 'NONE',  ( -103.6795216995605244, 1379.963998356777893, 305.2549191247096587 ) ) ;
#82911 = CARTESIAN_POINT ( 'NONE',  ( -11.36633173080000070, 1491.361353432889928, 207.7497694925790199 ) ) ;
#82912 = CARTESIAN_POINT ( 'NONE',  ( 17.84338787571943641, 1501.977400791986611, 237.8836641337660467 ) ) ;
#82913 = CARTESIAN_POINT ( 'NONE',  ( 40.41497139838102726, 1425.029171221357274, 269.1178663084699565 ) ) ;
#82914 = CARTESIAN_POINT ( 'NONE',  ( 22.89347097630000150, 1507.627022993330229, 210.0374582935500030 ) ) ;
#82915 = CARTESIAN_POINT ( 'NONE',  ( -13.51802790139999999, 1379.878742302120145, 211.2357070591689876 ) ) ;
#82916 = CARTESIAN_POINT ( 'NONE',  ( -21.83550407203936672, 1523.678648413191695, 183.2743720722710634 ) ) ;
#82917 = CARTESIAN_POINT ( 'NONE',  ( -56.07992718850910308, 1385.043137000280012, 235.9174924357720045 ) ) ;
#82918 = CARTESIAN_POINT ( 'NONE',  ( -16.68062049856681739, 1524.382868172863937, 236.8314524626098319 ) ) ;
#82919 = CARTESIAN_POINT ( 'NONE',  ( -3.739876349838270109, 1508.551704408389924, 204.4696467160270288 ) ) ;
#82920 = EDGE_LOOP ( 'NONE', ( #29690, #107498, #26162, #31460, #42501 ) ) ;
#82921 = CARTESIAN_POINT ( 'NONE',  ( -28.37476903577010034, 1508.765197044639990, 208.8169969777860047 ) ) ;
#82922 = PRODUCT_DEFINITION ( 'UNKNOWN', '', #38682, #80423 ) ;
#82923 = CARTESIAN_POINT ( 'NONE',  ( -15.97953102573920070, 1409.479266170219944, 225.4412730300549867 ) ) ;
#82925 = ORIENTED_EDGE ( 'NONE', *, *, #102669, .T. ) ;
#82924 = CARTESIAN_POINT ( 'NONE',  ( 0.5054431922854470960, 1412.724905019189919, 184.9686944227329946 ) ) ;
#82926 = DIRECTION ( 'NONE',  ( 0.5032920991127231014, -0.8641163480519905571, 0.000000000000000000 ) ) ;
#82927 = CARTESIAN_POINT ( 'NONE',  ( 40.27303016874642339, 1443.635579762076532, 137.1189739665458092 ) ) ;
#82928 = CARTESIAN_POINT ( 'NONE',  ( -7.544733521240000407, 1384.899971913130003, 219.0877090842990071 ) ) ;
#82929 = CARTESIAN_POINT ( 'NONE',  ( -109.3101328239999930, 1384.844761704930079, 311.2642414982589685 ) ) ;
#82930 = CARTESIAN_POINT ( 'NONE',  ( -0.2673276340219670200, 1419.096787968140006, 184.6139809674839967 ) ) ;
#82931 = CARTESIAN_POINT ( 'NONE',  ( 1.260378580130000037, 1465.786016857930008, 235.4507837586979804 ) ) ;
#82932 = CARTESIAN_POINT ( 'NONE',  ( 19.69577440509999988, 1410.523406920930029, 220.5361315035979999 ) ) ;
#82933 = DIRECTION ( 'NONE',  ( 0.01255267363915089744, 0.04169729272521120744, -0.9990514331924543745 ) ) ;
#82934 = CARTESIAN_POINT ( 'NONE',  ( -16.40174870470000101, 1423.220782154630115, 228.3136831567979925 ) ) ;
#82935 = CARTESIAN_POINT ( 'NONE',  ( 8.761644880424068305, 1498.445921004877619, 199.9006591228519198 ) ) ;
#82936 = CARTESIAN_POINT ( 'NONE',  ( 23.55086976260000142, 1411.110717726029861, 207.7642927257880103 ) ) ;
#82937 = CARTESIAN_POINT ( 'NONE',  ( -102.7365228770999295, 1314.643966242389752, 293.5583688343589301 ) ) ;
#82938 = CARTESIAN_POINT ( 'NONE',  ( 6.940379574320000522, 1431.113060387329824, 226.8285010592979916 ) ) ;
#82939 = CARTESIAN_POINT ( 'NONE',  ( -1.555904870050000000, 1417.383305120430123, 234.5694431353979894 ) ) ;
#82940 = CARTESIAN_POINT ( 'NONE',  ( -8.538839991170000587, 1362.569232148550100, 210.6218459616991936 ) ) ;
#82941 = EDGE_CURVE ( 'NONE', #55821, #67655, #7977, .T. ) ;
#82942 = CARTESIAN_POINT ( 'NONE',  ( 0.7360974386200019870, 1517.045004075700035, 205.0794574309270217 ) ) ;
#82943 = B_SPLINE_CURVE_WITH_KNOTS ( 'NONE', 3,
 ( #14724, #92527, #50553, #84131, #100917, #33176 ),
 .UNSPECIFIED., .F., .F.,
 ( 4, 2, 4 ),
 ( -0.2552102774606619939, -0.1273445234295760009, -2.595975838515229839E-06 ),
 .UNSPECIFIED. ) ;
#82945 = EDGE_CURVE ( 'NONE', #6825, #32838, #40862, .T. ) ;
#82944 = CARTESIAN_POINT ( 'NONE',  ( -10.30745342060079928, 1484.762341913489990, 185.0171830968129996 ) ) ;
#82946 = CARTESIAN_POINT ( 'NONE',  ( -109.1321487942470014, 1384.869787291219836, 311.2644937792119322 ) ) ;
#82947 = CARTESIAN_POINT ( 'NONE',  ( -4.221576979972950561, 1441.604095695570095, 168.5833479033780122 ) ) ;
#82949 = VERTEX_POINT ( 'NONE', #40407 ) ;
#82948 = CARTESIAN_POINT ( 'NONE',  ( -68.49543879489779385, 1379.747280870290069, 280.0944112600439553 ) ) ;
#82950 = VERTEX_POINT ( 'NONE', #58877 ) ;
#82951 = CARTESIAN_POINT ( 'NONE',  ( -9.403799494689495830, 1380.327828722814047, 217.1736609539314031 ) ) ;
#82952 = ORIENTED_EDGE ( 'NONE', *, *, #65494, .T. ) ;
#82953 = CARTESIAN_POINT ( 'NONE',  ( 3.043251597425320032, 1417.779699503100119, 234.3208248802520188 ) ) ;
#82954 = FACE_OUTER_BOUND ( 'NONE', #94253, .T. ) ;
#82956 = CARTESIAN_POINT ( 'NONE',  ( 15.90190012156959831, 1409.720761371890148, 192.1156709633790172 ) ) ;
#82955 = CARTESIAN_POINT ( 'NONE',  ( -11.74144633689528128, 1426.693258465743384, 144.4869926498055293 ) ) ;
#82957 = CARTESIAN_POINT ( 'NONE',  ( 6.564578685215000320, 1517.199196846569976, 210.8299485595169926 ) ) ;
#82958 = CARTESIAN_POINT ( 'NONE',  ( 37.55019156315650264, 1436.545190313800049, 135.0428358297800173 ) ) ;
#82959 = B_SPLINE_CURVE_WITH_KNOTS ( 'NONE', 5,
 ( #21630, #3787, #54737, #73736, #55836, #4319 ),
 .UNSPECIFIED., .F., .F.,
 ( 6, 6 ),
 ( -22.35973423652749759, -7.053367062128510057 ),
 .UNSPECIFIED. ) ;
#82960 = EDGE_CURVE ( 'NONE', #56695, #6679, #99198, .T. ) ;
#82961 = B_SPLINE_CURVE_WITH_KNOTS ( 'NONE', 3,
 ( #92418, #54108, #45704, #80386, #46803, #52990, #96073, #36176, #105033, #3150, #105596 ),
 .UNSPECIFIED., .F., .F.,
 ( 4, 2, 1, 2, 2, 4 ),
 ( 0.000000000000000000, 0.2499999999997608024, 0.3749999999994814703, 0.4374999999994910183, 0.4999999999995006217, 1.000000000000000000 ),
 .UNSPECIFIED. ) ;
#82962 = CARTESIAN_POINT ( 'NONE',  ( 33.93526097501167982, 1435.841486971047743, 135.9408947062673860 ) ) ;
#82963 = CARTESIAN_POINT ( 'NONE',  ( -2.595027496015959834, 1509.076031574679973, 179.4162640487629972 ) ) ;
#82964 = CARTESIAN_POINT ( 'NONE',  ( 11.44122415478343946, 1464.077397819507269, 231.7897981619890118 ) ) ;
#82965 = CARTESIAN_POINT ( 'NONE',  ( 0.000000000000000000, 0.000000000000000000, 0.000000000000000000 ) ) ;
#82966 = CARTESIAN_POINT ( 'NONE',  ( 38.71265708145079287, 1449.925712784929829, 134.0999999982089719 ) ) ;
#82967 = CARTESIAN_POINT ( 'NONE',  ( 3.696509732892085065, 1396.042145351627596, 219.6749981702555488 ) ) ;
#82968 = CARTESIAN_POINT ( 'NONE',  ( -3.071484426853159810, 1470.850312049700051, 187.3986296107530052 ) ) ;
#82969 = LINE ( 'NONE', #109829, #44103 ) ;
#82970 = ORIENTED_EDGE ( 'NONE', *, *, #6256, .T. ) ;
#82971 = ORIENTED_EDGE ( 'NONE', *, *, #86405, .F. ) ;
#82972 = AXIS2_PLACEMENT_3D ( 'NONE', #18786, #44576, #30376 ) ;
#82973 = B_SPLINE_CURVE_WITH_KNOTS ( 'NONE', 5,
 ( #44762, #36333, #13309, #38532, #20611, #80552 ),
 .UNSPECIFIED., .F., .F.,
 ( 6, 6 ),
 ( 177.0697656899999970, 181.8804217290000054 ),
 .UNSPECIFIED. ) ;
#82974 = CARTESIAN_POINT ( 'NONE',  ( -1.739522437470000016, 1431.560227954390029, 203.6467502218990262 ) ) ;
#82975 = DIRECTION ( 'NONE',  ( 0.3363363969984562996, 0.9417419115947303077, -4.718447854657144508E-13 ) ) ;
#82976 = CARTESIAN_POINT ( 'NONE',  ( 12.39029448242800058, 1499.902199860550127, 206.4711935520600150 ) ) ;
#82977 = CARTESIAN_POINT ( 'NONE',  ( -19.39428932798890060, 1507.987873490819993, 209.4883875057280136 ) ) ;
#82978 = CARTESIAN_POINT ( 'NONE',  ( -2.500000000000000000, 1439.419208558560058, 162.1010788394430051 ) ) ;
#82979 = CARTESIAN_POINT ( 'NONE',  ( 4.290508147279999740, 1515.379315998089851, 209.1218459616059988 ) ) ;
#82980 = VECTOR ( 'NONE', #30091, 1000.000000000000000 ) ;
#82981 = CARTESIAN_POINT ( 'NONE',  ( -27.26565262369999942, 1508.025370090229899, 204.2545478268079933 ) ) ;
#82982 = CARTESIAN_POINT ( 'NONE',  ( 38.81202642569470385, 1450.612734564189850, 135.0591088798190071 ) ) ;
#82983 = CARTESIAN_POINT ( 'NONE',  ( 0.9714241662080010942, 1464.771691177589901, 199.1654275922589932 ) ) ;
#82984 = EDGE_CURVE ( 'NONE', #56110, #31476, #94482, .T. ) ;
#82985 = CARTESIAN_POINT ( 'NONE',  ( 7.105427357599999217E-15, 1419.973720559130015, 171.2095165336979790 ) ) ;
#82986 = CARTESIAN_POINT ( 'NONE',  ( 1.523413191080000173, 1416.219761279530076, 190.3037518844979843 ) ) ;
#82987 = CARTESIAN_POINT ( 'NONE',  ( -76.82492145107710257, 1384.777666236809864, 278.4853710401239937 ) ) ;
#82988 = ORIENTED_EDGE ( 'NONE', *, *, #4208, .F. ) ;
#82989 = CARTESIAN_POINT ( 'NONE',  ( -6.555393155154999540, 1516.809497469189864, 201.7937966518470034 ) ) ;
#82990 = CARTESIAN_POINT ( 'NONE',  ( -7.727327152855000492, 1517.232977404109988, 207.4118332116069894 ) ) ;
#82991 = ORIENTED_EDGE ( 'NONE', *, *, #21920, .T. ) ;
#82993 = EDGE_CURVE ( 'NONE', #107006, #88595, #99752, .T. ) ;
#82992 = CARTESIAN_POINT ( 'NONE',  ( 38.48560341180350264, 1440.913060387330006, 265.5651213211320396 ) ) ;
#82994 = CARTESIAN_POINT ( 'NONE',  ( 18.47666778710000202, 1457.021925454829898, 227.5921493168980021 ) ) ;
#82995 = ORIENTED_EDGE ( 'NONE', *, *, #21247, .F. ) ;
#82996 = CARTESIAN_POINT ( 'NONE',  ( -0.07726448487090450956, 1452.995338504329993, 183.2382765356399830 ) ) ;
#82997 = CARTESIAN_POINT ( 'NONE',  ( -8.313145311751080513, 1507.316772571419961, 235.1568484389069909 ) ) ;
#82998 = DIRECTION ( 'NONE',  ( 0.4198226673190290081, -7.712017286126290910E-17, 0.9076061524720597795 ) ) ;
#82999 = CARTESIAN_POINT ( 'NONE',  ( -9.549407038459840180, 1461.437203121739913, 207.3744785622409665 ) ) ;
#83000 = CARTESIAN_POINT ( 'NONE',  ( -4.305050228820000768, 1421.448985974330071, 185.8634108395979752 ) ) ;
#83001 = CARTESIAN_POINT ( 'NONE',  ( -5.385694318444020467, 1511.434991102970116, 200.8007895389870043 ) ) ;
#83002 = CARTESIAN_POINT ( 'NONE',  ( -0.8378200133160000895, 1507.147729961930054, 180.8463070720979999 ) ) ;
#83003 = CARTESIAN_POINT ( 'NONE',  ( 29.79881796581619113, 1526.748660780343471, 196.6633055964653352 ) ) ;
#83004 = CARTESIAN_POINT ( 'NONE',  ( -21.84020450222076803, 1512.187213306747481, 183.2638850454220858 ) ) ;
#83005 = EDGE_CURVE ( 'NONE', #93599, #79565, #104991, .T. ) ;
#83007 = CARTESIAN_POINT ( 'NONE',  ( -10.43907017127172132, 1423.422407654868266, 137.2932306828950288 ) ) ;
#83006 = CARTESIAN_POINT ( 'NONE',  ( 11.96123311770000086, 1461.918702350729745, 232.8139469471979908 ) ) ;
#83008 = CARTESIAN_POINT ( 'NONE',  ( 13.72624666550403560, 1521.951704408389787, 222.4326881308259090 ) ) ;
#83009 = B_SPLINE_CURVE_WITH_KNOTS ( 'NONE', 3,
 ( #38964, #107286, #3758, #63128 ),
 .UNSPECIFIED., .F., .F.,
 ( 4, 4 ),
 ( 0.000000000000000000, 1.000000000000000000 ),
 .UNSPECIFIED. ) ;
#83010 = CARTESIAN_POINT ( 'NONE',  ( -7.329303116114999739, 1516.857992118400034, 216.4524001036569985 ) ) ;
#83011 = ORIENTED_EDGE ( 'NONE', *, *, #55884, .F. ) ;
#83012 = EDGE_CURVE ( 'NONE', #32787, #25418, #26616, .T. ) ;
#83013 = CARTESIAN_POINT ( 'NONE',  ( -0.6994492260031126563, 1486.354407208097427, 181.7735033864214813 ) ) ;
#83014 = FACE_OUTER_BOUND ( 'NONE', #63712, .T. ) ;
#83015 = CARTESIAN_POINT ( 'NONE',  ( 0.1364787244639666663, 1516.894040417452288, 216.8402977076042646 ) ) ;
#83016 = CARTESIAN_POINT ( 'NONE',  ( 2.297085715815000206, 1516.718889242609976, 213.1486234561869821 ) ) ;
#83017 = CARTESIAN_POINT ( 'NONE',  ( 3.778541329980110053, 1515.551842520359969, 212.4904429341349896 ) ) ;
#83018 = CARTESIAN_POINT ( 'NONE',  ( -11.60004869885203682, 1426.458005531418394, 139.1709612739483930 ) ) ;
#83020 = ORIENTED_EDGE ( 'NONE', *, *, #41288, .T. ) ;
#83019 = CARTESIAN_POINT ( 'NONE',  ( 4.534001422476420018, 1508.610336687640029, 213.3588515476280065 ) ) ;
#83021 = CARTESIAN_POINT ( 'NONE',  ( -19.86721352349999847, 1507.838653463430092, 229.2281063170979678 ) ) ;
#83022 = CARTESIAN_POINT ( 'NONE',  ( 8.208155165579999135, 1461.578545524030005, 225.7601664794979968 ) ) ;
#83023 = CARTESIAN_POINT ( 'NONE',  ( -10.96804868159999913, 1432.244841162460034, 151.7696487253979853 ) ) ;
#83024 = CARTESIAN_POINT ( 'NONE',  ( 19.17509738295899879, 1456.935641295649930, 224.9175647810569956 ) ) ;
#83025 = CARTESIAN_POINT ( 'NONE',  ( -57.85314987360000316, 1379.895658628149931, 259.2190729278590311 ) ) ;
#83026 = DIRECTION ( 'NONE',  ( -0.7799412787973096783, 0.3217084223181928548, 0.5368382369369347762 ) ) ;
#83027 = CARTESIAN_POINT ( 'NONE',  ( -8.104271283259439684, 1425.304381095269946, 204.5473957581349964 ) ) ;
#83028 = ADVANCED_FACE ( 'NONE', ( #59441 ), #15107, .F. ) ;
#83029 = CARTESIAN_POINT ( 'NONE',  ( -16.64903386090459847, 1482.394134636929948, 222.3169631199170055 ) ) ;
#83031 = CARTESIAN_POINT ( 'NONE',  ( -10.71468703753418872, 1425.002736333741268, 137.0999999980979567 ) ) ;
#83030 = CARTESIAN_POINT ( 'NONE',  ( -19.45296971400000174, 1482.733639547430130, 228.0655676717979929 ) ) ;
#83032 = CARTESIAN_POINT ( 'NONE',  ( -2.343308038029999985, 1485.565572279829894, 182.6780017771980056 ) ) ;
#83033 = ORIENTED_EDGE ( 'NONE', *, *, #74749, .T. ) ;
#83034 = CARTESIAN_POINT ( 'NONE',  ( 1.702405985064999960, 1516.999105586269934, 205.8518611507970206 ) ) ;
#83035 = CARTESIAN_POINT ( 'NONE',  ( 12.58326012370000058, 1407.771031778829865, 269.4439677704979772 ) ) ;
#83036 = EDGE_CURVE ( 'NONE', #33795, #99633, #58761, .T. ) ;
#83037 = CARTESIAN_POINT ( 'NONE',  ( -0.1068857359190000106, 1409.419549845830261, 185.2272142515979851 ) ) ;
#83038 = CARTESIAN_POINT ( 'NONE',  ( 31.81407709660777527, 1512.187213306747481, 221.9534378623329758 ) ) ;
#83039 = CARTESIAN_POINT ( 'NONE',  ( 23.02916308347723273, 1432.351854092651138, 216.0372900143995878 ) ) ;
#83040 = CARTESIAN_POINT ( 'NONE',  ( -9.929617209772274578, 1390.129315142706446, 216.4882401067509932 ) ) ;
#83041 = LINE ( 'NONE', #6334, #30731 ) ;
#83042 = CARTESIAN_POINT ( 'NONE',  ( -9.724834716106559089E-16, 1374.031200045389824, 209.1218459616989946 ) ) ;
#83043 = CARTESIAN_POINT ( 'NONE',  ( -1.836970198721029983E-15, 1374.913060387289988, 209.1218459572589836 ) ) ;
#83044 = CARTESIAN_POINT ( 'NONE',  ( -1.602465797461561925, 1451.492110311741271, 183.9566778351376399 ) ) ;
#83045 = CARTESIAN_POINT ( 'NONE',  ( -17.73803434250000066, 1408.913060387329779, 209.1218459616979999 ) ) ;
#83046 = CARTESIAN_POINT ( 'NONE',  ( -14.06293010156700163, 1415.542389211330146, 220.9878170194020015 ) ) ;
#83047 = CARTESIAN_POINT ( 'NONE',  ( -10.80145638409999975, 1500.322425017390060, 215.2964120902790057 ) ) ;
#83048 = DIRECTION ( 'NONE',  ( -0.3255681544571569219, -1.836970198721028948E-16, -0.9455185755993167351 ) ) ;
#83049 = B_SPLINE_SURFACE_WITH_KNOTS ( 'NONE', 5, 1, ( 
 ( #15505, #108491 ),
 ( #50261, #92234 ),
 ( #31776, #75464 ),
 ( #23907, #100088 ),
 ( #23370, #91683 ),
 ( #14958, #49153 ),
 ( #100624, #49704 ),
 ( #24460, #83833 ),
 ( #109598, #7135 ) ),
 .UNSPECIFIED., .F., .F., .F.,
 ( 6, 3, 6 ),
 ( 2, 2 ),
 ( 0.000000000000000000, 5.782490304330000441, 11.25975508159999983 ),
 ( -1.500000000000000000, 1.500000000000000000 ),
 .UNSPECIFIED. ) ;
#83050 = VECTOR ( 'NONE', #110251, 1000.000000000000000 ) ;
#83051 = CARTESIAN_POINT ( 'NONE',  ( 20.57820469800335061, 1507.771259987313442, 228.0150961245546455 ) ) ;
#83052 = CARTESIAN_POINT ( 'NONE',  ( 4.227606371040000255, 1441.557582927179965, 165.0907967835979662 ) ) ;
#83053 = CARTESIAN_POINT ( 'NONE',  ( -3.758278191160000059, 1475.720032253530007, 266.9554522522980164 ) ) ;
#83054 = CARTESIAN_POINT ( 'NONE',  ( -4.240346501305279681, 1446.384605478229787, 162.7848567535889970 ) ) ;
#83055 = CARTESIAN_POINT ( 'NONE',  ( -8.551515107930001136, 1437.707591943389843, 226.0657740139990040 ) ) ;
#83056 = CARTESIAN_POINT ( 'NONE',  ( -3.313501335607589748, 1397.551704408390151, 203.0565224509919915 ) ) ;
#83057 = CARTESIAN_POINT ( 'NONE',  ( -44.13200274799689993, 1384.768345979450032, 249.8261944712759828 ) ) ;
#83058 = LINE ( 'NONE', #7995, #23204 ) ;
#83059 = CONICAL_SURFACE ( 'NONE', #99103, 4.000000000000003553, 0.3430239404209998177 ) ;
#83060 = CARTESIAN_POINT ( 'NONE',  ( -9.862951377749247683, 1517.151704408390060, 228.3939896778649654 ) ) ;
#83061 = B_SPLINE_SURFACE_WITH_KNOTS ( 'NONE', 5, 5, ( 
 ( #1253, #85790, #61728, #86342, #10757, #705 ),
 ( #69024, #44928, #53320, #9087, #103126, #19117 ),
 ( #95851, #26427, #87466, #79075, #102024, #25863 ),
 ( #51103, #60065, #8519, #56055, #4016, #28651 ),
 ( #55516, #53891, #88027, #2927, #11311, #37599 ),
 ( #13465, #4552, #47111, #11850, #81237, #29737 ),
 ( #96411, #97504, #90182, #72323, #38142, #106454 ),
 ( #98039, #63924, #62281, #19687, #72861, #21313 ),
 ( #71801, #12387, #89099, #38686, #106996, #30285 ),
 ( #45480, #29199, #80707, #64477, #79623, #96967 ),
 ( #47655, #12930, #20773, #63389, #98592, #81783 ),
 ( #37043, #70694, #71238, #80151, #54974, #105361 ) ),
 .UNSPECIFIED., .F., .F., .F.,
 ( 6, 3, 3, 6 ),
 ( 6, 6 ),
 ( 14.42283113610000100, 18.25245354770000006, 23.76042384160000154, 29.04794202684080062 ),
 ( -1.219754076356229971E-05, 1.479898742370000075 ),
 .UNSPECIFIED. ) ;
#83062 = CARTESIAN_POINT ( 'NONE',  ( 1.353901205137101993, 1408.960339659235160, 230.6360952523062338 ) ) ;
#83063 = CARTESIAN_POINT ( 'NONE',  ( 31.62137330307827909, 1525.231909165033585, 216.6630335337264626 ) ) ;
#83064 = CARTESIAN_POINT ( 'NONE',  ( 8.143458402570486143, 1511.512562116153504, 205.2850637399104698 ) ) ;
#83065 =( BOUNDED_SURFACE ( )  B_SPLINE_SURFACE ( 3, 2, ( 
 ( #100569, #84325, #85409 ),
 ( #15450, #66997, #93805 ),
 ( #42325, #75401, #108990 ),
 ( #102223, #23307, #75928 ),
 ( #59693, #42887, #58590 ),
 ( #76479, #74846, #77045 ) ),
 .UNSPECIFIED., .F., .F., .F. ) 
 B_SPLINE_SURFACE_WITH_KNOTS ( ( 4, 2, 4 ),
 ( 3, 3 ),
 ( -2.732189474663471174E-17, 0.001312027981647287444, 0.002624055963294602209 ),
 ( 0.000000000000000000, 1.000000000000000000 ),
 .UNSPECIFIED. ) 
 GEOMETRIC_REPRESENTATION_ITEM ( )  RATIONAL_B_SPLINE_SURFACE ( (
 ( 1.000000000000000000, 0.9376006582765910036, 1.000000000000000000),
 ( 1.000000000000000000, 0.9569320108028100957, 1.000000000000000000),
 ( 1.000000000000000000, 0.9725743441611582885, 1.000000000000000000),
 ( 1.000000000000000000, 0.9942095667142945015, 1.000000000000000000),
 ( 1.000000000000000000, 1.000043666450159296, 1.000000000000000000),
 ( 1.000000000000000000, 1.000000000000000000, 1.000000000000000000) ) ) 
 REPRESENTATION_ITEM ( '' )  SURFACE ( )  );
#83066 = CARTESIAN_POINT ( 'NONE',  ( -21.38312428220000072, 1410.581396537829960, 200.7860588073580175 ) ) ;
#83067 = CARTESIAN_POINT ( 'NONE',  ( -15.81490237038799940, 1421.038332005997972, 227.0412555000420127 ) ) ;
#83068 = CARTESIAN_POINT ( 'NONE',  ( -3.345579560160000021, 1406.768167790330153, 269.6447283206980501 ) ) ;
#83069 = ORIENTED_EDGE ( 'NONE', *, *, #70651, .T. ) ;
#83070 = B_SPLINE_SURFACE_WITH_KNOTS ( 'NONE', 5, 5, ( 
 ( #16298, #33665, #53263, #102518, #104744, #17958 ),
 ( #76790, #87402, #59458, #68415, #1761, #86840 ),
 ( #86286, #85178, #106, #19058, #103070, #25809 ),
 ( #51595, #9571, #651, #78447, #52154, #26371 ),
 ( #44304, #69523, #94128, #16843, #60566, #43743 ),
 ( #77894, #77349, #70626, #93568, #60008, #85728 ),
 ( #94686, #10696, #8464, #68969, #61667, #34229 ),
 ( #44868, #42637, #17399, #1201, #9027, #104194 ),
 ( #43197, #34782, #35334, #103643, #70081, #26941 ) ),
 .UNSPECIFIED., .F., .F., .F.,
 ( 6, 3, 6 ),
 ( 6, 6 ),
 ( 2.999964336638760276, 5.147071007630000139, 7.294170209094329671 ),
 ( -0.0003925606712395320248, 2.000000000000000000 ),
 .UNSPECIFIED. ) ;
#83071 = LINE ( 'NONE', #22023, #57328 ) ;
#83072 = CARTESIAN_POINT ( 'NONE',  ( -13.59404883793579977, 1507.952376021150030, 209.4255341775249804 ) ) ;
#83073 = CARTESIAN_POINT ( 'NONE',  ( -19.58884347341419740, 1465.811382977840140, 204.1485388397669851 ) ) ;
#83075 = CARTESIAN_POINT ( 'NONE',  ( -2.487935121788300119, 1509.038615937200120, 204.6345961869410246 ) ) ;
#83074 = CARTESIAN_POINT ( 'NONE',  ( 11.40309688480000005, 1425.502102498530121, 141.8402116268979967 ) ) ;
#83076 = CARTESIAN_POINT ( 'NONE',  ( 16.86500409604441231, 1525.697947650497099, 236.3931732427541874 ) ) ;
#83077 = CARTESIAN_POINT ( 'NONE',  ( -14.59898950506980064, 1420.572608572590070, 213.0506973618599886 ) ) ;
#83078 = CARTESIAN_POINT ( 'NONE',  ( -5.504476062790000235, 1453.787349605589952, 201.3614901105490276 ) ) ;
#83079 = EDGE_CURVE ( 'NONE', #45257, #21520, #75998, .T. ) ;
#83080 = CARTESIAN_POINT ( 'NONE',  ( -3.261635970955000019, 1516.613881697390070, 202.1867125516770045 ) ) ;
#83081 = CARTESIAN_POINT ( 'NONE',  ( -15.74021840828143404, 1521.951704408389787, 221.9061614121420973 ) ) ;
#83082 = CARTESIAN_POINT ( 'NONE',  ( -11.90431320224219469, 1398.266029680347174, 203.8981089574260466 ) ) ;
#83083 = CARTESIAN_POINT ( 'NONE',  ( 16.65017489173500209, 1513.596256836700150, 195.0134922709670207 ) ) ;
#83084 = CARTESIAN_POINT ( 'NONE',  ( -20.23525057476570055, 1418.571322831110137, 207.2471207475410040 ) ) ;
#83085 = CARTESIAN_POINT ( 'NONE',  ( -33.87536109878649881, 1377.779994812849964, 222.3620478696320220 ) ) ;
#83086 = CARTESIAN_POINT ( 'NONE',  ( 19.76862476762880050, 1508.335801748439962, 229.3107566332930105 ) ) ;
#83088 = ORIENTED_EDGE ( 'NONE', *, *, #4527, .T. ) ;
#83087 = CARTESIAN_POINT ( 'NONE',  ( -48.20259525819999880, 1379.738770688249815, 241.4393370626590070 ) ) ;
#83089 = ORIENTED_EDGE ( 'NONE', *, *, #68063, .F. ) ;
#83090 = CARTESIAN_POINT ( 'NONE',  ( 11.48004703006369986, 1434.398966934330019, 151.4080194248590203 ) ) ;
#83091 = CARTESIAN_POINT ( 'NONE',  ( -10.93767073350000096, 1397.622345362329952, 216.8369142482779921 ) ) ;
#83092 = CARTESIAN_POINT ( 'NONE',  ( -22.30142397239999852, 1410.611543101329971, 213.5076809071279911 ) ) ;
#83093 = VERTEX_POINT ( 'NONE', #11237 ) ;
#83094 = CARTESIAN_POINT ( 'NONE',  ( -12.76036967837525182, 1444.996034417363035, 169.4538253455069707 ) ) ;
#83095 = CARTESIAN_POINT ( 'NONE',  ( 21.01461835239121001, 1509.697381924852380, 230.2161845864164320 ) ) ;
#83096 = CARTESIAN_POINT ( 'NONE',  ( -0.1681681984989999989, 1405.973120458229914, 121.6099336315979969 ) ) ;
#83098 = CARTESIAN_POINT ( 'NONE',  ( -13.70765206225300048, 1507.670578231209902, 184.2574963778999688 ) ) ;
#83097 = CARTESIAN_POINT ( 'NONE',  ( -2.253566441613126910E-10, 1426.918876941764893, 137.0999999980980135 ) ) ;
#83099 = AXIS2_PLACEMENT_3D ( 'NONE', #37852, #13716, #64173 ) ;
#83100 =( BOUNDED_SURFACE ( )  B_SPLINE_SURFACE ( 3, 2, ( 
 ( #27263, #103393, #84942 ),
 ( #103966, #76556, #110711 ),
 ( #102299, #25584, #35106 ),
 ( #18291, #1525, #93898 ),
 ( #55244, #79886, #64196 ),
 ( #89918, #28367, #30005 ),
 ( #72063, #96686, #54700 ),
 ( #2643, #54150, #106178 ),
 ( #106715, #37879, #72587 ),
 ( #79332, #88826, #98318 ) ),
 .UNSPECIFIED., .F., .F., .F. ) 
 B_SPLINE_SURFACE_WITH_KNOTS ( ( 4, 2, 2, 2, 4 ),
 ( 3, 3 ),
 ( 1.570796326794896558, 1.963495408493620697, 2.356194490192344837, 2.748893571891068976, 3.141592653589793116 ),
 ( 0.000000000000000000, 1.000000000000000000 ),
 .UNSPECIFIED. ) 
 GEOMETRIC_REPRESENTATION_ITEM ( )  RATIONAL_B_SPLINE_SURFACE ( (
 ( 1.000000000000000000, 0.7071067811865867636, 1.000000000000000000),
 ( 1.000000000000000000, 0.7166207884821557128, 1.000000000000000000),
 ( 1.000000000000000000, 0.7259222650907828367, 1.000000000000000000),
 ( 1.000000000000000000, 0.7428408967929600593, 1.000000000000000000),
 ( 1.000000000000000000, 0.7504512394524331942, 1.000000000000000000),
 ( 1.000000000000000000, 0.7630177051950730593, 1.000000000000000000),
 ( 1.000000000000000000, 0.7679730451978846739, 1.000000000000000000),
 ( 1.000000000000000000, 0.7746454561791621396, 1.000000000000000000),
 ( 1.000000000000000000, 0.7763684247039451813, 1.000000000000000000),
 ( 1.000000000000000000, 0.7763623250684347221, 1.000000000000000000) ) ) 
 REPRESENTATION_ITEM ( '' )  SURFACE ( )  );
#83101 = EDGE_CURVE ( 'NONE', #22154, #44485, #30140, .T. ) ;
#83102 = CARTESIAN_POINT ( 'NONE',  ( 1.733308840189999867, 1468.706793215829975, 182.8378066306980259 ) ) ;
#83103 = CARTESIAN_POINT ( 'NONE',  ( -7.292852437050000525, 1414.971279908829956, 193.7940289552979891 ) ) ;
#83104 = CARTESIAN_POINT ( 'NONE',  ( 44.13013120502959907, 1440.913053252359987, 270.2165820558270184 ) ) ;
#83105 = CARTESIAN_POINT ( 'NONE',  ( 11.07286074960780198, 1396.299733205200027, 209.1571633317650196 ) ) ;
#83106 = CARTESIAN_POINT ( 'NONE',  ( 2.500000000000000000, 1419.514443097085177, 137.6548205731159555 ) ) ;
#83107 = CARTESIAN_POINT ( 'NONE',  ( 11.80289981959999857, 1428.296111302430063, 148.4248248087979789 ) ) ;
#83108 = CARTESIAN_POINT ( 'NONE',  ( 7.538480495275000415, 1511.326779185850000, 202.9524984073069618 ) ) ;
#83109 = VERTEX_POINT ( 'NONE', #71725 ) ;
#83110 = CARTESIAN_POINT ( 'NONE',  ( 13.14904837430809970, 1435.770654509489987, 150.5852354599839771 ) ) ;
#83111 = B_SPLINE_CURVE_WITH_KNOTS ( 'NONE', 5,
 ( #42729, #76888, #60097, #88606, #63965, #47148 ),
 .UNSPECIFIED., .F., .F.,
 ( 6, 6 ),
 ( -2.000000000000000000, -4.763377830174775340E-06 ),
 .UNSPECIFIED. ) ;
#83112 = ORIENTED_EDGE ( 'NONE', *, *, #61306, .F. ) ;
#83113 = ORIENTED_EDGE ( 'NONE', *, *, #4374, .F. ) ;
#83114 = CARTESIAN_POINT ( 'NONE',  ( -18.77710419973470124, 1478.090298906489807, 228.5270538965380069 ) ) ;
#83115 = CARTESIAN_POINT ( 'NONE',  ( -10.92412005059999913, 1463.498050678130085, 231.8959999115979826 ) ) ;
#83116 = CARTESIAN_POINT ( 'NONE',  ( -12.93261679799999975, 1416.825245919230156, 196.5037248033980006 ) ) ;
#83117 = CARTESIAN_POINT ( 'NONE',  ( 1.710004548794999968, 1516.557392317769882, 215.6678473207969944 ) ) ;
#83118 = CARTESIAN_POINT ( 'NONE',  ( -12.60784501594030083, 1379.596188776910139, 209.4492041108660203 ) ) ;
#83119 = ORIENTED_EDGE ( 'NONE', *, *, #20070, .T. ) ;
#83120 = CARTESIAN_POINT ( 'NONE',  ( -11.36959371680000075, 1503.847165134090119, 207.0750569533189775 ) ) ;
#83121 = CARTESIAN_POINT ( 'NONE',  ( -37.01195473260000313, 1379.865299478330144, 219.4187096254589733 ) ) ;
#83122 = ORIENTED_EDGE ( 'NONE', *, *, #68564, .F. ) ;
#83123 = CARTESIAN_POINT ( 'NONE',  ( -6.949265684145000677, 1517.089216728169959, 205.6689289091970068 ) ) ;
#83124 = EDGE_LOOP ( 'NONE', ( #2583, #18432, #70299, #49252 ) ) ;
#83125 = CARTESIAN_POINT ( 'NONE',  ( -5.006259886824999228, 1516.939723362869927, 209.1347437590049765 ) ) ;
#83126 = CARTESIAN_POINT ( 'NONE',  ( -20.50069311049999854, 1509.057110915630119, 229.1414337057980219 ) ) ;
#83127 = EDGE_CURVE ( 'NONE', #86947, #18777, #104726, .T. ) ;
#83128 = CARTESIAN_POINT ( 'NONE',  ( -38.49454587240603587, 1428.649003040305843, 269.5844014560237270 ) ) ;
#83129 = CARTESIAN_POINT ( 'NONE',  ( 6.383820954904999567, 1512.069761553120088, 217.4930739719970063 ) ) ;
#83130 = ADVANCED_FACE ( 'NONE', ( #80631 ), #28572, .F. ) ;
#83132 = ORIENTED_EDGE ( 'NONE', *, *, #19041, .F. ) ;
#83131 = CARTESIAN_POINT ( 'NONE',  ( 0.3142797417281940064, 1415.426207913209964, 226.6044974060719994 ) ) ;
#83133 = CARTESIAN_POINT ( 'NONE',  ( -0.01294480814637470091, 1452.645328572880089, 183.2233851132330074 ) ) ;
#83134 = CARTESIAN_POINT ( 'NONE',  ( -28.14800220618010229, 1440.913060388109898, 231.7476473256940039 ) ) ;
#83135 = CARTESIAN_POINT ( 'NONE',  ( -81.19483833489999824, 1384.346490510059994, 304.9342802076590146 ) ) ;
#83136 = CARTESIAN_POINT ( 'NONE',  ( 21.04692457260000182, 1494.868043414790009, 208.8005846134330170 ) ) ;
#83137 = EDGE_CURVE ( 'NONE', #78921, #104968, #54351, .T. ) ;
#83138 = CARTESIAN_POINT ( 'NONE',  ( 7.595213675750000171, 1408.121098801730113, 270.1248737335980081 ) ) ;
#83139 = CIRCLE ( 'NONE', #84876, 26.99999999999999645 ) ;
#83140 = CARTESIAN_POINT ( 'NONE',  ( -7.712490991114999694, 1516.666407245520077, 213.7387074786470009 ) ) ;
#83141 = ADVANCED_FACE ( 'NONE', ( #79000 ), #63849, .F. ) ;
#83142 = CARTESIAN_POINT ( 'NONE',  ( 22.92272308539999770, 1409.722145098229930, 209.1789479422659781 ) ) ;
#83143 = CARTESIAN_POINT ( 'NONE',  ( 11.44665326297827335, 1425.798162341591706, 139.1345266541928538 ) ) ;
#83144 = CARTESIAN_POINT ( 'NONE',  ( 2.194612407920000230, 1441.754231285490050, 218.8080856977990152 ) ) ;
#83145 = CARTESIAN_POINT ( 'NONE',  ( -7.709874534326499607, 1516.566488792059999, 210.6406471876519788 ) ) ;
#83146 = CARTESIAN_POINT ( 'NONE',  ( 0.7579262867720020225, 1516.927039499179955, 210.8260166843570005 ) ) ;
#83147 = CARTESIAN_POINT ( 'NONE',  ( 3.024787391539412425E-15, 1523.409940573003951, 184.4225825198192013 ) ) ;
#83148 = CARTESIAN_POINT ( 'NONE',  ( 0.2805947326950000154, 1419.238439929829838, 184.6459534269980054 ) ) ;
#83149 = CARTESIAN_POINT ( 'NONE',  ( 0.8732702506809227883, 1409.114780694623732, 232.1132175656460674 ) ) ;
#83151 = ORIENTED_EDGE ( 'NONE', *, *, #80522, .F. ) ;
#83150 = CARTESIAN_POINT ( 'NONE',  ( -78.59200839480000411, 1388.281368029709938, 283.6153604521589386 ) ) ;
#83153 = CARTESIAN_POINT ( 'NONE',  ( -41.37939134543219666, 1385.174059347740013, 244.5779111204580261 ) ) ;
#83152 = B_SPLINE_CURVE_WITH_KNOTS ( 'NONE', 3,
 ( #105804, #86776, #78952, #29084, #69454, #10065, #95731, #17891, #52089, #36921, #70014, #26873, #78382, #45356, #9511, #1139, #35270, #61064, #1690, #53193, #35831, #87903, #2258, #104680, #36373, #70562 ),
 .UNSPECIFIED., .F., .F.,
 ( 4, 2, 2, 2, 2, 2, 2, 2, 2, 2, 2, 2, 4 ),
 ( 1.683460768918727255E-14, 0.0002930453684808659613, 0.0005860907369448972986, 0.0008791361054089286359, 0.001172181473872959973, 0.001758272210801022648, 0.002344362947729085322, 0.002637408316193116768, 0.002930453684657148214, 0.003223499053121179660, 0.003516544421585210672, 0.004102635158513215884, 0.004688725895441220662 ),
 .UNSPECIFIED. ) ;
#83154 = FACE_OUTER_BOUND ( 'NONE', #100259, .T. ) ;
#83155 = CARTESIAN_POINT ( 'NONE',  ( 204.2714532754875449, 1526.382868172863937, 223.7095399770875304 ) ) ;
#83156 = PRODUCT_DEFINITION_SHAPE ( 'NONE', 'NONE',  #110839 ) ;
#83157 = CARTESIAN_POINT ( 'NONE',  ( -1.547462741870939906, 1414.913060391199906, 225.9340804956229931 ) ) ;
#83158 = CARTESIAN_POINT ( 'NONE',  ( 10.95098205620359977, 1471.837422849929908, 212.3987392730099657 ) ) ;
#83159 = CARTESIAN_POINT ( 'NONE',  ( 12.91968529760000095, 1421.051477647549973, 203.8574114591390014 ) ) ;
#83160 = CARTESIAN_POINT ( 'NONE',  ( -2.157645518950584762, 1497.833544052899924, 198.0401058465139670 ) ) ;
#83162 = CARTESIAN_POINT ( 'NONE',  ( 9.345710454894810226, 1422.635914553260136, 212.8840094578699791 ) ) ;
#83161 = CARTESIAN_POINT ( 'NONE',  ( -7.328676208015000526, 1516.833844030519913, 216.0648195994369871 ) ) ;
#83163 = CARTESIAN_POINT ( 'NONE',  ( 22.75273496409577945, 1512.187213306747481, 183.6728937936772184 ) ) ;
#83164 = DIRECTION ( 'NONE',  ( 0.000000000000000000, -1.000000000000000000, 0.000000000000000000 ) ) ;
#83165 = EDGE_LOOP ( 'NONE', ( #87095, #83069, #69740, #12670 ) ) ;
#83166 = CARTESIAN_POINT ( 'NONE',  ( -7.719392420504999741, 1516.929962200689943, 202.5670673984569703 ) ) ;
#83167 = EDGE_CURVE ( 'NONE', #28587, #106196, #15888, .T. ) ;
#83168 = CARTESIAN_POINT ( 'NONE',  ( -15.90990504886499757, 1514.921193539169963, 224.3246445042669848 ) ) ;
#83169 = CARTESIAN_POINT ( 'NONE',  ( -0.1665868851619999869, 1457.817907875729816, 229.1616989435979974 ) ) ;
#83170 = AXIS2_PLACEMENT_3D ( 'NONE', #1173, #103039, #103612 ) ;
#83171 = CARTESIAN_POINT ( 'NONE',  ( 23.88591464079999582, 1447.475895483519935, 215.7787009847079958 ) ) ;
#83172 = CARTESIAN_POINT ( 'NONE',  ( 10.78424521582030060, 1461.890582932750249, 211.1530446443910023 ) ) ;
#83173 = EDGE_CURVE ( 'NONE', #2271, #14981, #4046, .T. ) ;
#83174 = CARTESIAN_POINT ( 'NONE',  ( 8.351838315039440630, 1424.363087015397468, 195.8336220494941529 ) ) ;
#83175 = CARTESIAN_POINT ( 'NONE',  ( 4.577412241270000237, 1466.377840905189942, 218.3518450454489823 ) ) ;
#83176 = CARTESIAN_POINT ( 'NONE',  ( 11.16660779294305428, 1418.351232793595273, 229.7242082764032602 ) ) ;
#83177 = CARTESIAN_POINT ( 'NONE',  ( 38.35993494222029909, 1448.483858230149735, 136.4260950382250144 ) ) ;
#83178 = CARTESIAN_POINT ( 'NONE',  ( -19.34868852410000173, 1426.386304191129966, 225.0623401300979936 ) ) ;
#83179 = CARTESIAN_POINT ( 'NONE',  ( -23.61600082529999867, 1436.133981643489960, 140.5568767735979918 ) ) ;
#83180 = CARTESIAN_POINT ( 'NONE',  ( -108.8860473499999983, 1387.891312791299924, 297.6832540484590481 ) ) ;
#83181 = CARTESIAN_POINT ( 'NONE',  ( 8.664645897209998893, 1509.043692491530010, 182.0634199293980089 ) ) ;
#83182 = CARTESIAN_POINT ( 'NONE',  ( -105.5443734370000044, 1391.490361483879951, 303.4240186844589857 ) ) ;
#83183 = CIRCLE ( 'NONE', #38486, 1.000000000000057954 ) ;
#83184 = CARTESIAN_POINT ( 'NONE',  ( -35.98267349529331227, 1456.700699973690234, 269.5452113222285675 ) ) ;
#83185 = ORIENTED_EDGE ( 'NONE', *, *, #41926, .T. ) ;
#83186 = CARTESIAN_POINT ( 'NONE',  ( 0.8167354255590000278, 1432.353341358199941, 150.3995506339979897 ) ) ;
#83187 = CARTESIAN_POINT ( 'NONE',  ( -36.90170175143411768, 1420.766042611142893, 269.2061551430031159 ) ) ;
#83188 = CARTESIAN_POINT ( 'NONE',  ( 11.18053625668549955, 1470.337374907619960, 207.1025468278700146 ) ) ;
#83189 = DIRECTION ( 'NONE',  ( -9.152776640618289361E-47, 1.000000000000000000, -1.836970198721029688E-16 ) ) ;
#83190 = CARTESIAN_POINT ( 'NONE',  ( 11.60004869885204037, 1427.049244394422431, 134.3455896538280570 ) ) ;
#83191 = CARTESIAN_POINT ( 'NONE',  ( -13.21072205002341171, 1443.129466954967029, 186.8022644757624562 ) ) ;
#83192 = B_SPLINE_SURFACE_WITH_KNOTS ( 'NONE', 5, 1, ( 
 ( #109193, #89614 ),
 ( #32479, #13999 ),
 ( #81753, #30252 ),
 ( #65543, #57146 ),
 ( #5059, #91273 ),
 ( #39773, #12905 ) ),
 .UNSPECIFIED., .F., .F., .F.,
 ( 6, 6 ),
 ( 2, 2 ),
 ( 0.000000000000000000, 16.96319496739999977 ),
 ( 0.000000000000000000, 14.00000000000000000 ),
 .UNSPECIFIED. ) ;
#83193 = CARTESIAN_POINT ( 'NONE',  ( -8.654005124046650010, 1437.544186111149884, 209.5117930731329920 ) ) ;
#83194 = CARTESIAN_POINT ( 'NONE',  ( -2.329920886068990171, 1515.492270357839971, 213.2601720499270073 ) ) ;
#83195 = LINE ( 'NONE', #39539, #25282 ) ;
#83196 = CARTESIAN_POINT ( 'NONE',  ( -15.26371167349380009, 1415.677402202059966, 208.6401185093320123 ) ) ;
#83197 = CARTESIAN_POINT ( 'NONE',  ( 24.09734436609999975, 1435.413501786879806, 137.5049309707980001 ) ) ;
#83198 = CARTESIAN_POINT ( 'NONE',  ( -5.498048945769999918, 1436.980437970689991, 209.3664492512450011 ) ) ;
#83200 = ORIENTED_EDGE ( 'NONE', *, *, #105523, .T. ) ;
#83199 = CARTESIAN_POINT ( 'NONE',  ( -14.77051726120000019, 1409.598147220230203, 226.1676228370980084 ) ) ;
#83201 = CARTESIAN_POINT ( 'NONE',  ( -0.007886336557676770082, 1415.935475482089942, 191.2199948426670062 ) ) ;
#83202 = CARTESIAN_POINT ( 'NONE',  ( 7.500396670941167798, 1516.934665496271919, 209.1219157010845322 ) ) ;
#83203 = EDGE_LOOP ( 'NONE', ( #90135, #8221, #55788, #52632 ) ) ;
#83204 = EDGE_LOOP ( 'NONE', ( #83943, #54720, #13251, #105324 ) ) ;
#83205 = CARTESIAN_POINT ( 'NONE',  ( 17.97699752310530030, 1415.938742849230039, 209.2714468986380041 ) ) ;
#83206 = CARTESIAN_POINT ( 'NONE',  ( -18.66420869458028164, 1526.382868172864164, 232.7837831374281166 ) ) ;
#83208 = CARTESIAN_POINT ( 'NONE',  ( -26.58541136219999856, 1440.913060377119791, 225.2688052979979716 ) ) ;
#83207 = CARTESIAN_POINT ( 'NONE',  ( 4.594279763170000308, 1454.322381208490015, 217.3118965033989980 ) ) ;
#83209 = CARTESIAN_POINT ( 'NONE',  ( -5.723713397950000115, 1444.578274639889969, 217.6728780112489972 ) ) ;
#83210 = CARTESIAN_POINT ( 'NONE',  ( -11.72951527989999754, 1433.271247870570051, 150.8356771812979957 ) ) ;
#83211 = FACE_OUTER_BOUND ( 'NONE', #20282, .T. ) ;
#83212 = CARTESIAN_POINT ( 'NONE',  ( 17.60627569411529691, 1410.895669416499913, 224.1775087544040161 ) ) ;
#83213 = LINE ( 'NONE', #108972, #75026 ) ;
#83214 = CARTESIAN_POINT ( 'NONE',  ( -12.72284891840000043, 1416.311719779230089, 195.5584137648980061 ) ) ;
#83215 = FACE_BOUND ( 'NONE', #31503, .T. ) ;
#83216 = CARTESIAN_POINT ( 'NONE',  ( 1.939356653819999998, 1451.897712681530038, 183.5537167668979919 ) ) ;
#83217 = CARTESIAN_POINT ( 'NONE',  ( 7.942782220523640468, 1364.774038235526405, 209.6218459617148824 ) ) ;
#83218 = CARTESIAN_POINT ( 'NONE',  ( -21.40871077047420812, 1509.777521100951390, 188.0411421299259302 ) ) ;
#83220 = ORIENTED_EDGE ( 'NONE', *, *, #22765, .F. ) ;
#83219 = CARTESIAN_POINT ( 'NONE',  ( -2.679525294690940073E-09, 1415.359588412369931, 243.1548238962059827 ) ) ;
#83221 = ORIENTED_EDGE ( 'NONE', *, *, #19408, .F. ) ;
#83222 = CARTESIAN_POINT ( 'NONE',  ( -11.85095945016420060, 1431.285170179160104, 149.8809506189519993 ) ) ;
#83223 = AXIS2_PLACEMENT_3D ( 'NONE', #49324, #29, #84561 ) ;
#83224 = CARTESIAN_POINT ( 'NONE',  ( 19.51639363059999965, 1499.800465969690094, 221.7092710762990180 ) ) ;
#83225 = CARTESIAN_POINT ( 'NONE',  ( -3.182038422270000222, 1473.815937567429955, 270.2907995558980474 ) ) ;
#83226 = CARTESIAN_POINT ( 'NONE',  ( 0.9833190725767226859, 1473.213984233044357, 219.2916102971160512 ) ) ;
#83227 = CARTESIAN_POINT ( 'NONE',  ( -109.2808341013028297, 1358.631207110788409, 311.1659210709986496 ) ) ;
#83228 = CARTESIAN_POINT ( 'NONE',  ( 36.89893150947609968, 1450.594831177580090, 135.9584847841670125 ) ) ;
#83229 = DIRECTION ( 'NONE',  ( 0.4794255386042038380, 0.000000000000000000, 0.8775825618903722036 ) ) ;
#83230 = CARTESIAN_POINT ( 'NONE',  ( -8.369061852370000665, 1384.792577061449947, 199.7768212591290080 ) ) ;
#83231 = CARTESIAN_POINT ( 'NONE',  ( -2.470168521978401088, 1523.481610426287716, 175.3649660270905315 ) ) ;
#83232 = CARTESIAN_POINT ( 'NONE',  ( -5.038090724669999965, 1458.590897767190199, 218.1407348443790113 ) ) ;
#83233 = CARTESIAN_POINT ( 'NONE',  ( 11.28921847714573801, 1367.009324610933390, 208.3718459617010978 ) ) ;
#83234 = CARTESIAN_POINT ( 'NONE',  ( -43.95932380871909828, 1429.872527714419903, 267.6715504426759935 ) ) ;
#83235 = EDGE_LOOP ( 'NONE', ( #109969, #70428, #23719, #85456, #83414 ) ) ;
#83236 = CARTESIAN_POINT ( 'NONE',  ( -13.80599379854099951, 1434.979619881170038, 146.4346930281899972 ) ) ;
#83237 = ORIENTED_EDGE ( 'NONE', *, *, #109837, .F. ) ;
#83238 = ORIENTED_EDGE ( 'NONE', *, *, #56752, .T. ) ;
#83239 = CARTESIAN_POINT ( 'NONE',  ( 2.493073829755000137, 1516.826109302209943, 211.9861720575370043 ) ) ;
#83240 = CARTESIAN_POINT ( 'NONE',  ( 4.640548489927184050, 1423.702551843624406, 183.8769998837497610 ) ) ;
#83241 = CARTESIAN_POINT ( 'NONE',  ( -20.87480701074316869, 1525.712835404586031, 184.1764597564572625 ) ) ;
#83243 = CARTESIAN_POINT ( 'NONE',  ( -4.051722416713680275, 1441.572133640756192, 170.5366858311234353 ) ) ;
#83242 = CARTESIAN_POINT ( 'NONE',  ( 2.298048923505000118, 1516.764084769670262, 212.5672535042169784 ) ) ;
#83244 = CARTESIAN_POINT ( 'NONE',  ( -18.18247686910000027, 1455.458619197430153, 190.5294738202979943 ) ) ;
#83245 = CARTESIAN_POINT ( 'NONE',  ( -2.942030012410809636, 1512.314860016870171, 201.2300683927209946 ) ) ;
#83246 = ORIENTED_EDGE ( 'NONE', *, *, #96527, .F. ) ;
#83247 = CARTESIAN_POINT ( 'NONE',  ( -26.05003822329999963, 1435.407090719000053, 135.4328170717980129 ) ) ;
#83248 = CARTESIAN_POINT ( 'NONE',  ( 5.777745395274999751, 1516.908489800550115, 202.5639360494670029 ) ) ;
#83249 = EDGE_CURVE ( 'NONE', #108494, #98226, #67741, .T. ) ;
#83250 = DIRECTION ( 'NONE',  ( -1.734723475976805580E-13, 0.000000000000000000, 1.000000000000000000 ) ) ;
#83252 = AXIS2_PLACEMENT_3D ( 'NONE', #82718, #6008, #109035 ) ;
#83251 = CARTESIAN_POINT ( 'NONE',  ( -45.99657213052490334, 1384.603192663479831, 219.5987073974170016 ) ) ;
#83253 = CARTESIAN_POINT ( 'NONE',  ( -33.57555963875730498, 1421.581647479509911, 269.7571208528079865 ) ) ;
#83254 = DIRECTION ( 'NONE',  ( 0.9109372852568263790, 0.3047011255600591273, -0.2781195541693470830 ) ) ;
#83255 = CARTESIAN_POINT ( 'NONE',  ( -5.492330765480000210, 1396.104856804229939, 199.1956356928480147 ) ) ;
#83257 = EDGE_LOOP ( 'NONE', ( #81568, #64365, #22709, #26783 ) ) ;
#83256 = CARTESIAN_POINT ( 'NONE',  ( 15.27152964737910068, 1506.433683733550197, 193.3098315259690025 ) ) ;
#83258 = VERTEX_POINT ( 'NONE', #101250 ) ;
#83259 = CARTESIAN_POINT ( 'NONE',  ( -11.87044479798669983, 1432.661806071300134, 149.9816004235700007 ) ) ;
#83260 = CARTESIAN_POINT ( 'NONE',  ( -29.30029655192924309, 1525.907212628473644, 221.3719603026177367 ) ) ;
#83261 = CARTESIAN_POINT ( 'NONE',  ( 5.277460848200000498, 1426.742654866309977, 191.8370381630989812 ) ) ;
#83262 = CARTESIAN_POINT ( 'NONE',  ( -24.97832055750000180, 1436.146980076459840, 137.6305210645979855 ) ) ;
#83263 = CARTESIAN_POINT ( 'NONE',  ( -24.31747465770000005, 1442.264844603690108, 211.7949302672280112 ) ) ;
#83264 = CARTESIAN_POINT ( 'NONE',  ( 6.951175128784999657, 1517.170721208160103, 211.4121022339570004 ) ) ;
#83265 = CARTESIAN_POINT ( 'NONE',  ( 6.024952519936291218, 1460.026342669724045, 201.5977334549522766 ) ) ;
#83266 = CARTESIAN_POINT ( 'NONE',  ( 5.418632516149999745, 1435.861377308850024, 154.6842388019980206 ) ) ;
#83267 = EDGE_CURVE ( 'NONE', #68340, #80530, #104170, .T. ) ;
#83268 = CARTESIAN_POINT ( 'NONE',  ( 8.678413303154190572, 1437.443562278949912, 211.8714791696150144 ) ) ;
#83269 = CARTESIAN_POINT ( 'NONE',  ( -13.25967441350000087, 1414.983771848930019, 220.4242586862980033 ) ) ;
#83270 = CARTESIAN_POINT ( 'NONE',  ( 2.282301578035000222, 1516.836638729160086, 207.4044134838369757 ) ) ;
#83271 = VERTEX_POINT ( 'NONE', #95094 ) ;
#83272 = CARTESIAN_POINT ( 'NONE',  ( -40.71747597329999735, 1448.637563247749995, 134.0999997049979982 ) ) ;
#83273 = CARTESIAN_POINT ( 'NONE',  ( -9.132731034919599367, 1438.960184460119763, 208.5834308107819766 ) ) ;
#83274 = CYLINDRICAL_SURFACE ( 'NONE', #101174, 0.9999999999999927836 ) ;
#83275 = ORIENTED_EDGE ( 'NONE', *, *, #69548, .T. ) ;
#83276 = CARTESIAN_POINT ( 'NONE',  ( 21.53712143570574611, 1523.621879633028584, 234.3036048850996451 ) ) ;
#83277 = CARTESIAN_POINT ( 'NONE',  ( 12.95032542627530070, 1434.763327472709989, 149.4134100183379985 ) ) ;
#83278 = CARTESIAN_POINT ( 'NONE',  ( 14.41084201949999866, 1416.311719782429918, 196.9001076125980205 ) ) ;
#83279 = CARTESIAN_POINT ( 'NONE',  ( 18.18137294690000161, 1507.608465325429734, 188.5297611294979845 ) ) ;
#83280 = CARTESIAN_POINT ( 'NONE',  ( -12.23489732466240021, 1490.237667237379810, 209.6383001084460034 ) ) ;
#83281 = CARTESIAN_POINT ( 'NONE',  ( 3.494924776181328241, 1450.853411195030276, 184.0590517355477971 ) ) ;
#83282 = CARTESIAN_POINT ( 'NONE',  ( 9.627390985499999942, 1488.793226916890035, 203.8059392817090156 ) ) ;
#83283 = CARTESIAN_POINT ( 'NONE',  ( -4.484642789696589915, 1476.314628642159960, 199.7897337046530026 ) ) ;
#83284 = CARTESIAN_POINT ( 'NONE',  ( 23.33747645580530872, 1449.558087810723009, 217.2477752679129139 ) ) ;
#83285 = PLANE ( 'NONE',  #74583 ) ;
#83286 = CARTESIAN_POINT ( 'NONE',  ( 37.14919262310827008, 1450.989556404924770, 134.7273727559652059 ) ) ;
#83287 = CARTESIAN_POINT ( 'NONE',  ( 2.292307230374999616, 1516.548716157039962, 216.0554627912370051 ) ) ;
#83288 = ORIENTED_EDGE ( 'NONE', *, *, #51714, .T. ) ;
#83289 = CARTESIAN_POINT ( 'NONE',  ( 7.718113422873809526, 1516.881120708040044, 208.9373617900340037 ) ) ;
#83290 = CARTESIAN_POINT ( 'NONE',  ( 2.370970874524634286, 1427.002265528474027, 134.0999999980980135 ) ) ;
#83291 = CARTESIAN_POINT ( 'NONE',  ( -17.76136201589839914, 1508.551704408389924, 211.4804395128520014 ) ) ;
#83292 = AXIS2_PLACEMENT_3D ( 'NONE', #61829, #37150, #53987 ) ;
#83293 = CARTESIAN_POINT ( 'NONE',  ( 3.297216976270555264E-15, 1524.340287715038357, 184.7892624828776320 ) ) ;
#83294 = AXIS2_PLACEMENT_3D ( 'NONE', #104862, #55580, #38199 ) ;
#83295 = CARTESIAN_POINT ( 'NONE',  ( -3.076485559970000061, 1476.334861387889987, 220.1839305697990028 ) ) ;
#83296 = EDGE_CURVE ( 'NONE', #73043, #75650, #102378, .T. ) ;
#83297 = CARTESIAN_POINT ( 'NONE',  ( -8561.628222781668228, 50.13405481564041821, 11261.64903810799478 ) ) ;
#83298 = FACE_OUTER_BOUND ( 'NONE', #48749, .T. ) ;
#83299 = CARTESIAN_POINT ( 'NONE',  ( -7.633360230528516865, 1508.421455160203095, 219.5388691105322891 ) ) ;
#83300 = CARTESIAN_POINT ( 'NONE',  ( 18.79647799810000208, 1416.822690122329959, 209.8352284151899880 ) ) ;
#83301 = CARTESIAN_POINT ( 'NONE',  ( -109.1588850255340049, 1385.157736184130044, 297.1405484719870174 ) ) ;
#83302 = CARTESIAN_POINT ( 'NONE',  ( 34.64222682503879724, 1440.913060385429844, 250.2068170142590020 ) ) ;
#83304 = CARTESIAN_POINT ( 'NONE',  ( 4.328003007221930432, 1515.120004566319949, 208.2632874389240101 ) ) ;
#83303 = CARTESIAN_POINT ( 'NONE',  ( -109.3504185190000015, 1384.949684454260023, 297.1387114502589952 ) ) ;
#83305 = CARTESIAN_POINT ( 'NONE',  ( 9.327653393340000321, 1434.415568160490011, 206.2244200652989718 ) ) ;
#83306 = ORIENTED_EDGE ( 'NONE', *, *, #63149, .T. ) ;
#83307 = EDGE_LOOP ( 'NONE', ( #105064, #59146, #27987, #43983 ) ) ;
#83308 = CARTESIAN_POINT ( 'NONE',  ( 8.631780704876279131, 1438.018275767699834, 210.0183142686710198 ) ) ;
#83309 = CARTESIAN_POINT ( 'NONE',  ( -19.59660595549623352, 1485.403676447882845, 190.1777878984926247 ) ) ;
#83310 = CARTESIAN_POINT ( 'NONE',  ( -3.792859824510000255, 1442.868606696990128, 200.6312857326389860 ) ) ;
#83311 = CARTESIAN_POINT ( 'NONE',  ( 11.39524851002120087, 1502.549053284450110, 211.1908584932759823 ) ) ;
#83312 = CARTESIAN_POINT ( 'NONE',  ( -13.15550074822679960, 1379.513481804130151, 208.2695128736829986 ) ) ;
#83313 = CARTESIAN_POINT ( 'NONE',  ( -11.73605607501253800, 1425.975716723378582, 144.1609217550800395 ) ) ;
#83314 = CARTESIAN_POINT ( 'NONE',  ( 0.07192813133532849346, 1508.551704408389924, 220.0014440396450084 ) ) ;
#83315 = CARTESIAN_POINT ( 'NONE',  ( -53.29909992077880077, 1383.806574426890165, 268.0697932026679950 ) ) ;
#83316 = AXIS2_PLACEMENT_3D ( 'NONE', #8804, #68755, #77144 ) ;
#83317 = CARTESIAN_POINT ( 'NONE',  ( -4.827505465935000295, 1511.354819475749991, 200.9509497084369798 ) ) ;
#83318 = CARTESIAN_POINT ( 'NONE',  ( 23.84529322929999751, 1452.080364399029804, 136.9869226563980078 ) ) ;
#83319 = CARTESIAN_POINT ( 'NONE',  ( -11.96237584231419859, 1502.200202672119985, 208.9057378585949891 ) ) ;
#83320 = CARTESIAN_POINT ( 'NONE',  ( 10.93055278244830042, 1491.052779700740075, 210.3465334192150067 ) ) ;
#83322 = EDGE_LOOP ( 'NONE', ( #110250, #78273, #73668, #106011 ) ) ;
#83321 = CARTESIAN_POINT ( 'NONE',  ( 33.93019615848955084, 1522.382868172863937, 220.5829544587961095 ) ) ;
#83323 = CARTESIAN_POINT ( 'NONE',  ( -1.371718781699999834, 1452.291798068730031, 183.7871359344979965 ) ) ;
#83324 = CARTESIAN_POINT ( 'NONE',  ( -66.17857789960000048, 1380.533260727070001, 264.6360122460590105 ) ) ;
#83325 = CARTESIAN_POINT ( 'NONE',  ( 19.80644525996869731, 1508.319852367809972, 229.3611815521799997 ) ) ;
#83326 = ORIENTED_EDGE ( 'NONE', *, *, #29028, .T. ) ;
#83327 = EDGE_LOOP ( 'NONE', ( #64424, #21497, #3748, #59351 ) ) ;
#83328 = CARTESIAN_POINT ( 'NONE',  ( -11.18076303840567043, 1517.151704408390060, 213.9857921429048417 ) ) ;
#83329 = CARTESIAN_POINT ( 'NONE',  ( 34.39071349362669849, 1437.045099478719976, 136.5484881409109903 ) ) ;
#83331 = CARTESIAN_POINT ( 'NONE',  ( 3.625350584860000058, 1486.483312423590178, 219.2891606026990132 ) ) ;
#83330 = CARTESIAN_POINT ( 'NONE',  ( -11.72470770320000000, 1437.821967610810134, 147.7443706334980220 ) ) ;
#83332 = CARTESIAN_POINT ( 'NONE',  ( -8.804296921149999733, 1463.411480388290101, 203.0665974443489858 ) ) ;
#83333 = CARTESIAN_POINT ( 'NONE',  ( -106.1566356689999964, 1380.912478904339878, 299.4828590531589612 ) ) ;
#83334 = CARTESIAN_POINT ( 'NONE',  ( 0.4757565577110009492, 1443.099148102289973, 202.9022611692290070 ) ) ;
#83335 = CARTESIAN_POINT ( 'NONE',  ( -14.33147639189130018, 1508.551704408389924, 215.5212910536350250 ) ) ;
#83336 = CARTESIAN_POINT ( 'NONE',  ( 8.512645889544598887, 1409.210328532190033, 196.8199130449370102 ) ) ;
#83337 = CARTESIAN_POINT ( 'NONE',  ( 0.4960531002210000207, 1409.436441156229876, 185.2773253857980080 ) ) ;
#83338 = CARTESIAN_POINT ( 'NONE',  ( 3.909710721586129534, 1517.151704408390060, 220.4764703678949900 ) ) ;
#83339 = CARTESIAN_POINT ( 'NONE',  ( 2.952227049714620133, 1431.436650656529991, 200.0252637764760095 ) ) ;
#83340 = CARTESIAN_POINT ( 'NONE',  ( 11.57667674939999891, 1432.352206966599852, 151.1966745221979807 ) ) ;
#83341 = DIRECTION ( 'NONE',  ( -0.01305701037215670386, -0.0004560323763018947962, 0.9999146496149624586 ) ) ;
#83342 = VERTEX_POINT ( 'NONE', #84482 ) ;
#83343 = CARTESIAN_POINT ( 'NONE',  ( -0.8115383875230000044, 1428.579607037230062, 149.5143047311979672 ) ) ;
#83344 = CARTESIAN_POINT ( 'NONE',  ( -7.439099705655682016, 1427.747574558798760, 134.0999999980980419 ) ) ;
#83345 = CARTESIAN_POINT ( 'NONE',  ( -12.38857139729999979, 1434.838224429319780, 150.7171454246980034 ) ) ;
#83346 = CARTESIAN_POINT ( 'NONE',  ( -1.384842749328709995E-10, 1466.428514968140007, 243.0202938729159996 ) ) ;
#83347 = CARTESIAN_POINT ( 'NONE',  ( -1.250333264278968182, 1515.565566433391041, 213.0675868911715725 ) ) ;
#83348 = DIRECTION ( 'NONE',  ( -0.000000000000000000, 1.000000000000000000, 0.000000000000000000 ) ) ;
#83349 = CARTESIAN_POINT ( 'NONE',  ( -109.9182707039999940, 1385.320420619579863, 311.4131465352589885 ) ) ;
#83350 = CARTESIAN_POINT ( 'NONE',  ( -113.4000000000000057, 1306.913060387289988, 304.2218459572590064 ) ) ;
#83351 = CARTESIAN_POINT ( 'NONE',  ( -11.32426234103323992, 1362.877771080770117, 208.3718459617010978 ) ) ;
#83352 = DIRECTION ( 'NONE',  ( -0.9455185755993178454, 0.000000000000000000, 0.3255681544571539243 ) ) ;
#83353 = CARTESIAN_POINT ( 'NONE',  ( 13.67340988617599962, 1509.035597116779854, 233.8281335272939714 ) ) ;
#83354 = CARTESIAN_POINT ( 'NONE',  ( -4.775348822359999801, 1443.097051919790147, 200.2639737031189782 ) ) ;
#83355 = CARTESIAN_POINT ( 'NONE',  ( 7.719640903004999721, 1516.939452820819952, 209.1117431028050078 ) ) ;
#83356 = DIRECTION ( 'NONE',  ( 5.980589973904019347E-17, -1.000000000000000000, 1.736889445713099699E-16 ) ) ;
#83357 = B_SPLINE_CURVE_WITH_KNOTS ( 'NONE', 5,
 ( #43081, #18395, #25695, #86175, #10019, #94016, #52039, #51472, #85058, #34114, #35779, #101289, #7806, #110822, #17280 ),
 .UNSPECIFIED., .F., .F.,
 ( 6, 3, 3, 3, 6 ),
 ( -40.68480120859999971, -31.17413108959999946, -27.78806269829999920, -24.40199430689999716, -21.66346122957535059 ),
 .UNSPECIFIED. ) ;
#83358 = CARTESIAN_POINT ( 'NONE',  ( -14.38571989283190078, 1379.606419413119966, 208.0590348354299692 ) ) ;
#83359 = CARTESIAN_POINT ( 'NONE',  ( 7.425514022726639851, 1425.169617594710189, 212.4007796381419837 ) ) ;
#83360 = ORIENTED_EDGE ( 'NONE', *, *, #35850, .T. ) ;
#83361 = CARTESIAN_POINT ( 'NONE',  ( 27.70845915349999800, 1431.442877780980098, 238.1060703150980089 ) ) ;
#83363 = DIRECTION ( 'NONE',  ( -0.9455185755993178454, 0.000000000000000000, 0.3255681544571539243 ) ) ;
#83362 = CARTESIAN_POINT ( 'NONE',  ( -0.5201890262859999448, 1489.031164216529987, 181.6009856616979903 ) ) ;
#83364 = CARTESIAN_POINT ( 'NONE',  ( -2.576756359376459748, 1419.518892921469842, 186.1246943225270059 ) ) ;
#83365 = CARTESIAN_POINT ( 'NONE',  ( -11.53417333799999867, 1422.407019910830059, 220.7517733711979986 ) ) ;
#83366 = CARTESIAN_POINT ( 'NONE',  ( -29.52277910021149410, 1509.964081442534962, 206.5892769569061045 ) ) ;
#83367 = CARTESIAN_POINT ( 'NONE',  ( -3.968827101022720072, 1517.051704408389924, 229.5396913742049776 ) ) ;
#83368 = CARTESIAN_POINT ( 'NONE',  ( -18.95884658670000178, 1416.837177087930058, 207.7798958566280021 ) ) ;
#83369 = ORIENTED_EDGE ( 'NONE', *, *, #72631, .T. ) ;
#83370 = DIRECTION ( 'NONE',  ( 0.4882662618185556469, -0.4884709562387110626, 0.7231819843448625829 ) ) ;
#83371 = LINE ( 'NONE', #39730, #29335 ) ;
#83372 = CARTESIAN_POINT ( 'NONE',  ( 15.93137308367099969, 1422.193468637389742, 227.6991775834419798 ) ) ;
#83373 = CARTESIAN_POINT ( 'NONE',  ( 29.02628104525710029, 1509.926680456929944, 206.2525988547419900 ) ) ;
#83374 = ORIENTED_EDGE ( 'NONE', *, *, #17846, .F. ) ;
#83375 = ORIENTED_EDGE ( 'NONE', *, *, #4853, .T. ) ;
#83376 = CARTESIAN_POINT ( 'NONE',  ( -84.13302388679998955, 1385.053691251499913, 288.0534502569590245 ) ) ;
#83377 = CARTESIAN_POINT ( 'NONE',  ( -24.12229142288359895, 1410.858807618380069, 209.1426138600969864 ) ) ;
#83378 = B_SPLINE_CURVE_WITH_KNOTS ( 'NONE', 3,
 ( #40194, #13311, #82751, #47506, #4932, #107393, #6042, #108502, #64876, #31788, #48054, #97883, #12790, #65979, #88941, #98983, #3871, #56456, #106300, #29583, #90591, #77123, #102835, #25576, #23921, #41847, #15520, #58116, #84403, #41304, #68188, #93342, #51349, #6594, #16071, #67621, #67075, #57573, #8228, #68730, #92249, #8782, #7690, #75477, #32884, #58663, #76549, #109071, #101180, #91697, #14972, #59226 ),
 .UNSPECIFIED., .F., .F.,
 ( 4, 2, 1, 1, 2, 2, 1, 1, 1, 2, 2, 2, 2, 2, 2, 1, 1, 2, 2, 2, 2, 1, 1, 1, 2, 2, 2, 1, 1, 2, 2, 4 ),
 ( 0.000000000000000000, 0.06249999999962202457, 0.09374999999942285056, 0.1093749999993230693, 0.1171874999993217648, 0.1249999999993204602, 0.1874999999986683430, 0.2187499999984028887, 0.2343749999982787102, 0.2421874999982251975, 0.2499999999981717125, 0.3124999999986546872, 0.3437499999989667154, 0.3749999999992787991, 0.4374999999999192313, 0.4687500000002467471, 0.4843750000005004885, 0.4921875000006212253, 0.5000000000007419620, 0.6250000000024934499, 0.6875000000033619774, 0.7187500000038832271, 0.7343750000041439074, 0.7421875000042691406, 0.7460937500042493786, 0.7500000000042296167, 0.8125000000035560443, 0.8437500000031180614, 0.8593750000028943514, 0.8671875000027038372, 0.8750000000025132119, 1.000000000000000000 ),
 .UNSPECIFIED. ) ;
#83379 = ORIENTED_EDGE ( 'NONE', *, *, #102828, .T. ) ;
#83380 = DIRECTION ( 'NONE',  ( 0.000000000000000000, 1.000000000000000000, 0.000000000000000000 ) ) ;
#83381 = CARTESIAN_POINT ( 'NONE',  ( 20.45347777980000004, 1495.695647834889996, 214.2365953844490036 ) ) ;
#83382 = CARTESIAN_POINT ( 'NONE',  ( -0.1019605806445679913, 1450.916620931209991, 185.2438843135239779 ) ) ;
#83384 = AXIS2_PLACEMENT_3D ( 'NONE', #83804, #58619, #66489 ) ;
#83383 = CARTESIAN_POINT ( 'NONE',  ( 3.744428047356039624, 1509.032041130069956, 213.3627866063060026 ) ) ;
#83385 = VERTEX_POINT ( 'NONE', #506 ) ;
#83386 = AXIS2_PLACEMENT_3D ( 'NONE', #13904, #31826, #48091 ) ;
#83387 = EDGE_CURVE ( 'NONE', #30233, #61499, #59311, .T. ) ;
#83388 = CARTESIAN_POINT ( 'NONE',  ( 46.12601432200399643, 1442.805762345989933, 266.9727633061970096 ) ) ;
#83389 = CARTESIAN_POINT ( 'NONE',  ( -4.554954834814580522, 1508.731366863229823, 205.6342592302619892 ) ) ;
#83390 = CARTESIAN_POINT ( 'NONE',  ( 0.01016139356220000130, 1420.445651128929967, 183.2785305846980179 ) ) ;
#83391 =( BOUNDED_SURFACE ( )  B_SPLINE_SURFACE ( 4, 2, ( 
 ( #54446, #10200, #62870 ),
 ( #97519, #37058, #61739 ),
 ( #46036, #62295, #43811 ),
 ( #96982, #105376, #70156 ),
 ( #88582, #10768, #80166 ) ),
 .UNSPECIFIED., .F., .F., .T. ) 
 B_SPLINE_SURFACE_WITH_KNOTS ( ( 5, 5 ),
 ( 3, 3 ),
 ( 1.967616199060000071, 3.613988937050000239 ),
 ( 5.300753508050029872, 6.148918325191019996 ),
 .UNSPECIFIED. ) 
 GEOMETRIC_REPRESENTATION_ITEM ( )  RATIONAL_B_SPLINE_SURFACE ( (
 ( 0.8627701935039280290, 0.8230948968151540202, 0.9542086668560899598),
 ( 0.8627701935039280290, 0.8230948968151540202, 0.9542086668560899598),
 ( 0.8627701935039280290, 0.8230948968151540202, 0.9542086668560899598),
 ( 0.8627701935039280290, 0.8230948968151540202, 0.9542086668560899598),
 ( 0.8627701935039280290, 0.8230948968151540202, 0.9542086668560899598) ) ) 
 REPRESENTATION_ITEM ( '' )  SURFACE ( )  );
#83392 = CARTESIAN_POINT ( 'NONE',  ( 6.547881374914999775, 1516.647534046129977, 205.6658385469270058 ) ) ;
#83393 = ORIENTED_EDGE ( 'NONE', *, *, #107543, .T. ) ;
#83394 = CARTESIAN_POINT ( 'NONE',  ( 18.40544744198233218, 1458.966239857264327, 227.7214915631488452 ) ) ;
#83395 = CARTESIAN_POINT ( 'NONE',  ( 15.30763528260880157, 1512.674009804160050, 195.6562266886770090 ) ) ;
#83396 = CARTESIAN_POINT ( 'NONE',  ( 3.722374432750000128, 1427.445946224140016, 212.8307634929090284 ) ) ;
#83397 = ORIENTED_EDGE ( 'NONE', *, *, #75460, .F. ) ;
#83398 = CARTESIAN_POINT ( 'NONE',  ( 2.664611940229999920, 1448.598609929289978, 183.3941765823980177 ) ) ;
#83400 = EDGE_CURVE ( 'NONE', #69273, #96354, #5572, .T. ) ;
#83399 = CARTESIAN_POINT ( 'NONE',  ( 27.01855575919810093, 1451.963933047730052, 135.0858731167039934 ) ) ;
#83401 = CARTESIAN_POINT ( 'NONE',  ( -14.15402813869910048, 1513.231391185889834, 193.8860313682340006 ) ) ;
#83403 = CARTESIAN_POINT ( 'NONE',  ( 5.931178066143490746, 1504.797995861300024, 220.4212288460319940 ) ) ;
#83402 = CIRCLE ( 'NONE', #103058, 2.027965567643763567 ) ;
#83404 = CARTESIAN_POINT ( 'NONE',  ( 7.749386596619999956, 1421.739053608140011, 195.8155783956989922 ) ) ;
#83405 = CARTESIAN_POINT ( 'NONE',  ( 1.285768303291729975, 1431.378437453980041, 218.5251442782430047 ) ) ;
#83406 = CARTESIAN_POINT ( 'NONE',  ( -11.48467662286570068, 1491.814333413060012, 204.7694204252460111 ) ) ;
#83407 = CARTESIAN_POINT ( 'NONE',  ( -5.218327569770000451, 1496.717035854290089, 199.1635217715490001 ) ) ;
#83408 = CARTESIAN_POINT ( 'NONE',  ( 1.890470286680180134, 1408.979077064439934, 186.8977652987280180 ) ) ;
#83410 = CARTESIAN_POINT ( 'NONE',  ( -113.4000000000000057, 1305.913060387289988, 304.2218459572590064 ) ) ;
#83409 = CARTESIAN_POINT ( 'NONE',  ( -16.70783830106690004, 1412.306682225960003, 191.6972782329859797 ) ) ;
#83411 = CARTESIAN_POINT ( 'NONE',  ( 10.69336184592519956, 1424.688236166109846, 206.5739417092179906 ) ) ;
#83412 = CARTESIAN_POINT ( 'NONE',  ( -11.86940574820000016, 1378.451602169099942, 212.7299449014490165 ) ) ;
#83413 = CARTESIAN_POINT ( 'NONE',  ( 2.439001525050000119, 1430.488531030629929, 150.2249694046979869 ) ) ;
#83414 = ORIENTED_EDGE ( 'NONE', *, *, #63323, .F. ) ;
#83415 = CARTESIAN_POINT ( 'NONE',  ( 6.215408291180000155, 1427.423536210829980, 214.3676144191779827 ) ) ;
#83416 = FACE_OUTER_BOUND ( 'NONE', #1204, .T. ) ;
#83417 = CARTESIAN_POINT ( 'NONE',  ( 32.05392771830349830, 1524.756004293091792, 202.1328669733503318 ) ) ;
#83418 = CARTESIAN_POINT ( 'NONE',  ( -8.762939274969999914, 1387.561927349079951, 200.2973833142889930 ) ) ;
#83419 = CARTESIAN_POINT ( 'NONE',  ( 10.69109047475079954, 1427.380511044090099, 209.6415026742359942 ) ) ;
#83420 = CARTESIAN_POINT ( 'NONE',  ( 12.26400251256059981, 1421.315719094279984, 203.4348889297749849 ) ) ;
#83421 = CARTESIAN_POINT ( 'NONE',  ( 1.618075321620000118, 1431.058998840389904, 218.0723462992190207 ) ) ;
#83422 = PLANE ( 'NONE',  #90735 ) ;
#83423 = FACE_OUTER_BOUND ( 'NONE', #65623, .T. ) ;
#83424 = CARTESIAN_POINT ( 'NONE',  ( 11.93338584299999994, 1433.461450241920147, 149.9037928783980078 ) ) ;
#83425 = CARTESIAN_POINT ( 'NONE',  ( 18.93537658700000037, 1468.059964608529981, 268.3665355201979992 ) ) ;
#83426 = CARTESIAN_POINT ( 'NONE',  ( -16.79355120555579717, 1420.470915846049820, 203.2250788671829866 ) ) ;
#83427 = CARTESIAN_POINT ( 'NONE',  ( -109.1387513648781038, 1387.705443260920674, 297.5371259159040278 ) ) ;
#83428 = CARTESIAN_POINT ( 'NONE',  ( -14.92155151558594106, 1422.314549108387382, 229.4637292657217813 ) ) ;
#83429 = CARTESIAN_POINT ( 'NONE',  ( -17.74532079129999929, 1486.483557334729994, 188.0959163475980063 ) ) ;
#83430 = CARTESIAN_POINT ( 'NONE',  ( 10.37251527352099956, 1441.250888917769998, 153.2543604269490061 ) ) ;
#83431 = CARTESIAN_POINT ( 'NONE',  ( -17.25956576649999974, 1409.515777705929850, 224.0944197546979808 ) ) ;
#83432 = CARTESIAN_POINT ( 'NONE',  ( 4.283856666023710069, 1440.956247486469920, 155.9231014612180104 ) ) ;
#83433 = CIRCLE ( 'NONE', #12002, 32.13701971169416538 ) ;
#83434 = CARTESIAN_POINT ( 'NONE',  ( -1.096329832589999942, 1473.937728199189905, 216.5791357104590134 ) ) ;
#83435 = CARTESIAN_POINT ( 'NONE',  ( -22.74803453391479735, 1523.678648413191695, 183.6833808205264802 ) ) ;
#83436 = CARTESIAN_POINT ( 'NONE',  ( 12.78667967550000029, 1416.822694282129987, 222.9174006480979813 ) ) ;
#83437 = CARTESIAN_POINT ( 'NONE',  ( -2.038847259689249736, 1522.382868172863937, 173.3106345060153046 ) ) ;
#83438 = CYLINDRICAL_SURFACE ( 'NONE', #38448, 0.9999999999999942268 ) ;
#83439 = DIRECTION ( 'NONE',  ( 0.8771707526546712597, 0.03063147977167200720, -0.4792005667090091237 ) ) ;
#83440 = CARTESIAN_POINT ( 'NONE',  ( 0.2063577645740160005, 1459.399669238419847, 182.9788367490870087 ) ) ;
#83442 = ORIENTED_EDGE ( 'NONE', *, *, #93355, .F. ) ;
#83441 = CARTESIAN_POINT ( 'NONE',  ( 9.504367897392947739, 1467.890094308543212, 205.9436694967274946 ) ) ;
#83443 = CARTESIAN_POINT ( 'NONE',  ( -27.40283359139997543, 1444.740067931808653, 161.6370709818978639 ) ) ;
#83444 = CARTESIAN_POINT ( 'NONE',  ( -28.01253743957580156, 1509.025311965089941, 210.6956320615649929 ) ) ;
#83445 = CARTESIAN_POINT ( 'NONE',  ( 11.87564264789999946, 1433.006668304930145, 147.6243415688980178 ) ) ;
#83446 = CARTESIAN_POINT ( 'NONE',  ( -41.10614458632299772, 1440.770232259229942, 134.0999999980669770 ) ) ;
#83447 = CARTESIAN_POINT ( 'NONE',  ( -109.7181425929999961, 1384.896750758799953, 297.0862127012590008 ) ) ;
#83448 = EDGE_LOOP ( 'NONE', ( #87898, #68824, #80716, #25794 ) ) ;
#83449 = CARTESIAN_POINT ( 'NONE',  ( -5.433843300389891162, 1391.480867605429921, 203.3409103162060205 ) ) ;
#83450 = B_SPLINE_CURVE_WITH_KNOTS ( 'NONE', 3,
 ( #53796, #11222, #2828, #11754 ),
 .UNSPECIFIED., .F., .F.,
 ( 4, 4 ),
 ( 0.000000000000000000, 0.0002220129587134778289 ),
 .UNSPECIFIED. ) ;
#83451 = LINE ( 'NONE', #65580, #90323 ) ;
#83452 = CARTESIAN_POINT ( 'NONE',  ( -104.1632271132076539, 1380.312642488052916, 306.9056418433917770 ) ) ;
#83453 = FACE_OUTER_BOUND ( 'NONE', #93554, .T. ) ;
#83454 = CARTESIAN_POINT ( 'NONE',  ( -2.469737631213410278, 1507.227429411520006, 221.7265308815400147 ) ) ;
#83455 = CARTESIAN_POINT ( 'NONE',  ( 38.84918024652115065, 1422.961239324861481, 269.1580888396505316 ) ) ;
#83456 = DIRECTION ( 'NONE',  ( -0.000000000000000000, -1.000000000000000000, -0.000000000000000000 ) ) ;
#83457 = CARTESIAN_POINT ( 'NONE',  ( -12.57230900989999967, 1379.603104922460261, 209.9510306230349954 ) ) ;
#83458 = CARTESIAN_POINT ( 'NONE',  ( 3.426760023489999973, 1434.222170298339961, 184.7792794946979882 ) ) ;
#83459 = CARTESIAN_POINT ( 'NONE',  ( -55.78789393184250400, 1385.041865729660230, 235.3527397816559983 ) ) ;
#83460 = CARTESIAN_POINT ( 'NONE',  ( 12.51099983133400073, 1416.825784014559986, 196.0986189223339977 ) ) ;
#83461 = CARTESIAN_POINT ( 'NONE',  ( 9.840543299160298574, 1424.658749102479987, 208.3834677199979808 ) ) ;
#83462 = VERTEX_POINT ( 'NONE', #16153 ) ;
#83463 = CARTESIAN_POINT ( 'NONE',  ( -33.93392822810000098, 1451.575813952230192, 135.5854759724980170 ) ) ;
#83464 = CARTESIAN_POINT ( 'NONE',  ( -15.88978672354079968, 1409.721424571740044, 226.1318342661600127 ) ) ;
#83466 = VERTEX_POINT ( 'NONE', #50356 ) ;
#83465 = CARTESIAN_POINT ( 'NONE',  ( 3.843703091317430154, 1437.067272161539904, 227.2460596593799949 ) ) ;
#83467 = CARTESIAN_POINT ( 'NONE',  ( 5.469129087219999796, 1473.910357677790216, 219.1569924984989939 ) ) ;
#83468 = CARTESIAN_POINT ( 'NONE',  ( 9.600627300107769102, 1470.542558681519949, 212.2539986962150067 ) ) ;
#83469 = ADVANCED_FACE ( 'NONE', ( #26216 ), #16692, .F. ) ;
#83470 = CARTESIAN_POINT ( 'NONE',  ( 17.69622264849999738, 1430.679833671289771, 213.5595385020990022 ) ) ;
#83471 = CARTESIAN_POINT ( 'NONE',  ( -109.6605131529999824, 1384.774622188049989, 311.3207091772589479 ) ) ;
#83472 = CARTESIAN_POINT ( 'NONE',  ( -0.08002646896166820678, 1420.301969961120221, 183.4692128524420127 ) ) ;
#83473 = EDGE_CURVE ( 'NONE', #3217, #89419, #6975, .T. ) ;
#83474 = CARTESIAN_POINT ( 'NONE',  ( 17.98939361210000243, 1410.465183417029948, 222.9682872111980032 ) ) ;
#83475 = CARTESIAN_POINT ( 'NONE',  ( 0.3919100467378520136, 1450.899374586919976, 181.2708617675390030 ) ) ;
#83476 = CARTESIAN_POINT ( 'NONE',  ( -17.48680721799999915, 1424.154378231430201, 227.6286878164980010 ) ) ;
#83477 = CARTESIAN_POINT ( 'NONE',  ( 11.23074002719829068, 1499.222125023890158, 203.1659919298568013 ) ) ;
#83478 = LINE ( 'NONE', #68372, #101401 ) ;
#83479 = CARTESIAN_POINT ( 'NONE',  ( -113.4000000000000057, 1314.643966242390206, 293.5583688343590438 ) ) ;
#83480 = CARTESIAN_POINT ( 'NONE',  ( -4.098601998020408921, 1370.943769148376759, 208.3718459617010978 ) ) ;
#83481 = CARTESIAN_POINT ( 'NONE',  ( -2.805707806560000073, 1456.378508730689873, 200.0530498395189909 ) ) ;
#83482 = CARTESIAN_POINT ( 'NONE',  ( -6.561995998525000040, 1517.083030555940013, 205.8633713531569924 ) ) ;
#83483 = AXIS2_PLACEMENT_3D ( 'NONE', #16587, #41284, #56999 ) ;
#83484 = CARTESIAN_POINT ( 'NONE',  ( -5.567394890084230497, 1485.997473811110240, 182.5242378165860089 ) ) ;
#83485 = ORIENTED_EDGE ( 'NONE', *, *, #82851, .T. ) ;
#83486 = CARTESIAN_POINT ( 'NONE',  ( -109.1334478349630075, 1384.772525000819996, 311.2620895989360292 ) ) ;
#83487 = CARTESIAN_POINT ( 'NONE',  ( -4.236735269543610016, 1441.469422925089930, 163.3606698496620027 ) ) ;
#83489 = EDGE_LOOP ( 'NONE', ( #6541, #98113, #63550, #40202 ) ) ;
#83488 = CARTESIAN_POINT ( 'NONE',  ( -68.55293641758220247, 1379.747413382150171, 280.1582828589500309 ) ) ;
#83490 = CARTESIAN_POINT ( 'NONE',  ( -8.196710778187490831, 1382.211539317200504, 218.4653390582963368 ) ) ;
#83491 = VERTEX_POINT ( 'NONE', #85021 ) ;
#83492 = CARTESIAN_POINT ( 'NONE',  ( -16.60697873886304876, 1513.055456493683550, 221.1753219165195219 ) ) ;
#83493 = CARTESIAN_POINT ( 'NONE',  ( 11.08618182320000045, 1501.737459411990130, 206.1990983140089782 ) ) ;
#83495 = CARTESIAN_POINT ( 'NONE',  ( 15.85651032225270107, 1410.713550775690010, 191.5263126459360024 ) ) ;
#83494 = CARTESIAN_POINT ( 'NONE',  ( -11.74088322070292634, 1426.277669831848698, 144.4824319529912202 ) ) ;
#83496 = CARTESIAN_POINT ( 'NONE',  ( 0.01265818781360149997, 1516.959716008189844, 210.8316124642570060 ) ) ;
#83497 = B_SPLINE_CURVE_WITH_KNOTS ( 'NONE', 3,
 ( #66919, #98839, #48462, #32739, #24326, #58509, #83690, #92639, #22099, #15913 ),
 .UNSPECIFIED., .F., .F.,
 ( 4, 2, 2, 2, 4 ),
 ( 0.000000000000000000, 0.0007403986298595332041, 0.001480797259719066408, 0.002221195889578599612, 0.002961594519438132816 ),
 .UNSPECIFIED. ) ;
#83498 = CARTESIAN_POINT ( 'NONE',  ( 41.66793448034960079, 1443.219079709529979, 135.6262679568360170 ) ) ;
#83499 = CARTESIAN_POINT ( 'NONE',  ( -11.15486294749999985, 1425.160588235329897, 144.1660541355979888 ) ) ;
#83500 = DIRECTION ( 'NONE',  ( 0.000000000000000000, 1.000000000000000000, 0.000000000000000000 ) ) ;
#83501 = CARTESIAN_POINT ( 'NONE',  ( 4.383261023904437614, 1466.449861621304308, 233.9444969100850642 ) ) ;
#83502 = AXIS2_PLACEMENT_3D ( 'NONE', #77378, #18541, #26972 ) ;
#83503 = EDGE_CURVE ( 'NONE', #15766, #92171, #36958, .T. ) ;
#83504 = DIRECTION ( 'NONE',  ( -0.4999999999998399058, 0.7071067811867739472, 0.4999999999998399058 ) ) ;
#83505 = CARTESIAN_POINT ( 'NONE',  ( -2.500000000000000000, 1443.913060387330006, 150.6726614421979775 ) ) ;
#83506 = ORIENTED_EDGE ( 'NONE', *, *, #91939, .T. ) ;
#83507 = CARTESIAN_POINT ( 'NONE',  ( 24.04367183769999983, 1494.655699983489967, 207.1743773500889745 ) ) ;
#83508 = DIRECTION ( 'NONE',  ( -0.6736849260863839728, 0.000000000000000000, 0.7390186874254150995 ) ) ;
#83509 = ORIENTED_EDGE ( 'NONE', *, *, #62050, .T. ) ;
#83510 = ORIENTED_EDGE ( 'NONE', *, *, #4958, .F. ) ;
#83511 = LINE ( 'NONE', #40965, #7342 ) ;
#83512 = CARTESIAN_POINT ( 'NONE',  ( 10.44661746959009996, 1453.078959294469996, 210.9304775587480094 ) ) ;
#83513 = APPLICATION_CONTEXT ( 'automotive_design' ) ;
#83514 = FACE_OUTER_BOUND ( 'NONE', #54121, .T. ) ;
#83515 = CARTESIAN_POINT ( 'NONE',  ( -2.330134121946666692, 1515.499673595108106, 213.2081603283779998 ) ) ;
#83516 = CARTESIAN_POINT ( 'NONE',  ( -2.500000000000000000, 1439.402073989899918, 161.8071971399309916 ) ) ;
#83517 = CARTESIAN_POINT ( 'NONE',  ( 20.20959865099471031, 1522.382868172863937, 182.0120230947219966 ) ) ;
#83518 = VECTOR ( 'NONE', #11057, 1000.000000000000000 ) ;
#83519 = CARTESIAN_POINT ( 'NONE',  ( -26.74681214179999955, 1508.000506563529825, 202.6166866765980217 ) ) ;
#83520 = CARTESIAN_POINT ( 'NONE',  ( 38.81202640299100182, 1436.797832147280133, 135.6938345645050106 ) ) ;
#83521 = CARTESIAN_POINT ( 'NONE',  ( 2.502076662800340134, 1421.306659195480051, 183.2871562736519877 ) ) ;
#83522 = CARTESIAN_POINT ( 'NONE',  ( 29.41145171355093879, 1525.795403621571268, 221.5574853780759383 ) ) ;
#83523 = CARTESIAN_POINT ( 'NONE',  ( -10.55745637339999909, 1391.553749436410044, 215.2492821215389824 ) ) ;
#83524 = CARTESIAN_POINT ( 'NONE',  ( -82.21554644036051229, 1384.805079599279907, 285.8412598054820251 ) ) ;
#83525 = EDGE_LOOP ( 'NONE', ( #68177, #48516, #15786, #51337, #65592, #39853, #28593, #61259 ) ) ;
#83526 = CARTESIAN_POINT ( 'NONE',  ( -1.708721022705000037, 1516.531533746980131, 201.8006767011069940 ) ) ;
#83527 = CARTESIAN_POINT ( 'NONE',  ( 6.935801261535000428, 1516.621991115350056, 207.9918434378369909 ) ) ;
#83528 = VERTEX_POINT ( 'NONE', #43047 ) ;
#83529 = DIRECTION ( 'NONE',  ( -0.9455185755993166241, 1.675808339056839216E-14, 0.3255681544571569219 ) ) ;
#83530 = CARTESIAN_POINT ( 'NONE',  ( -0.002089120988227474544, 1451.815318029500077, 154.0389770418792921 ) ) ;
#83531 = ORIENTED_EDGE ( 'NONE', *, *, #33330, .F. ) ;
#83532 = CARTESIAN_POINT ( 'NONE',  ( -14.08840122829999864, 1415.996778985530000, 221.5650976514979789 ) ) ;
#83533 = EDGE_CURVE ( 'NONE', #88894, #43306, #62765, .T. ) ;
#83534 = CARTESIAN_POINT ( 'NONE',  ( -11.84451602989710040, 1432.336085667850057, 150.3016814433159993 ) ) ;
#83535 = CARTESIAN_POINT ( 'NONE',  ( -2.958237724348658393, 1515.068899831253702, 213.4511871771338178 ) ) ;
#83536 = CARTESIAN_POINT ( 'NONE',  ( 11.18076303840565799, 1517.051704408389924, 204.2578997804941707 ) ) ;
#83537 = CARTESIAN_POINT ( 'NONE',  ( 20.79738390328718722, 1511.187213306747708, 181.2030061003470394 ) ) ;
#83538 = CARTESIAN_POINT ( 'NONE',  ( 14.13657958834579986, 1436.257374515989795, 150.1576261981630012 ) ) ;
#83539 = CARTESIAN_POINT ( 'NONE',  ( -1.531246620494349863E-13, 1515.064792882589927, 204.7923971856590128 ) ) ;
#83540 = CARTESIAN_POINT ( 'NONE',  ( -6.105460705908933861, 1510.769285144274590, 201.6400650806163242 ) ) ;
#83541 = CARTESIAN_POINT ( 'NONE',  ( 24.17850564169770067, 1447.751960943020094, 206.2131088459789794 ) ) ;
#83543 = CARTESIAN_POINT ( 'NONE',  ( -12.25009443214260152, 1507.051235695380001, 190.1744699773550167 ) ) ;
#83542 = CARTESIAN_POINT ( 'NONE',  ( 13.72863203839999890, 1461.767185418329973, 230.8959970784979987 ) ) ;
#83544 = CARTESIAN_POINT ( 'NONE',  ( -4.644457551160845910, 1422.126592464929672, 184.6658150771102953 ) ) ;
#83545 = CIRCLE ( 'NONE', #65673, 1.000000000000000888 ) ;
#83546 = CARTESIAN_POINT ( 'NONE',  ( 2.485217193935000068, 1516.534320418310244, 216.8308781079170160 ) ) ;
#83547 = VERTEX_POINT ( 'NONE', #69367 ) ;
#83548 = LINE ( 'NONE', #107108, #12227 ) ;
#83549 = DIRECTION ( 'NONE',  ( -0.02617694830788839730, 0.9996573249755569268, 0.000000000000000000 ) ) ;
#83550 = CARTESIAN_POINT ( 'NONE',  ( -22.07691418023513918, 1523.843271061951100, 233.7988799057568201 ) ) ;
#83551 = CARTESIAN_POINT ( 'NONE',  ( 2.879642153204999833, 1516.812046502680005, 212.5681757458869754 ) ) ;
#83552 = CARTESIAN_POINT ( 'NONE',  ( 18.51267882970000045, 1508.236097878829924, 188.5103842655979918 ) ) ;
#83553 = CARTESIAN_POINT ( 'NONE',  ( -2.466508595303360085, 1483.693203563210091, 198.7383541362370067 ) ) ;
#83555 = ORIENTED_EDGE ( 'NONE', *, *, #6559, .T. ) ;
#83554 = CARTESIAN_POINT ( 'NONE',  ( -4.261736551907977955, 1515.372048949686587, 211.4519800884182246 ) ) ;
#83556 = CARTESIAN_POINT ( 'NONE',  ( 0.9136860870960000769, 1489.469559537029909, 187.0247168341979886 ) ) ;
#83557 = CARTESIAN_POINT ( 'NONE',  ( 2.375641846589999773, 1508.210248838890038, 220.4645691950989885 ) ) ;
#83558 = CARTESIAN_POINT ( 'NONE',  ( -11.56091194390000076, 1431.144279896319858, 151.0927142626980242 ) ) ;
#83559 = CARTESIAN_POINT ( 'NONE',  ( -15.55456937169999954, 1415.677402205460112, 209.5577859103179890 ) ) ;
#83560 = CARTESIAN_POINT ( 'NONE',  ( -109.9467939726550014, 1384.263593440159866, 311.4193346354339837 ) ) ;
#83561 = CARTESIAN_POINT ( 'NONE',  ( 9.236167301360001858, 1423.625854809029988, 144.1549878472980026 ) ) ;
#83562 = CARTESIAN_POINT ( 'NONE',  ( -6.021347807395219576, 1427.070447557959824, 201.9849352095830000 ) ) ;
#83563 = CARTESIAN_POINT ( 'NONE',  ( 12.29928450579999932, 1445.315142612919999, 187.0920815097979926 ) ) ;
#83564 = ADVANCED_FACE ( 'NONE', ( #17242 ), #6173, .T. ) ;
#83566 = CARTESIAN_POINT ( 'NONE',  ( -11.05549909325160129, 1482.557859868360083, 206.1126638933569950 ) ) ;
#83565 = CARTESIAN_POINT ( 'NONE',  ( -26.64855247050000386, 1508.005992643229774, 213.8736264213379741 ) ) ;
#83568 = CARTESIAN_POINT ( 'NONE',  ( -19.23853081770000273, 1466.576780668189940, 213.8528554934590034 ) ) ;
#83567 = AXIS2_PLACEMENT_3D ( 'NONE', #7563, #92121, #15397 ) ;
#83569 = VERTEX_POINT ( 'NONE', #29536 ) ;
#83570 = CARTESIAN_POINT ( 'NONE',  ( -6.949574985774999547, 1517.102359858469754, 205.8627441332170065 ) ) ;
#83571 = CARTESIAN_POINT ( 'NONE',  ( 12.67137506719999962, 1407.308516313030168, 266.8981195266979967 ) ) ;
#83572 = EDGE_CURVE ( 'NONE', #20921, #79507, #30219, .T. ) ;
#83573 = CARTESIAN_POINT ( 'NONE',  ( 0.1796731001380000026, 1410.302589273230069, 185.0125001767980280 ) ) ;
#83574 = CARTESIAN_POINT ( 'NONE',  ( 10.93965183780649930, 1490.038857010280026, 208.6218812487679770 ) ) ;
#83575 = CARTESIAN_POINT ( 'NONE',  ( 24.46704740869997963, 1438.251643707298626, 212.7269232099579881 ) ) ;
#83576 = CARTESIAN_POINT ( 'NONE',  ( 2.960916190616809995, 1454.351986964310072, 218.0342237851930065 ) ) ;
#83577 = CARTESIAN_POINT ( 'NONE',  ( 9.196349486490200675, 1522.051704408389924, 214.4668224883511698 ) ) ;
#83578 = CARTESIAN_POINT ( 'NONE',  ( 17.96267386539620503, 1457.880262292270345, 230.1796244582303927 ) ) ;
#83579 = CARTESIAN_POINT ( 'NONE',  ( -15.01829424220000142, 1417.605436662430293, 203.9468348563890174 ) ) ;
#83580 = CARTESIAN_POINT ( 'NONE',  ( -13.47721440219999955, 1444.366909545699855, 187.4582783821979888 ) ) ;
#83581 = CARTESIAN_POINT ( 'NONE',  ( -19.84205502019262823, 1485.634645662600633, 190.5026249870552704 ) ) ;
#83582 = CARTESIAN_POINT ( 'NONE',  ( -5.202920445667687410, 1495.777355175065622, 199.0561123049738512 ) ) ;
#83583 = CARTESIAN_POINT ( 'NONE',  ( -4.325805437739999704, 1515.203925700790023, 210.5851323563490212 ) ) ;
#83584 = CARTESIAN_POINT ( 'NONE',  ( -13.08147547106499964, 1513.492015765619954, 195.3332637180670019 ) ) ;
#83585 = CIRCLE ( 'NONE', #101393, 0.9999999999999947820 ) ;
#83586 = CARTESIAN_POINT ( 'NONE',  ( -26.93833921311239976, 1508.003628666910117, 211.6437312287430075 ) ) ;
#83587 = CARTESIAN_POINT ( 'NONE',  ( -3.756925840770000136, 1475.646169757629877, 269.0400499448979872 ) ) ;
#83588 = CARTESIAN_POINT ( 'NONE',  ( -4.221461939218559500, 1446.221127877819981, 168.5609095037160046 ) ) ;
#83589 = CARTESIAN_POINT ( 'NONE',  ( -15.20279846676549873, 1514.921193439789931, 193.2119408159660168 ) ) ;
#83590 = EDGE_CURVE ( 'NONE', #26374, #103670, #37398, .T. ) ;
#83591 = CARTESIAN_POINT ( 'NONE',  ( 17.64653741881929960, 1410.885868213330014, 223.6671089294119952 ) ) ;
#83592 = CARTESIAN_POINT ( 'NONE',  ( -47.10372409975749974, 1384.754037987969923, 255.7871177528320175 ) ) ;
#83593 = CARTESIAN_POINT ( 'NONE',  ( -107.0320685023289968, 1391.913060387289988, 301.6402820273519865 ) ) ;
#83594 = AXIS2_PLACEMENT_3D ( 'NONE', #86402, #16955, #34894 ) ;
#83595 = CARTESIAN_POINT ( 'NONE',  ( 16.49511133113979966, 1507.275789587220061, 193.5424140907059893 ) ) ;
#83596 = CARTESIAN_POINT ( 'NONE',  ( -25.28355254197510149, 1470.075220752909900, 211.5054833620599766 ) ) ;
#83597 = CARTESIAN_POINT ( 'NONE',  ( -16.48487877296663129, 1525.795403383247276, 236.4701076103954165 ) ) ;
#83598 = CARTESIAN_POINT ( 'NONE',  ( -45.67177343128329881, 1440.913044206929953, 266.1885934837860077 ) ) ;
#83599 = EDGE_CURVE ( 'NONE', #43475, #13362, #22623, .T. ) ;
#83600 = CARTESIAN_POINT ( 'NONE',  ( -21.22058966110000000, 1410.149336617530025, 200.8725164463980093 ) ) ;
#83601 = EDGE_CURVE ( 'NONE', #63032, #71548, #49907, .T. ) ;
#83602 = CARTESIAN_POINT ( 'NONE',  ( -8.744618109030934505, 1382.059479685067572, 200.2933607043580366 ) ) ;
#83603 = CARTESIAN_POINT ( 'NONE',  ( -15.23376569592200092, 1422.124418483453837, 227.7537583617639996 ) ) ;
#83604 = CARTESIAN_POINT ( 'NONE',  ( 10.25492199526250126, 1479.646048717419944, 206.2690387796579898 ) ) ;
#83605 = ORIENTED_EDGE ( 'NONE', *, *, #31181, .T. ) ;
#83606 = CARTESIAN_POINT ( 'NONE',  ( -4.163396682581677943, 1410.434738167183923, 232.1586877586055095 ) ) ;
#83607 = EDGE_CURVE ( 'NONE', #16982, #48606, #17659, .T. ) ;
#83608 = CARTESIAN_POINT ( 'NONE',  ( -9.393915101222290787, 1447.312189566800043, 190.7225392970269979 ) ) ;
#83609 = CARTESIAN_POINT ( 'NONE',  ( -13.59063756412279922, 1508.278172206230010, 209.6547395369879894 ) ) ;
#83610 = CARTESIAN_POINT ( 'NONE',  ( -13.97985296196779892, 1420.196174965909904, 195.9955836505269815 ) ) ;
#83612 = CARTESIAN_POINT ( 'NONE',  ( -15.28532365586499964, 1514.287526756679881, 194.0255556049669963 ) ) ;
#83611 = CARTESIAN_POINT ( 'NONE',  ( 21.83550407203906119, 1523.678648413191468, 183.2743720722706655 ) ) ;
#83613 = CARTESIAN_POINT ( 'NONE',  ( 17.44950774654776282, 1525.163527997520305, 237.2402625269670580 ) ) ;
#83614 = CARTESIAN_POINT ( 'NONE',  ( -6.805045110652309326, 1517.051704409849890, 205.2482747741559876 ) ) ;
#83615 = CARTESIAN_POINT ( 'NONE',  ( 40.16554548739999575, 1445.100731327120002, 136.9467556218980064 ) ) ;
#83616 = ADVANCED_FACE ( 'NONE', ( #96200 ), #925, .T. ) ;
#83617 = CARTESIAN_POINT ( 'NONE',  ( -0.03232799881073839671, 1407.837594165210248, 222.3069522186050051 ) ) ;
#83618 = CARTESIAN_POINT ( 'NONE',  ( -1.709358701255000001, 1516.542957540330008, 202.1882582765869927 ) ) ;
#83619 = CARTESIAN_POINT ( 'NONE',  ( 0.000000000000000000, 1440.913060387330006, 134.0999999980979851 ) ) ;
#83621 = CARTESIAN_POINT ( 'NONE',  ( -5.376254996749998888E-14, 1377.913060387289988, 209.1218459616989946 ) ) ;
#83620 = AXIS2_PLACEMENT_3D ( 'NONE', #37021, #61706, #77928 ) ;
#83622 = CARTESIAN_POINT ( 'NONE',  ( 15.37702282283500033, 1512.655881406850085, 195.6173956022669813 ) ) ;
#83623 = CARTESIAN_POINT ( 'NONE',  ( -15.98597864390959700, 1420.860748498030034, 203.3503307164980072 ) ) ;
#83624 = CARTESIAN_POINT ( 'NONE',  ( -25.21612278913649874, 1380.250372108039983, 214.0628279411979804 ) ) ;
#83625 = CARTESIAN_POINT ( 'NONE',  ( 20.50777286777820052, 1509.292534432200227, 229.3763492124210188 ) ) ;
#83626 = EDGE_CURVE ( 'NONE', #9968, #78057, #57525, .T. ) ;
#83628 = ORIENTED_EDGE ( 'NONE', *, *, #86576, .T. ) ;
#83627 = CARTESIAN_POINT ( 'NONE',  ( -29.78513307010349820, 1379.623410526950011, 218.0480817708150028 ) ) ;
#83629 = ORIENTED_EDGE ( 'NONE', *, *, #76872, .T. ) ;
#83630 = CARTESIAN_POINT ( 'NONE',  ( 11.21685831077579820, 1434.247512195129957, 151.6038547891890005 ) ) ;
#83631 = CARTESIAN_POINT ( 'NONE',  ( -12.90441353309999961, 1397.988352241829944, 211.5057569300479940 ) ) ;
#83632 = CARTESIAN_POINT ( 'NONE',  ( -19.38290977210000321, 1410.951314247329947, 222.2178025500979857 ) ) ;
#83633 = ORIENTED_EDGE ( 'NONE', *, *, #83601, .F. ) ;
#83634 = CARTESIAN_POINT ( 'NONE',  ( -13.21180937474541572, 1444.695490197944309, 169.3896175514511242 ) ) ;
#83635 = CARTESIAN_POINT ( 'NONE',  ( 21.52065832966763637, 1509.707847311939531, 229.6525536875780631 ) ) ;
#83636 = CARTESIAN_POINT ( 'NONE',  ( -7.625190063675000296, 1512.177707669779920, 211.6636587291770013 ) ) ;
#83638 = CARTESIAN_POINT ( 'NONE',  ( -14.16428767310739900, 1509.316879318749898, 183.3251262769900052 ) ) ;
#83637 = CARTESIAN_POINT ( 'NONE',  ( -0.2476383817669989829, 1444.562280487289854, 199.4410856530290062 ) ) ;
#83639 = EDGE_CURVE ( 'NONE', #59940, #23656, #44560, .T. ) ;
#83640 = CARTESIAN_POINT ( 'NONE',  ( 1.016818722979999867, 1449.241593506360005, 183.5274279965980213 ) ) ;
#83641 = CARTESIAN_POINT ( 'NONE',  ( -4.385072903111329801, 1462.684657158180016, 200.4014842359929958 ) ) ;
#83642 = CARTESIAN_POINT ( 'NONE',  ( -17.06926747740000039, 1417.584731029579871, 207.6120866810690018 ) ) ;
#83643 = FILL_AREA_STYLE ('',( #74172 ) ) ;
#83645 = EDGE_CURVE ( 'NONE', #95978, #102807, #35592, .T. ) ;
#83644 = CARTESIAN_POINT ( 'NONE',  ( 10.52768771694820060, 1396.280695343850084, 212.5326781301700123 ) ) ;
#83646 = CARTESIAN_POINT ( 'NONE',  ( -1.270728281904929924, 1414.996443537369942, 226.4582996361970118 ) ) ;
#83647 = CARTESIAN_POINT ( 'NONE',  ( 11.57651590190000057, 1432.340302014539930, 151.1968537399980050 ) ) ;
#83648 = CARTESIAN_POINT ( 'NONE',  ( 7.396545043135000164, 1511.069621805459974, 202.7496783315469884 ) ) ;
#83649 = ORIENTED_EDGE ( 'NONE', *, *, #30950, .F. ) ;
#83650 = CARTESIAN_POINT ( 'NONE',  ( 13.20770753281709986, 1435.164461038139962, 150.0426743444330384 ) ) ;
#83651 = VERTEX_POINT ( 'NONE', #64831 ) ;
#83652 = EDGE_CURVE ( 'NONE', #11573, #110638, #31990, .T. ) ;
#83653 = ORIENTED_EDGE ( 'NONE', *, *, #54269, .T. ) ;
#83654 = CARTESIAN_POINT ( 'NONE',  ( -19.35158686409289786, 1497.937538563279986, 229.1472795281780179 ) ) ;
#83655 = CARTESIAN_POINT ( 'NONE',  ( -4.919574813549999703, 1465.704333999829942, 234.5361420446980105 ) ) ;
#83656 = CARTESIAN_POINT ( 'NONE',  ( -108.6472038312455339, 1388.244902418070296, 310.5484619707673346 ) ) ;
#83657 = CARTESIAN_POINT ( 'NONE',  ( 1.130607463874999885, 1516.632821972880038, 215.6700465578769865 ) ) ;
#83658 = CARTESIAN_POINT ( 'NONE',  ( -6.942420851809999682, 1472.648385638490026, 209.3924741736690009 ) ) ;
#83659 = ADVANCED_FACE ( 'NONE', ( #47458 ), #64272, .F. ) ;
#83660 = ORIENTED_EDGE ( 'NONE', *, *, #11868, .F. ) ;
#83661 = CARTESIAN_POINT ( 'NONE',  ( -11.61029339299999918, 1501.887990476489904, 208.8313362839550109 ) ) ;
#83662 = CARTESIAN_POINT ( 'NONE',  ( 2.500000000000000000, 1448.375488404329872, 162.6818385019500113 ) ) ;
#83663 = CARTESIAN_POINT ( 'NONE',  ( -11.54050778800000110, 1380.034650811800020, 207.7392432702189922 ) ) ;
#83664 = EDGE_LOOP ( 'NONE', ( #81447, #47987, #22482, #3988 ) ) ;
#83665 = CARTESIAN_POINT ( 'NONE',  ( -0.01328397755539850039, 1516.939580991450157, 205.8601936452070049 ) ) ;
#83666 = ORIENTED_EDGE ( 'NONE', *, *, #23447, .T. ) ;
#83667 = CARTESIAN_POINT ( 'NONE',  ( 3.460866170685000132, 1517.020847257979995, 209.8575449048190080 ) ) ;
#83668 = CARTESIAN_POINT ( 'NONE',  ( -20.20853920450000274, 1508.359852705729736, 228.9359805712980176 ) ) ;
#83669 = CARTESIAN_POINT ( 'NONE',  ( -9.200229741499999392, 1410.168877032430146, 188.1184974272979957 ) ) ;
#83670 = CARTESIAN_POINT ( 'NONE',  ( -0.2331131841380000014, 1408.921200879130083, 231.7611516523979844 ) ) ;
#83672 = EDGE_LOOP ( 'NONE', ( #71203, #56393, #11165, #75581 ) ) ;
#83671 = CARTESIAN_POINT ( 'NONE',  ( -0.1620860067307069718, 1416.842625005220043, 227.3681785903409889 ) ) ;
#83673 = CARTESIAN_POINT ( 'NONE',  ( 20.22892916700000043, 1427.700964219130128, 222.9554382744980217 ) ) ;
#83674 = CARTESIAN_POINT ( 'NONE',  ( 19.66678637246580053, 1519.551704408389924, 202.3500283489900085 ) ) ;
#83675 = CARTESIAN_POINT ( 'NONE',  ( -87.00440039350000632, 1383.772198133360007, 307.5612418777589596 ) ) ;
#83676 = FACE_OUTER_BOUND ( 'NONE', #73086, .T. ) ;
#83677 = AXIS2_PLACEMENT_3D ( 'NONE', #27024, #52783, #62309 ) ;
#83678 = CARTESIAN_POINT ( 'NONE',  ( 8.240145091180000492, 1408.795471539129949, 270.3822351589980144 ) ) ;
#83679 = CARTESIAN_POINT ( 'NONE',  ( 4.039897278065000208, 1516.787536375099990, 214.1203611275269907 ) ) ;
#83680 = AXIS2_PLACEMENT_3D ( 'NONE', #13069, #71398, #2526 ) ;
#83681 = CARTESIAN_POINT ( 'NONE',  ( 24.04558608239999984, 1411.114406507129843, 208.5460494714599804 ) ) ;
#83682 = EDGE_CURVE ( 'NONE', #109412, #96903, #89230, .T. ) ;
#83683 = CARTESIAN_POINT ( 'NONE',  ( 0.02057132068849890430, 1507.157206512230232, 237.3547131625103646 ) ) ;
#83684 = CARTESIAN_POINT ( 'NONE',  ( 0.7065304258729989684, 1442.384625720290160, 219.0605242788890052 ) ) ;
#83685 = CIRCLE ( 'NONE', #15714, 1.000000000000015099 ) ;
#83686 = DIRECTION ( 'NONE',  ( -5.980589973904019347E-17, 1.000000000000000000, -1.736889445713099699E-16 ) ) ;
#83687 = CARTESIAN_POINT ( 'NONE',  ( 2.300729626665000360, 1516.923170579120097, 210.8225527465970117 ) ) ;
#83689 = EDGE_CURVE ( 'NONE', #8151, #36202, #16979, .T. ) ;
#83688 = CARTESIAN_POINT ( 'NONE',  ( -21.95372433850575788, 1524.425415513989265, 233.6963910516591909 ) ) ;
#83690 = CARTESIAN_POINT ( 'NONE',  ( 17.37723644544120560, 1525.394081235439444, 181.1943427199432790 ) ) ;
#83691 = CARTESIAN_POINT ( 'NONE',  ( 0.5085445767741282319, 1408.930819155293875, 231.7415010692618296 ) ) ;
#83693 = ORIENTED_EDGE ( 'NONE', *, *, #72708, .F. ) ;
#83692 = CARTESIAN_POINT ( 'NONE',  ( -72.14102753049999706, 1388.281750947200180, 272.8737667914590475 ) ) ;
#83694 = CARTESIAN_POINT ( 'NONE',  ( -45.77496769243909824, 1385.147792078759949, 253.0719673062270090 ) ) ;
#83695 = CARTESIAN_POINT ( 'NONE',  ( 31.33756686635629762, 1523.580204110582599, 196.3415365203907186 ) ) ;
#83696 = CARTESIAN_POINT ( 'NONE',  ( -3.180365954810094209, 1370.226539215819685, 208.0370721656823321 ) ) ;
#83697 = CARTESIAN_POINT ( 'NONE',  ( -2.277036528833521700, 1495.095314405110230, 220.0578060253683361 ) ) ;
#83698 = CARTESIAN_POINT ( 'NONE',  ( 6.157268126266139951, 1484.877070555129876, 217.9975064028730287 ) ) ;
#83699 = CARTESIAN_POINT ( 'NONE',  ( -24.02706688199999974, 1444.687161772040099, 212.1394894004279763 ) ) ;
#83700 = CARTESIAN_POINT ( 'NONE',  ( 3.346707516019999940, 1443.005054410889898, 217.3642451189890323 ) ) ;
#83701 = EDGE_CURVE ( 'NONE', #81284, #24484, #30645, .T. ) ;
#83702 = B_SPLINE_CURVE_WITH_KNOTS ( 'NONE', 3,
 ( #25682, #16712, #17266, #94002, #34099, #100735, #58217, #7250, #24571, #43067, #77227, #24019, #529, #92342, #41958, #93443, #41412, #8335, #75579, #102399, #101274, #58762, #76657, #110807, #59875, #68292, #34653, #68837, #102553, #67350, #41582, #8504, #9070, #76833, #93604, #77931, #103683 ),
 .UNSPECIFIED., .F., .F.,
 ( 4, 3, 3, 3, 3, 3, 3, 3, 3, 3, 3, 3, 4 ),
 ( -12.84118046881009967, -12.56545256453010140, -11.90146324839760084, -11.19785799506759894, -10.45680950016819999, -9.662019177287570315, -8.697168689982460066, -7.747513139449250019, -6.994387148789269482, -6.090255947446629570, -5.292960030990699671, -4.586645094369940168, -3.918736331710000798 ),
 .UNSPECIFIED. ) ;
#83704 = CARTESIAN_POINT ( 'NONE',  ( -8.023175132090001327, 1384.900545175629986, 218.7875346266789904 ) ) ;
#83703 = CARTESIAN_POINT ( 'NONE',  ( 3.260378255074999565, 1516.582197289609894, 216.8321318079170226 ) ) ;
#83705 = CARTESIAN_POINT ( 'NONE',  ( -9.135900476020308858, 1449.599620636940244, 210.0844635627520063 ) ) ;
#83706 = CARTESIAN_POINT ( 'NONE',  ( 1.550651194191815074, 1515.551704408391060, 205.2291894524878728 ) ) ;
#83707 = VECTOR ( 'NONE', #63950, 1000.000000000000114 ) ;
#83708 = ORIENTED_EDGE ( 'NONE', *, *, #44618, .F. ) ;
#83709 = CARTESIAN_POINT ( 'NONE',  ( 6.940473334145000450, 1516.833525648419936, 202.5658237375970145 ) ) ;
#83710 = CARTESIAN_POINT ( 'NONE',  ( -16.22329233456500219, 1513.248517198770060, 223.4469878791670112 ) ) ;
#83711 = CARTESIAN_POINT ( 'NONE',  ( -0.2712367748239999932, 1477.407383352130182, 230.1216438035979763 ) ) ;
#83712 = CARTESIAN_POINT ( 'NONE',  ( 21.99352617080000272, 1452.352678890530115, 220.2843750103979801 ) ) ;
#83713 = SHAPE_REPRESENTATION ( 'Handle Screw', ( #21632 ), #103904 ) ;
#83714 = CARTESIAN_POINT ( 'NONE',  ( 7.556399103406818085, 1438.573724557855030, 153.9060459267900853 ) ) ;
#83715 = CARTESIAN_POINT ( 'NONE',  ( -8.392959608848258313, 1461.613719735366431, 204.2281241542300734 ) ) ;
#83716 = CARTESIAN_POINT ( 'NONE',  ( -1.693091880119999892, 1443.235800636190106, 218.9922110084989981 ) ) ;
#83717 = CARTESIAN_POINT ( 'NONE',  ( 15.57452430335069415, 1420.988626805493368, 227.6587458589921482 ) ) ;
#83718 = CARTESIAN_POINT ( 'NONE',  ( 29.18247107518470074, 1435.677098379100016, 136.0908610070169971 ) ) ;
#83719 = EDGE_CURVE ( 'NONE', #10158, #98691, #64231, .T. ) ;
#83720 = CARTESIAN_POINT ( 'NONE',  ( 8.559858904628349308, 1437.030483964089854, 207.9845584131589931 ) ) ;
#83721 = CARTESIAN_POINT ( 'NONE',  ( -21.39355008749999953, 1429.473757846430090, 219.8698122737980043 ) ) ;
#83722 = DIRECTION ( 'NONE',  ( -1.755985294532469921E-16, 1.000000000000000000, -1.338183447452831989E-16 ) ) ;
#83723 = CARTESIAN_POINT ( 'NONE',  ( -108.2398228239999867, 1388.716949575770059, 298.2120931944590438 ) ) ;
#83724 = CARTESIAN_POINT ( 'NONE',  ( -17.30756165510000244, 1415.800549802929936, 226.2855322628980161 ) ) ;
#83725 = CARTESIAN_POINT ( 'NONE',  ( -19.53786426058999481, 1511.187213306747708, 237.7197124308268030 ) ) ;
#83726 = CARTESIAN_POINT ( 'NONE',  ( -35.03237507324672606, 1457.739610860745643, 269.5320035884349750 ) ) ;
#83727 = ORIENTED_EDGE ( 'NONE', *, *, #37704, .F. ) ;
#83729 = ADVANCED_FACE ( 'NONE', ( #40144 ), #49118, .T. ) ;
#83728 = CARTESIAN_POINT ( 'NONE',  ( -7.942873757061038376, 1438.931140274130030, 205.4976076133249876 ) ) ;
#83730 = CARTESIAN_POINT ( 'NONE',  ( 8.972793222467396745, 1506.569407720433446, 188.9290252029455246 ) ) ;
#83731 = AXIS2_PLACEMENT_3D ( 'NONE', #47970, #31155, #56380 ) ;
#83732 = CARTESIAN_POINT ( 'NONE',  ( -3.487586080072700323, 1508.611352721110052, 213.7999951061069908 ) ) ;
#83733 = CARTESIAN_POINT ( 'NONE',  ( -4.762729318109999888, 1475.513060387329915, 229.9230423263979901 ) ) ;
#83734 = CARTESIAN_POINT ( 'NONE',  ( -15.10152500592460711, 1451.764323980957215, 222.8996944938442937 ) ) ;
#83735 = CARTESIAN_POINT ( 'NONE',  ( -28.82461960859999905, 1509.587741801030006, 208.9199936958729893 ) ) ;
#83736 = CARTESIAN_POINT ( 'NONE',  ( -9.539087469214889481, 1439.128768127180138, 208.8797462174109967 ) ) ;
#83737 = CARTESIAN_POINT ( 'NONE',  ( 16.57584690634417157, 1524.538969332612623, 180.6844723161869979 ) ) ;
#83738 = CARTESIAN_POINT ( 'NONE',  ( -5.563644771257700405, 1416.329487563220937, 231.9365388964823467 ) ) ;
#83739 = CARTESIAN_POINT ( 'NONE',  ( -22.83007936460490583, 1450.886360539059751, 142.2906941818467317 ) ) ;
#83740 = CARTESIAN_POINT ( 'NONE',  ( 23.69434222019999936, 1435.324930578030035, 137.3226534152980207 ) ) ;
#83741 = EDGE_CURVE ( 'NONE', #5014, #104178, #97421, .T. ) ;
#83742 = CARTESIAN_POINT ( 'NONE',  ( -12.88149101045983969, 1442.882090648938174, 169.4389559976919202 ) ) ;
#83744 = EDGE_LOOP ( 'NONE', ( #52006, #59993, #86434, #63678 ) ) ;
#83743 = CARTESIAN_POINT ( 'NONE',  ( -15.10324083849999965, 1409.440477179229902, 225.7327363557979822 ) ) ;
#83745 = CARTESIAN_POINT ( 'NONE',  ( -0.1744917581095109804, 1415.933499560010205, 191.2651992481820002 ) ) ;
#83746 = EDGE_CURVE ( 'NONE', #32838, #14716, #5137, .T. ) ;
#83747 = CARTESIAN_POINT ( 'NONE',  ( -14.01398736212220086, 1379.590348564800024, 211.9184487047760115 ) ) ;
#83748 = ORIENTED_EDGE ( 'NONE', *, *, #97588, .F. ) ;
#83749 = EDGE_LOOP ( 'NONE', ( #21119, #73507 ) ) ;
#83750 = CARTESIAN_POINT ( 'NONE',  ( 18.05420922962109742, 1416.521607925270018, 208.9025094127229920 ) ) ;
#83751 = CARTESIAN_POINT ( 'NONE',  ( -20.39893125376764615, 1526.069472839381206, 233.1323736274921998 ) ) ;
#83753 = CARTESIAN_POINT ( 'NONE',  ( 1.782252617107189963, 1456.535908150360001, 219.5922471067279673 ) ) ;
#83752 = CARTESIAN_POINT ( 'NONE',  ( 2.090891989490000213, 1455.065938962190103, 218.3193683645590113 ) ) ;
#83754 = CARTESIAN_POINT ( 'NONE',  ( -2.236878054880000022, 1443.656060954389886, 218.5246926830890004 ) ) ;
#83755 = CARTESIAN_POINT ( 'NONE',  ( -11.63091869309999993, 1433.120749602059959, 151.0277071862979881 ) ) ;
#83756 = EDGE_CURVE ( 'NONE', #93856, #65412, #74844, .T. ) ;
#83757 = CARTESIAN_POINT ( 'NONE',  ( -3.424720339024999838, 1517.051704408389924, 217.6596685689069943 ) ) ;
#83758 = DIRECTION ( 'NONE',  ( 1.000000000000000000, 0.000000000000000000, 0.000000000000000000 ) ) ;
#83759 = CIRCLE ( 'NONE', #53334, 12.26364123839999998 ) ;
#83760 = CARTESIAN_POINT ( 'NONE',  ( -2.737416067801649255, 1524.382868172804365, 241.6058578387446403 ) ) ;
#83761 = CARTESIAN_POINT ( 'NONE',  ( -24.46878230119999742, 1438.129412883440182, 210.7492543162080096 ) ) ;
#83762 = CARTESIAN_POINT ( 'NONE',  ( -3.459700914049689491, 1454.194523623659961, 199.2295117871159960 ) ) ;
#83763 = CARTESIAN_POINT ( 'NONE',  ( 1.420881903539999991, 1452.418224524330071, 183.4780528254979970 ) ) ;
#83764 = AXIS2_PLACEMENT_3D ( 'NONE', #56811, #73063, #25788 ) ;
#83765 = CARTESIAN_POINT ( 'NONE',  ( 7.776966983056124327, 1363.498993241026710, 210.6218459617142003 ) ) ;
#83766 = EDGE_CURVE ( 'NONE', #66886, #18900, #28466, .T. ) ;
#83767 = CARTESIAN_POINT ( 'NONE',  ( -29.01830120112816758, 1510.037320134664242, 216.7338135098987095 ) ) ;
#83769 = ORIENTED_EDGE ( 'NONE', *, *, #50763, .T. ) ;
#83768 = CARTESIAN_POINT ( 'NONE',  ( -10.96015512746500065, 1512.830284628050094, 193.2119433744669834 ) ) ;
#83770 = ORIENTED_EDGE ( 'NONE', *, *, #46877, .F. ) ;
#83771 = CARTESIAN_POINT ( 'NONE',  ( -11.83486635870610115, 1430.212806064799906, 149.5583259460390195 ) ) ;
#83772 = AXIS2_PLACEMENT_3D ( 'NONE', #102940, #59876, #41959 ) ;
#83773 = CARTESIAN_POINT ( 'NONE',  ( -13.85617977377259891, 1502.671218317619832, 227.4591309510049939 ) ) ;
#83774 = CARTESIAN_POINT ( 'NONE',  ( -4.128050607539999639, 1471.647764304730117, 269.8667864051980132 ) ) ;
#83775 = CARTESIAN_POINT ( 'NONE',  ( 12.71038982811789886, 1507.471771741610155, 233.3404631503599944 ) ) ;
#83776 = CARTESIAN_POINT ( 'NONE',  ( -128.4815115702291735, 1331.448250124730521, 295.9827786358369508 ) ) ;
#83777 = CARTESIAN_POINT ( 'NONE',  ( 41.42720720492820163, 1445.199782766380167, 136.3775557862170160 ) ) ;
#83778 = CARTESIAN_POINT ( 'NONE',  ( 19.47227132649999959, 1453.313060387329870, 205.4425732447180053 ) ) ;
#83779 = CARTESIAN_POINT ( 'NONE',  ( -8.371033538129999840, 1384.892342672460245, 199.7750077441390033 ) ) ;
#83780 = CARTESIAN_POINT ( 'NONE',  ( 18.28970766670409986, 1431.718711396310027, 208.8872839595150026 ) ) ;
#83781 = CARTESIAN_POINT ( 'NONE',  ( 31.23437356469446868, 1518.913060387330006, 222.8968241038843701 ) ) ;
#83782 = CARTESIAN_POINT ( 'NONE',  ( 9.842969107811420315, 1365.740588703662070, 210.6218459616991936 ) ) ;
#83783 = CARTESIAN_POINT ( 'NONE',  ( -33.69037434309119305, 1416.536361657399766, 267.3739642188930361 ) ) ;
#83784 = ORIENTED_EDGE ( 'NONE', *, *, #50906, .T. ) ;
#83785 = DIRECTION ( 'NONE',  ( 0.000000000000000000, 0.000000000000000000, 1.000000000000000000 ) ) ;
#83786 = EDGE_CURVE ( 'NONE', #29284, #26062, #39088, .T. ) ;
#83787 = ORIENTED_EDGE ( 'NONE', *, *, #13053, .F. ) ;
#83788 = EDGE_LOOP ( 'NONE', ( #74991, #9401, #50076 ) ) ;
#83789 = CARTESIAN_POINT ( 'NONE',  ( -1.118903308544999975, 1517.003078582959688, 212.0031713441969998 ) ) ;
#83790 = CARTESIAN_POINT ( 'NONE',  ( 7.708815788408339920, 1516.526058372639909, 206.7773338513199803 ) ) ;
#83791 = CARTESIAN_POINT ( 'NONE',  ( 7.234729710160780591, 1424.755084673710144, 194.1035305753040348 ) ) ;
#83792 = EDGE_CURVE ( 'NONE', #84504, #27375, #108887, .T. ) ;
#83794 = DIRECTION ( 'NONE',  ( -0.000000000000000000, -1.000000000000000000, -0.000000000000000000 ) ) ;
#83793 = CARTESIAN_POINT ( 'NONE',  ( 7.723480079395000253, 1517.086065052259983, 213.1573821953169841 ) ) ;
#83795 = CARTESIAN_POINT ( 'NONE',  ( -17.83707058670000123, 1485.487226716729992, 188.7688766075980027 ) ) ;
#83796 = CARTESIAN_POINT ( 'NONE',  ( -16.79675064196879930, 1489.050962929880143, 229.2737794733750150 ) ) ;
#83797 = ORIENTED_EDGE ( 'NONE', *, *, #92251, .T. ) ;
#83798 = CARTESIAN_POINT ( 'NONE',  ( -101.8495347479999964, 1379.485289779529921, 303.2301490391590164 ) ) ;
#83799 = CARTESIAN_POINT ( 'NONE',  ( -3.262264688434999726, 1516.633288330999903, 202.5742890007669814 ) ) ;
#83800 = CARTESIAN_POINT ( 'NONE',  ( -0.8539859765994225471, 1391.413060387289988, 209.6421419849122572 ) ) ;
#83801 = CARTESIAN_POINT ( 'NONE',  ( -33.28386102025609716, 1384.564240416580105, 207.5449807085249745 ) ) ;
#83802 = DIRECTION ( 'NONE',  ( 1.000000000000000000, 0.000000000000000000, 0.000000000000000000 ) ) ;
#83803 = CARTESIAN_POINT ( 'NONE',  ( -20.02800037099130037, 1485.574564704460045, 204.1280240222589839 ) ) ;
#83805 = ORIENTED_EDGE ( 'NONE', *, *, #87461, .T. ) ;
#83804 = CARTESIAN_POINT ( 'NONE',  ( -19.63722818156799832, 1519.551704408389924, 200.0074286628000095 ) ) ;
#83806 = ORIENTED_EDGE ( 'NONE', *, *, #100669, .T. ) ;
#83807 = FACE_OUTER_BOUND ( 'NONE', #67154, .T. ) ;
#83808 = CARTESIAN_POINT ( 'NONE',  ( 19.85917061082260560, 1471.740793072367751, 269.5234486458308538 ) ) ;
#83809 = CARTESIAN_POINT ( 'NONE',  ( -0.7718352176453070479, 1425.376890532889774, 191.1258158093919803 ) ) ;
#83810 = CARTESIAN_POINT ( 'NONE',  ( -12.90095066418269987, 1435.961952425909885, 150.7867089012090105 ) ) ;
#83811 = CARTESIAN_POINT ( 'NONE',  ( -24.41126177309999790, 1441.219864611299954, 212.0468573069780120 ) ) ;
#83812 = CARTESIAN_POINT ( 'NONE',  ( 5.788097227154999302, 1517.099836525840146, 211.6039138304569747 ) ) ;
#83813 = CARTESIAN_POINT ( 'NONE',  ( -68.78703070794840357, 1379.747968482269926, 280.2966647601920158 ) ) ;
#83814 = DIRECTION ( 'NONE',  ( 0.000000000000000000, 2.109423746789999926E-15, -1.000000000000000000 ) ) ;
#83815 = DIRECTION ( 'NONE',  ( 0.0001174300971986191948, -0.01238049094271260857, -0.9999233518896285533 ) ) ;
#83816 = DIRECTION ( 'NONE',  ( 0.000000000000000000, 0.000000000000000000, -1.000000000000000000 ) ) ;
#83817 = CARTESIAN_POINT ( 'NONE',  ( 7.708745647785000266, 1516.523379810429788, 207.4137536659370085 ) ) ;
#83818 = ORIENTED_EDGE ( 'NONE', *, *, #5942, .T. ) ;
#83819 = CARTESIAN_POINT ( 'NONE',  ( -2.291311050504480029, 1451.952740248410009, 184.5693412410579697 ) ) ;
#83820 = CARTESIAN_POINT ( 'NONE',  ( -11.29523006607699998, 1425.738182144259781, 112.3423121099719850 ) ) ;
#83821 = CARTESIAN_POINT ( 'NONE',  ( -19.93790229973292583, 1456.566460236430203, 225.3001283633010985 ) ) ;
#83822 = ORIENTED_EDGE ( 'NONE', *, *, #94264, .F. ) ;
#83823 = FACE_OUTER_BOUND ( 'NONE', #92806, .T. ) ;
#83824 = CARTESIAN_POINT ( 'NONE',  ( -21.39772323737049931, 1509.704958956720020, 229.7894127843639751 ) ) ;
#83825 = B_SPLINE_SURFACE_WITH_KNOTS ( 'NONE', 5, 5, ( 
 ( #52312, #28188, #44453, #87559, #95398, #53981 ),
 ( #71896, #37693, #27097, #97059, #46122, #79714 ),
 ( #78597, #2473, #86435, #1343, #70238, #104345 ),
 ( #35482, #10848, #9726, #20323, #1914, #79165 ),
 ( #11941, #36051, #36590, #95946, #88114, #11404 ),
 ( #37143, #26520, #60718, #43891, #69675, #103798 ) ),
 .UNSPECIFIED., .F., .F., .F.,
 ( 6, 6 ),
 ( 6, 6 ),
 ( 5.893385646620069807, 9.819835850959931278 ),
 ( -0.0002904017899300670230, 0.5000000000000000000 ),
 .UNSPECIFIED. ) ;
#83826 = CARTESIAN_POINT ( 'NONE',  ( 2.742624438480730120, 1469.000773353729983, 234.2676976455010163 ) ) ;
#83827 = CARTESIAN_POINT ( 'NONE',  ( 16.89232299734824494, 1526.349689584397083, 183.3465833397473261 ) ) ;
#83828 = DIRECTION ( 'NONE',  ( -0.9455185755993178454, 0.000000000000000000, 0.3255681544571537578 ) ) ;
#83829 = CARTESIAN_POINT ( 'NONE',  ( 7.452983947829999956, 1488.341756661690169, 200.6284170905290125 ) ) ;
#83830 = CARTESIAN_POINT ( 'NONE',  ( 3.242220536386509977, 1430.716549863509954, 218.0395271528590229 ) ) ;
#83831 = CARTESIAN_POINT ( 'NONE',  ( 4.283856666023710069, 1440.956247486469920, 155.9231014612180104 ) ) ;
#83833 = CARTESIAN_POINT ( 'NONE',  ( -11.88064286090000010, 1433.444786854229960, 151.0525681022980109 ) ) ;
#83832 = CARTESIAN_POINT ( 'NONE',  ( 7.334328272665000092, 1517.005755693489846, 214.1256940922069987 ) ) ;
#83834 = AXIS2_PLACEMENT_3D ( 'NONE', #26751, #25631, #85537 ) ;
#83835 = CARTESIAN_POINT ( 'NONE',  ( -7.321844861203470778, 1508.611350403038159, 214.6352815287768010 ) ) ;
#83836 = CARTESIAN_POINT ( 'NONE',  ( -3.452289220704999551, 1517.069378699710114, 215.6835323934670328 ) ) ;
#83837 = ORIENTED_EDGE ( 'NONE', *, *, #49384, .T. ) ;
#83838 = CARTESIAN_POINT ( 'NONE',  ( -12.78730321389999958, 1416.837309283630020, 195.3260687431979932 ) ) ;
#83839 = CARTESIAN_POINT ( 'NONE',  ( 16.05363106209999557, 1409.473654529731448, 193.0726681433975784 ) ) ;
#83840 = CIRCLE ( 'NONE', #73144, 2.500000000000002220 ) ;
#83841 = CARTESIAN_POINT ( 'NONE',  ( -17.05002540721839921, 1508.551704408389924, 212.5108514724210238 ) ) ;
#83842 = AXIS2_PLACEMENT_3D ( 'NONE', #966, #27248, #86597 ) ;
#83843 = PLANE ( 'NONE',  #44011 ) ;
#83844 = CARTESIAN_POINT ( 'NONE',  ( 2.471036798109852217, 1525.556089352344543, 176.9933267734384117 ) ) ;
#83845 = CARTESIAN_POINT ( 'NONE',  ( -2.410378730680590387, 1422.953362613660147, 191.3737400771369721 ) ) ;
#83846 = CARTESIAN_POINT ( 'NONE',  ( -11.35024028979760047, 1471.051957719560050, 207.9336051671150187 ) ) ;
#83847 = CARTESIAN_POINT ( 'NONE',  ( -7.393903476774015715, 1508.404769111208452, 219.6263016596369937 ) ) ;
#83848 = DIRECTION ( 'NONE',  ( 1.755985294532464991E-16, -1.000000000000000000, 1.338183447452830017E-16 ) ) ;
#83849 = CARTESIAN_POINT ( 'NONE',  ( 18.40645885720379837, 1425.561895475727397, 224.9115623075386452 ) ) ;
#83850 = DIRECTION ( 'NONE',  ( -5.980589973904019347E-17, 1.000000000000000000, -1.736889445713099699E-16 ) ) ;
#83851 = CARTESIAN_POINT ( 'NONE',  ( 39.36215256232259918, 1440.913060371679876, 258.3690201510549969 ) ) ;
#83853 = CARTESIAN_POINT ( 'NONE',  ( -12.98226713004480004, 1414.913060387349788, 219.9156686614909972 ) ) ;
#83852 = CARTESIAN_POINT ( 'NONE',  ( -10.03887960096509957, 1471.216923981430227, 211.3304923876179942 ) ) ;
#83854 = CARTESIAN_POINT ( 'NONE',  ( 12.81144342830000049, 1416.820969729830040, 221.9974425081979916 ) ) ;
#83855 = EDGE_LOOP ( 'NONE', ( #59217, #34995, #103777 ) ) ;
#83856 = ORIENTED_EDGE ( 'NONE', *, *, #805, .T. ) ;
#83857 = CARTESIAN_POINT ( 'NONE',  ( 16.50080780802032976, 1409.524096883290667, 193.0397102418697273 ) ) ;
#83858 = CARTESIAN_POINT ( 'NONE',  ( 4.363122647530000009, 1407.471318475729959, 146.1721969590979882 ) ) ;
#83859 = CARTESIAN_POINT ( 'NONE',  ( -0.8262471098266214176, 1416.839570617953314, 228.0322529358493853 ) ) ;
#83860 =( GEOMETRIC_REPRESENTATION_CONTEXT ( 3 ) GLOBAL_UNCERTAINTY_ASSIGNED_CONTEXT ( ( #68184 ) ) GLOBAL_UNIT_ASSIGNED_CONTEXT ( ( #2320, #20714, #12879 ) ) REPRESENTATION_CONTEXT ( 'NONE', 'WORKASPACE' ) );
#83861 = CARTESIAN_POINT ( 'NONE',  ( -12.51045652733512981, 1414.677402202029953, 206.7437175916260230 ) ) ;
#83862 = CARTESIAN_POINT ( 'NONE',  ( 12.94448954231351223, 1519.913060387329779, 232.8165751327380519 ) ) ;
#83863 = CARTESIAN_POINT ( 'NONE',  ( -31.34137657907970365, 1523.481610118011986, 221.9025654077134391 ) ) ;
#83864 = CARTESIAN_POINT ( 'NONE',  ( -67.25368799669159614, 1383.788001927330015, 291.4842415952459760 ) ) ;
#83865 = CARTESIAN_POINT ( 'NONE',  ( -13.34812806750000114, 1435.002040243610054, 194.7561373876979758 ) ) ;
#83866 = DIRECTION ( 'NONE',  ( -0.8672669759446666182, -0.000000000000000000, -0.4978433412588672557 ) ) ;
#83867 = CARTESIAN_POINT ( 'NONE',  ( 10.78559096389430039, 1490.798478570170118, 211.2342276834129962 ) ) ;
#83869 = ORIENTED_EDGE ( 'NONE', *, *, #79857, .T. ) ;
#83868 = CARTESIAN_POINT ( 'NONE',  ( 1.117082004689999852, 1456.189923892289926, 218.9231241165990127 ) ) ;
#83870 = CARTESIAN_POINT ( 'NONE',  ( -1.453934354320000066, 1450.715845829520049, 182.8043077764980069 ) ) ;
#83871 = EDGE_CURVE ( 'NONE', #100575, #49285, #66707, .T. ) ;
#83872 = CARTESIAN_POINT ( 'NONE',  ( -62.11202123059999991, 1379.179948843659986, 266.5711502991589441 ) ) ;
#83873 = EDGE_CURVE ( 'NONE', #12155, #25949, #16559, .T. ) ;
#83874 = CARTESIAN_POINT ( 'NONE',  ( 4.913312227257480735, 1508.551704408389924, 206.0253317281220120 ) ) ;
#83875 = VERTEX_POINT ( 'NONE', #32832 ) ;
#83876 = EDGE_LOOP ( 'NONE', ( #43418, #39033, #52465, #15054, #108366 ) ) ;
#83877 = CYLINDRICAL_SURFACE ( 'NONE', #9918, 0.4999999999999909517 ) ;
#83878 = CARTESIAN_POINT ( 'NONE',  ( -2.849563100782699809, 1515.551843419129909, 205.1388868728199952 ) ) ;
#83880 = FACE_OUTER_BOUND ( 'NONE', #40239, .T. ) ;
#83879 = CARTESIAN_POINT ( 'NONE',  ( 11.68639022145140061, 1416.948096802429973, 206.9947965055779946 ) ) ;
#83881 = B_SPLINE_CURVE_WITH_KNOTS ( 'NONE', 5,
 ( #57479, #15427, #6496, #32252, #66975, #109515 ),
 .UNSPECIFIED., .F., .F.,
 ( 6, 6 ),
 ( -10.10903599265445862, 0.000000000000000000 ),
 .UNSPECIFIED. ) ;
#83882 = CARTESIAN_POINT ( 'NONE',  ( -7.039396212389999796, 1462.541328984289976, 202.2656929340689942 ) ) ;
#83883 = CARTESIAN_POINT ( 'NONE',  ( -106.8601319760000052, 1381.472917120250031, 298.7909924236589632 ) ) ;
#83884 = CARTESIAN_POINT ( 'NONE',  ( 0.7784496931670009667, 1443.289378548789955, 202.9161012966990256 ) ) ;
#83885 = DIRECTION ( 'NONE',  ( -2.664535259100376091E-15, 0.000000000000000000, -1.000000000000000000 ) ) ;
#83886 = CARTESIAN_POINT ( 'NONE',  ( -16.00433963532579895, 1508.551704408389924, 213.8256925265339987 ) ) ;
#83887 = CARTESIAN_POINT ( 'NONE',  ( -0.3338142544270000234, 1475.117443318730011, 235.9516215253979965 ) ) ;
#83888 = CARTESIAN_POINT ( 'NONE',  ( 18.12084340177599984, 1425.008237496925858, 225.3902487627179880 ) ) ;
#83889 = CARTESIAN_POINT ( 'NONE',  ( 4.218089546350000774, 1425.254492614629953, 185.4299342609980101 ) ) ;
#83890 = CARTESIAN_POINT ( 'NONE',  ( 5.802908049555659531, 1433.707189344080007, 202.5774238276749770 ) ) ;
#83891 = CARTESIAN_POINT ( 'NONE',  ( 11.30175581209999969, 1432.339690545260055, 151.5220148439979937 ) ) ;
#83892 = AXIS2_PLACEMENT_3D ( 'NONE', #87244, #86683, #53106 ) ;
#83893 = EDGE_CURVE ( 'NONE', #94153, #44415, #101669, .T. ) ;
#83894 = CARTESIAN_POINT ( 'NONE',  ( -3.053802859332280129, 1450.477919606039904, 184.6720589006399678 ) ) ;
#83895 = ORIENTED_EDGE ( 'NONE', *, *, #33180, .T. ) ;
#83896 = CARTESIAN_POINT ( 'NONE',  ( -0.8041763403130000043, 1426.566393376330097, 144.1938086916980239 ) ) ;
#83897 = CARTESIAN_POINT ( 'NONE',  ( 19.03816721145270208, 1457.216680265689774, 226.4213465897580022 ) ) ;
#83898 = FACE_OUTER_BOUND ( 'NONE', #45682, .T. ) ;
#83899 = VECTOR ( 'NONE', #65050, 1000.000000000000227 ) ;
#83900 = CARTESIAN_POINT ( 'NONE',  ( -2.503156170453839640E-09, 1471.497077799589988, 257.8074999948410095 ) ) ;
#83901 = LINE ( 'NONE', #41910, #33785 ) ;
#83902 = CARTESIAN_POINT ( 'NONE',  ( 1.521671328670000101, 1476.675504237689893, 198.4650445948989841 ) ) ;
#83903 = CARTESIAN_POINT ( 'NONE',  ( -105.5726867909999953, 1391.548264773439996, 305.3922420788589420 ) ) ;
#83904 = DIRECTION ( 'NONE',  ( -1.836970198721029688E-16, -1.000000000000000000, 0.000000000000000000 ) ) ;
#83905 = CARTESIAN_POINT ( 'NONE',  ( -9.328535443860001664, 1363.278783432130012, 207.6218459616989946 ) ) ;
#83906 = CARTESIAN_POINT ( 'NONE',  ( -45.88366687282530165, 1440.699494908059933, 266.4123290765789989 ) ) ;
#83907 = CARTESIAN_POINT ( 'NONE',  ( 0.9710166503239879843, 1429.611445877699907, 217.3767824417549832 ) ) ;
#83908 = CARTESIAN_POINT ( 'NONE',  ( -8.619814553459999473, 1424.664384728270079, 205.6756477520589783 ) ) ;
#83909 = CARTESIAN_POINT ( 'NONE',  ( -3.455495871984999745, 1516.939877939420057, 209.1351200182310208 ) ) ;
#83910 = B_SPLINE_CURVE_WITH_KNOTS ( 'NONE', 3,
 ( #7440, #41604, #32646, #73139, #64766, #51112, #110452, #42705, #8530, #59516, #90475, #82071, #66823, #75758, #34293, #68476, #98877, #102577, #30576, #109904, #58958, #24223, #56343, #101473, #60075, #5376, #13750, #33185, #33731, #16906, #67924, #58410, #92534, #15802, #7985, #85236, #93091, #47936, #93628, #81512, #25873, #39534, #38961, #107282, #54249, #2742, #37424, #96223, #36308, #45290, #79431, #53133, #78888, #104620, #79974, #18382, #20055, #2194, #52578, #77768, #1079, #86713, #78313, #88375, #44738, #27916, #10005, #36863, #95118, #70503, #3292, #87270, #11131, #45841, #17821, #28470, #60992, #44176, #71056, #19500, #10564, #62099, #52022, #18938, #11665, #53702, #87843, #105179, #61539, #62662, #96784, #94548, #86162, #102939, #26241, #35764, #104062 ),
 .UNSPECIFIED., .F., .F.,
 ( 4, 3, 3, 3, 3, 3, 3, 3, 3, 3, 3, 3, 3, 3, 3, 3, 3, 3, 3, 3, 3, 3, 3, 3, 3, 3, 3, 3, 3, 3, 3, 3, 4 ),
 ( 31.89279723145740064, 34.15041588771699566, 37.70401514765850237, 40.03546223828480066, 42.06456480448240143, 43.93975577359619678, 45.67355729532359732, 47.34970776216830046, 48.95441885073729793, 50.14584306709999595, 51.69408452324559988, 53.32263554308429576, 55.06445428949349719, 57.02053842314010268, 59.91870409476419468, 62.02803367172320748, 63.82160321651739565, 65.49947758280899279, 67.05801106692298674, 68.35602240260000428, 71.04588944904199366, 73.84938310448460186, 76.80220749988789919, 79.96770714888299381, 83.54395628944999430, 88.79562199458749205, 92.73437127344060116, 95.91053324874698660, 98.89661206464120369, 101.7236155873209782, 104.5506191099999853, 107.1327756825400002, 108.8243481894799913 ),
 .UNSPECIFIED. ) ;
#83911 = CARTESIAN_POINT ( 'NONE',  ( 2.605323841626010495, 1407.938395893999996, 222.1469575270010068 ) ) ;
#83912 = EDGE_CURVE ( 'NONE', #92743, #17250, #41300, .T. ) ;
#83913 = CARTESIAN_POINT ( 'NONE',  ( 2.885914701209999933, 1421.960919705029937, 112.2554183042980185 ) ) ;
#83914 = CARTESIAN_POINT ( 'NONE',  ( 7.486382904747519440, 1425.304133027429998, 212.2744240526909891 ) ) ;
#83915 = CIRCLE ( 'NONE', #21219, 0.9999999999999953371 ) ;
#83916 = CARTESIAN_POINT ( 'NONE',  ( -26.48819218400589648, 1451.824455620959952, 135.6820404289399846 ) ) ;
#83917 = ORIENTED_EDGE ( 'NONE', *, *, #42847, .F. ) ;
#83918 = CIRCLE ( 'NONE', #98229, 30.13701971169416183 ) ;
#83919 = CARTESIAN_POINT ( 'NONE',  ( 20.65399528909999916, 1428.491072936029923, 221.4883061032980152 ) ) ;
#83921 = CARTESIAN_POINT ( 'NONE',  ( -15.18091661680750093, 1512.335564144490036, 222.0139412780119983 ) ) ;
#83920 = CARTESIAN_POINT ( 'NONE',  ( 0.4810529050879999713, 1489.033618959729893, 181.7121226793979929 ) ) ;
#83922 = EDGE_CURVE ( 'NONE', #98379, #55385, #57913, .T. ) ;
#83923 = CARTESIAN_POINT ( 'NONE',  ( -2.178334822207929733, 1419.510208088270019, 185.9423002976799921 ) ) ;
#83924 = CARTESIAN_POINT ( 'NONE',  ( -20.42128912490000303, 1430.525542552929892, 211.9067694171880021 ) ) ;
#83925 = CARTESIAN_POINT ( 'NONE',  ( -1.555712611759999975, 1486.517518480790159, 220.5567381263990114 ) ) ;
#83926 = CARTESIAN_POINT ( 'NONE',  ( -14.28944682607799876, 1452.414061908529902, 148.3378489825130089 ) ) ;
#83927 = CARTESIAN_POINT ( 'NONE',  ( -25.00976051679999657, 1436.598010167069788, 137.9330532114979917 ) ) ;
#83928 = ORIENTED_EDGE ( 'NONE', *, *, #94463, .F. ) ;
#83929 = CARTESIAN_POINT ( 'NONE',  ( 12.17073519972539941, 1499.730396604210000, 205.6506567772970016 ) ) ;
#83930 = CARTESIAN_POINT ( 'NONE',  ( 13.27836209250000010, 1419.795885124230153, 228.8595217210979911 ) ) ;
#83931 = CARTESIAN_POINT ( 'NONE',  ( 10.86917929760000057, 1461.683381044490034, 210.6457789368390081 ) ) ;
#83932 = VERTEX_POINT ( 'NONE', #86006 ) ;
#83933 = ORIENTED_EDGE ( 'NONE', *, *, #32289, .F. ) ;
#83934 = B_SPLINE_CURVE_WITH_KNOTS ( 'NONE', 3,
 ( #75371, #42298, #58014, #76450, #7589, #59667, #75903, #59124, #49614, #93245, #40643, #92150, #109510, #33887, #42861, #68083, #8679, #31684, #93777, #65866, #74814, #91599, #108960, #32247, #66427, #87626, #36117, #19845, #96572 ),
 .UNSPECIFIED., .F., .F.,
 ( 4, 2, 2, 2, 1, 1, 2, 2, 2, 2, 1, 1, 1, 2, 2, 2, 4 ),
 ( 0.000000000000000000, 0.2499999999998866462, 0.3749999999998336331, 0.4374999999997182809, 0.4687499999996613265, 0.4843749999996329048, 0.4921874999996959654, 0.4999999999997590261, 0.6250000000015900614, 0.6875000000025056623, 0.7187500000029128921, 0.7343750000031081804, 0.7421875000031570302, 0.7460937500031412650, 0.7500000000031254999, 0.8750000000015626389, 1.000000000000000000 ),
 .UNSPECIFIED. ) ;
#83935 = CARTESIAN_POINT ( 'NONE',  ( -79.49029774420000649, 1385.156174356060092, 282.9512253370589860 ) ) ;
#83936 = CARTESIAN_POINT ( 'NONE',  ( -23.01639577485230248, 1409.746539370839855, 209.2889146252420005 ) ) ;
#83937 = ORIENTED_EDGE ( 'NONE', *, *, #88292, .F. ) ;
#83938 = DIRECTION ( 'NONE',  ( -0.7067700363771036720, 0.03085824620770448792, -0.7067700363771036720 ) ) ;
#83939 = AXIS2_PLACEMENT_3D ( 'NONE', #84778, #26537, #84232 ) ;
#83940 = LINE ( 'NONE', #109162, #9836 ) ;
#83941 = CARTESIAN_POINT ( 'NONE',  ( -0.1201301491520000014, 1498.355800884429982, 236.9777592396980310 ) ) ;
#83942 = CARTESIAN_POINT ( 'NONE',  ( 3.273053440758749932, 1508.551704408389924, 214.1089286421269833 ) ) ;
#83943 = ORIENTED_EDGE ( 'NONE', *, *, #90708, .T. ) ;
#83944 = CARTESIAN_POINT ( 'NONE',  ( 44.80943101484369606, 1448.445176812669843, 268.7884264490030546 ) ) ;
#83945 = CARTESIAN_POINT ( 'NONE',  ( -10.25368860849440011, 1391.913060387289988, 204.2726074216130030 ) ) ;
#83946 = CARTESIAN_POINT ( 'NONE',  ( -7.544775971910000045, 1425.914422796229928, 205.6924955586589761 ) ) ;
#83947 = CARTESIAN_POINT ( 'NONE',  ( -7.723480117524999855, 1517.086065052259983, 205.0863097070169943 ) ) ;
#83948 = VERTEX_POINT ( 'NONE', #67575 ) ;
#83949 = CARTESIAN_POINT ( 'NONE',  ( 18.50997094255976450, 1458.745266264683323, 227.6095332770021287 ) ) ;
#83950 = CARTESIAN_POINT ( 'NONE',  ( 15.28055237174110026, 1513.058738973280015, 195.1605214075740093 ) ) ;
#83951 = CARTESIAN_POINT ( 'NONE',  ( 22.78697251350000030, 1409.735498424730167, 208.5774519181389905 ) ) ;
#83952 = VERTEX_POINT ( 'NONE', #24970 ) ;
#83954 = AXIS2_PLACEMENT_3D ( 'NONE', #66576, #106879, #64913 ) ;
#83953 = CARTESIAN_POINT ( 'NONE',  ( -10.47089315501180096, 1479.680542141990145, 209.9211099033080075 ) ) ;
#83955 = CARTESIAN_POINT ( 'NONE',  ( 26.86955400987890030, 1451.969623626720022, 135.0836937022390032 ) ) ;
#83956 = CARTESIAN_POINT ( 'NONE',  ( -3.136939361362319989, 1508.551704408389924, 214.0246383682069791 ) ) ;
#83957 = CARTESIAN_POINT ( 'NONE',  ( 11.45359756358510062, 1502.235480409970023, 214.6720392030410096 ) ) ;
#83958 = CARTESIAN_POINT ( 'NONE',  ( 7.393048916919999769, 1422.547170412949981, 195.6029701833990089 ) ) ;
#83959 = CARTESIAN_POINT ( 'NONE',  ( -1.155858387869529880, 1432.298546261019965, 218.5606594621140175 ) ) ;
#83960 = CARTESIAN_POINT ( 'NONE',  ( 10.50353041784589969, 1479.239315140000144, 205.9928938130530014 ) ) ;
#83961 = CARTESIAN_POINT ( 'NONE',  ( 9.679025545887689930, 1409.251059407319872, 190.1046045489409835 ) ) ;
#83963 = DIRECTION ( 'NONE',  ( 0.4794255386042027833, 0.000000000000000000, -0.8775825618903728698 ) ) ;
#83962 = CARTESIAN_POINT ( 'NONE',  ( 2.632612402369999938, 1417.642861214730146, 234.7516877880979962 ) ) ;
#83964 = CARTESIAN_POINT ( 'NONE',  ( 2.500000000000000000, 1439.615672362369878, 170.5246407131980106 ) ) ;
#83965 = CARTESIAN_POINT ( 'NONE',  ( -11.75382108840000051, 1380.709723816700034, 215.6909694682190093 ) ) ;
#83966 = CARTESIAN_POINT ( 'NONE',  ( -7.770779690674999962, 1514.639648807489948, 203.1969910678269855 ) ) ;
#83967 = ORIENTED_EDGE ( 'NONE', *, *, #48772, .F. ) ;
#83968 = CARTESIAN_POINT ( 'NONE',  ( 12.85972207402829959, 1415.932840154009909, 221.4945844118829825 ) ) ;
#83969 = CARTESIAN_POINT ( 'NONE',  ( 11.07540512644239961, 1432.346177023590144, 151.6859256421019779 ) ) ;
#83970 = CARTESIAN_POINT ( 'NONE',  ( -107.0590093890329939, 1384.929322890390040, 311.2486562067720115 ) ) ;
#83971 = B_SPLINE_SURFACE_WITH_KNOTS ( 'NONE', 5, 5, ( 
 ( #65441, #64892, #57593, #48075, #82768, #30706 ),
 ( #107963, #23940, #31260, #98999, #49187, #74943 ),
 ( #99551, #83317, #55931, #58135, #22836, #22276 ),
 ( #57041, #4951, #32371, #90050, #91716, #91167 ),
 ( #13333, #14443, #6061, #31812, #6612, #47525 ),
 ( #39093, #73270, #108520, #23404, #107410, #56478 ),
 ( #51661, #62866, #10765, #44372, #86907, #96419 ),
 ( #77956, #103135, #10197, #18031, #70702, #1262 ),
 ( #60630, #28661, #35401, #17460, #27008, #52223 ),
 ( #45490, #85799, #43806, #19697, #9097, #43262 ),
 ( #26435, #70151, #77409, #86350, #715, #1828 ),
 ( #61196, #69589, #37052, #95313, #18573, #19126 ) ),
 .UNSPECIFIED., .F., .F., .F.,
 ( 6, 3, 3, 6 ),
 ( 6, 6 ),
 ( 3.686514310900000257, 6.076675143260000134, 7.815970586829999789, 8.927001670169998349 ),
 ( 0.000000000000000000, 1.000000000000000000 ),
 .UNSPECIFIED. ) ;
#83972 = CARTESIAN_POINT ( 'NONE',  ( -12.61023785360000105, 1389.243603996410002, 203.7013712461890123 ) ) ;
#83973 = CARTESIAN_POINT ( 'NONE',  ( 11.60004869885203860, 1428.965959225140750, 137.0999999980979851 ) ) ;
#83974 = CARTESIAN_POINT ( 'NONE',  ( 11.93448652393150056, 1426.000812207319996, 202.8330995219750150 ) ) ;
#83975 = CARTESIAN_POINT ( 'NONE',  ( -10.88408651048750109, 1462.776658813379981, 207.1941354553020176 ) ) ;
#83976 = CARTESIAN_POINT ( 'NONE',  ( -5.052203703969999182, 1465.000168611230038, 255.3819207742980097 ) ) ;
#83977 = CIRCLE ( 'NONE', #73204, 0.5001123349366123350 ) ;
#83978 = CARTESIAN_POINT ( 'NONE',  ( -22.09303006097569977, 1509.609508347655265, 191.2819047646252386 ) ) ;
#83979 = CARTESIAN_POINT ( 'NONE',  ( -19.39983987835443457, 1501.977400791986611, 178.9515629539737631 ) ) ;
#83980 = CARTESIAN_POINT ( 'NONE',  ( 2.952248067976335655, 1431.436657857991577, 200.0252705656226908 ) ) ;
#83981 = B_SPLINE_SURFACE_WITH_KNOTS ( 'NONE', 5, 5, ( 
 ( #74766, #92100, #91554, #14830, #55776, #23229, #49018, #108904, #75323, #15377, #6991, #32744 ),
 ( #66924, #102142, #1363, #35505, #85905, #58514, #9748, #84246, #110556, #34403, #15918, #17006 ),
 ( #101034, #86457, #16464, #43914, #819, #25976, #277, #103235, #33842, #26547, #68033, #85335 ),
 ( #78058, #50120, #68576, #7545, #41699, #50657, #43371, #94292, #60741, #34947, #75858, #110009 ),
 ( #84788, #24332, #102679, #69132, #9211, #77519, #42807, #94863, #60174, #76968, #33285, #76402 ),
 ( #67476, #92644, #101581, #24868, #17570, #59073, #42255, #8087, #93195, #25422, #8632, #51206 ),
 ( #51770, #18137, #52334, #59615, #93728, #79736, #104365, #79189, #80824, #11964, #44475, #28768 ),
 ( #70813, #2495, #105480, #20348, #78621, #36612, #61849, #19802, #10299, #97082, #62400, #36073 ),
 ( #88686, #46149, #106034, #62970, #54552, #69699, #3045, #10872, #70258, #12516, #37171, #104926 ),
 ( #89221, #29310, #28211, #4132, #103818, #80279, #27117, #46694, #52881, #96526, #71367, #95420 ),
 ( #3594, #61301, #55093, #95968, #18683, #37718, #71919, #63509, #97627, #54006, #20895, #88138 ),
 ( #87009, #1936, #27662, #19229, #53437, #87584, #45044, #11426, #45595, #83022, #55645, #89766 ),
 ( #21976, #91967, #39919, #6314, #57304, #23097, #90863, #91430, #48338, #14152, #81351, #13586 ),
 ( #64044, #106572, #4666, #29858, #74088, #15243, #90305, #56168, #65685, #72980, #72440, #47225 ),
 ( #99803, #98161, #38805, #107118, #14705, #30960, #21434, #73539, #13037, #57840, #64597, #47772 ) ),
 .UNSPECIFIED., .F., .F., .F.,
 ( 6, 3, 3, 3, 6 ),
 ( 6, 3, 3, 6 ),
 ( 1.933639075400000129, 17.84603210599999912, 29.17820978809999843, 40.51038747020000130, 62.05803630019999417 ),
 ( -1.387778780779999841E-17, 21.09090217629999842, 42.18180435250000215, 84.36360870510000609 ),
 .UNSPECIFIED. ) ;
#83982 = CARTESIAN_POINT ( 'NONE',  ( -10.57062719580679833, 1462.108563417960113, 209.4792213203020026 ) ) ;
#83983 = CARTESIAN_POINT ( 'NONE',  ( 0.1285806494137262390, 1467.142390093758650, 235.6418487887863193 ) ) ;
#83984 = VECTOR ( 'NONE', #39699, 1000.000000000000000 ) ;
#83985 = CARTESIAN_POINT ( 'NONE',  ( -108.2312007977781150, 1388.989242186072715, 298.2560762306327433 ) ) ;
#83986 = CARTESIAN_POINT ( 'NONE',  ( 7.711490135329969853, 1466.076247724719906, 215.4504701760220087 ) ) ;
#83987 = CARTESIAN_POINT ( 'NONE',  ( -5.623474965688048840E-07, 1451.660737107639989, 154.0815186765750013 ) ) ;
#83988 = CARTESIAN_POINT ( 'NONE',  ( 4.356015308734789926, 1474.202971721140102, 219.6788459741880217 ) ) ;
#83989 = CARTESIAN_POINT ( 'NONE',  ( -17.51945758520000140, 1410.021940554830053, 225.1819460669979946 ) ) ;
#83990 = CIRCLE ( 'NONE', #89362, 1.000000000000000000 ) ;
#83991 = CARTESIAN_POINT ( 'NONE',  ( 24.03538182579999827, 1410.920334398729892, 209.8065141638319915 ) ) ;
#83992 = FACE_OUTER_BOUND ( 'NONE', #78759, .T. ) ;
#83993 = CARTESIAN_POINT ( 'NONE',  ( -76.99707197885182097, 1526.382868172863937, 19.35599459046246551 ) ) ;
#83994 = CARTESIAN_POINT ( 'NONE',  ( 1.842962231260000028, 1515.492058413689847, 204.9833025705389957 ) ) ;
#83995 = CARTESIAN_POINT ( 'NONE',  ( -2.534335827540424191, 1523.982201850120191, 175.6705872193751929 ) ) ;
#83996 = CARTESIAN_POINT ( 'NONE',  ( -8.627754931006530015, 1437.492696044950208, 228.3379672962190057 ) ) ;
#83997 = CARTESIAN_POINT ( 'NONE',  ( -6.282168602139999614, 1416.518938592030054, 226.3608756584980028 ) ) ;
#83998 = CARTESIAN_POINT ( 'NONE',  ( -18.08215423386650045, 1419.595351661949962, 206.0399610832670021 ) ) ;
#83999 = CARTESIAN_POINT ( 'NONE',  ( 0.1711675699698229913, 1479.644119743519923, 182.1096778402390157 ) ) ;
#84001 = EDGE_LOOP ( 'NONE', ( #38614, #78706, #101911 ) ) ;
#84000 = DIRECTION ( 'NONE',  ( 0.000000000000000000, 0.000000000000000000, 1.000000000000000000 ) ) ;
#84002 = CARTESIAN_POINT ( 'NONE',  ( -27.48389906189999721, 1444.324653571829913, 168.8435737885979790 ) ) ;
#84003 = DIRECTION ( 'NONE',  ( -0.000000000000000000, -1.000000000000000000, -0.000000000000000000 ) ) ;
#84004 = CARTESIAN_POINT ( 'NONE',  ( 11.87911642610000129, 1433.311711444109960, 149.6991885728979810 ) ) ;
#84005 = CARTESIAN_POINT ( 'NONE',  ( -40.60962964096870564, 1447.683802589750030, 134.0999999984229873 ) ) ;
#84006 = CARTESIAN_POINT ( 'NONE',  ( -16.93236825730539863, 1416.913057013589878, 207.4470323342559936 ) ) ;
#84007 = ORIENTED_EDGE ( 'NONE', *, *, #109177, .F. ) ;
#84008 = CARTESIAN_POINT ( 'NONE',  ( -17.44950774654834191, 1525.163527997503707, 181.0034293964202448 ) ) ;
#84009 = CARTESIAN_POINT ( 'NONE',  ( 10.02421119480000122, 1480.534221758890226, 205.8829018067289951 ) ) ;
#84010 = CARTESIAN_POINT ( 'NONE',  ( -103.7301809698822836, 1380.001629040962371, 305.5444498813670293 ) ) ;
#84011 = CARTESIAN_POINT ( 'NONE',  ( 33.35590117750199113, 1523.678648413191695, 216.3310373540456339 ) ) ;
#84012 = CARTESIAN_POINT ( 'NONE',  ( 6.692730968182499574, 1468.376655453269905, 207.5243187692509821 ) ) ;
#84013 = CARTESIAN_POINT ( 'NONE',  ( -4.283857371189049523, 1440.956241081810049, 155.9231041381889895 ) ) ;
#84014 = AXIS2_PLACEMENT_3D ( 'NONE', #9523, #77843, #29493 ) ;
#84015 = CARTESIAN_POINT ( 'NONE',  ( 11.78824854703250047, 1517.051704408389924, 211.4132493584619965 ) ) ;
#84016 = CARTESIAN_POINT ( 'NONE',  ( 7.287323794812330391, 1409.167539341809970, 222.1940209109550040 ) ) ;
#84017 = FACE_OUTER_BOUND ( 'NONE', #99377, .T. ) ;
#84018 = CARTESIAN_POINT ( 'NONE',  ( -52.55142712537259797, 1385.028519113429866, 229.4265120724080020 ) ) ;
#84019 = CARTESIAN_POINT ( 'NONE',  ( -19.33418355719779314, 1523.342713519623203, 239.2327152390762990 ) ) ;
#84020 = CARTESIAN_POINT ( 'NONE',  ( 10.99360220178390080, 1422.464694587929898, 207.9550673526719891 ) ) ;
#84021 = ORIENTED_EDGE ( 'NONE', *, *, #43794, .T. ) ;
#84022 = CARTESIAN_POINT ( 'NONE',  ( -32.07935534639999986, 1451.639962313729939, 135.6410485310980221 ) ) ;
#84023 = CARTESIAN_POINT ( 'NONE',  ( 12.93929867839850445, 1442.831169986190389, 169.4513495753705570 ) ) ;
#84024 = EDGE_CURVE ( 'NONE', #71879, #71004, #58615, .T. ) ;
#84026 = EDGE_LOOP ( 'NONE', ( #99030, #81861, #67970, #455, #12468, #66868 ) ) ;
#84025 = CARTESIAN_POINT ( 'NONE',  ( 5.456719627610000067, 1455.595244131089885, 218.2350948550090095 ) ) ;
#84027 = CARTESIAN_POINT ( 'NONE',  ( 2.642967448119999840, 1474.430884426989905, 219.8158656094990135 ) ) ;
#84028 = CARTESIAN_POINT ( 'NONE',  ( -19.42542553481155210, 1410.952741031847154, 222.1281440059015040 ) ) ;
#84029 = CARTESIAN_POINT ( 'NONE',  ( -109.6599402350000076, 1384.850943695260185, 311.3226715812589873 ) ) ;
#84030 = CARTESIAN_POINT ( 'NONE',  ( -10.94209231895430179, 1492.979988125699947, 207.3926202358989883 ) ) ;
#84031 = AXIS2_PLACEMENT_3D ( 'NONE', #64927, #47563, #66593 ) ;
#84032 = ADVANCED_FACE ( 'NONE', ( #8181 ), #23145, .T. ) ;
#84033 = CARTESIAN_POINT ( 'NONE',  ( 41.56671398617861968, 1445.561493043028804, 269.6392712540816774 ) ) ;
#84034 = FACE_OUTER_BOUND ( 'NONE', #12169, .T. ) ;
#84035 = CARTESIAN_POINT ( 'NONE',  ( -17.33360664199999945, 1423.504494455729855, 226.8663630496979806 ) ) ;
#84036 = CARTESIAN_POINT ( 'NONE',  ( 1.637935685380000006, 1417.125777826330022, 233.0400666244979959 ) ) ;
#84037 = CARTESIAN_POINT ( 'NONE',  ( 7.350381515560000523, 1447.407902261689969, 203.5674967681089811 ) ) ;
#84038 = CARTESIAN_POINT ( 'NONE',  ( -102.6162175075999556, 1366.350733876290860, 306.9753977562709224 ) ) ;
#84039 = CARTESIAN_POINT ( 'NONE',  ( 1.910127611640000132E-10, 1497.713060387329961, 230.7369720342980202 ) ) ;
#84040 = CARTESIAN_POINT ( 'NONE',  ( -3.389496885370000268, 1455.558964272489902, 200.3052646134590304 ) ) ;
#84041 = CARTESIAN_POINT ( 'NONE',  ( 5.771797426184999580, 1516.647618671360078, 206.2459958378869942 ) ) ;
#84042 = CARTESIAN_POINT ( 'NONE',  ( 3.655438681079999697, 1446.309375399810051, 170.5481836884979714 ) ) ;
#84043 = EDGE_LOOP ( 'NONE', ( #66523, #96460, #36436, #9147 ) ) ;
#84044 = CARTESIAN_POINT ( 'NONE',  ( 15.24173004819999910, 1496.337352016130126, 225.2051578755979904 ) ) ;
#84045 = CARTESIAN_POINT ( 'NONE',  ( 14.45783246989999959, 1416.839692131129823, 196.8516148386979694 ) ) ;
#84047 = ORIENTED_EDGE ( 'NONE', *, *, #85030, .T. ) ;
#84046 = CARTESIAN_POINT ( 'NONE',  ( -68.50706126879998692, 1379.747743051580073, 280.0840774303590024 ) ) ;
#84048 = CARTESIAN_POINT ( 'NONE',  ( -17.49566125220889745, 1417.678474892549957, 206.5987077655250062 ) ) ;
#84049 = ORIENTED_EDGE ( 'NONE', *, *, #109332, .F. ) ;
#84050 = CARTESIAN_POINT ( 'NONE',  ( -16.72494119730692219, 1513.190421808320480, 221.5564311681714571 ) ) ;
#84051 = CARTESIAN_POINT ( 'NONE',  ( 11.58467648010000062, 1500.424311713589987, 206.6405206915289909 ) ) ;
#84053 = CARTESIAN_POINT ( 'NONE',  ( 16.18466855446819963, 1410.575406595820141, 191.5979442498370133 ) ) ;
#84052 = CARTESIAN_POINT ( 'NONE',  ( -4.017110540329999856E-16, 1428.413060387330006, 91.31218443469779800 ) ) ;
#84054 = CARTESIAN_POINT ( 'NONE',  ( -2.864043456445000135, 1516.811292230880099, 211.4208600009669965 ) ) ;
#84055 =( BOUNDED_CURVE ( )  B_SPLINE_CURVE ( 3, ( #22391, #24053, #74506, #5635 ),
 .UNSPECIFIED., .F., .F. ) 
 B_SPLINE_CURVE_WITH_KNOTS ( ( 4, 4 ),
 ( 3.077567002946369978, 3.089415543895895233 ),
 .UNSPECIFIED. ) 
 CURVE ( )  GEOMETRIC_REPRESENTATION_ITEM ( )  RATIONAL_B_SPLINE_CURVE ( ( 1.000000000000000000, 0.9999883010406638295, 0.9999883010406638295, 1.000000000000000000 ) ) 
 REPRESENTATION_ITEM ( '' )  );
#84056 = CARTESIAN_POINT ( 'NONE',  ( 40.61087357212399951, 1439.649675151470092, 135.7177083055400146 ) ) ;
#84057 = AXIS2_PLACEMENT_3D ( 'NONE', #67447, #32713, #66895 ) ;
#84058 = B_SPLINE_SURFACE_WITH_KNOTS ( 'NONE', 5, 5, ( 
 ( #104807, #27548, #79077, #78511, #86344, #96970, #26429, #94744, #18024 ),
 ( #70696, #70143, #52217, #62283, #96413, #61730, #28653, #19689, #37045 ),
 ( #88568, #71241, #43798, #77949, #107553, #72864, #64480, #73966, #90749 ),
 ( #98042, #14028, #48219, #13469, #46575, #47114, #82358, #56613, #30840 ),
 ( #72327, #5658, #98596, #82901, #57182, #108097, #65016, #73417, #31392 ),
 ( #63927, #106457, #29740, #39806, #37601, #99134, #21316, #30288, #106999 ) ),
 .UNSPECIFIED., .F., .F., .F.,
 ( 6, 6 ),
 ( 6, 3, 6 ),
 ( 39.30566995039999512, 56.26181244329999487 ),
 ( 0.000000000000000000, 1.000000000000000000, 2.000000000000000000 ),
 .UNSPECIFIED. ) ;
#84059 = CARTESIAN_POINT ( 'NONE',  ( -6.526374435250000161, 1408.296887866830048, 262.4989398474979794 ) ) ;
#84060 = CARTESIAN_POINT ( 'NONE',  ( 2.923263220760000447, 1409.521015951630034, 231.4220154199980186 ) ) ;
#84061 = CARTESIAN_POINT ( 'NONE',  ( 12.13888692642257183, 1463.730258954271221, 231.4890017161033597 ) ) ;
#84062 = CARTESIAN_POINT ( 'NONE',  ( 14.27756146466140130, 1416.835288280145733, 196.5246214017432180 ) ) ;
#84063 = CARTESIAN_POINT ( 'NONE',  ( -38.11951386541859677, 1438.734027036600082, 136.6166153979129945 ) ) ;
#84064 = ORIENTED_EDGE ( 'NONE', *, *, #58489, .F. ) ;
#84065 = CARTESIAN_POINT ( 'NONE',  ( -22.19117979949999864, 1483.602007700189915, 216.8115292462290142 ) ) ;
#84066 = AXIS2_PLACEMENT_3D ( 'NONE', #87791, #35709, #44684 ) ;
#84067 = DIRECTION ( 'NONE',  ( -0.006061051702997927691, 0.03006260551789778981, -0.9995296410821086219 ) ) ;
#84068 = ORIENTED_EDGE ( 'NONE', *, *, #26729, .T. ) ;
#84069 = EDGE_LOOP ( 'NONE', ( #72122, #86595, #27285, #15542, #93819, #87347 ) ) ;
#84070 = CARTESIAN_POINT ( 'NONE',  ( -29.58887310228988454, 1509.966559353374123, 210.7380451519620976 ) ) ;
#84071 = CARTESIAN_POINT ( 'NONE',  ( 10.50325117827930121, 1452.939424683670040, 210.5253075612140208 ) ) ;
#84072 = CYLINDRICAL_SURFACE ( 'NONE', #34903, 2.000000000000000000 ) ;
#84073 = CARTESIAN_POINT ( 'NONE',  ( -9.318301627430487954, 1418.493606820336026, 196.8603084725207566 ) ) ;
#84074 = CIRCLE ( 'NONE', #35808, 0.9999999999999991118 ) ;
#84075 = CARTESIAN_POINT ( 'NONE',  ( 3.906031934150000051, 1515.551704408389924, 210.6104729190590206 ) ) ;
#84076 = CARTESIAN_POINT ( 'NONE',  ( -28.13477487810000000, 1508.112005706330137, 208.1343964124890249 ) ) ;
#84077 = CARTESIAN_POINT ( 'NONE',  ( 36.37832866288330536, 1435.767865547150222, 135.6938344640039986 ) ) ;
#84078 = CARTESIAN_POINT ( 'NONE',  ( 1.275439612931326350, 1516.597747112960633, 216.5200775691153865 ) ) ;
#84079 = DIRECTION ( 'NONE',  ( 1.000000000000000000, 4.676737444244369870E-15, 0.000000000000000000 ) ) ;
#84080 = CARTESIAN_POINT ( 'NONE',  ( -11.05867130699999912, 1391.913060387289988, 212.4652102573489856 ) ) ;
#84081 = CARTESIAN_POINT ( 'NONE',  ( -80.64106813425020448, 1384.797475026949996, 283.9371454116219979 ) ) ;
#84082 = ORIENTED_EDGE ( 'NONE', *, *, #32981, .T. ) ;
#84083 = CARTESIAN_POINT ( 'NONE',  ( -1.130002532395000037, 1516.621991115350056, 202.1860446705670142 ) ) ;
#84084 = CARTESIAN_POINT ( 'NONE',  ( -0.7533003905399979772, 1516.992029636990083, 208.3816250717139837 ) ) ;
#84085 = ORIENTED_EDGE ( 'NONE', *, *, #106868, .T. ) ;
#84086 = CARTESIAN_POINT ( 'NONE',  ( 11.77965714447340062, 1427.405098614149892, 147.0346648747149914 ) ) ;
#84087 = CARTESIAN_POINT ( 'NONE',  ( 4.873051833723480719, 1511.395873688979691, 217.6024705955157970 ) ) ;
#84088 = VERTEX_POINT ( 'NONE', #27211 ) ;
#84089 = CARTESIAN_POINT ( 'NONE',  ( -15.39071949251769844, 1488.664425019170039, 224.1266901275320151 ) ) ;
#84090 = CARTESIAN_POINT ( 'NONE',  ( 19.64992912941728420, 1519.551704408389924, 207.6921549202155290 ) ) ;
#84091 = CARTESIAN_POINT ( 'NONE',  ( 20.54534055259999903, 1497.714303034489831, 214.2326470396490095 ) ) ;
#84092 = CARTESIAN_POINT ( 'NONE',  ( -13.12106589760000119, 1429.130020020729944, 222.3637170071979767 ) ) ;
#84093 = DIRECTION ( 'NONE',  ( 0.000000000000000000, 0.000000000000000000, 1.000000000000000000 ) ) ;
#84094 = DIRECTION ( 'NONE',  ( 0.02616798426500960631, 0.9993150019883682011, -0.02616798426500970345 ) ) ;
#84095 = CARTESIAN_POINT ( 'NONE',  ( -16.66101146819999812, 1410.867390116229899, 191.7375337716979971 ) ) ;
#84096 = CARTESIAN_POINT ( 'NONE',  ( -50.69029307030000098, 1379.698255449190128, 241.2869840843590055 ) ) ;
#84097 = CARTESIAN_POINT ( 'NONE',  ( 25.05069432898669746, 1467.310853283639972, 206.2197278823790043 ) ) ;
#84099 = CARTESIAN_POINT ( 'NONE',  ( 4.349503564207779505, 1466.664839270300035, 198.9308445094160049 ) ) ;
#84098 = CARTESIAN_POINT ( 'NONE',  ( 14.14095063499999938, 1460.769213631630237, 232.7918287509980075 ) ) ;
#84100 = CARTESIAN_POINT ( 'NONE',  ( 0.03226293719758020068, 1410.297897419189894, 233.2219341505459909 ) ) ;
#84101 = CIRCLE ( 'NONE', #98405, 1.000000000000000888 ) ;
#84102 = B_SPLINE_SURFACE_WITH_KNOTS ( 'NONE', 5, 5, ( 
 ( #26384, #9585, #43756, #101421, #58910, #70643 ),
 ( #20187, #61682, #11803, #12338, #54385, #21265 ),
 ( #54924, #55474, #63340, #96920, #97995, #27495 ),
 ( #88518, #45972, #105311, #89600, #2878, #36445 ),
 ( #79032, #46528, #20729, #80106, #95805, #38101 ),
 ( #104760, #11268, #3425, #37556, #71757, #89052 ),
 ( #28603, #28045, #80663, #3977, #97460, #105873 ),
 ( #29154, #72279, #106411, #62235, #87415, #29695 ),
 ( #2333, #70095, #63880, #12893, #47070, #62804 ),
 ( #1774, #35912, #104208, #96361, #19072, #53276 ),
 ( #45430, #44882, #19639, #10710, #53843, #87980 ),
 ( #79574, #36997, #71189, #30795, #82853, #99636 ) ),
 .UNSPECIFIED., .F., .F., .F.,
 ( 6, 3, 3, 6 ),
 ( 6, 6 ),
 ( 12.96038195415450112, 20.44306750080000157, 27.92530488589999749, 32.63944941254549548 ),
 ( -0.0004481616454996779951, 2.000000000000000000 ),
 .UNSPECIFIED. ) ;
#84103 = CARTESIAN_POINT ( 'NONE',  ( 2.872700517194999748, 1516.559109716219837, 216.8315272385270021 ) ) ;
#84104 = ORIENTED_EDGE ( 'NONE', *, *, #36438, .T. ) ;
#84105 = CARTESIAN_POINT ( 'NONE',  ( 0.000000000000000000, 1420.119835273649869, 209.1218459616989946 ) ) ;
#84106 = CARTESIAN_POINT ( 'NONE',  ( -21.48632729253362683, 1524.478200376951236, 234.0867245257886395 ) ) ;
#84107 = CARTESIAN_POINT ( 'NONE',  ( -4.030514550714999977, 1516.901952101700090, 213.7446888144170032 ) ) ;
#84108 = CARTESIAN_POINT ( 'NONE',  ( -2.900360919557655404, 1484.442349350321592, 183.3005521221487299 ) ) ;
#84109 = CARTESIAN_POINT ( 'NONE',  ( -11.36592991815751930, 1425.607193177090494, 138.8060541407250525 ) ) ;
#84111 = EDGE_LOOP ( 'NONE', ( #73192, #61586, #24683, #21221, #94892, #87373 ) ) ;
#84110 = CARTESIAN_POINT ( 'NONE',  ( -12.04464620951310039, 1501.663624780660030, 211.4747504816580204 ) ) ;
#84112 = CARTESIAN_POINT ( 'NONE',  ( 1.114940886579999901, 1507.624369720630057, 186.1695746267980098 ) ) ;
#84113 = AXIS2_PLACEMENT_3D ( 'NONE', #2228, #11700, #104653 ) ;
#84114 = CARTESIAN_POINT ( 'NONE',  ( 0.7957076353959989801, 1507.773683908890007, 220.9213704339990159 ) ) ;
#84115 = CARTESIAN_POINT ( 'NONE',  ( -11.81020015660000055, 1428.491553152430015, 149.0224012402979668 ) ) ;
#84116 = CARTESIAN_POINT ( 'NONE',  ( -3.795106648980000053, 1436.657525481489984, 227.2555632666989993 ) ) ;
#84117 = CARTESIAN_POINT ( 'NONE',  ( -6.669163846439519538, 1441.537731776070132, 202.6633789087379967 ) ) ;
#84118 = CARTESIAN_POINT ( 'NONE',  ( -18.83642247210000065, 1444.248298674089938, 209.1218459616989946 ) ) ;
#84119 = CARTESIAN_POINT ( 'NONE',  ( -7.986570398085929057, 1425.428834413810137, 204.3462609999209860 ) ) ;
#84120 = DIRECTION ( 'NONE',  ( -1.000000000000000000, 1.836970198721029688E-16, 0.000000000000000000 ) ) ;
#84122 = CARTESIAN_POINT ( 'NONE',  ( -9.046333464132644053, 1421.595937556994159, 137.0999999980981272 ) ) ;
#84121 = CARTESIAN_POINT ( 'NONE',  ( -19.55717248739999903, 1482.733170048929878, 227.9176884791980058 ) ) ;
#84123 = CARTESIAN_POINT ( 'NONE',  ( -3.347801439296141712, 1523.382868172864164, 176.1543725841967500 ) ) ;
#84124 = ORIENTED_EDGE ( 'NONE', *, *, #15619, .T. ) ;
#84125 = CARTESIAN_POINT ( 'NONE',  ( 1.119717716265000051, 1517.038650117239968, 205.6590103047369951 ) ) ;
#84126 = CARTESIAN_POINT ( 'NONE',  ( 14.57089808959999999, 1407.761835850630177, 266.8771382033980331 ) ) ;
#84127 = CARTESIAN_POINT ( 'NONE',  ( 0.3489445596310000175, 1409.432092389130048, 185.2414967315980050 ) ) ;
#84128 = CARTESIAN_POINT ( 'NONE',  ( 19.40597849089999727, 1430.302767083830076, 194.2683597324979985 ) ) ;
#84129 = CARTESIAN_POINT ( 'NONE',  ( 7.849644149121719927, 1506.562754132946338, 229.7714992871970878 ) ) ;
#84130 = CARTESIAN_POINT ( 'NONE',  ( -8.917314821172499961, 1388.823621879021857, 217.7347579895273952 ) ) ;
#84131 = CARTESIAN_POINT ( 'NONE',  ( 11.88915038004449976, 1434.057645928349984, 147.6474571075449944 ) ) ;
#84132 = CARTESIAN_POINT ( 'NONE',  ( 13.15726445491959851, 1416.851343895820037, 196.3340833728059920 ) ) ;
#84133 = VECTOR ( 'NONE', #92911, 1000.000000000000000 ) ;
#84134 = CARTESIAN_POINT ( 'NONE',  ( -14.20524777670000027, 1416.384019283110092, 203.1488900704489993 ) ) ;
#84135 = B_SPLINE_CURVE_WITH_KNOTS ( 'NONE', 5,
 ( #85489, #31794, #40749, #33431, #8788, #25583 ),
 .UNSPECIFIED., .F., .F.,
 ( 6, 6 ),
 ( -158.0163518690000046, -29.52656374779999737 ),
 .UNSPECIFIED. ) ;
#84136 = CARTESIAN_POINT ( 'NONE',  ( -13.23918200329999983, 1446.369626751160013, 188.0966930123980205 ) ) ;
#84137 = CARTESIAN_POINT ( 'NONE',  ( -21.50121674829999918, 1519.913060387329779, 217.6081450858680171 ) ) ;
#84138 = CARTESIAN_POINT ( 'NONE',  ( -16.52203042950529976, 1419.645406836163829, 209.2874580465681902 ) ) ;
#84139 = CARTESIAN_POINT ( 'NONE',  ( -9.358593017869999642, 1499.345927103390068, 216.6356661042690064 ) ) ;
#84140 = CARTESIAN_POINT ( 'NONE',  ( -4.623067421070000016, 1470.601194648889987, 189.6761541078989808 ) ) ;
#84141 = CARTESIAN_POINT ( 'NONE',  ( -18.73855303819999918, 1441.999967869690181, 210.0191439483600107 ) ) ;
#84142 = B_SPLINE_CURVE_WITH_KNOTS ( 'NONE', 3,
 ( #62592, #37347, #96709, #11593, #94470, #17743, #9381, #55269, #106198, #55820 ),
 .UNSPECIFIED., .F., .F.,
 ( 4, 2, 2, 2, 4 ),
 ( 0.000000000000000000, 0.2500000000000000000, 0.5000000000000000000, 0.7500000000000000000, 1.000000000000000000 ),
 .UNSPECIFIED. ) ;
#84143 = CARTESIAN_POINT ( 'NONE',  ( 11.56050893731089069, 1425.527752771575024, 138.1868504500434085 ) ) ;
#84144 = DIRECTION ( 'NONE',  ( 0.9996573249755517088, 0.02617694830808744988, 0.000000000000000000 ) ) ;
#84145 = CARTESIAN_POINT ( 'NONE',  ( -21.88607058480000234, 1471.666806670330061, 268.8545562589980022 ) ) ;
#84146 = CARTESIAN_POINT ( 'NONE',  ( -22.45507226509999654, 1509.697208789830029, 190.1127326308979946 ) ) ;
#84147 = CARTESIAN_POINT ( 'NONE',  ( -11.93960757607870526, 1486.509476884231617, 184.3548908711684362 ) ) ;
#84148 = CARTESIAN_POINT ( 'NONE',  ( -42.70309239024810211, 1384.775110267059972, 247.0700973881439779 ) ) ;
#84149 = CARTESIAN_POINT ( 'NONE',  ( -106.4253901501439969, 1391.913060387279984, 303.6850724643759918 ) ) ;
#84150 = VECTOR ( 'NONE', #31044, 1000.000000000000000 ) ;
#84151 = CARTESIAN_POINT ( 'NONE',  ( 12.00789815276349870, 1415.778512723340100, 223.3240165415109857 ) ) ;
#84152 = CARTESIAN_POINT ( 'NONE',  ( -107.1236086970000088, 1379.003802515750067, 300.1442006366590363 ) ) ;
#84153 = CARTESIAN_POINT ( 'NONE',  ( -16.48231804958369651, 1525.661276915132476, 236.6690270335203934 ) ) ;
#84154 = CARTESIAN_POINT ( 'NONE',  ( -15.27152961130000008, 1506.433683729329914, 224.9338604266980326 ) ) ;
#84155 = CARTESIAN_POINT ( 'NONE',  ( -21.39776896220000069, 1411.020744638729866, 200.7714563019480067 ) ) ;
#84156 = CARTESIAN_POINT ( 'NONE',  ( -11.74116011270453441, 1378.248599687866090, 205.3698352297566032 ) ) ;
#84157 = CARTESIAN_POINT ( 'NONE',  ( -15.97682509406200069, 1420.725243137946109, 227.0315895234790275 ) ) ;
#84158 = FACE_OUTER_BOUND ( 'NONE', #90239, .T. ) ;
#84159 = CARTESIAN_POINT ( 'NONE',  ( 1.636503137890000126, 1433.447543843880112, 150.4001344053979778 ) ) ;
#84160 = CARTESIAN_POINT ( 'NONE',  ( -8.388522766530359220, 1438.665884974980145, 228.5043048793920093 ) ) ;
#84161 = CARTESIAN_POINT ( 'NONE',  ( 17.05907944273679178, 1524.678541297843367, 181.0477197495561370 ) ) ;
#84162 = CARTESIAN_POINT ( 'NONE',  ( 8.129480593693450885, 1461.711641629619862, 228.8738001905419992 ) ) ;
#84165 = CARTESIAN_POINT ( 'NONE',  ( -12.02588869021349893, 1377.660024128230134, 211.7516534935400045 ) ) ;
#84164 = AXIS2_PLACEMENT_3D ( 'NONE', #14203, #5828, #108274 ) ;
#84163 = CARTESIAN_POINT ( 'NONE',  ( 20.27427188109263412, 1522.051704408389924, 209.5053779269578342 ) ) ;
#84166 = CARTESIAN_POINT ( 'NONE',  ( 11.71263799655990034, 1426.711684079400129, 142.4234639450059774 ) ) ;
#84167 = DIRECTION ( 'NONE',  ( 0.1215789942062129869, 0.8574459172214418112, -0.5000050471826120724 ) ) ;
#84168 = CARTESIAN_POINT ( 'NONE',  ( -123.8569892973000037, 1368.558218059089995, 298.5091666678990237 ) ) ;
#84169 = CARTESIAN_POINT ( 'NONE',  ( 8.600728112939199477, 1449.621004864970018, 203.3312769315649859 ) ) ;
#84170 = CARTESIAN_POINT ( 'NONE',  ( -10.79382269979189957, 1414.913060387349788, 196.1395788316550011 ) ) ;
#84171 = CIRCLE ( 'NONE', #46655, 7.799999999999999822 ) ;
#84172 = CARTESIAN_POINT ( 'NONE',  ( -2.874588960795000148, 1516.606339319019980, 202.5748942495170013 ) ) ;
#84173 = DIRECTION ( 'NONE',  ( -0.9965178241622074662, 5.841351974388313542E-13, 0.08338001035631943669 ) ) ;
#84174 = DIRECTION ( 'NONE',  ( 9.120238070098449704E-47, -1.000000000000000000, 1.836970198721029688E-16 ) ) ;
#84176 = CARTESIAN_POINT ( 'NONE',  ( 16.23061965993500166, 1512.609537213029853, 197.8388957390669987 ) ) ;
#84175 = B_SPLINE_CURVE_WITH_KNOTS ( 'NONE', 3,
 ( #93488, #58806, #110300, #49311, #16758, #58263 ),
 .UNSPECIFIED., .F., .F.,
 ( 4, 2, 4 ),
 ( 0.000000000000000000, 0.5000000000000000000, 1.000000000000000000 ),
 .UNSPECIFIED. ) ;
#84177 = FACE_BOUND ( 'NONE', #106323, .T. ) ;
#84178 = CARTESIAN_POINT ( 'NONE',  ( 9.768019850709098135E-14, 1379.967725634990074, 211.0169302589330016 ) ) ;
#84179 = CARTESIAN_POINT ( 'NONE',  ( 21.65564397057390167, 1509.711599606019945, 229.5146149028980176 ) ) ;
#84181 = VERTEX_POINT ( 'NONE', #81873 ) ;
#84180 = CARTESIAN_POINT ( 'NONE',  ( -36.36302950906589615, 1379.637461949829913, 223.8613856847539978 ) ) ;
#84182 = ORIENTED_EDGE ( 'NONE', *, *, #55600, .F. ) ;
#84183 = CARTESIAN_POINT ( 'NONE',  ( 11.85619637978460084, 1434.445867023679966, 151.0459428651619760 ) ) ;
#84184 = CARTESIAN_POINT ( 'NONE',  ( -7.640780140759999561, 1396.708123330030048, 219.5175282754979946 ) ) ;
#84185 = ORIENTED_EDGE ( 'NONE', *, *, #33639, .F. ) ;
#84186 = CARTESIAN_POINT ( 'NONE',  ( -18.15654714260000091, 1466.352650648189865, 200.0994765531190183 ) ) ;
#84187 = CARTESIAN_POINT ( 'NONE',  ( -25.83536284099999847, 1509.142434271929915, 199.3925956580679895 ) ) ;
#84188 = DIRECTION ( 'NONE',  ( -0.9510565162951541973, 0.000000000000000000, -0.3090169943749456194 ) ) ;
#84190 = CARTESIAN_POINT ( 'NONE',  ( -13.72400085267329928, 1508.042562144249814, 184.2047245799730035 ) ) ;
#84189 = CARTESIAN_POINT ( 'NONE',  ( 0.3721991211270009869, 1444.512068895790208, 199.7834513889890218 ) ) ;
#84191 = CARTESIAN_POINT ( 'NONE',  ( 17.17241001986483795, 1512.187213306747481, 179.6185504016043240 ) ) ;
#84192 = AXIS2_PLACEMENT_3D ( 'NONE', #83043, #6336, #64065 ) ;
#84193 = B_SPLINE_CURVE_WITH_KNOTS ( 'NONE', 3,
 ( #13428, #90702, #99093, #29159, #22372, #47618, #38650, #12898, #81743, #12343 ),
 .UNSPECIFIED., .F., .F.,
 ( 4, 3, 3, 4 ),
 ( 12.29943377043420050, 12.57237910427029881, 12.96917103366740065, 13.22068347260000110 ),
 .UNSPECIFIED. ) ;
#84194 = CARTESIAN_POINT ( 'NONE',  ( 0.3227009101319999740, 1429.777580095530084, 184.2093850951980016 ) ) ;
#84195 = CARTESIAN_POINT ( 'NONE',  ( -4.291074684768139136, 1463.648453777529994, 200.1571786948010185 ) ) ;
#84196 = DIRECTION ( 'NONE',  ( -0.000000000000000000, 1.000000000000000000, -0.000000000000000000 ) ) ;
#84197 =( NAMED_UNIT ( * ) SI_UNIT ( $, .STERADIAN. ) SOLID_ANGLE_UNIT ( ) );
#84198 = DIRECTION ( 'NONE',  ( 0.000000000000000000, -1.000000000000000000, 0.000000000000000000 ) ) ;
#84199 = CARTESIAN_POINT ( 'NONE',  ( 14.43876446305509909, 1416.576002138870081, 196.8713507784850094 ) ) ;
#84200 = CARTESIAN_POINT ( 'NONE',  ( 11.76895885309999912, 1432.295726632820106, 150.8120184455979995 ) ) ;
#84201 = CARTESIAN_POINT ( 'NONE',  ( 11.74015320060000001, 1428.979986575930070, 144.1938086916980239 ) ) ;
#84202 = ORIENTED_EDGE ( 'NONE', *, *, #50162, .F. ) ;
#84203 = CARTESIAN_POINT ( 'NONE',  ( 13.19223160394649952, 1436.077184055619909, 150.6575128507280112 ) ) ;
#84204 = VERTEX_POINT ( 'NONE', #64013 ) ;
#84205 = ORIENTED_EDGE ( 'NONE', *, *, #30305, .F. ) ;
#84206 = EDGE_CURVE ( 'NONE', #68158, #23166, #51815, .T. ) ;
#84207 = LINE ( 'NONE', #25385, #1948 ) ;
#84208 = CARTESIAN_POINT ( 'NONE',  ( -12.61245242799999922, 1462.538255556929926, 230.8538998375979929 ) ) ;
#84209 = CARTESIAN_POINT ( 'NONE',  ( -19.53786426058999481, 1512.187213306747481, 236.7197124308268030 ) ) ;
#84210 = CARTESIAN_POINT ( 'NONE',  ( 4.617490466775000080, 1516.685667699390024, 216.4467608883869900 ) ) ;
#84211 = CARTESIAN_POINT ( 'NONE',  ( -8.517173909402618648, 1511.399508273092124, 214.1045348855529369 ) ) ;
#84212 = EDGE_LOOP ( 'NONE', ( #10625, #31896, #52469, #60555 ) ) ;
#84213 = CARTESIAN_POINT ( 'NONE',  ( -13.31089767809999991, 1503.456584348290107, 208.6977459381109838 ) ) ;
#84214 = CARTESIAN_POINT ( 'NONE',  ( -4.590060415194109567, 1517.051704403100075, 216.8444262830430205 ) ) ;
#84215 = CARTESIAN_POINT ( 'NONE',  ( -18.76550561599999867, 1375.296266888390164, 210.4015402955490117 ) ) ;
#84216 = ORIENTED_EDGE ( 'NONE', *, *, #73344, .F. ) ;
#84217 = CARTESIAN_POINT ( 'NONE',  ( 3.253141137235000091, 1516.858171774179937, 205.8542424163969997 ) ) ;
#84218 = ORIENTED_EDGE ( 'NONE', *, *, #49598, .F. ) ;
#84219 = CARTESIAN_POINT ( 'NONE',  ( -105.5765988122880117, 1378.244841141890220, 304.0458102224590107 ) ) ;
#84220 = CARTESIAN_POINT ( 'NONE',  ( -18.63787277240000151, 1508.244465050730014, 229.7911781032980230 ) ) ;
#84221 = CARTESIAN_POINT ( 'NONE',  ( -2.883409893379999644, 1409.181735910630096, 187.1726428837980052 ) ) ;
#84222 = CARTESIAN_POINT ( 'NONE',  ( 7.570419115124999543, 1513.830194289070278, 215.4430188042069858 ) ) ;
#84224 = ORIENTED_EDGE ( 'NONE', *, *, #33043, .F. ) ;
#84223 = CARTESIAN_POINT ( 'NONE',  ( 0.2210724871696759797, 1414.913057862230062, 225.4904853195299950 ) ) ;
#84225 = CARTESIAN_POINT ( 'NONE',  ( 18.52345746059999954, 1425.819856484229831, 224.6762942411980077 ) ) ;
#84226 = CARTESIAN_POINT ( 'NONE',  ( -9.833393186232900263, 1522.051704408389924, 212.5077547680540135 ) ) ;
#84227 = CARTESIAN_POINT ( 'NONE',  ( -113.4000000000000057, 1384.298466609749994, 311.1795487272589753 ) ) ;
#84228 = CARTESIAN_POINT ( 'NONE',  ( 6.163562822530000318, 1453.283431879389809, 216.1943447892690244 ) ) ;
#84229 = CARTESIAN_POINT ( 'NONE',  ( 13.45498908490000112, 1409.718027471030155, 270.3655313000979845 ) ) ;
#84230 = CARTESIAN_POINT ( 'NONE',  ( 6.559168636745000391, 1516.960844870249957, 214.1244393295569921 ) ) ;
#84231 = CARTESIAN_POINT ( 'NONE',  ( 23.30293074599999770, 1409.831462182929954, 209.3510310548809912 ) ) ;
#84232 = DIRECTION ( 'NONE',  ( -0.6709778558543708638, 0.000000000000000000, 0.7414773880254684757 ) ) ;
#84233 = CARTESIAN_POINT ( 'NONE',  ( 17.12862684171479799, 1428.407653715900096, 203.1217192725700045 ) ) ;
#84235 = EDGE_CURVE ( 'NONE', #108856, #58309, #42712, .T. ) ;
#84234 = CARTESIAN_POINT ( 'NONE',  ( 7.096078592938200202, 1508.610125760119899, 215.7702303952080172 ) ) ;
#84236 = CARTESIAN_POINT ( 'NONE',  ( -2.864043456445000135, 1516.811292230880099, 211.4208600009669965 ) ) ;
#84237 = ADVANCED_FACE ( 'NONE', ( #10402 ), #44572, .F. ) ;
#84238 = CARTESIAN_POINT ( 'NONE',  ( 9.404231802118440342, 1434.496204735389938, 206.4601034896920169 ) ) ;
#84239 = CARTESIAN_POINT ( 'NONE',  ( 0.000000000000000000, 1391.913060387289988, 209.1218459616989946 ) ) ;
#84240 = VECTOR ( 'NONE', #48406, 1000.000000000000000 ) ;
#84241 = DIRECTION ( 'NONE',  ( -0.4882662618185556469, -0.4884709562387110626, -0.7231819843448625829 ) ) ;
#84242 = ADVANCED_FACE ( 'NONE', ( #90270 ), #58559, .F. ) ;
#84244 = EDGE_LOOP ( 'NONE', ( #57813, #59008, #103485, #45535 ) ) ;
#84243 = CARTESIAN_POINT ( 'NONE',  ( -50.67894630349999829, 1388.315910739649780, 260.4082215553589776 ) ) ;
#84245 = CARTESIAN_POINT ( 'NONE',  ( -50.80630162021439844, 1385.117156927359929, 263.3851759514899982 ) ) ;
#84246 = CARTESIAN_POINT ( 'NONE',  ( 28.68965969039999919, 1467.163325376930061, 264.4914803740979892 ) ) ;
#84247 = EDGE_CURVE ( 'NONE', #53816, #88646, #8724, .T. ) ;
#84248 = CARTESIAN_POINT ( 'NONE',  ( -14.17232384770000131, 1420.119835273649869, 215.1506258166890007 ) ) ;
#84249 = EDGE_CURVE ( 'NONE', #37815, #46291, #99982, .T. ) ;
#84250 = CARTESIAN_POINT ( 'NONE',  ( 0.5112448275903194173, 1494.259742798005163, 220.2441603401746022 ) ) ;
#84251 = CARTESIAN_POINT ( 'NONE',  ( -5.494428884519999556, 1439.687232618090093, 154.7535770051980251 ) ) ;
#84252 = CARTESIAN_POINT ( 'NONE',  ( -4.602356253840000022, 1468.583955076089978, 189.7619545879989857 ) ) ;
#84253 = CARTESIAN_POINT ( 'NONE',  ( 1.265885663164209918, 1452.808453964450109, 183.4299257876890010 ) ) ;
#84254 = VECTOR ( 'NONE', #82074, 1000.000000000000000 ) ;
#84256 = CARTESIAN_POINT ( 'NONE',  ( -8.581120891109998539, 1384.889202694100277, 218.6696492785689827 ) ) ;
#84255 = CARTESIAN_POINT ( 'NONE',  ( 4.035490712554999249, 1516.630499592039996, 216.8333966482170183 ) ) ;
#84257 = CARTESIAN_POINT ( 'NONE',  ( -9.300631542242799199, 1448.922893710790049, 209.3136721124899964 ) ) ;
#84258 = CARTESIAN_POINT ( 'NONE',  ( -1.467768375174040179E-06, 1443.913060387330006, 126.8032257208279958 ) ) ;
#84259 = VERTEX_POINT ( 'NONE', #21942 ) ;
#84260 = CARTESIAN_POINT ( 'NONE',  ( 6.551643386774999023, 1516.807958722750072, 203.3403553877570005 ) ) ;
#84261 = CARTESIAN_POINT ( 'NONE',  ( 7.260305718849559220, 1509.032998983409925, 215.6421393903620753 ) ) ;
#84262 = CARTESIAN_POINT ( 'NONE',  ( -5.015142591918240125E-06, 1473.897713703340060, 270.2927021991790184 ) ) ;
#84263 = CARTESIAN_POINT ( 'NONE',  ( 38.60438541171740212, 1444.259423793630049, 137.1474472167479917 ) ) ;
#84264 = CARTESIAN_POINT ( 'NONE',  ( 13.15726445491959851, 1416.851343895820037, 196.3340833728059920 ) ) ;
#84265 = EDGE_CURVE ( 'NONE', #90367, #63483, #37135, .T. ) ;
#84266 = CARTESIAN_POINT ( 'NONE',  ( 4.165856372939999552, 1466.952023279489822, 218.2924068021489745 ) ) ;
#84267 = CARTESIAN_POINT ( 'NONE',  ( 10.80652762920177068, 1418.183843313859370, 229.8617425724453653 ) ) ;
#84268 = CIRCLE ( 'NONE', #59281, 1.999999905350034135 ) ;
#84269 = CARTESIAN_POINT ( 'NONE',  ( 26.79407473893059688, 1436.762045311259953, 136.7822278276699990 ) ) ;
#84270 = CARTESIAN_POINT ( 'NONE',  ( 40.26005730150239970, 1444.258505248250231, 137.0889318870590046 ) ) ;
#84271 = CARTESIAN_POINT ( 'NONE',  ( -22.47419750299999919, 1431.292034285129830, 216.7620959875980020 ) ) ;
#84272 = CARTESIAN_POINT ( 'NONE',  ( -39.37087574719232208, 1458.242454951586524, 269.1450746934871745 ) ) ;
#84273 = CARTESIAN_POINT ( 'NONE',  ( -109.8137238629999928, 1386.503517745790077, 297.1124110337590309 ) ) ;
#84274 = CARTESIAN_POINT ( 'NONE',  ( -16.70916575280000060, 1418.348764620830252, 226.8567342135980027 ) ) ;
#84275 = CARTESIAN_POINT ( 'NONE',  ( -21.45462491533616856, 1525.320849883639539, 184.8030411736961298 ) ) ;
#84276 = ADVANCED_FACE ( 'NONE', ( #32028 ), #93836, .F. ) ;
#84277 = CIRCLE ( 'NONE', #73593, 3.458500000000000352 ) ;
#84278 = CARTESIAN_POINT ( 'NONE',  ( -29.59278033692705989, 1462.546246255090409, 269.4665297251061133 ) ) ;
#84279 = ORIENTED_EDGE ( 'NONE', *, *, #2290, .F. ) ;
#84280 = CARTESIAN_POINT ( 'NONE',  ( -8.021408998099778032, 1439.374425103640078, 205.6230372236330197 ) ) ;
#84281 = CARTESIAN_POINT ( 'NONE',  ( -22.27581235781267210, 1411.016249941691967, 269.4899098767419900 ) ) ;
#84282 = ADVANCED_FACE ( 'NONE', ( #90828 ), #74049, .F. ) ;
#84283 = CARTESIAN_POINT ( 'NONE',  ( -3.487584424475879796, 1508.551704408389924, 214.1089243866350103 ) ) ;
#84284 = CARTESIAN_POINT ( 'NONE',  ( 15.81656968443809852, 1472.200743377989966, 189.2032588538999960 ) ) ;
#84285 = CARTESIAN_POINT ( 'NONE',  ( -2.305574648787668934, 1486.517880883643556, 181.6960553283176978 ) ) ;
#84286 = CARTESIAN_POINT ( 'NONE',  ( -12.80112241844660304, 1444.980343738463034, 186.0141167343691109 ) ) ;
#84287 = LINE ( 'NONE', #14315, #96823 ) ;
#84288 = DIRECTION ( 'NONE',  ( -0.8236474686100957454, 0.5669078173028199163, -0.01484500364209119690 ) ) ;
#84290 = EDGE_CURVE ( 'NONE', #16403, #50191, #71377, .T. ) ;
#84289 = TOROIDAL_SURFACE ( 'NONE', #95008, 3.500000000000000000, 0.5000000000000000000 ) ;
#84291 = CARTESIAN_POINT ( 'NONE',  ( 44.70560407356640553, 1436.310412499470203, 269.9106010176490145 ) ) ;
#84292 = CARTESIAN_POINT ( 'NONE',  ( -13.79754060518530068, 1451.192747375349654, 150.4573299455038864 ) ) ;
#84293 = CARTESIAN_POINT ( 'NONE',  ( -17.48265144437409901, 1415.426207913209964, 209.4361257033870061 ) ) ;
#84294 = CARTESIAN_POINT ( 'NONE',  ( 24.21135359159999823, 1435.361628672109873, 136.7755279798980155 ) ) ;
#84295 = CARTESIAN_POINT ( 'NONE',  ( 2.229731609205000353, 1512.142919181319940, 216.7158852195469763 ) ) ;
#84296 = ORIENTED_EDGE ( 'NONE', *, *, #69383, .F. ) ;
#84297 = CARTESIAN_POINT ( 'NONE',  ( 0.1687944357386129968, 1416.535698381769862, 190.8841062147539844 ) ) ;
#84298 = CARTESIAN_POINT ( 'NONE',  ( 6.922360974429970794E-17, 1415.677402202029953, 209.1218459616989946 ) ) ;
#84299 = ORIENTED_EDGE ( 'NONE', *, *, #67834, .T. ) ;
#84300 = VERTEX_POINT ( 'NONE', #93026 ) ;
#84301 = CARTESIAN_POINT ( 'NONE',  ( 18.04214276402350237, 1416.520646088689773, 208.7607546544149955 ) ) ;
#84302 = CARTESIAN_POINT ( 'NONE',  ( 31.44837959398592986, 1512.187213306747481, 220.9083067115976462 ) ) ;
#84304 = CARTESIAN_POINT ( 'NONE',  ( 1.320171144199999900E-07, 1461.184553862830171, 220.7697451771979900 ) ) ;
#84303 = CARTESIAN_POINT ( 'NONE',  ( 4.899054846310000322, 1455.523628246389990, 218.0750725402190255 ) ) ;
#84305 = CARTESIAN_POINT ( 'NONE',  ( -1.329478768440000014, 1444.143597569490112, 218.0942856802089977 ) ) ;
#84306 = CARTESIAN_POINT ( 'NONE',  ( -0.2155932246156589960, 1507.120203089579945, 237.3367940327759982 ) ) ;
#84307 = CARTESIAN_POINT ( 'NONE',  ( -12.30803116578610101, 1378.373984365000069, 209.8366931216010016 ) ) ;
#84308 = CARTESIAN_POINT ( 'NONE',  ( -2.874266342428972720, 1419.656144692103226, 186.1867820991938913 ) ) ;
#84309 = CARTESIAN_POINT ( 'NONE',  ( -2.792392588003544507, 1524.382868172863937, 241.3440112565233449 ) ) ;
#84310 = CARTESIAN_POINT ( 'NONE',  ( -24.20181402199999710, 1438.345721746319896, 212.1538216921279911 ) ) ;
#84311 = FACE_BOUND ( 'NONE', #95593, .T. ) ;
#84312 = CARTESIAN_POINT ( 'NONE',  ( 1.894296828289999901, 1450.413579275490065, 182.1789249826979926 ) ) ;
#84313 = MECHANICAL_DESIGN_GEOMETRIC_PRESENTATION_REPRESENTATION (  '', ( #62877 ), #66442 ) ;
#84314 = CARTESIAN_POINT ( 'NONE',  ( 8.373095552927001251, 1364.012926167303931, 210.6218459617142003 ) ) ;
#84315 = CARTESIAN_POINT ( 'NONE',  ( -26.18770677744814890, 1509.940770221357525, 223.8536542907335161 ) ) ;
#84317 = ORIENTED_EDGE ( 'NONE', *, *, #90425, .T. ) ;
#84316 = CARTESIAN_POINT ( 'NONE',  ( -3.716008649246309893E-10, 1417.166781705879885, 236.3045603347029839 ) ) ;
#84318 = ORIENTED_EDGE ( 'NONE', *, *, #35229, .T. ) ;
#84319 = CARTESIAN_POINT ( 'NONE',  ( -11.74676045389069934, 1426.724606243880089, 144.8518338750650116 ) ) ;
#84320 = DIRECTION ( 'NONE',  ( -1.836970198721029688E-16, -1.000000000000000000, 0.000000000000000000 ) ) ;
#84321 = CARTESIAN_POINT ( 'NONE',  ( -6.501109238009999736, 1473.833204323429982, 270.1283629013980203 ) ) ;
#84322 = CARTESIAN_POINT ( 'NONE',  ( -31.41104781486813735, 1512.187213306747481, 215.9140555522426723 ) ) ;
#84324 = AXIS2_PLACEMENT_3D ( 'NONE', #2862, #103071, #52155 ) ;
#84323 = CARTESIAN_POINT ( 'NONE',  ( -119.6058480740470600, 1348.229899472569514, 310.4276940313061459 ) ) ;
#84325 = CARTESIAN_POINT ( 'NONE',  ( 2.273033093151322515, 1525.821544997590763, 240.9339456143064524 ) ) ;
#84326 = CARTESIAN_POINT ( 'NONE',  ( -8.613169722380000337, 1384.571784085250101, 199.8866694092689897 ) ) ;
#84327 = DIRECTION ( 'NONE',  ( -9.153092986051941045E-47, 1.000000000000000000, -1.836970198721029688E-16 ) ) ;
#84328 = CARTESIAN_POINT ( 'NONE',  ( -16.37061378800000000, 1453.313060387329870, 197.9545095496979741 ) ) ;
#84329 = CARTESIAN_POINT ( 'NONE',  ( 9.266584390650891123, 1367.960107183285118, 207.6218459616987673 ) ) ;
#84330 = CARTESIAN_POINT ( 'NONE',  ( -8.732873948900369498, 1448.331813658970077, 211.7966235495169940 ) ) ;
#84331 = CARTESIAN_POINT ( 'NONE',  ( -6.111941472593700020, 1406.147481121090095, 267.2193986730749771 ) ) ;
#84332 = CARTESIAN_POINT ( 'NONE',  ( -13.44357912138760014, 1435.903515400679908, 150.4587087247620047 ) ) ;
#84333 = ORIENTED_EDGE ( 'NONE', *, *, #4420, .F. ) ;
#84334 = CARTESIAN_POINT ( 'NONE',  ( -12.54019733330000008, 1391.397793261360221, 209.7548870936209937 ) ) ;
#84335 = ORIENTED_EDGE ( 'NONE', *, *, #25098, .F. ) ;
#84336 = ORIENTED_EDGE ( 'NONE', *, *, #26404, .T. ) ;
#84337 = ADVANCED_FACE ( 'NONE', ( #14111 ), #15740, .T. ) ;
#84338 = VECTOR ( 'NONE', #85662, 1000.000000000000000 ) ;
#84339 = DIRECTION ( 'NONE',  ( 0.000000000000000000, 1.000000000000000000, 0.000000000000000000 ) ) ;
#84340 = CARTESIAN_POINT ( 'NONE',  ( 5.972104285402170198, 1424.417304221970198, 193.5739037265429943 ) ) ;
#84342 = DIRECTION ( 'NONE',  ( 0.000000000000000000, 1.000000000000000000, 0.000000000000000000 ) ) ;
#84341 = CARTESIAN_POINT ( 'NONE',  ( 1.134357970594999987, 1516.744381837270112, 213.1504571913470159 ) ) ;
#84343 = CARTESIAN_POINT ( 'NONE',  ( 5.399591297624999342, 1511.369014903080142, 217.1050657870570149 ) ) ;
#84344 = CARTESIAN_POINT ( 'NONE',  ( -16.50115809955429569, 1479.761560564670162, 228.9857987416320100 ) ) ;
#84345 = ORIENTED_EDGE ( 'NONE', *, *, #91691, .T. ) ;
#84346 = CARTESIAN_POINT ( 'NONE',  ( -109.5441724459999904, 1374.744572155790138, 302.6503169382589817 ) ) ;
#84347 = CARTESIAN_POINT ( 'NONE',  ( -2.487103457664999961, 1516.577434278289957, 202.5755431900869894 ) ) ;
#84348 = AXIS2_PLACEMENT_3D ( 'NONE', #93603, #94165, #43780 ) ;
#84349 = ADVANCED_FACE ( 'NONE', ( #41541 ), #83070, .T. ) ;
#84350 = CARTESIAN_POINT ( 'NONE',  ( -0.9098585486950000467, 1457.945133860129999, 229.8353278698979807 ) ) ;
#84351 = CARTESIAN_POINT ( 'NONE',  ( -41.90775481675180458, 1384.588829037659934, 214.8211095916259978 ) ) ;
#84352 = CARTESIAN_POINT ( 'NONE',  ( -6.232532119210000054, 1407.162969929730025, 197.7132727109980124 ) ) ;
#84353 = MANIFOLD_SOLID_BREP ( 'Stock-MAS-682-1', #86002 ) ;
#84354 = CARTESIAN_POINT ( 'NONE',  ( -109.0826469409999930, 1385.476187853860210, 311.2341188642590168 ) ) ;
#84356 = ORIENTED_EDGE ( 'NONE', *, *, #17976, .T. ) ;
#84355 = CARTESIAN_POINT ( 'NONE',  ( 30.61619818474186161, 1525.211477436245787, 196.6452937733279214 ) ) ;
#84357 = CARTESIAN_POINT ( 'NONE',  ( 4.124127541549999165, 1440.791920158089852, 218.1322488136489994 ) ) ;
#84358 = CARTESIAN_POINT ( 'NONE',  ( 20.38375078520000017, 1488.682100828129933, 225.5247866212980057 ) ) ;
#84359 = CARTESIAN_POINT ( 'NONE',  ( -29.36670733768233887, 1526.000688113674414, 220.9053709888523827 ) ) ;
#84360 = B_SPLINE_CURVE_WITH_KNOTS ( 'NONE', 5,
 ( #96524, #89220, #1935, #55092, #11425, #36611, #53435, #46693, #45043 ),
 .UNSPECIFIED., .F., .F.,
 ( 6, 3, 6 ),
 ( 0.000000000000000000, 0.5050532947773366255, 1.000000000000000000 ),
 .UNSPECIFIED. ) ;
#84361 = CARTESIAN_POINT ( 'NONE',  ( -1.542835357908670213, 1425.203189277900037, 191.1789319604989714 ) ) ;
#84362 = CARTESIAN_POINT ( 'NONE',  ( -25.00975368239999952, 1436.598045630599927, 137.9330133891980097 ) ) ;
#84363 = CARTESIAN_POINT ( 'NONE',  ( -24.43616090849999978, 1442.711509888459886, 211.0968183358479848 ) ) ;
#84364 = CARTESIAN_POINT ( 'NONE',  ( -3.251394400264999707, 1516.757508073510053, 210.8375504612070017 ) ) ;
#84365 = VECTOR ( 'NONE', #40741, 1000.000000000000000 ) ;
#84366 = CARTESIAN_POINT ( 'NONE',  ( -68.28255781740000430, 1379.747652651810085, 279.1103140797590072 ) ) ;
#84367 = CARTESIAN_POINT ( 'NONE',  ( 5.465008655120000114, 1438.535486872679940, 154.7353332079979964 ) ) ;
#84368 = CARTESIAN_POINT ( 'NONE',  ( -14.01548211210000083, 1415.603106624230122, 227.2686154209980032 ) ) ;
#84369 = CARTESIAN_POINT ( 'NONE',  ( 3.634203233935680899, 1440.827878596160645, 156.5853169787592094 ) ) ;
#84370 = EDGE_CURVE ( 'NONE', #65085, #86613, #78523, .T. ) ;
#84371 =( BOUNDED_CURVE ( )  B_SPLINE_CURVE ( 3, ( #32231, #92677, #34435, #49599 ),
 .UNSPECIFIED., .F., .F. ) 
 B_SPLINE_CURVE_WITH_KNOTS ( ( 4, 4 ),
 ( 4.712388980386121418, 5.974262833424425878 ),
 .UNSPECIFIED. ) 
 CURVE ( )  GEOMETRIC_REPRESENTATION_ITEM ( )  RATIONAL_B_SPLINE_CURVE ( ( 1.000000000000000000, 0.8716501122597870577, 0.8716501122597870577, 1.000000000000000000 ) ) 
 REPRESENTATION_ITEM ( '' )  );
#84372 = CARTESIAN_POINT ( 'NONE',  ( -4.626591905484999323, 1517.096587378560116, 207.4170511287669854 ) ) ;
#84373 = ORIENTED_EDGE ( 'NONE', *, *, #45523, .T. ) ;
#84374 = CARTESIAN_POINT ( 'NONE',  ( -2.028054181814160195, 1451.945093940709967, 184.4146074275660112 ) ) ;
#84375 = CARTESIAN_POINT ( 'NONE',  ( -11.43480509645590004, 1425.837052296090178, 122.9426100432909834 ) ) ;
#84376 = CONICAL_SURFACE ( 'NONE', #107643, 26.99999999999999645, 0.2186689458740001812 ) ;
#84377 = CARTESIAN_POINT ( 'NONE',  ( -19.59816656100214161, 1457.069254779966741, 225.8938671853012181 ) ) ;
#84378 = ORIENTED_EDGE ( 'NONE', *, *, #26100, .T. ) ;
#84379 = CARTESIAN_POINT ( 'NONE',  ( 20.16980298980000086, 1476.181277814190025, 211.1145665738389710 ) ) ;
#84380 = ADVANCED_FACE ( 'NONE', ( #11787 ), #42915, .T. ) ;
#84381 = CARTESIAN_POINT ( 'NONE',  ( -24.15338685722906931, 1509.761910428660258, 226.0312979713074242 ) ) ;
#84382 = CARTESIAN_POINT ( 'NONE',  ( 16.05356316396359873, 1459.304920975610003, 229.2720038708899892 ) ) ;
#84383 = CARTESIAN_POINT ( 'NONE',  ( -12.28650587490000134, 1415.606339304159974, 207.8979284120589739 ) ) ;
#84384 = CARTESIAN_POINT ( 'NONE',  ( -11.44665353847253186, 1425.798163151176823, 139.1345268192609126 ) ) ;
#84385 = CARTESIAN_POINT ( 'NONE',  ( 4.229271784049999816, 1486.647279628789875, 199.0365265047990135 ) ) ;
#84386 = CARTESIAN_POINT ( 'NONE',  ( 4.815666442453239604, 1430.144935948600050, 217.2987612619500055 ) ) ;
#84387 = CARTESIAN_POINT ( 'NONE',  ( 4.228339101480629303, 1441.548126968499901, 165.4114336615949981 ) ) ;
#84388 = EDGE_CURVE ( 'NONE', #51752, #77903, #88503, .T. ) ;
#84390 = CARTESIAN_POINT ( 'NONE',  ( 41.62259071379843078, 1442.636017130879281, 135.5651479417171004 ) ) ;
#84389 = CARTESIAN_POINT ( 'NONE',  ( 3.458526497885000328, 1516.742629295279812, 214.1194197574270106 ) ) ;
#84391 = CARTESIAN_POINT ( 'NONE',  ( 20.07643654349999807, 1508.105275064629950, 189.2153773721979917 ) ) ;
#84392 = CARTESIAN_POINT ( 'NONE',  ( -0.7391220051939990654, 1517.130100026000036, 216.0715493048870144 ) ) ;
#84393 = EDGE_LOOP ( 'NONE', ( #91706, #36828, #28169, #89282 ) ) ;
#84394 = CARTESIAN_POINT ( 'NONE',  ( 7.721597366031249798, 1517.014167129519819, 209.4083824335259862 ) ) ;
#84395 = CARTESIAN_POINT ( 'NONE',  ( -16.43158760069999857, 1420.644935630800092, 203.2808212549389850 ) ) ;
#84396 = CARTESIAN_POINT ( 'NONE',  ( 0.8420133151470000632, 1420.713779431030162, 183.4825641757979895 ) ) ;
#84397 = ADVANCED_FACE ( 'NONE', ( #80092 ), #103732, .T. ) ;
#84398 = CARTESIAN_POINT ( 'NONE',  ( 0.2114266107359989988, 1473.440120809589871, 219.3699305249989777 ) ) ;
#84399 = CARTESIAN_POINT ( 'NONE',  ( 3.317918599975760330, 1524.412928176729338, 176.3321646713325208 ) ) ;
#84400 = CARTESIAN_POINT ( 'NONE',  ( -2.795964621609999590, 1422.864594294989956, 191.4386244948990168 ) ) ;
#84401 = DIRECTION ( 'NONE',  ( 0.3463916474862910877, -0.4475252625663905248, -0.8244598024868261543 ) ) ;
#84402 = CARTESIAN_POINT ( 'NONE',  ( -6.383994317592076584, 1508.334478455586122, 219.9868654066591773 ) ) ;
#84403 = CARTESIAN_POINT ( 'NONE',  ( 17.66474287497711515, 1423.264464242703070, 226.2584317618739078 ) ) ;
#84404 = CARTESIAN_POINT ( 'NONE',  ( 18.19849895938333262, 1425.217889718911692, 224.8178544575432340 ) ) ;
#84405 = CARTESIAN_POINT ( 'NONE',  ( -11.96519809220000141, 1440.444625599219989, 147.6189886498980002 ) ) ;
#84406 = CARTESIAN_POINT ( 'NONE',  ( 26.13694933561869860, 1446.561492598689938, 138.0017900573960219 ) ) ;
#84408 = CARTESIAN_POINT ( 'NONE',  ( -4.869818399669999742, 1491.215867106689984, 188.8099941780989752 ) ) ;
#84407 = CARTESIAN_POINT ( 'NONE',  ( -6.335383617200819550, 1419.419978031070059, 194.8118966042659963 ) ) ;
#84409 = LINE ( 'NONE', #76008, #4528 ) ;
#84410 = VERTEX_POINT ( 'NONE', #45284 ) ;
#84411 = EDGE_LOOP ( 'NONE', ( #5594, #47633, #55569, #109728, #28948, #28972 ) ) ;
#84412 = CARTESIAN_POINT ( 'NONE',  ( -20.20959865099510111, 1512.187213306747481, 182.0120230947222524 ) ) ;
#84413 = ADVANCED_FACE ( 'NONE', ( #46940 ), #7096, .T. ) ;
#84414 = CARTESIAN_POINT ( 'NONE',  ( -19.57305745864531232, 1485.442696534264769, 190.1378261536969774 ) ) ;
#84415 = CIRCLE ( 'NONE', #37667, 7.500000000000000000 ) ;
#84416 = CARTESIAN_POINT ( 'NONE',  ( -27.76495496469999935, 1507.998797203929826, 210.4908169915179883 ) ) ;
#84417 = CARTESIAN_POINT ( 'NONE',  ( 2.333436892953952402, 1410.372785154803296, 185.5288099421988477 ) ) ;
#84418 = CARTESIAN_POINT ( 'NONE',  ( -12.51099982459209947, 1416.825784013739849, 222.1450729932890056 ) ) ;
#84419 = EDGE_CURVE ( 'NONE', #66359, #83109, #66069, .T. ) ;
#84420 = DIRECTION ( 'NONE',  ( -0.6205445805634668410, -0.7071067811868648745, 0.3390050494208930454 ) ) ;
#84421 = CARTESIAN_POINT ( 'NONE',  ( 3.350338079455601026, 1523.604703353109699, 242.0808062845893289 ) ) ;
#84422 = FACE_OUTER_BOUND ( 'NONE', #9759, .T. ) ;
#84423 = CARTESIAN_POINT ( 'NONE',  ( -53.93025590565110150, 1383.805580870739959, 269.3293466918710237 ) ) ;
#84424 = CARTESIAN_POINT ( 'NONE',  ( 5.164757510559999653E-11, 1452.913060387330006, 152.5211280458980241 ) ) ;
#84425 = CARTESIAN_POINT ( 'NONE',  ( 10.04089988029999958, 1469.832478305790119, 209.8601729685539965 ) ) ;
#84426 = CARTESIAN_POINT ( 'NONE',  ( 10.90104120139269916, 1491.125730471760107, 210.6098627452870176 ) ) ;
#84428 = ORIENTED_EDGE ( 'NONE', *, *, #63757, .T. ) ;
#84427 = CARTESIAN_POINT ( 'NONE',  ( 1.423783606090000209, 1455.243702336090109, 218.4445187910790196 ) ) ;
#84429 = CARTESIAN_POINT ( 'NONE',  ( -1.555023069489999799, 1450.600071333589995, 182.6247344782979951 ) ) ;
#84430 = TOROIDAL_SURFACE ( 'NONE', #64809, 32.13701971169416538, 1.000000000000000000 ) ;
#84431 = CARTESIAN_POINT ( 'NONE',  ( -51.33305125110000233, 1379.090210325960015, 243.4729415681590012 ) ) ;
#84432 = CARTESIAN_POINT ( 'NONE',  ( -17.06951414919999621, 1409.509140956229885, 223.5446133271979932 ) ) ;
#84433 = ORIENTED_EDGE ( 'NONE', *, *, #57074, .F. ) ;
#84434 = ORIENTED_EDGE ( 'NONE', *, *, #54340, .T. ) ;
#84435 = CARTESIAN_POINT ( 'NONE',  ( 16.15901746733320010, 1509.190936235299887, 232.4330185199439995 ) ) ;
#84436 = B_SPLINE_CURVE_WITH_KNOTS ( 'NONE', 3,
 ( #67620, #59769, #83299, #41303, #83847, #8227, #17156, #108501, #58115, #68187, #49165, #40743, #25575, #76001, #93890, #7146, #75476, #31787, #74919, #92248, #84402, #51348, #109609, #59225, #109069, #32883, #24474, #67074, #101179, #110153, #33424, #25022, #58662, #32351, #50272, #100634, #92798, #85481, #93341, #16069, #16607, #50804, #84934, #40193, #42393, #76548, #57572, #74375, #65978, #100101, #23381, #43517, #42961, #17714, #60317, #70396, #77122, #86058 ),
 .UNSPECIFIED., .F., .F.,
 ( 4, 2, 2, 1, 1, 1, 2, 2, 2, 1, 1, 1, 1, 2, 2, 2, 2, 2, 1, 1, 2, 2, 2, 1, 1, 1, 1, 2, 2, 2, 2, 1, 1, 1, 2, 2, 4 ),
 ( 0.000000000000000000, 0.06249999999997843392, 0.09374999999996395939, 0.1093749999999522465, 0.1171874999999481665, 0.1210937499999469452, 0.1230468749999446831, 0.1249999999999424072, 0.1874999999998670508, 0.2187499999998282207, 0.2343749999998072653, 0.2421874999997992994, 0.2460937499997886690, 0.2480468749997860878, 0.2499999999997835343, 0.3749999999996027067, 0.4374999999995103361, 0.4687499999994658162, 0.4843749999994422240, 0.4921874999994306221, 0.4960937499994216848, 0.4999999999994128030, 0.5624999999992654764, 0.5937499999991936450, 0.6093749999991554533, 0.6171874999991310284, 0.6210937499991219246, 0.6230468749991209254, 0.6249999999991199262, 0.6874999999992971178, 0.7187499999993872679, 0.7343749999994357847, 0.7421874999994599875, 0.7460937499994694244, 0.7480468749994741984, 0.7499999999994789723, 1.000000000000000000 ),
 .UNSPECIFIED. ) ;
#84437 = CARTESIAN_POINT ( 'NONE',  ( -8.659690377148740126, 1385.678185119990076, 218.6116173138180159 ) ) ;
#84438 = CARTESIAN_POINT ( 'NONE',  ( 38.50077277891229954, 1439.111704508520006, 136.6477633019350151 ) ) ;
#84440 = CYLINDRICAL_SURFACE ( 'NONE', #30556, 1.999999999999915179 ) ;
#84439 = DIRECTION ( 'NONE',  ( -5.980589973904019347E-17, 1.000000000000000000, -1.736889445713099699E-16 ) ) ;
#84441 = CARTESIAN_POINT ( 'NONE',  ( -9.400435900700001568, 1463.222323258790311, 204.0377083383889953 ) ) ;
#84442 = CARTESIAN_POINT ( 'NONE',  ( -107.7092647940000063, 1381.097588197639880, 298.6008682247589832 ) ) ;
#84443 = CARTESIAN_POINT ( 'NONE',  ( -4.161170142461470434, 1448.299083512420111, 185.1109003841999936 ) ) ;
#84444 = CARTESIAN_POINT ( 'NONE',  ( -11.14671771210699980, 1434.019356486030119, 151.6529807626459956 ) ) ;
#84445 = CARTESIAN_POINT ( 'NONE',  ( -2.195064489079999959, 1456.689498309789997, 202.6654703318990300 ) ) ;
#84446 = CARTESIAN_POINT ( 'NONE',  ( 2.678395535690000440, 1409.943584582829999, 185.6434079368980008 ) ) ;
#84447 = CARTESIAN_POINT ( 'NONE',  ( -0.5794993947522789624, 1485.974153057100011, 197.2331900926350272 ) ) ;
#84448 = CARTESIAN_POINT ( 'NONE',  ( 3.566694622846560137, 1432.299330911419929, 200.9781325985559874 ) ) ;
#84449 = LINE ( 'NONE', #84981, #96625 ) ;
#84450 = VECTOR ( 'NONE', #53302, 1000.000000000000114 ) ;
#84451 = CARTESIAN_POINT ( 'NONE',  ( -23.84529289740000380, 1452.080364410629954, 136.9869225417980090 ) ) ;
#84452 = ORIENTED_EDGE ( 'NONE', *, *, #96111, .F. ) ;
#84453 = CARTESIAN_POINT ( 'NONE',  ( -19.79636808800000125, 1468.588933445289967, 204.4688411793389946 ) ) ;
#84454 = CARTESIAN_POINT ( 'NONE',  ( 9.865354089699437168, 1509.383614495533493, 237.5628902309379669 ) ) ;
#84455 = CARTESIAN_POINT ( 'NONE',  ( 18.94792778995129723, 1457.631852883570218, 226.8423414700259855 ) ) ;
#84456 = CARTESIAN_POINT ( 'NONE',  ( 12.53380499169999851, 1445.052233488290085, 169.4755105685979970 ) ) ;
#84457 = CARTESIAN_POINT ( 'NONE',  ( 17.64503773310000057, 1507.624276183330039, 188.4842591371979950 ) ) ;
#84458 = CARTESIAN_POINT ( 'NONE',  ( -2.104209200065090229E-11, 1469.985873362830034, 253.9841755105239827 ) ) ;
#84459 = CARTESIAN_POINT ( 'NONE',  ( 18.90014522646387363, 1436.390526415187651, 146.5512626475670857 ) ) ;
#84460 = CARTESIAN_POINT ( 'NONE',  ( -1.138464810440000141, 1416.254459047329874, 228.0025200077980116 ) ) ;
#84461 = CARTESIAN_POINT ( 'NONE',  ( 0.7400002793700010129, 1477.398841704889946, 198.7251293859989971 ) ) ;
#84462 = CARTESIAN_POINT ( 'NONE',  ( -104.1918408169999992, 1389.706606718110152, 306.6384001822589767 ) ) ;
#84463 = CARTESIAN_POINT ( 'NONE',  ( -0.04336102728451687871, 1486.225514230211502, 181.8152960724703178 ) ) ;
#84464 = CARTESIAN_POINT ( 'NONE',  ( -8.622403150218080015, 1362.632156860364148, 210.6218459616991936 ) ) ;
#84465 = CARTESIAN_POINT ( 'NONE',  ( -46.03287938273930280, 1439.834097020150239, 266.6776158563489503 ) ) ;
#84466 = CARTESIAN_POINT ( 'NONE',  ( -3.604910588070000088, 1439.699991058859950, 185.4007874081979992 ) ) ;
#84467 = CARTESIAN_POINT ( 'NONE',  ( -7.737164119570000054, 1425.957155233719959, 206.5199506646890200 ) ) ;
#84468 = CARTESIAN_POINT ( 'NONE',  ( -2.292217048824999992, 1516.941178807709775, 209.1350424789999920 ) ) ;
#84469 = EDGE_CURVE ( 'NONE', #71856, #36364, #89310, .T. ) ;
#84470 = CARTESIAN_POINT ( 'NONE',  ( -4.500000000000000000, 1448.210448412289907, 183.1418046154980175 ) ) ;
#84471 = CARTESIAN_POINT ( 'NONE',  ( -33.28034951413935971, 1522.862737210649811, 200.8029765415142833 ) ) ;
#84472 = CARTESIAN_POINT ( 'NONE',  ( 7.495651997220180718, 1425.996480991439967, 212.3299467758739922 ) ) ;
#84473 = CARTESIAN_POINT ( 'NONE',  ( -25.89716630254590157, 1451.282408691979981, 136.5524683703120274 ) ) ;
#84474 = ORIENTED_EDGE ( 'NONE', *, *, #39882, .T. ) ;
#84475 = CARTESIAN_POINT ( 'NONE',  ( 12.06072352979999884, 1421.519012089930129, 225.6702541985979735 ) ) ;
#84477 = CARTESIAN_POINT ( 'NONE',  ( -16.63505975150000182, 1409.493969474430060, 194.0661809352979787 ) ) ;
#84476 = CARTESIAN_POINT ( 'NONE',  ( -11.05827631052790139, 1492.152225823860135, 207.1157292965639840 ) ) ;
#84478 = CARTESIAN_POINT ( 'NONE',  ( -19.70220409820000285, 1465.426396456590055, 207.1886372403690189 ) ) ;
#84479 = CARTESIAN_POINT ( 'NONE',  ( -16.38962540390479816, 1508.551704408489968, 213.5063151782250088 ) ) ;
#84480 = CARTESIAN_POINT ( 'NONE',  ( 8.192509002470000468, 1427.073616020289819, 211.9190997776489951 ) ) ;
#84481 = EDGE_CURVE ( 'NONE', #104691, #44473, #7054, .T. ) ;
#84482 = CARTESIAN_POINT ( 'NONE',  ( -32.02808312589930040, 1511.187213306747708, 197.2787714533499752 ) ) ;
#84483 = CARTESIAN_POINT ( 'NONE',  ( -25.91590772737680126, 1441.261220175949802, 138.4451201564890255 ) ) ;
#84484 = ORIENTED_EDGE ( 'NONE', *, *, #2389, .F. ) ;
#84485 = CARTESIAN_POINT ( 'NONE',  ( -5.000072644374990105, 1407.851873216519834, 270.1321895591700013 ) ) ;
#84486 = CARTESIAN_POINT ( 'NONE',  ( 16.67138977455960003, 1423.371517972810125, 229.1847574738629874 ) ) ;
#84487 = CARTESIAN_POINT ( 'NONE',  ( -7.512750246095000861, 1509.038615934239942, 214.6352815282469919 ) ) ;
#84488 = ORIENTED_EDGE ( 'NONE', *, *, #29894, .T. ) ;
#84489 = ORIENTED_EDGE ( 'NONE', *, *, #30425, .F. ) ;
#84490 = CARTESIAN_POINT ( 'NONE',  ( -23.30548261472260307, 1409.842060052059878, 209.3678414107039885 ) ) ;
#84491 = ORIENTED_EDGE ( 'NONE', *, *, #37919, .F. ) ;
#84492 = CARTESIAN_POINT ( 'NONE',  ( 16.87240902346729854, 1409.502257893559772, 222.1138755377239988 ) ) ;
#84493 = CARTESIAN_POINT ( 'NONE',  ( -11.74015320060000001, 1428.979986575930070, 144.1938086916980239 ) ) ;
#84494 = CARTESIAN_POINT ( 'NONE',  ( -0.6593404618510000370, 1498.354494260629963, 236.8901980696979876 ) ) ;
#84495 = CARTESIAN_POINT ( 'NONE',  ( -18.73484119289999938, 1410.876217116529915, 223.4750562042979993 ) ) ;
#84496 = CARTESIAN_POINT ( 'NONE',  ( 44.86486795881990020, 1448.468081076540102, 266.4437032002720116 ) ) ;
#84497 = CARTESIAN_POINT ( 'NONE',  ( -11.27879581752189964, 1391.913060387259975, 206.8130796129140094 ) ) ;
#84498 = CARTESIAN_POINT ( 'NONE',  ( -16.47101786845277616, 1421.300047538932859, 226.9904063017911540 ) ) ;
#84499 = CARTESIAN_POINT ( 'NONE',  ( 6.548821941055000373, 1516.688761843659904, 205.0844676760469838 ) ) ;
#84500 = ORIENTED_EDGE ( 'NONE', *, *, #11341, .F. ) ;
#84501 = CARTESIAN_POINT ( 'NONE',  ( 18.90551579537861926, 1457.715061770846432, 226.9289634256394663 ) ) ;
#84502 = CARTESIAN_POINT ( 'NONE',  ( 15.30900797519679912, 1512.850289816009990, 195.4165148025099938 ) ) ;
#84503 = FACE_OUTER_BOUND ( 'NONE', #5894, .T. ) ;
#84504 = VERTEX_POINT ( 'NONE', #39618 ) ;
#84505 = CARTESIAN_POINT ( 'NONE',  ( 2.500000000000000000, 1448.894380914000067, 182.3534011237979939 ) ) ;
#84506 = ADVANCED_FACE ( 'NONE', ( #7115 ), #77800, .F. ) ;
#84507 = CARTESIAN_POINT ( 'NONE',  ( 5.390485732382727768, 1434.547431617676921, 202.5152773920257800 ) ) ;
#84508 = CARTESIAN_POINT ( 'NONE',  ( -3.626138226838250045, 1508.551704408389924, 213.8360464113480077 ) ) ;
#84509 = CARTESIAN_POINT ( 'NONE',  ( 8.172889386072169415, 1503.933201077479907, 218.9089046230789961 ) ) ;
#84510 = ADVANCED_FACE ( 'NONE', ( #7657 ), #92020, .T. ) ;
#84511 = CARTESIAN_POINT ( 'NONE',  ( 7.468327728180000236, 1422.304606718539844, 195.6660984653989885 ) ) ;
#84512 = CARTESIAN_POINT ( 'NONE',  ( -4.115857443736018695, 1425.929640604822680, 186.1083528362279651 ) ) ;
#84513 = CARTESIAN_POINT ( 'NONE',  ( 10.09505638416009887, 1480.032748459799905, 205.9636802426639974 ) ) ;
#84514 = CARTESIAN_POINT ( 'NONE',  ( 11.77382529147789825, 1409.324211426370084, 191.4068515141649982 ) ) ;
#84516 = CARTESIAN_POINT ( 'NONE',  ( -33.28034951413935971, 1501.977400791986611, 200.8029765415142549 ) ) ;
#84515 = CARTESIAN_POINT ( 'NONE',  ( 30.30264253605709612, 1524.678541297860875, 196.4364760679688402 ) ) ;
#84517 = CARTESIAN_POINT ( 'NONE',  ( -3.487592469391230132, 1509.038615938009798, 204.6345961782960217 ) ) ;
#84518 = EDGE_CURVE ( 'NONE', #31602, #50150, #32075, .T. ) ;
#84519 = CARTESIAN_POINT ( 'NONE',  ( -13.44109269829999853, 1379.757631704399955, 212.9304593775090098 ) ) ;
#84520 = CARTESIAN_POINT ( 'NONE',  ( 15.75226268009177133, 1422.687348061682542, 229.7547754696312268 ) ) ;
#84521 = EDGE_LOOP ( 'NONE', ( #31817, #27838, #41899, #32726 ) ) ;
#84522 = CARTESIAN_POINT ( 'NONE',  ( -32.86470156657997421, 1523.580204110582372, 201.0415738463118203 ) ) ;
#84523 = CARTESIAN_POINT ( 'NONE',  ( 11.30564476295229959, 1432.342987147049826, 151.4629857478109898 ) ) ;
#84524 = CARTESIAN_POINT ( 'NONE',  ( -10.59266146615069992, 1483.275693043989804, 203.6749203483539929 ) ) ;
#84525 = EDGE_CURVE ( 'NONE', #7222, #32267, #41021, .T. ) ;
#84526 = CARTESIAN_POINT ( 'NONE',  ( -12.36341556440000033, 1392.311023796360132, 208.2952674222930227 ) ) ;
#84527 = CARTESIAN_POINT ( 'NONE',  ( 9.345988979242928707, 1422.635736885719780, 212.8844760481530045 ) ) ;
#84528 = CARTESIAN_POINT ( 'NONE',  ( 11.46771554947700089, 1425.480055491239909, 202.9414045442640031 ) ) ;
#84529 = CARTESIAN_POINT ( 'NONE',  ( -11.02103722150159903, 1462.518561201050034, 208.4069885853160145 ) ) ;
#84530 = CARTESIAN_POINT ( 'NONE',  ( -2.446787376320000096, 1432.353341358199941, 150.2884730787980061 ) ) ;
#84531 = CARTESIAN_POINT ( 'NONE',  ( -9.069281542731840062, 1383.978804767730253, 218.5605570552479833 ) ) ;
#84532 = CARTESIAN_POINT ( 'NONE',  ( 11.90340384559999976, 1433.321539026439950, 150.0592069925980070 ) ) ;
#84533 = LINE ( 'NONE', #57160, #91568 ) ;
#84534 = CARTESIAN_POINT ( 'NONE',  ( 12.70648376455249995, 1416.221314539589912, 196.3383158254220007 ) ) ;
#84535 = DIRECTION ( 'NONE',  ( 0.000000000000000000, 1.000000000000000000, 0.000000000000000000 ) ) ;
#84536 = CARTESIAN_POINT ( 'NONE',  ( 12.24079733762730093, 1421.235242715860068, 203.4476007142680203 ) ) ;
#84537 = CARTESIAN_POINT ( 'NONE',  ( 6.713874036901299469, 1465.139200243409960, 217.4101378742359998 ) ) ;
#84538 = CARTESIAN_POINT ( 'NONE',  ( -18.30666397350000096, 1486.096651966729951, 188.7550239447980118 ) ) ;
#84539 = CARTESIAN_POINT ( 'NONE',  ( 9.862951377358559313, 1519.551704408389924, 189.8497022443989977 ) ) ;
#84540 = CARTESIAN_POINT ( 'NONE',  ( -17.42058327870000056, 1410.018568801629954, 225.3436448546980273 ) ) ;
#84541 = ADVANCED_FACE ( 'NONE', ( #41814 ), #100044, .T. ) ;
#84542 = CARTESIAN_POINT ( 'NONE',  ( 23.81975463350000055, 1410.917033270829961, 210.6872995559480159 ) ) ;
#84543 = CARTESIAN_POINT ( 'NONE',  ( 3.873467265494015432, 1446.300338666319021, 170.5362326314338191 ) ) ;
#84544 = CARTESIAN_POINT ( 'NONE',  ( -35.96079425170172783, 1435.914111285932677, 135.0260409222823057 ) ) ;
#84545 = CARTESIAN_POINT ( 'NONE',  ( 9.279405586231710856, 1450.853110869679995, 207.7367179206380001 ) ) ;
#84546 = CARTESIAN_POINT ( 'NONE',  ( -2.737416067801661690, 1524.382868172804365, 176.6378340846514448 ) ) ;
#84547 = CARTESIAN_POINT ( 'NONE',  ( -9.573037427669609301, 1423.427966565790030, 192.3355729243529879 ) ) ;
#84548 = ADVANCED_FACE ( 'NONE', ( #35065 ), #96425, .T. ) ;
#84549 = CARTESIAN_POINT ( 'NONE',  ( 2.297085715815000206, 1516.718889242609976, 213.1486234561869821 ) ) ;
#84550 = CARTESIAN_POINT ( 'NONE',  ( -14.68398163311469951, 1420.764401514960127, 209.3424412080640025 ) ) ;
#84551 = CARTESIAN_POINT ( 'NONE',  ( 0.1713633400619609948, 1479.529269706499917, 182.1146112136229931 ) ) ;
#84553 = VERTEX_POINT ( 'NONE', #78169 ) ;
#84552 = CARTESIAN_POINT ( 'NONE',  ( -2.805963291598290166, 1407.650164048290208, 222.1876714739069882 ) ) ;
#84554 = CARTESIAN_POINT ( 'NONE',  ( -12.73318793669440829, 1444.994950788470533, 164.6858276811441328 ) ) ;
#84555 = PLANE ( 'NONE',  #22907 ) ;
#84556 = CARTESIAN_POINT ( 'NONE',  ( 12.91281063729999978, 1434.774390924990257, 149.8853380536980069 ) ) ;
#84557 = CARTESIAN_POINT ( 'NONE',  ( -40.02226351667210480, 1448.570981148800229, 134.0999999981999906 ) ) ;
#84558 = CARTESIAN_POINT ( 'NONE',  ( -27.74152896854549866, 1446.393007474169963, 137.1637341980870133 ) ) ;
#84559 = ORIENTED_EDGE ( 'NONE', *, *, #66484, .T. ) ;
#84560 = DIRECTION ( 'NONE',  ( -0.7071067811870476172, -8.350994019970553111E-15, 0.7071067811860475283 ) ) ;
#84561 = DIRECTION ( 'NONE',  ( 0.8775825618903763115, 0.000000000000000000, -0.4794255386041963996 ) ) ;
#84562 = CARTESIAN_POINT ( 'NONE',  ( -105.2598989700874199, 1381.083690021850998, 308.6936584762340203 ) ) ;
#84563 = CARTESIAN_POINT ( 'NONE',  ( 1.514120561980000183E-16, 1515.551704408389924, 209.1218459616989946 ) ) ;
#84564 = CARTESIAN_POINT ( 'NONE',  ( -0.5682668705760020034, 1506.801775235190007, 221.9434713837989932 ) ) ;
#84565 = CARTESIAN_POINT ( 'NONE',  ( -16.14386229810000017, 1410.940818424630152, 209.1303365420530156 ) ) ;
#84566 = LINE ( 'NONE', #108670, #20860 ) ;
#84567 = FACE_OUTER_BOUND ( 'NONE', #67886, .T. ) ;
#84568 = CARTESIAN_POINT ( 'NONE',  ( 2.990245160869999808, 1439.681522767690012, 184.2324485070979847 ) ) ;
#84569 = CARTESIAN_POINT ( 'NONE',  ( -76.07878363630570107, 1385.141112864619799, 277.2891741808400639 ) ) ;
#84570 = CARTESIAN_POINT ( 'NONE',  ( -10.82459666645259944, 1391.913060387289988, 212.9211246486700304 ) ) ;
#84571 = CARTESIAN_POINT ( 'NONE',  ( 11.08034903154059947, 1427.227500383180086, 208.8464042652539945 ) ) ;
#84572 = ORIENTED_EDGE ( 'NONE', *, *, #32610, .F. ) ;
#84573 = CARTESIAN_POINT ( 'NONE',  ( -30.93305835920000035, 1451.832845973630128, 134.8030507067980182 ) ) ;
#84574 = CARTESIAN_POINT ( 'NONE',  ( 17.22654844235838567, 1443.501467202828508, 162.9224179604370590 ) ) ;
#84576 = ORIENTED_EDGE ( 'NONE', *, *, #70826, .F. ) ;
#84575 = CARTESIAN_POINT ( 'NONE',  ( -2.157482617120746404, 1526.189899547014420, 240.2809648701897061 ) ) ;
#84577 = DIRECTION ( 'NONE',  ( 9.341989762165448955E-47, -1.000000000000000000, 1.836970198721029688E-16 ) ) ;
#84578 = CARTESIAN_POINT ( 'NONE',  ( 18.17556130014969895, 1429.975338228749933, 210.2973223115409951 ) ) ;
#84579 = CARTESIAN_POINT ( 'NONE',  ( -7.893155011514420671, 1363.585497717410817, 210.6218459617142003 ) ) ;
#84580 = CARTESIAN_POINT ( 'NONE',  ( -11.00351831549999915, 1492.170254952789946, 204.4829265568189953 ) ) ;
#84581 = CARTESIAN_POINT ( 'NONE',  ( 40.71297843928967808, 1448.600067007655298, 269.6231773872929125 ) ) ;
#84582 = DIRECTION ( 'NONE',  ( 0.1070030146457386366, 0.000000000000000000, 0.9942586961433749204 ) ) ;
#84583 = CARTESIAN_POINT ( 'NONE',  ( 19.00106994256368864, 1437.749780598343705, 213.2493778570810434 ) ) ;
#84584 = FACE_OUTER_BOUND ( 'NONE', #71732, .T. ) ;
#84585 = CARTESIAN_POINT ( 'NONE',  ( 9.348472636800000402, 1450.695831709190088, 206.5041896299389919 ) ) ;
#84586 = CARTESIAN_POINT ( 'NONE',  ( -6.863927053981574211, 1440.110827762987810, 185.9524514171546912 ) ) ;
#84587 = CARTESIAN_POINT ( 'NONE',  ( -5.551115123129999164E-16, 1408.913060387329779, 226.8598803041980148 ) ) ;
#84588 = CARTESIAN_POINT ( 'NONE',  ( -2.418203496729999902, 1454.903534402890045, 199.2876688155090221 ) ) ;
#84589 = CARTESIAN_POINT ( 'NONE',  ( 4.028307740155000261, 1516.797038924770050, 205.8554964580370097 ) ) ;
#84590 = CARTESIAN_POINT ( 'NONE',  ( 3.653657264300000040, 1446.290935082700116, 168.9981087564979987 ) ) ;
#84591 = ORIENTED_EDGE ( 'NONE', *, *, #14729, .T. ) ;
#84592 = CARTESIAN_POINT ( 'NONE',  ( -1.682837345762272729, 1464.049852190644287, 199.4516691750211521 ) ) ;
#84593 = CARTESIAN_POINT ( 'NONE',  ( -2.911830323659999831, 1496.243737683489826, 197.8821088022990011 ) ) ;
#84595 = ORIENTED_EDGE ( 'NONE', *, *, #5811, .F. ) ;
#84594 = CARTESIAN_POINT ( 'NONE',  ( -68.65709740368080816, 1379.747649760600098, 280.2671915801650471 ) ) ;
#84596 = CARTESIAN_POINT ( 'NONE',  ( -8.732807974784785543, 1381.269952321672918, 217.9317737700656039 ) ) ;
#84597 = EDGE_LOOP ( 'NONE', ( #109569, #51622, #51316 ) ) ;
#84598 = CARTESIAN_POINT ( 'NONE',  ( -16.20149550001009686, 1514.624327922590282, 223.9881805485040616 ) ) ;
#84599 = CARTESIAN_POINT ( 'NONE',  ( -24.93712286909999776, 1430.363841025129886, 208.7990758118230019 ) ) ;
#84601 = CARTESIAN_POINT ( 'NONE',  ( 15.77750609497879886, 1410.568644415290009, 191.5438104861989927 ) ) ;
#84600 = CARTESIAN_POINT ( 'NONE',  ( -10.81095005467450143, 1425.339529372819925, 121.9063493438599863 ) ) ;
#84602 = CARTESIAN_POINT ( 'NONE',  ( -5.770820179264999794, 1516.591755933730155, 210.8331571987770019 ) ) ;
#84603 = CARTESIAN_POINT ( 'NONE',  ( 38.46909107666640182, 1438.310882937109909, 136.5544058681170156 ) ) ;
#84604 = CARTESIAN_POINT ( 'NONE',  ( 21.42853521715711196, 1524.678541297860647, 234.0213767294899583 ) ) ;
#84605 = CARTESIAN_POINT ( 'NONE',  ( -39.40331698669999838, 1435.955742992169917, 259.1105223372980504 ) ) ;
#84606 = CARTESIAN_POINT ( 'NONE',  ( 10.89260962470000038, 1478.390639884389884, 204.6475587744990037 ) ) ;
#84607 = CARTESIAN_POINT ( 'NONE',  ( 13.65456221587469265, 1462.853443838520207, 230.7442824398011112 ) ) ;
#84608 = SHAPE_DEFINITION_REPRESENTATION ( #108163, #60858 ) ;
#84609 = CARTESIAN_POINT ( 'NONE',  ( 37.48372878014170340, 1450.753171827339884, 134.0999999986339901 ) ) ;
#84610 = PLANE ( 'NONE',  #65091 ) ;
#84611 = ORIENTED_EDGE ( 'NONE', *, *, #32164, .F. ) ;
#84612 = CARTESIAN_POINT ( 'NONE',  ( -18.29179302776010019, 1466.060351544859941, 217.7541585804449937 ) ) ;
#84613 = CARTESIAN_POINT ( 'NONE',  ( 18.54647816425740103, 1507.559819934359894, 190.5563924540620064 ) ) ;
#84614 = VERTEX_POINT ( 'NONE', #54661 ) ;
#84615 = ORIENTED_EDGE ( 'NONE', *, *, #17086, .T. ) ;
#84616 = CARTESIAN_POINT ( 'NONE',  ( -29.77441358006530692, 1509.998745987574921, 208.8337216755480483 ) ) ;
#84617 = CARTESIAN_POINT ( 'NONE',  ( 27.74152896581870209, 1446.393007474679962, 137.1637341980689939 ) ) ;
#84618 = DIRECTION ( 'NONE',  ( -0.7071067811865474617, -4.750184379286195842E-17, -0.7071067811865474617 ) ) ;
#84619 = CARTESIAN_POINT ( 'NONE',  ( -13.58885879944450004, 1508.451085982560016, 209.7742480560209799 ) ) ;
#84620 = CARTESIAN_POINT ( 'NONE',  ( 4.326992699839999901, 1515.158586648489973, 209.4786834863980118 ) ) ;
#84621 = CARTESIAN_POINT ( 'NONE',  ( -5.906564182353549519, 1454.472896573619892, 201.8136876099350161 ) ) ;
#84622 = CARTESIAN_POINT ( 'NONE',  ( 33.91369107978050579, 1435.681798568110025, 135.3769914806310055 ) ) ;
#84623 = CARTESIAN_POINT ( 'NONE',  ( 2.282008349603394048, 1516.544479074524361, 216.2688515719049462 ) ) ;
#84624 = CARTESIAN_POINT ( 'NONE',  ( 26.17054978140000188, 1441.643302558009964, 138.0857572941980038 ) ) ;
#84625 = CARTESIAN_POINT ( 'NONE',  ( -12.31951492099999967, 1391.575075857879938, 211.0344521122790127 ) ) ;
#84626 = CARTESIAN_POINT ( 'NONE',  ( -98.12353807537789407, 1384.868073826160071, 295.8671642013550240 ) ) ;
#84627 = VERTEX_POINT ( 'NONE', #88241 ) ;
#84628 = CARTESIAN_POINT ( 'NONE',  ( -5.780232115465000042, 1516.760434454289907, 201.7950504087270076 ) ) ;
#84629 = CARTESIAN_POINT ( 'NONE',  ( 4.042388501175000037, 1517.045004075700035, 209.8579434088520088 ) ) ;
#84630 = ORIENTED_EDGE ( 'NONE', *, *, #96749, .F. ) ;
#84631 = CARTESIAN_POINT ( 'NONE',  ( 10.79382126600000014, 1414.913060387329779, 222.1041115775979904 ) ) ;
#84632 = CARTESIAN_POINT ( 'NONE',  ( 20.19677127349999779, 1497.697269792330189, 228.1166628511979866 ) ) ;
#84633 = ORIENTED_EDGE ( 'NONE', *, *, #23551, .F. ) ;
#84634 = CARTESIAN_POINT ( 'NONE',  ( -13.45946769660000086, 1415.628674266529742, 221.4934452861980105 ) ) ;
#84635 = EDGE_CURVE ( 'NONE', #47452, #83109, #15657, .T. ) ;
#84636 = CARTESIAN_POINT ( 'NONE',  ( -16.90809753623369360, 1442.831169986191526, 162.4344573440251338 ) ) ;
#84637 = CARTESIAN_POINT ( 'NONE',  ( -17.30321976762949987, 1420.074570463099917, 205.0181995903979839 ) ) ;
#84638 = CARTESIAN_POINT ( 'NONE',  ( -3.660324660266798702, 1488.780526855528251, 219.3830879640146350 ) ) ;
#84639 = B_SPLINE_CURVE_WITH_KNOTS ( 'NONE', 3,
 ( #53368, #9679, #36003, #70196, #10803, #43848, #74845, #32273, #17503, #51702, #1300, #34883, #80759, #72912, #21909, #62907, #89152, #45531, #4602, #12440, #105410, #88073, #29248, #71854, #11900, #4067, #46625, #38192, #54483, #11360, #79671, #28702, #46074, #106503, #98091, #19738, #72374, #104854, #80206, #88620, #29792, #3524, #44973, #2976, #37094, #71296, #97018 ),
 .UNSPECIFIED., .F., .F.,
 ( 4, 2, 1, 1, 1, 2, 2, 2, 1, 1, 1, 1, 2, 2, 2, 1, 1, 1, 2, 2, 2, 1, 2, 2, 2, 1, 1, 2, 2, 4 ),
 ( 0.000000000000000000, 0.06249999999977556842, 0.09374999999964436781, 0.1093749999995976691, 0.1171874999995746874, 0.1210937499995635575, 0.1249999999995524136, 0.1874999999989931387, 0.2187499999986940447, 0.2343749999985445254, 0.2421874999984697518, 0.2460937499984326982, 0.2480468749984321430, 0.2499999999984315602, 0.3124999999987914667, 0.3437499999989717669, 0.3593749999990795141, 0.3671874999991333044, 0.3710937499991602273, 0.3749999999991870947, 0.4374999999993113287, 0.4687499999993546829, 0.4843749999993763877, 0.4999999999993980371, 0.6249999999994978461, 0.6874999999995653477, 0.7187499999995988764, 0.7343749999996155298, 0.7499999999996322941, 1.000000000000000000 ),
 .UNSPECIFIED. ) ;
#84640 = CARTESIAN_POINT ( 'NONE',  ( -13.39783700169999925, 1429.123728478029989, 222.2884932514979823 ) ) ;
#84641 = CARTESIAN_POINT ( 'NONE',  ( -8.974062746725300244, 1446.631196276342735, 153.7453213382308661 ) ) ;
#84642 = CARTESIAN_POINT ( 'NONE',  ( -9.165442406359998628, 1473.716948313090143, 204.3954301531890110 ) ) ;
#84643 = CARTESIAN_POINT ( 'NONE',  ( 6.766670517840000620, 1494.440262355989717, 218.9700614872689926 ) ) ;
#84644 = CARTESIAN_POINT ( 'NONE',  ( -56.68565291850000420, 1379.730069603700031, 254.3216308741590410 ) ) ;
#84645 = CARTESIAN_POINT ( 'NONE',  ( -15.87931877369999967, 1462.584440484630022, 222.8385820429980129 ) ) ;
#84647 = CARTESIAN_POINT ( 'NONE',  ( -7.891238773387773797, 1521.951704408389787, 228.7291753153190825 ) ) ;
#84646 = CARTESIAN_POINT ( 'NONE',  ( 18.07871887829999835, 1459.074710307329951, 227.9662036256980002 ) ) ;
#84648 = CARTESIAN_POINT ( 'NONE',  ( -5.022887173791962923, 1423.013679199760418, 184.8136794012343103 ) ) ;
#84649 = CARTESIAN_POINT ( 'NONE',  ( -2.499951737868360002, 1420.086717788219858, 94.80349057415200775 ) ) ;
#84650 = ORIENTED_EDGE ( 'NONE', *, *, #26714, .F. ) ;
#84651 = DIRECTION ( 'NONE',  ( 4.510281037539694659E-14, 0.000000000000000000, 1.000000000000000000 ) ) ;
#84652 = EDGE_CURVE ( 'NONE', #95096, #46920, #110700, .T. ) ;
#84653 = CARTESIAN_POINT ( 'NONE',  ( -22.08327125186907125, 1523.604703353109699, 233.8169256665491105 ) ) ;
#84654 = CARTESIAN_POINT ( 'NONE',  ( -0.7369042090349989804, 1517.080322339569875, 214.1333973382469935 ) ) ;
#84655 = CARTESIAN_POINT ( 'NONE',  ( -2.897552558531884870, 1484.306681456201659, 183.3139059294359754 ) ) ;
#84657 = ORIENTED_EDGE ( 'NONE', *, *, #23472, .F. ) ;
#84656 = CARTESIAN_POINT ( 'NONE',  ( -4.325405441708600307, 1515.219201591195315, 211.4519800884384608 ) ) ;
#84658 = CARTESIAN_POINT ( 'NONE',  ( 1.118234699620000105, 1453.152003547129880, 188.5610888405979892 ) ) ;
#84659 = CARTESIAN_POINT ( 'NONE',  ( 0.6929005668539989227, 1508.551703792989883, 220.2186279790989829 ) ) ;
#84660 = EDGE_CURVE ( 'NONE', #82365, #24499, #64309, .T. ) ;
#84661 = CARTESIAN_POINT ( 'NONE',  ( -11.74858685269999903, 1426.686222183830068, 144.9813623866980095 ) ) ;
#84662 = CARTESIAN_POINT ( 'NONE',  ( 1.639265462144630092, 1430.995086660350125, 199.7986407524330161 ) ) ;
#84663 = CARTESIAN_POINT ( 'NONE',  ( -10.92959825596109980, 1462.004401642820085, 210.4728761127730081 ) ) ;
#84664 = CARTESIAN_POINT ( 'NONE',  ( 2.968865197519999555, 1449.559759134390106, 190.1955703363989869 ) ) ;
#84665 = SPHERICAL_SURFACE ( 'NONE', #35935, 2.000000000000000000 ) ;
#84666 = CARTESIAN_POINT ( 'NONE',  ( 11.13973213087689906, 1470.272412021129867, 206.9146623043149873 ) ) ;
#84668 = CARTESIAN_POINT ( 'NONE',  ( -10.37387122080000168, 1479.853456435389944, 210.7819233329290114 ) ) ;
#84667 = CARTESIAN_POINT ( 'NONE',  ( -20.96279981269999837, 1495.371218722530102, 226.8017206206980063 ) ) ;
#84669 = CARTESIAN_POINT ( 'NONE',  ( 3.156194964112319479, 1466.544005466739918, 236.1242056213270075 ) ) ;
#84670 = ORIENTED_EDGE ( 'NONE', *, *, #43456, .F. ) ;
#84671 = CARTESIAN_POINT ( 'NONE',  ( -2.298369507954999946, 1516.779243033999819, 205.8702346062869992 ) ) ;
#84672 = CARTESIAN_POINT ( 'NONE',  ( 30.12538801500000218, 1414.390931448930132, 266.8625852646979979 ) ) ;
#84673 = CARTESIAN_POINT ( 'NONE',  ( 4.500000000000000000, 1425.929641636930000, 183.3886486283980162 ) ) ;
#84674 = CARTESIAN_POINT ( 'NONE',  ( 24.08617896360000188, 1449.722506852089964, 204.7855894934380103 ) ) ;
#84675 = CARTESIAN_POINT ( 'NONE',  ( 18.91079974722019941, 1425.084603971189836, 222.8166007544258491 ) ) ;
#84677 = B_SPLINE_CURVE_WITH_KNOTS ( 'NONE', 3,
 ( #108663, #83449, #6744, #7850, #76717, #76167, #86215, #69450, #85105, #59390, #42018, #8953 ),
 .UNSPECIFIED., .F., .F.,
 ( 4, 2, 2, 2, 2, 4 ),
 ( 0.08322961861458730293, 0.09974321616496879817, 0.1194478573530819987, 0.1410535409231579995, 0.1638632366236909832, 0.1642061257107060024 ),
 .UNSPECIFIED. ) ;
#84676 = CARTESIAN_POINT ( 'NONE',  ( -8.071897329778668251, 1387.339191243697087, 218.5828327136565008 ) ) ;
#84678 = CARTESIAN_POINT ( 'NONE',  ( -1.804408714559999849, 1450.411044013399987, 182.7103574280979785 ) ) ;
#84679 = EDGE_CURVE ( 'NONE', #36772, #102747, #97206, .T. ) ;
#84680 = B_SPLINE_CURVE_WITH_KNOTS ( 'NONE', 3,
 ( #26357, #36419, #10685, #85166, #97966, #54358, #19614, #80636, #12313, #20700 ),
 .UNSPECIFIED., .F., .F.,
 ( 4, 2, 2, 2, 4 ),
 ( -0.1358568304961229878, -0.09953452613532230708, -0.06373121003967659182, -0.02032877986101701284, 0.000000000000000000 ),
 .UNSPECIFIED. ) ;
#84681 = CARTESIAN_POINT ( 'NONE',  ( 0.000000000000000000, 1523.382868172864164, 209.1218459616979999 ) ) ;
#84682 = CARTESIAN_POINT ( 'NONE',  ( -14.68950664279999963, 1417.178464496219931, 203.9617939164890004 ) ) ;
#84683 = CARTESIAN_POINT ( 'NONE',  ( -14.46612070239999959, 1444.027671829609972, 188.8340718453980003 ) ) ;
#84684 = CARTESIAN_POINT ( 'NONE',  ( -18.65529551030000022, 1453.313060387329870, 216.4487054234179766 ) ) ;
#84685 = LINE ( 'NONE', #34290, #35833 ) ;
#84686 = CARTESIAN_POINT ( 'NONE',  ( -4.165531658079999922, 1496.711016394489889, 219.7171372811990295 ) ) ;
#84687 = CARTESIAN_POINT ( 'NONE',  ( 1.113400972200000005, 1478.239378852390018, 201.5788048326690216 ) ) ;
#84688 = CARTESIAN_POINT ( 'NONE',  ( -13.84930592310000108, 1431.437219492539953, 209.1218459616979999 ) ) ;
#84689 = CARTESIAN_POINT ( 'NONE',  ( -10.99386358867370106, 1508.551709148380041, 208.1089302384970097 ) ) ;
#84690 = CARTESIAN_POINT ( 'NONE',  ( -2.472546487080370170, 1422.360492482099744, 192.6709265187130029 ) ) ;
#84691 = CARTESIAN_POINT ( 'NONE',  ( -14.53064231559999975, 1473.849484241330174, 269.2157382448979774 ) ) ;
#84692 = CARTESIAN_POINT ( 'NONE',  ( -30.83402112502179904, 1524.872178180563878, 196.5182538919386843 ) ) ;
#84693 = CARTESIAN_POINT ( 'NONE',  ( -22.27620219389999789, 1509.702625318030186, 189.6894442619980055 ) ) ;
#84694 = CARTESIAN_POINT ( 'NONE',  ( -24.44412394876377093, 1444.690170677753258, 211.0767915248584075 ) ) ;
#84695 = CARTESIAN_POINT ( 'NONE',  ( -57.27374972444740564, 1384.706877432339979, 276.1255075189790205 ) ) ;
#84696 = CARTESIAN_POINT ( 'NONE',  ( -24.13664782116140017, 1384.958061910630022, 202.9396497235290155 ) ) ;
#84697 = CARTESIAN_POINT ( 'NONE',  ( 12.03450403489540044, 1415.834070662830072, 223.3500408510359989 ) ) ;
#84698 = DIRECTION ( 'NONE',  ( 0.000000000000000000, -1.000000000000000000, 0.000000000000000000 ) ) ;
#84699 = CARTESIAN_POINT ( 'NONE',  ( -15.55458060831606382, 1415.677404892448294, 209.5577834297775155 ) ) ;
#84700 = CARTESIAN_POINT ( 'NONE',  ( -2.330134126090000368, 1515.551704408389924, 205.2922258481490303 ) ) ;
#84701 = CARTESIAN_POINT ( 'NONE',  ( -23.03428792449999918, 1410.212555181330117, 205.5016647962879972 ) ) ;
#84702 =( BOUNDED_SURFACE ( )  B_SPLINE_SURFACE ( 3, 2, ( 
 ( #25416, #103232, #95417 ),
 ( #34943, #61845, #10867 ),
 ( #18680, #45040, #52878 ),
 ( #1932, #86454, #10295 ),
 ( #70809, #69129, #79185 ),
 ( #60737, #25971, #94288 ),
 ( #94859, #18134, #44471 ),
 ( #78616, #27658, #59610 ),
 ( #9745, #17002, #76963 ),
 ( #51202, #43911, #78054 ),
 ( #85331, #8628, #42803 ),
 ( #37167, #88134, #71915 ),
 ( #13582, #89762, #20891 ),
 ( #81347, #64040, #4128 ) ),
 .UNSPECIFIED., .F., .F., .F. ) 
 B_SPLINE_SURFACE_WITH_KNOTS ( ( 4, 2, 2, 2, 2, 2, 4 ),
 ( 3, 3 ),
 ( 0.000000000000000000, 0.0009440840677145154007, 0.001416126101571773101, 0.001888168135429030801, 0.002360210169286288719, 0.002832252203143546202, 0.003776336270858061603 ),
 ( 0.000000000000000000, 1.000000000000000000 ),
 .UNSPECIFIED. ) 
 GEOMETRIC_REPRESENTATION_ITEM ( )  RATIONAL_B_SPLINE_SURFACE ( (
 ( 1.000000000000000000, 0.8070209408750085300, 1.000000000000000000),
 ( 1.000000000000000000, 0.8215603905277785168, 1.000000000000000000),
 ( 1.000000000000000000, 0.8340988699069226131, 1.000000000000000000),
 ( 1.000000000000000000, 0.8516751610454621479, 1.000000000000000000),
 ( 1.000000000000000000, 0.8573697395118552445, 1.000000000000000000),
 ( 1.000000000000000000, 0.8683586635697856382, 1.000000000000000000),
 ( 1.000000000000000000, 0.8736518481707646888, 1.000000000000000000),
 ( 1.000000000000000000, 0.8840377753031072317, 1.000000000000000000),
 ( 1.000000000000000000, 0.8891294171307223548, 1.000000000000000000),
 ( 1.000000000000000000, 0.8992456600573884851, 1.000000000000000000),
 ( 1.000000000000000000, 0.9042785869247129682, 1.000000000000000000),
 ( 1.000000000000000000, 0.9189749222850194244, 1.000000000000000000),
 ( 1.000000000000000000, 0.9283978182339867047, 1.000000000000000000),
 ( 1.000000000000000000, 0.9376006582765946673, 1.000000000000000000) ) ) 
 REPRESENTATION_ITEM ( '' )  SURFACE ( )  );
#84703 = CARTESIAN_POINT ( 'NONE',  ( -11.50806463233310772, 1378.506956290408880, 204.6827186876646181 ) ) ;
#84704 = CARTESIAN_POINT ( 'NONE',  ( 4.702100396339999655, 1484.396536161289987, 219.5556203100990160 ) ) ;
#84705 = B_SPLINE_CURVE_WITH_KNOTS ( 'NONE', 3,
 ( #4522, #5618, #106965, #97470, #40310, #39770, #64983, #3986, #98559, #73930, #12902, #106421, #13433, #31356, #99099, #29706, #38111, #65540, #54935, #98006, #47623, #12349, #21827, #91270, #99648, #20740, #22939, #39201, #56026, #105883, #63891, #21276, #90151, #81749, #55485, #29164, #5056, #48737, #46539, #73377, #57142, #14550, #82863 ),
 .UNSPECIFIED., .F., .F.,
 ( 4, 3, 3, 3, 3, 3, 3, 3, 3, 3, 3, 3, 3, 3, 4 ),
 ( -1.999999998304380133, -1.940506176228419921, -1.795837195207230064, -1.649175357432780098, -1.501247921597500090, -1.351435166382589870, -1.200651412290280051, -1.049213174562420026, -0.8974822393858350456, -0.7399797023974719057, -0.5893366077835271444, -0.4397854573115069776, -0.2915963409840560683, -0.1449609066947019631, 0.000000000000000000 ),
 .UNSPECIFIED. ) ;
#84706 = CARTESIAN_POINT ( 'NONE',  ( 10.35103189252669864, 1480.844217530770038, 207.0564529105199938 ) ) ;
#84707 = CARTESIAN_POINT ( 'NONE',  ( -5.790397269885580123, 1452.878744171119934, 206.0071839347059779 ) ) ;
#84708 = CARTESIAN_POINT ( 'NONE',  ( -19.40999286329999762, 1446.496631621190090, 200.0861365869990038 ) ) ;
#84709 = CARTESIAN_POINT ( 'NONE',  ( 16.85976061912555579, 1525.821544997590308, 182.0492613858612003 ) ) ;
#84710 = CARTESIAN_POINT ( 'NONE',  ( -22.19117979951819919, 1483.602007699049864, 216.8115292459999921 ) ) ;
#84712 = CARTESIAN_POINT ( 'NONE',  ( -15.33574365116500182, 1514.703592237370003, 193.3867305263669891 ) ) ;
#84711 = CARTESIAN_POINT ( 'NONE',  ( -22.53878309250000100, 1411.058442772730132, 212.0450770775579770 ) ) ;
#84713 = CARTESIAN_POINT ( 'NONE',  ( 11.71865588026039973, 1426.707724708179967, 142.8540073575470046 ) ) ;
#84714 = CARTESIAN_POINT ( 'NONE',  ( -2.469737522550000453, 1507.227429587890128, 221.7265305498989960 ) ) ;
#84715 = CARTESIAN_POINT ( 'NONE',  ( -6.701092706527290055, 1517.051709179880163, 205.3286261131629828 ) ) ;
#84716 = CARTESIAN_POINT ( 'NONE',  ( 7.722580314274999580, 1517.051704408389924, 210.6910072246569996 ) ) ;
#84717 = VECTOR ( 'NONE', #66746, 1000.000000000000000 ) ;
#84718 = CARTESIAN_POINT ( 'NONE',  ( -0.06979898235752290958, 1408.910622953190114, 224.1218459617979875 ) ) ;
#84719 = CARTESIAN_POINT ( 'NONE',  ( -2.292940207144999576, 1516.565291103010168, 202.5758065368070220 ) ) ;
#84720 = DIRECTION ( 'NONE',  ( -0.6709778558543747495, 0.000000000000000000, 0.7414773880254650340 ) ) ;
#84721 = DIRECTION ( 'NONE',  ( 9.500914144214121536E-47, -1.000000000000000000, 1.836970198721029688E-16 ) ) ;
#84722 = CARTESIAN_POINT ( 'NONE',  ( 16.28235094783499903, 1514.570049710740022, 194.2914897994669730 ) ) ;
#84723 = FACE_BOUND ( 'NONE', #101044, .T. ) ;
#84724 = CARTESIAN_POINT ( 'NONE',  ( -28.23626297441629873, 1380.228258317559948, 215.8353171725599964 ) ) ;
#84725 = CARTESIAN_POINT ( 'NONE',  ( 21.81488504828589825, 1509.642650274630114, 228.1804615763130073 ) ) ;
#84726 = CIRCLE ( 'NONE', #36461, 1.000000000000085043 ) ;
#84728 = VERTEX_POINT ( 'NONE', #6980 ) ;
#84727 = CARTESIAN_POINT ( 'NONE',  ( -52.24721073780899872, 1379.695346391380099, 249.9998916442930010 ) ) ;
#84729 = EDGE_LOOP ( 'NONE', ( #59979, #99563, #67797, #75372, #24329, #21911 ) ) ;
#84730 = CARTESIAN_POINT ( 'NONE',  ( 11.37082106925189962, 1434.131391724269861, 151.4751752372850149 ) ) ;
#84731 = CARTESIAN_POINT ( 'NONE',  ( -2.663926418229999982, 1397.071489263530111, 221.9487469225979908 ) ) ;
#84732 = ORIENTED_EDGE ( 'NONE', *, *, #7293, .T. ) ;
#84733 = CARTESIAN_POINT ( 'NONE',  ( -107.4962408000000096, 1378.913060387289988, 308.3050959158589990 ) ) ;
#84734 = CARTESIAN_POINT ( 'NONE',  ( -109.1309838779999950, 1384.924111747649931, 311.2646842872590014 ) ) ;
#84735 = CARTESIAN_POINT ( 'NONE',  ( 15.90990255763500016, 1516.814170398969964, 193.9190501556669801 ) ) ;
#84737 = CARTESIAN_POINT ( 'NONE',  ( -13.73190975862210017, 1508.113242452410077, 184.1859641058979946 ) ) ;
#84736 = CARTESIAN_POINT ( 'NONE',  ( 2.531901238200000126, 1444.224916984790070, 200.5256934874690273 ) ) ;
#84738 = CARTESIAN_POINT ( 'NONE',  ( 17.31952399019999689, 1507.813089787830222, 230.9486221998979829 ) ) ;
#84739 = CARTESIAN_POINT ( 'NONE',  ( 1.921582663709999972, 1449.239314806859966, 183.7267869822979947 ) ) ;
#84740 = CARTESIAN_POINT ( 'NONE',  ( -5.314268782590000129, 1416.216252248729916, 191.8300084588979928 ) ) ;
#84741 = CARTESIAN_POINT ( 'NONE',  ( 0.7491281650140010351, 1417.862047144630196, 204.0277727146790028 ) ) ;
#84742 = B_SPLINE_SURFACE_WITH_KNOTS ( 'NONE', 5, 5, ( 
 ( #88449, #104139, #87914, #52648, #63277, #10641 ),
 ( #46466, #80598, #1701, #45907, #105814, #3364 ),
 ( #96294, #44808, #72221, #106343, #3913, #86785 ),
 ( #62168, #11201, #27424, #71694, #19574, #61607 ),
 ( #37491, #20660, #20127, #28540, #29629, #53777 ),
 ( #38042, #95190, #45366, #29092, #44249, #2810 ),
 ( #97389, #19004, #36929, #10074, #79505, #54862 ),
 ( #78392, #71126, #2269, #88985, #70026, #18449 ),
 ( #78962, #105247, #62739, #11738, #53204, #87345 ) ),
 .UNSPECIFIED., .F., .F., .F.,
 ( 6, 3, 6 ),
 ( 6, 6 ),
 ( 3.182111802360319874, 6.655162634330000770, 7.748822666508919710 ),
 ( -0.0004160027669829020002, 2.000000000000000000 ),
 .UNSPECIFIED. ) ;
#84743 = CARTESIAN_POINT ( 'NONE',  ( 4.566198684544860775, 1396.072515563980005, 199.0791066682190262 ) ) ;
#84744 = DIRECTION ( 'NONE',  ( 0.000000000000000000, 0.000000000000000000, -1.000000000000000000 ) ) ;
#84745 = CARTESIAN_POINT ( 'NONE',  ( 11.86664183439999931, 1432.373872705260283, 149.9823177143980217 ) ) ;
#84746 = CARTESIAN_POINT ( 'NONE',  ( 6.439137434935000570, 1514.557408760799945, 201.1783224906369867 ) ) ;
#84747 = ORIENTED_EDGE ( 'NONE', *, *, #7727, .T. ) ;
#84748 = CARTESIAN_POINT ( 'NONE',  ( 13.07083448467220066, 1435.604313765049938, 150.5504815018899762 ) ) ;
#84749 = CIRCLE ( 'NONE', #52559, 1.000000000000007994 ) ;
#84750 = VERTEX_POINT ( 'NONE', #100487 ) ;
#84751 = ORIENTED_EDGE ( 'NONE', *, *, #41192, .T. ) ;
#84752 = CARTESIAN_POINT ( 'NONE',  ( 13.48176841661342706, 1444.196030681880757, 169.3584259374786143 ) ) ;
#84753 = CARTESIAN_POINT ( 'NONE',  ( -4.034591554379999501, 1464.976194902429825, 235.4333245580980076 ) ) ;
#84754 = FACE_OUTER_BOUND ( 'NONE', #15311, .T. ) ;
#84755 = CARTESIAN_POINT ( 'NONE',  ( 4.035490712554999249, 1516.630499592039996, 216.8333966482170183 ) ) ;
#84756 = CARTESIAN_POINT ( 'NONE',  ( -8.150371712873907271, 1511.506728505250976, 212.9804710034640038 ) ) ;
#84757 = B_SPLINE_SURFACE_WITH_KNOTS ( 'NONE', 5, 4, ( 
 ( #9152, #36555, #103763, #76915, #44422 ),
 ( #17515, #78564, #2440, #60682, #19172 ),
 ( #18083, #53947, #9691, #69640, #766 ),
 ( #34348, #27064, #8583, #51713, #1880 ),
 ( #43316, #77464, #34895, #69083, #52278 ),
 ( #1312, #103184, #18626, #86403, #43859 ) ),
 .UNSPECIFIED., .F., .F., .F.,
 ( 6, 6 ),
 ( 5, 5 ),
 ( 0.000000000000000000, 52.98902693510000006 ),
 ( 40.20365518519999881, 50.26548245740000453 ),
 .UNSPECIFIED. ) ;
#84758 = CARTESIAN_POINT ( 'NONE',  ( 11.73855662635810049, 1421.952273329259924, 209.4052689870339918 ) ) ;
#84759 = CARTESIAN_POINT ( 'NONE',  ( 2.500000000000000000, 1448.201357973759968, 168.5759913970699984 ) ) ;
#84760 = CARTESIAN_POINT ( 'NONE',  ( -11.59474938729999849, 1379.412984648580050, 207.1178716384889924 ) ) ;
#84761 = VERTEX_POINT ( 'NONE', #83143 ) ;
#84762 = CARTESIAN_POINT ( 'NONE',  ( 6.546951682585000043, 1516.606339319019980, 206.2472570094369928 ) ) ;
#84763 = ORIENTED_EDGE ( 'NONE', *, *, #84962, .F. ) ;
#84764 = CARTESIAN_POINT ( 'NONE',  ( 21.85224605700239664, 1440.913060387330006, 226.6615408831969773 ) ) ;
#84765 = DIRECTION ( 'NONE',  ( 0.9942586961433743653, 0.000000000000000000, -0.1070030146457445208 ) ) ;
#84766 = CARTESIAN_POINT ( 'NONE',  ( -2.760778262710000153, 1409.009468888630181, 188.0459436639980026 ) ) ;
#84767 = CARTESIAN_POINT ( 'NONE',  ( 7.378505815095000031, 1513.311928781879942, 216.7671994646370024 ) ) ;
#84769 = ORIENTED_EDGE ( 'NONE', *, *, #77513, .T. ) ;
#84768 = DIRECTION ( 'NONE',  ( 0.9999994573234139983, 9.540975887252238799E-32, -0.001041802705676339504 ) ) ;
#84770 = CARTESIAN_POINT ( 'NONE',  ( 19.19790826559999886, 1425.425173530230040, 222.4585045609979943 ) ) ;
#84771 = DIRECTION ( 'NONE',  ( 1.755985294532469921E-16, -1.000000000000000000, 1.338183447452831989E-16 ) ) ;
#84772 = DIRECTION ( 'NONE',  ( -0.1262450234450830377, -0.9881880602473954722, -0.08687089063570453684 ) ) ;
#84773 = CARTESIAN_POINT ( 'NONE',  ( 5.641423425050000162, 1453.485726096290136, 216.6286100207389893 ) ) ;
#84774 = FACE_OUTER_BOUND ( 'NONE', #49893, .T. ) ;
#84775 = B_SPLINE_SURFACE_WITH_KNOTS ( 'NONE', 5, 1, ( 
 ( #79233, #106073 ),
 ( #46193, #38303 ),
 ( #96577, #45647 ),
 ( #72484, #62454 ),
 ( #80327, #2542 ),
 ( #10918, #12013 ) ),
 .UNSPECIFIED., .F., .F., .F.,
 ( 6, 6 ),
 ( 2, 2 ),
 ( -3.552713678800000397E-15, 17.98770270289999829 ),
 ( 0.000000000000000000, 14.00000000000000000 ),
 .UNSPECIFIED. ) ;
#84776 = CARTESIAN_POINT ( 'NONE',  ( -1.703779643355000095, 1517.057265928030120, 213.1670284501570052 ) ) ;
#84777 = CARTESIAN_POINT ( 'NONE',  ( -2.739337719001559979, 1429.065489528160015, 200.1608258868419910 ) ) ;
#84778 = CARTESIAN_POINT ( 'NONE',  ( 18.51436573157378618, 1512.187213306747481, 237.1421867457405881 ) ) ;
#84779 = ADVANCED_FACE ( 'NONE', ( #90421 ), #64161, .F. ) ;
#84780 = CARTESIAN_POINT ( 'NONE',  ( 6.725587746340760731, 1508.728101425929935, 216.3255536485930293 ) ) ;
#84781 = CARTESIAN_POINT ( 'NONE',  ( -3.445407572115000150, 1516.764084769670262, 211.4198948937369948 ) ) ;
#84782 = CARTESIAN_POINT ( 'NONE',  ( 9.760716701452610167, 1435.124984824069998, 208.1605893237319833 ) ) ;
#84783 = CARTESIAN_POINT ( 'NONE',  ( 13.96308414129999953, 1409.400662026229838, 192.3471292444979781 ) ) ;
#84784 = CARTESIAN_POINT ( 'NONE',  ( 10.96966286673369950, 1432.359740019160199, 151.7701370213850112 ) ) ;
#84786 = EDGE_LOOP ( 'NONE', ( #100896, #82657, #72082, #12602, #55908, #37788, #37266, #61119, #46306, #70701, #100972, #40560, #1003, #65640, #96279 ) ) ;
#84785 = CARTESIAN_POINT ( 'NONE',  ( -61.70697236710000055, 1389.529122514739811, 255.3348362324589971 ) ) ;
#84787 = CARTESIAN_POINT ( 'NONE',  ( -56.94714792227870248, 1385.081906637989960, 275.5148282826739887 ) ) ;
#84788 = CARTESIAN_POINT ( 'NONE',  ( 36.81313713790000008, 1440.913060390829969, 254.5659540704979804 ) ) ;
#84789 = DIRECTION ( 'NONE',  ( -0.9993779836618710277, -0.0009462243742934110021, -0.03525266559235790131 ) ) ;
#84790 = CARTESIAN_POINT ( 'NONE',  ( -17.88319654240000034, 1498.319094940030027, 229.4271405375980066 ) ) ;
#84791 = CARTESIAN_POINT ( 'NONE',  ( -2.373667526830000263, 1462.975913846089952, 202.4942268867290238 ) ) ;
#84792 = CARTESIAN_POINT ( 'NONE',  ( 44.93136576140000926, 1440.913060387330006, 269.6838065358980430 ) ) ;
#84793 = AXIS2_PLACEMENT_3D ( 'NONE', #6672, #41391, #40272 ) ;
#84795 = CARTESIAN_POINT ( 'NONE',  ( -5.303300877965000382, 1513.301704408390151, 198.8687976239669979 ) ) ;
#84794 = CARTESIAN_POINT ( 'NONE',  ( -1.710012758625000018, 1517.232977404109988, 216.8491730849570160 ) ) ;
#84796 = DIRECTION ( 'NONE',  ( -1.986952269380850554E-13, 0.03085824620771311644, 0.9995237709234254808 ) ) ;
#84797 = CARTESIAN_POINT ( 'NONE',  ( -106.7969504679039972, 1381.490362223440115, 309.5173506577110061 ) ) ;
#84798 = EDGE_LOOP ( 'NONE', ( #83089, #5023, #8337, #44856, #102615 ) ) ;
#84799 = CARTESIAN_POINT ( 'NONE',  ( -2.292940207144999576, 1516.565291103010168, 202.5758065368070220 ) ) ;
#84800 = CARTESIAN_POINT ( 'NONE',  ( 0.3744771583600000064, 1467.623228442029813, 229.4021283991980056 ) ) ;
#84801 = AXIS2_PLACEMENT_3D ( 'NONE', #2100, #86621, #9914 ) ;
#84802 = CARTESIAN_POINT ( 'NONE',  ( 24.54353315340000208, 1443.825479976730094, 213.3278313276680080 ) ) ;
#84803 = CARTESIAN_POINT ( 'NONE',  ( 38.58235177202990940, 1444.329162690310113, 137.1361782392559689 ) ) ;
#84804 = DIRECTION ( 'NONE',  ( -0.000000000000000000, -1.000000000000000000, -0.000000000000000000 ) ) ;
#84805 = CARTESIAN_POINT ( 'NONE',  ( -1.142849984530000196, 1443.644273027190138, 218.3503460313989990 ) ) ;
#84806 = CARTESIAN_POINT ( 'NONE',  ( 8.041051540796583907, 1417.091402351465149, 230.7851105917766290 ) ) ;
#84807 = CARTESIAN_POINT ( 'NONE',  ( 30.86935880328820048, 1436.051794213489757, 136.3934173885100165 ) ) ;
#84808 = CARTESIAN_POINT ( 'NONE',  ( 38.68457868389829457, 1448.131034673710019, 136.4755686143420235 ) ) ;
#84809 = LINE ( 'NONE', #42275, #71779 ) ;
#84810 = CARTESIAN_POINT ( 'NONE',  ( -109.4729007030000076, 1386.928382911489962, 297.3007661288589816 ) ) ;
#84811 = CARTESIAN_POINT ( 'NONE',  ( 14.38189351659999993, 1509.358429554029954, 184.5350612304979734 ) ) ;
#84812 = CARTESIAN_POINT ( 'NONE',  ( -21.08094518543032336, 1525.506926151470907, 184.0391977492186015 ) ) ;
#84813 = DIRECTION ( 'NONE',  ( -0.000000000000000000, -1.000000000000000000, -0.000000000000000000 ) ) ;
#84814 = VERTEX_POINT ( 'NONE', #47887 ) ;
#84815 = CARTESIAN_POINT ( 'NONE',  ( 9.698064461892839105, 1462.705242386489999, 208.0596150282290182 ) ) ;
#84816 = FACE_OUTER_BOUND ( 'NONE', #41202, .T. ) ;
#84817 = CARTESIAN_POINT ( 'NONE',  ( 11.40070752235540041, 1470.941042065359852, 209.0206955636659814 ) ) ;
#84818 = CARTESIAN_POINT ( 'NONE',  ( -7.599227184291730275, 1512.341036968809931, 211.3567690145959830 ) ) ;
#84819 = CARTESIAN_POINT ( 'NONE',  ( 11.44901156743445902, 1425.804225261266083, 139.1025670327599926 ) ) ;
#84820 = CARTESIAN_POINT ( 'NONE',  ( -0.4151546846821903003, 1522.382868172863937, 173.3106345060153046 ) ) ;
#84821 = CARTESIAN_POINT ( 'NONE',  ( -29.28654146900000299, 1509.872632246929925, 209.3496755897299977 ) ) ;
#84822 = CARTESIAN_POINT ( 'NONE',  ( 7.106794650369999466, 1425.525179449380175, 212.0614358484589843 ) ) ;
#84823 = CARTESIAN_POINT ( 'NONE',  ( -2.936816566051450028, 1515.374151772610048, 213.3816236500609875 ) ) ;
#84824 = CARTESIAN_POINT ( 'NONE',  ( -20.96933869981734588, 1450.949473037474036, 144.4962461051783578 ) ) ;
#84825 = B_SPLINE_CURVE_WITH_KNOTS ( 'NONE', 5,
 ( #65513, #105858, #64411, #55458, #99623, #47596 ),
 .UNSPECIFIED., .F., .F.,
 ( 6, 6 ),
 ( 0.000000000000000000, 1.000000000000000000 ),
 .UNSPECIFIED. ) ;
#84826 = CARTESIAN_POINT ( 'NONE',  ( -18.05420922962109742, 1416.521607925270018, 209.3411825106769868 ) ) ;
#84827 = CARTESIAN_POINT ( 'NONE',  ( 23.99508155959999911, 1435.335429155559950, 136.6133439143980013 ) ) ;
#84828 = CARTESIAN_POINT ( 'NONE',  ( 4.427981723884999887, 1510.423579818969984, 216.6708627338570068 ) ) ;
#84829 = EDGE_LOOP ( 'NONE', ( #79676, #95858, #69078, #46960 ) ) ;
#84830 = VECTOR ( 'NONE', #51470, 1000.000000000000114 ) ;
#84831 = CARTESIAN_POINT ( 'NONE',  ( 1.239262138261830071, 1414.972329067380088, 191.7539262446190094 ) ) ;
#84832 = CARTESIAN_POINT ( 'NONE',  ( 4.141698392683508700, 1493.371568340419344, 219.5018937535342900 ) ) ;
#84833 = ORIENTED_EDGE ( 'NONE', *, *, #99266, .T. ) ;
#84834 = ORIENTED_EDGE ( 'NONE', *, *, #42848, .T. ) ;
#84835 = CARTESIAN_POINT ( 'NONE',  ( -8.881784197000000993E-16, 1414.413060387330006, 209.1218459616989946 ) ) ;
#84836 = CARTESIAN_POINT ( 'NONE',  ( 7.467587119939531171, 1516.687838964707225, 208.2872662270863486 ) ) ;
#84838 = CARTESIAN_POINT ( 'NONE',  ( -22.50357283319999979, 1452.344118194430166, 225.2792279245980183 ) ) ;
#84837 = CARTESIAN_POINT ( 'NONE',  ( 11.02695407560000085, 1426.510375595630194, 92.69043260369780057 ) ) ;
#84839 = CARTESIAN_POINT ( 'NONE',  ( -1.676218328139999825, 1445.210232295889909, 217.9771989461590351 ) ) ;
#84840 = CARTESIAN_POINT ( 'NONE',  ( 4.178231331191369691, 1424.123642773229903, 184.3799813994870078 ) ) ;
#84841 = CARTESIAN_POINT ( 'NONE',  ( -12.30243638853569976, 1378.355143918360227, 209.9197086792210030 ) ) ;
#84842 = CARTESIAN_POINT ( 'NONE',  ( -2.727235894615162692, 1420.119452836188657, 186.0440366003105908 ) ) ;
#84843 = CARTESIAN_POINT ( 'NONE',  ( -0.8350686643532179154, 1526.382868172863937, 240.9330574173806951 ) ) ;
#84844 = CARTESIAN_POINT ( 'NONE',  ( -24.21720135390000195, 1438.555912338969847, 211.3959883349679956 ) ) ;
#84845 = CARTESIAN_POINT ( 'NONE',  ( 2.246798639239999673, 1452.411382190229915, 183.6586391263979863 ) ) ;
#84846 = CARTESIAN_POINT ( 'NONE',  ( 8.803103321107110801, 1364.263256477290497, 207.6218459616988241 ) ) ;
#84847 = CARTESIAN_POINT ( 'NONE',  ( -6.519909027102049670, 1477.757526204120040, 213.0818532017610210 ) ) ;
#84849 = ORIENTED_EDGE ( 'NONE', *, *, #22964, .F. ) ;
#84848 = CARTESIAN_POINT ( 'NONE',  ( -2.386211797780819926E-09, 1414.144573887250090, 247.2442443194049986 ) ) ;
#84850 = ORIENTED_EDGE ( 'NONE', *, *, #69999, .T. ) ;
#84851 = CARTESIAN_POINT ( 'NONE',  ( -11.84830064420589935, 1431.103738429200121, 149.8426049743330282 ) ) ;
#84852 = ADVANCED_FACE ( 'NONE', ( #108342 ), #90979, .T. ) ;
#84853 = ADVANCED_FACE ( 'NONE', ( #55766 ), #107262, .F. ) ;
#84854 = CARTESIAN_POINT ( 'NONE',  ( -19.87603051640006058, 1484.414881828269699, 191.2154138880676726 ) ) ;
#84855 = CARTESIAN_POINT ( 'NONE',  ( -3.422119479379999607, 1471.692614597330021, 269.8663692098979823 ) ) ;
#84856 = CARTESIAN_POINT ( 'NONE',  ( 13.15423960803081371, 1434.846439206664854, 146.8772667774931904 ) ) ;
#84857 = CARTESIAN_POINT ( 'NONE',  ( -130.5852908491498852, 1331.448250124730066, 299.8337207750958555 ) ) ;
#84859 = EDGE_CURVE ( 'NONE', #96103, #105990, #31625, .T. ) ;
#84858 = DIRECTION ( 'NONE',  ( 1.000000000000000000, -0.000000000000000000, -0.000000000000000000 ) ) ;
#84860 = CARTESIAN_POINT ( 'NONE',  ( -2.476313965196780043, 1475.157094210569994, 197.9550708103259922 ) ) ;
#84861 = ADVANCED_FACE ( 'NONE', ( #98834 ), #16022, .F. ) ;
#84862 = CARTESIAN_POINT ( 'NONE',  ( -22.92822468967000304, 1507.593738162509908, 207.9867144894979845 ) ) ;
#84863 = CARTESIAN_POINT ( 'NONE',  ( 5.738076989630942037, 1370.712929383438905, 209.6218459617033432 ) ) ;
#84864 = CARTESIAN_POINT ( 'NONE',  ( -10.28551112630600173, 1447.520881842850031, 210.2972423999289902 ) ) ;
#84865 = CARTESIAN_POINT ( 'NONE',  ( -8.265472002072838720, 1407.311149223810162, 269.6288060363389718 ) ) ;
#84866 = CARTESIAN_POINT ( 'NONE',  ( -13.96141929067220033, 1435.007875777050003, 148.7887252966330038 ) ) ;
#84867 = ORIENTED_EDGE ( 'NONE', *, *, #12567, .T. ) ;
#84868 = CARTESIAN_POINT ( 'NONE',  ( -12.55604107059999919, 1391.387401865550146, 208.6966032511679714 ) ) ;
#84869 = CARTESIAN_POINT ( 'NONE',  ( 14.00316683389999994, 1442.877080914420048, 189.4713982969979895 ) ) ;
#84870 = B_SPLINE_SURFACE_WITH_KNOTS ( 'NONE', 5, 3, ( 
 ( #62514, #70359, #55757, #97726 ),
 ( #19345, #3149, #55201, #28323 ),
 ( #97174, #12624, #46256, #45146 ),
 ( #46802, #104472, #2597, #20447 ),
 ( #106672, #61957, #79287, #80932 ),
 ( #53545, #29962, #88785, #96636 ),
 ( #12066, #37829, #36722, #19906 ),
 ( #45703, #37281, #72015, #4230 ),
 ( #10412, #38364, #64154, #98273 ),
 ( #44582, #74747, #31618, #14262 ),
 ( #40576, #14815, #56841, #74205 ),
 ( #22636, #92083, #6431, #108885 ),
 ( #31068, #32178, #65249, #47329 ),
 ( #66362, #91537, #64709, #48452 ),
 ( #73651, #56284, #108335, #15357 ),
 ( #90414, #98827, #23763, #38907 ),
 ( #65796, #99360, #41126, #107229 ),
 ( #100481, #90973, #81458, #109449 ),
 ( #101017, #82590, #5881, #40025 ),
 ( #66909, #4763, #22087, #99917 ),
 ( #23212, #32729, #49550, #57412 ),
 ( #13144, #13694, #75306, #24315 ),
 ( #49002, #73089, #83135, #30519 ),
 ( #83675, #57950, #6972, #89875 ),
 ( #47880, #82017, #5322, #39481 ),
 ( #107783, #16991, #103804, #34388 ),
 ( #102126, #59055, #43356, #92625 ),
 ( #24853, #69682, #17554, #51755 ),
 ( #43898, #15900, #75845, #50100 ),
 ( #93176, #102661, #84227, #7527 ) ),
 .UNSPECIFIED., .F., .F., .F.,
 ( 6, 3, 3, 3, 3, 3, 3, 3, 3, 6 ),
 ( 4, 4 ),
 ( 0.000000000000000000, 15.39383910899999997, 27.58084801740000103, 41.39509552349999666, 65.53909258059999843, 90.91108773649999364, 117.6367619669999982, 132.4493970709999928, 144.8160795070000120, 161.8240513320000105 ),
 ( 0.000000000000000000, 2.092690777440000094 ),
 .UNSPECIFIED. ) ;
#84871 = AXIS2_PLACEMENT_3D ( 'NONE', #101701, #401, #67594 ) ;
#84872 = ORIENTED_EDGE ( 'NONE', *, *, #48120, .F. ) ;
#84873 = EDGE_LOOP ( 'NONE', ( #70486, #109680, #27748, #94117 ) ) ;
#84874 = CARTESIAN_POINT ( 'NONE',  ( 5.027021143375445256, 1422.868624059190324, 184.4318487489844642 ) ) ;
#84875 = CARTESIAN_POINT ( 'NONE',  ( 5.178343518078389884, 1424.209805733240046, 193.3007077610879776 ) ) ;
#84876 = AXIS2_PLACEMENT_3D ( 'NONE', #35368, #102546, #60040 ) ;
#84877 = CARTESIAN_POINT ( 'NONE',  ( 1.712644716155000024, 1516.636036526019780, 214.1174694231270053 ) ) ;
#84878 = CARTESIAN_POINT ( 'NONE',  ( 5.385523161694999672, 1511.435001052829875, 217.7746220723570048 ) ) ;
#84879 = CARTESIAN_POINT ( 'NONE',  ( -17.31871724090759912, 1489.038281045860003, 229.1406144452789988 ) ) ;
#84880 = B_SPLINE_SURFACE_WITH_KNOTS ( 'NONE', 5, 1, ( 
 ( #95984, #77536 ),
 ( #45061, #19249 ),
 ( #60757, #2510 ),
 ( #52355, #79204 ),
 ( #95438, #62418 ),
 ( #104384, #96544 ),
 ( #86472, #87600 ),
 ( #18157, #78636 ),
 ( #52898, #103834 ) ),
 .UNSPECIFIED., .F., .F., .F.,
 ( 6, 3, 6 ),
 ( 2, 2 ),
 ( 0.7097524320850000512, 4.064565650359999616, 10.06422694349720004 ),
 ( -13.51875974050000018, -1.265881781690000096 ),
 .UNSPECIFIED. ) ;
#84881 = VERTEX_POINT ( 'NONE', #32734 ) ;
#84882 = CARTESIAN_POINT ( 'NONE',  ( -105.7140364039999980, 1374.461008904089795, 303.4364470169589936 ) ) ;
#84883 = B_SPLINE_CURVE_WITH_KNOTS ( 'NONE', 5,
 ( #89375, #44632, #2641, #87740, #80431, #12667, #69846, #19391, #106176, #53034, #104521, #1523, #103964, #78211, #11018 ),
 .UNSPECIFIED., .F., .F.,
 ( 6, 3, 3, 3, 6 ),
 ( 0.000000000000000000, 0.1200066420014513496, 0.2400132840077169871, 0.4800265680154341408, 1.000000000000000000 ),
 .UNSPECIFIED. ) ;
#84884 = EDGE_CURVE ( 'NONE', #24269, #5750, #91049, .T. ) ;
#84885 = CARTESIAN_POINT ( 'NONE',  ( 3.259101798884999734, 1517.102359858469754, 202.1722709844570147 ) ) ;
#84886 = B_SPLINE_CURVE_WITH_KNOTS ( 'NONE', 3,
 ( #102668, #25967, #60166, #94284, #51763, #58506, #23770, #92090, #67030, #102253, #100596, #7645 ),
 .UNSPECIFIED., .F., .F.,
 ( 4, 2, 2, 2, 2, 4 ),
 ( 0.000000000000000000, 0.0007194225121792683416, 0.001079133768269217473, 0.001438845024359166388, 0.002158267536539043834, 0.002877690048718921281 ),
 .UNSPECIFIED. ) ;
#84887 = CARTESIAN_POINT ( 'NONE',  ( -27.96811930129999979, 1509.876319213429952, 202.1748059118680203 ) ) ;
#84888 = B_SPLINE_SURFACE_WITH_KNOTS ( 'NONE', 4, 5, ( 
 ( #49307, #21853, #13459, #47106, #38681, #40885 ),
 ( #56602, #12926, #100250, #106450, #4548, #106991 ),
 ( #65007, #48210, #81232, #72857, #66128, #99123 ),
 ( #5648, #22402, #30280, #47649, #14576, #14019 ),
 ( #64473, #31381, #98588, #108086, #63919, #82348 ) ),
 .UNSPECIFIED., .F., .F., .F.,
 ( 5, 5 ),
 ( 6, 6 ),
 ( 6.621488669309999686, 17.01656664660000118 ),
 ( -5.551115123129999410E-17, 1.000000000000000000 ),
 .UNSPECIFIED. ) ;
#84889 = CARTESIAN_POINT ( 'NONE',  ( 10.11781796957937551, 1428.435797280887527, 134.0999999980966777 ) ) ;
#84890 = EDGE_CURVE ( 'NONE', #37235, #17035, #5223, .T. ) ;
#84891 = CARTESIAN_POINT ( 'NONE',  ( -36.31252284909629680, 1384.572199005869834, 209.7182559141370177 ) ) ;
#84892 = CARTESIAN_POINT ( 'NONE',  ( -1.303360707740000013, 1408.418417413329962, 195.5769302267979981 ) ) ;
#84894 = VERTEX_POINT ( 'NONE', #25966 ) ;
#84893 = CARTESIAN_POINT ( 'NONE',  ( 15.71383115701936006, 1506.606278687632539, 193.5425396900113810 ) ) ;
#84896 = EDGE_CURVE ( 'NONE', #43055, #64021, #92633, .T. ) ;
#84895 = CARTESIAN_POINT ( 'NONE',  ( 19.32263322520000060, 1455.378559704889767, 209.1218459616989946 ) ) ;
#84897 = CARTESIAN_POINT ( 'NONE',  ( 27.27473106160000071, 1488.690404413930082, 210.2221370544380079 ) ) ;
#84898 = CARTESIAN_POINT ( 'NONE',  ( -50.84265507320838395, 1379.695343721229619, 247.3880999093737216 ) ) ;
#84899 = CARTESIAN_POINT ( 'NONE',  ( 10.41177329615350011, 1460.024665156439823, 205.9063136364349873 ) ) ;
#84900 = CARTESIAN_POINT ( 'NONE',  ( -24.16964372749999868, 1435.415582199720120, 137.3389635753979974 ) ) ;
#84901 = CARTESIAN_POINT ( 'NONE',  ( -7.321169269124999879, 1516.531533746980131, 210.8305669548069829 ) ) ;
#84902 = CARTESIAN_POINT ( 'NONE',  ( -68.58568551959999127, 1379.747647795449893, 279.7303794029589881 ) ) ;
#84903 = CARTESIAN_POINT ( 'NONE',  ( -14.14317614989999861, 1413.182323360430019, 227.0405350710979633 ) ) ;
#84904 = CARTESIAN_POINT ( 'NONE',  ( -21.60894078472486868, 1521.951704408389787, 199.6722430288449175 ) ) ;
#84905 = VECTOR ( 'NONE', #69658, 1000.000000000000114 ) ;
#84906 = CARTESIAN_POINT ( 'NONE',  ( -0.007128875282218469743, 1517.006509894990131, 208.3750284165899984 ) ) ;
#84907 = ORIENTED_EDGE ( 'NONE', *, *, #87021, .T. ) ;
#84908 = CARTESIAN_POINT ( 'NONE',  ( -11.55783143579999894, 1415.365618343329970, 228.9844200364979940 ) ) ;
#84909 = CARTESIAN_POINT ( 'NONE',  ( -19.86712494847475341, 1456.673296078442945, 225.4261212115576427 ) ) ;
#84910 = EDGE_LOOP ( 'NONE', ( #44055, #43164, #62926, #100342 ) ) ;
#84911 = CARTESIAN_POINT ( 'NONE',  ( 7.358001737349999516, 1481.503913299690112, 209.0774419860809985 ) ) ;
#84912 = CARTESIAN_POINT ( 'NONE',  ( 12.76251288935960027, 1435.676538582969897, 150.7804224899010137 ) ) ;
#84913 = ADVANCED_FACE ( 'NONE', ( #67466 ), #24859, .T. ) ;
#84914 = CARTESIAN_POINT ( 'NONE',  ( -4.219438644781110526, 1441.595895916910195, 183.5288106640859951 ) ) ;
#84915 = AXIS2_PLACEMENT_3D ( 'NONE', #47593, #83380, #99619 ) ;
#84916 = CARTESIAN_POINT ( 'NONE',  ( -0.1613635714646410035, 1507.107001889669846, 180.9028745560509890 ) ) ;
#84917 = CARTESIAN_POINT ( 'NONE',  ( 21.39771952614790251, 1509.704955107219803, 188.4542851670070149 ) ) ;
#84918 = CARTESIAN_POINT ( 'NONE',  ( 3.689783165729999759, 1486.815214840489944, 198.5515965981990121 ) ) ;
#84919 = DIRECTION ( 'NONE',  ( 0.000000000000000000, 0.000000000000000000, -1.000000000000000000 ) ) ;
#84920 = CARTESIAN_POINT ( 'NONE',  ( 3.550311703873260096E-15, 1384.899971913130003, 209.1218459572589836 ) ) ;
#84922 = CARTESIAN_POINT ( 'NONE',  ( -1.842963721827329815, 1515.551704300040001, 205.2922259627210053 ) ) ;
#84921 = CARTESIAN_POINT ( 'NONE',  ( -2.480187054844999572, 1517.025470194390209, 213.7472054950769973 ) ) ;
#84923 = CARTESIAN_POINT ( 'NONE',  ( 20.65148255260000099, 1509.627424728229926, 188.0185848083980034 ) ) ;
#84924 = CARTESIAN_POINT ( 'NONE',  ( -3.260357166894999992, 1517.133889586189980, 216.8465783791270098 ) ) ;
#84925 = ORIENTED_EDGE ( 'NONE', *, *, #56186, .F. ) ;
#84926 = CARTESIAN_POINT ( 'NONE',  ( 7.720004413545239252, 1516.953334728320215, 209.1872673121889932 ) ) ;
#84927 = DIRECTION ( 'NONE',  ( 0.000000000000000000, 0.000000000000000000, -1.000000000000000000 ) ) ;
#84928 = ORIENTED_EDGE ( 'NONE', *, *, #8810, .F. ) ;
#84929 = CARTESIAN_POINT ( 'NONE',  ( -17.32162814183379851, 1508.551704408389924, 212.1341644048549995 ) ) ;
#84930 = CARTESIAN_POINT ( 'NONE',  ( 3.350338079455601026, 1523.604703353109699, 176.1628856388066708 ) ) ;
#84931 = UNCERTAINTY_MEASURE_WITH_UNIT (LENGTH_MEASURE( 1.000000000000000082E-05 ), #81981, 'distance_accuracy_value', 'NONE');
#84932 = LINE ( 'NONE', #100099, #84365 ) ;
#84933 = DIRECTION ( 'NONE',  ( -0.6736849260863841948, 0.000000000000000000, 0.7390186874254148774 ) ) ;
#84934 = CARTESIAN_POINT ( 'NONE',  ( -4.303904342535483707, 1508.176176452014033, 220.6005507373670014 ) ) ;
#84935 = B_SPLINE_CURVE_WITH_KNOTS ( 'NONE', 5,
 ( #73627, #34208, #31593, #85155, #42615, #68392 ),
 .UNSPECIFIED., .F., .F.,
 ( 6, 6 ),
 ( -157.9969979290000026, -29.50720980459999510 ),
 .UNSPECIFIED. ) ;
#84936 = CARTESIAN_POINT ( 'NONE',  ( 5.808294004517759568, 1494.502801637436960, 219.1507311820781752 ) ) ;
#84937 = CARTESIAN_POINT ( 'NONE',  ( 11.74015320060000001, 1428.979986575930070, 144.1938086916980239 ) ) ;
#84938 = FACE_OUTER_BOUND ( 'NONE', #48825, .T. ) ;
#84939 = CARTESIAN_POINT ( 'NONE',  ( 44.53839032258289876, 1440.913060367359776, 264.9617148667340416 ) ) ;
#84941 = CARTESIAN_POINT ( 'NONE',  ( 16.93884299705920071, 1507.634939766059915, 188.0954313100240256 ) ) ;
#84940 = CARTESIAN_POINT ( 'NONE',  ( -2.379179684863220068, 1422.184173668060112, 193.0946223031349689 ) ) ;
#84942 = CARTESIAN_POINT ( 'NONE',  ( 2.792392588003544507, 1524.382868172863937, 241.3440112565233449 ) ) ;
#84943 = EDGE_LOOP ( 'NONE', ( #64838, #32150, #93702, #91078 ) ) ;
#84944 = ORIENTED_EDGE ( 'NONE', *, *, #90350, .F. ) ;
#84945 = CARTESIAN_POINT ( 'NONE',  ( 28.27139721233048419, 1526.382868172863937, 219.5606225550385489 ) ) ;
#84946 = EDGE_CURVE ( 'NONE', #87917, #33774, #27807, .T. ) ;
#84947 = CARTESIAN_POINT ( 'NONE',  ( 16.91620036578183672, 1409.772676212749047, 192.7760182944116707 ) ) ;
#84948 = CARTESIAN_POINT ( 'NONE',  ( -28.20849547050000083, 1509.668627049429915, 211.1040453917479738 ) ) ;
#84949 = CARTESIAN_POINT ( 'NONE',  ( 1.123001734155827158, 1410.331803268985368, 185.2141170702371085 ) ) ;
#84950 = ADVANCED_FACE ( 'NONE', ( #7534 ), #65184, .T. ) ;
#84951 = CARTESIAN_POINT ( 'NONE',  ( -3.153913303612108532, 1425.996417847233033, 185.6247366075170646 ) ) ;
#84952 = CARTESIAN_POINT ( 'NONE',  ( 10.18770750727360053, 1422.434970378240223, 211.9211229168350030 ) ) ;
#84953 = CARTESIAN_POINT ( 'NONE',  ( 3.115880651068799967, 1508.551704408389924, 219.3718644903320012 ) ) ;
#84954 = CARTESIAN_POINT ( 'NONE',  ( -19.86464703721610192, 1441.435635517049832, 212.6459273959629854 ) ) ;
#84955 = CARTESIAN_POINT ( 'NONE',  ( -59.11443824985749984, 1383.797908678129943, 279.0809373516989922 ) ) ;
#84956 = CIRCLE ( 'NONE', #56381, 2.500000000000002220 ) ;
#84957 = CARTESIAN_POINT ( 'NONE',  ( -9.783936650027678539, 1438.409968310599879, 210.7790528106160082 ) ) ;
#84958 = CARTESIAN_POINT ( 'NONE',  ( 11.41815806276019885, 1492.743991988549851, 212.4766916504889878 ) ) ;
#84960 = EDGE_LOOP ( 'NONE', ( #67159, #13963, #62724, #61876 ) ) ;
#84959 = CARTESIAN_POINT ( 'NONE',  ( -2.288930271459999943, 1457.528235387290124, 219.1297011245989950 ) ) ;
#84961 = CARTESIAN_POINT ( 'NONE',  ( 31.74003925670048432, 1524.382868172804365, 216.5565202880893594 ) ) ;
#84962 = EDGE_CURVE ( 'NONE', #99871, #102807, #19221, .T. ) ;
#84963 = B_SPLINE_SURFACE_WITH_KNOTS ( 'NONE', 5, 5, ( 
 ( #65831, #4263, #56316, #90449, #38396, #107813, #64182, #13726, #55787 ),
 ( #31099, #40057, #74237, #108368, #20475, #54685, #88811, #72572, #106699 ),
 ( #12095, #89903, #13174, #77390, #94169, #1806, #43784, #41162, #44349 ),
 ( #60051, #103686, #693, #9614, #26415, #34271, #100511, #18554, #77934 ),
 ( #26987, #1241, #78492, #95292, #94730, #66392, #32211, #18008, #91567 ),
 ( #85774, #23790, #75337, #52747, #83710, #15390, #57979, #14843, #6460 ),
 ( #51637, #35378, #17439, #150, #23243, #49032, #52201, #86329, #68453 ),
 ( #9074, #86881, #10175, #57442, #103114, #43242, #92113, #35943, #99948 ),
 ( #69567, #34822, #61175, #69009, #74779, #60607, #40608, #25849, #83168 ) ),
 .UNSPECIFIED., .F., .F., .F.,
 ( 6, 3, 6 ),
 ( 6, 3, 6 ),
 ( 9.902195898180000455, 12.38020728900000123, 16.40090783169999966 ),
 ( 0.000000000000000000, 0.5000000000000000000, 1.000000000000000000 ),
 .UNSPECIFIED. ) ;
#84964 = CARTESIAN_POINT ( 'NONE',  ( -62.34512127969999540, 1383.170447440649923, 249.3521481918589870 ) ) ;
#84965 = CARTESIAN_POINT ( 'NONE',  ( 32.38845791999495560, 1512.187213306747481, 202.1182848005512085 ) ) ;
#84966 = VERTEX_POINT ( 'NONE', #97617 ) ;
#84967 = EDGE_LOOP ( 'NONE', ( #16304, #2431, #34886, #13979 ) ) ;
#84968 = DIRECTION ( 'NONE',  ( 1.000000000000000000, 0.000000000000000000, 0.000000000000000000 ) ) ;
#84969 = CARTESIAN_POINT ( 'NONE',  ( 29.65946186579095922, 1526.335487865669393, 201.2508909606647478 ) ) ;
#84970 = CARTESIAN_POINT ( 'NONE',  ( 37.95268740653450124, 1438.587537029340183, 136.6052002288919880 ) ) ;
#84972 = CARTESIAN_POINT ( 'NONE',  ( 31.34137657934008558, 1523.382868172864164, 196.3411265156547358 ) ) ;
#84971 = CARTESIAN_POINT ( 'NONE',  ( -11.43185072513739797, 1443.913060387330006, 147.9056598087979921 ) ) ;
#84973 = CARTESIAN_POINT ( 'NONE',  ( -7.459107715590000076, 1463.395188125190089, 202.0447620364989803 ) ) ;
#84974 = CARTESIAN_POINT ( 'NONE',  ( -108.4073513729999974, 1382.402421960810216, 297.8403850943590214 ) ) ;
#84975 = CARTESIAN_POINT ( 'NONE',  ( 11.36216713388179933, 1503.110266152410077, 211.0233809544849919 ) ) ;
#84976 = CARTESIAN_POINT ( 'NONE',  ( -11.91658583868719923, 1508.551704408389924, 217.2927667623789887 ) ) ;
#84977 = ADVANCED_FACE ( 'NONE', ( #37163 ), #24924, .F. ) ;
#84978 = CARTESIAN_POINT ( 'NONE',  ( 4.533938656610000173, 1410.006645354029843, 186.2297118026980058 ) ) ;
#84979 = CARTESIAN_POINT ( 'NONE',  ( 4.304887325260000175, 1424.164641267230081, 184.8345661179979800 ) ) ;
#84980 = CARTESIAN_POINT ( 'NONE',  ( 2.301917092608350313, 1432.768594694289959, 200.9374038220679779 ) ) ;
#84981 = CARTESIAN_POINT ( 'NONE',  ( -1.906460855849449881E-08, 1515.051704408389924, 204.7920544413669859 ) ) ;
#84982 = CARTESIAN_POINT ( 'NONE',  ( -25.25200564400000047, 1450.804212513650100, 137.6134969548979825 ) ) ;
#84983 = CARTESIAN_POINT ( 'NONE',  ( 1.440267586269999844, 1465.218598317130272, 235.8491212012980043 ) ) ;
#84984 = VERTEX_POINT ( 'NONE', #2487 ) ;
#84985 = EDGE_CURVE ( 'NONE', #100850, #86349, #49987, .T. ) ;
#84986 = CARTESIAN_POINT ( 'NONE',  ( 4.967313642998160361, 1470.582637015879982, 187.7810769942950060 ) ) ;
#84987 = CARTESIAN_POINT ( 'NONE',  ( 12.19431714289060587, 1509.463056330486779, 236.6448779725608347 ) ) ;
#84988 = PLANE ( 'NONE',  #83834 ) ;
#84989 = CARTESIAN_POINT ( 'NONE',  ( 21.13431379670319998, 1409.651086887829933, 206.4149708788170301 ) ) ;
#84990 = ADVANCED_FACE ( 'NONE', ( #104918 ), #38248, .F. ) ;
#84991 = CARTESIAN_POINT ( 'NONE',  ( 14.68671602690000100, 1430.156356569229956, 190.6741761820979946 ) ) ;
#84992 = CARTESIAN_POINT ( 'NONE',  ( -7.471909415769559706E-09, 1475.245055346789968, 265.8384215023410206 ) ) ;
#84993 = CARTESIAN_POINT ( 'NONE',  ( 23.91303816115560466, 1436.560782071131371, 140.3770785067727616 ) ) ;
#84994 = CARTESIAN_POINT ( 'NONE',  ( -1.546949757679999760, 1416.828040475729949, 228.0209010782980101 ) ) ;
#84995 = CARTESIAN_POINT ( 'NONE',  ( -1.630423233649999970, 1417.460556004529963, 234.9148393419980039 ) ) ;
#84996 = CARTESIAN_POINT ( 'NONE',  ( -2.737226383349999903, 1476.451468402690125, 199.1237168845889869 ) ) ;
#84997 = CARTESIAN_POINT ( 'NONE',  ( -107.5745933759999957, 1387.689086384770007, 310.1919576522590205 ) ) ;
#84998 = VECTOR ( 'NONE', #86285, 1000.000000000000000 ) ;
#84999 = CARTESIAN_POINT ( 'NONE',  ( -0.5298339765193601503, 1485.566302121303579, 181.9011267176622084 ) ) ;
#85000 = CARTESIAN_POINT ( 'NONE',  ( -3.982247585420000124, 1360.759224656429978, 207.6218459616989946 ) ) ;
#85001 = CARTESIAN_POINT ( 'NONE',  ( -45.80615043228049643, 1438.856719389719956, 266.4146728030800091 ) ) ;
#85002 = CARTESIAN_POINT ( 'NONE',  ( 14.03164605154790223, 1509.388572056619978, 234.6445892514809941 ) ) ;
#85003 = CARTESIAN_POINT ( 'NONE',  ( -8.112741595579999299, 1424.858451744329841, 208.8832813207109780 ) ) ;
#85004 = EDGE_CURVE ( 'NONE', #22042, #24522, #65313, .T. ) ;
#85005 = ORIENTED_EDGE ( 'NONE', *, *, #4126, .F. ) ;
#85006 = CARTESIAN_POINT ( 'NONE',  ( 1.127928333405000094, 1516.989863902050047, 209.1117210464550169 ) ) ;
#85007 = FACE_BOUND ( 'NONE', #55994, .T. ) ;
#85008 = B_SPLINE_SURFACE_WITH_KNOTS ( 'NONE', 5, 1, ( 
 ( #96468, #46635 ),
 ( #19173, #79133 ),
 ( #37659, #46085 ),
 ( #86955, #29258 ),
 ( #79682, #95365 ),
 ( #70753, #62343 ),
 ( #36015, #105982 ),
 ( #20840, #97568 ),
 ( #71306, #3534 ) ),
 .UNSPECIFIED., .F., .F., .F.,
 ( 6, 3, 6 ),
 ( 2, 2 ),
 ( 0.000000000000000000, 5.782490304330000441, 11.25975508159999983 ),
 ( -1.500000000000000000, 1.500000000000000000 ),
 .UNSPECIFIED. ) ;
#85009 = CARTESIAN_POINT ( 'NONE',  ( -26.87832471722010297, 1441.334257773779882, 137.4807412269939846 ) ) ;
#85010 = CARTESIAN_POINT ( 'NONE',  ( 7.279817883549699609, 1426.451502940120008, 212.8375798222039919 ) ) ;
#85011 = ADVANCED_FACE ( 'NONE', ( #83014 ), #57832, .F. ) ;
#85012 = CARTESIAN_POINT ( 'NONE',  ( -26.26714492849760063, 1451.099761601440150, 136.4712888930870065 ) ) ;
#85013 = VERTEX_POINT ( 'NONE', #107109 ) ;
#85014 = CARTESIAN_POINT ( 'NONE',  ( 25.86260026069999896, 1440.913060418369923, 221.4996202440979971 ) ) ;
#85016 = CARTESIAN_POINT ( 'NONE',  ( -15.29028528244239915, 1512.571279492540043, 222.4326579091490146 ) ) ;
#85015 = CARTESIAN_POINT ( 'NONE',  ( -3.143095077906852719, 1525.137881624898682, 176.7009515179215668 ) ) ;
#85017 =( BOUNDED_SURFACE ( )  B_SPLINE_SURFACE ( 1, 2, ( 
 ( #58549, #7576, #41731 ),
 ( #50154, #77002, #45627 ) ),
 .UNSPECIFIED., .F., .F., .F. ) 
 B_SPLINE_SURFACE_WITH_KNOTS ( ( 2, 2 ),
 ( 3, 3 ),
 ( -10000.00000000000000, 10000.00000000000000 ),
 ( 5.770213224421889997, 5.870145916345279602 ),
 .UNSPECIFIED. ) 
 GEOMETRIC_REPRESENTATION_ITEM ( )  RATIONAL_B_SPLINE_SURFACE ( (
 ( 0.8711730262222420196, 0.8776363487315159695, 0.8864705793990830252),
 ( 0.8711730262222420196, 0.8776363487315159695, 0.8864705793990830252) ) ) 
 REPRESENTATION_ITEM ( '' )  SURFACE ( )  );
#85018 = CARTESIAN_POINT ( 'NONE',  ( 3.203789175851970288E-09, 1424.294192408320214, 227.6053815985079893 ) ) ;
#85019 = CARTESIAN_POINT ( 'NONE',  ( -24.04315183071442519, 1445.026065455099797, 213.4541038297220439 ) ) ;
#85020 = CARTESIAN_POINT ( 'NONE',  ( 4.811281351129999884, 1423.102872354400233, 207.5441001112789934 ) ) ;
#85021 = CARTESIAN_POINT ( 'NONE',  ( 16.73628186595824019, 1526.382868172863937, 184.0591879540915272 ) ) ;
#85022 = EDGE_CURVE ( 'NONE', #44794, #105370, #50628, .T. ) ;
#85023 = DIRECTION ( 'NONE',  ( -0.9786619618251634067, 0.000000000000000000, -0.2054769195713292418 ) ) ;
#85024 = ORIENTED_EDGE ( 'NONE', *, *, #47341, .T. ) ;
#85025 = CARTESIAN_POINT ( 'NONE',  ( -3.003389061728070075, 1410.104144440540040, 269.8660872768579679 ) ) ;
#85026 = CARTESIAN_POINT ( 'NONE',  ( 10.71406017268189892, 1419.905362405259893, 231.5852711379240247 ) ) ;
#85027 = CARTESIAN_POINT ( 'NONE',  ( 9.401681046103311346, 1434.490268153120041, 206.4448289074559852 ) ) ;
#85028 = ORIENTED_EDGE ( 'NONE', *, *, #31550, .F. ) ;
#85029 = ORIENTED_EDGE ( 'NONE', *, *, #70207, .T. ) ;
#85030 = EDGE_CURVE ( 'NONE', #109826, #79273, #95686, .T. ) ;
#85031 = CARTESIAN_POINT ( 'NONE',  ( -23.69647183529550105, 1410.728790039680007, 210.2360925051529819 ) ) ;
#85032 = CARTESIAN_POINT ( 'NONE',  ( -11.87328627558470018, 1482.014094172719979, 208.6022272904490080 ) ) ;
#85033 = CARTESIAN_POINT ( 'NONE',  ( -109.9849726248329915, 1384.916895159399928, 311.4561123681800154 ) ) ;
#85034 = CARTESIAN_POINT ( 'NONE',  ( -11.30500403589999792, 1428.976642997429963, 112.4493539157979995 ) ) ;
#85035 = EDGE_CURVE ( 'NONE', #48892, #85148, #107919, .T. ) ;
#85036 = CARTESIAN_POINT ( 'NONE',  ( -18.66712256547790005, 1432.215067861279977, 194.5764810006290020 ) ) ;
#85037 = CARTESIAN_POINT ( 'NONE',  ( 3.961944270670380241, 1508.551704410290085, 213.6667069116419952 ) ) ;
#85038 = CARTESIAN_POINT ( 'NONE',  ( 36.73751017938760555, 1461.736580476300105, 266.4401257845650548 ) ) ;
#85039 = VECTOR ( 'NONE', #8282, 1000.000000000000000 ) ;
#85040 = CARTESIAN_POINT ( 'NONE',  ( -4.236980942262600358, 1508.610336716400070, 204.5878351888970030 ) ) ;
#85041 = CARTESIAN_POINT ( 'NONE',  ( -16.30652261508721423, 1421.098027771803800, 227.0172576140167848 ) ) ;
#85042 = CARTESIAN_POINT ( 'NONE',  ( -2.879642191334999879, 1516.812046502680005, 205.6755161564470313 ) ) ;
#85043 = ORIENTED_EDGE ( 'NONE', *, *, #46053, .F. ) ;
#85044 = CARTESIAN_POINT ( 'NONE',  ( 18.97915715501314793, 1457.436128530311407, 226.6750837173330240 ) ) ;
#85045 = CARTESIAN_POINT ( 'NONE',  ( 15.25688964212639931, 1512.464953430890091, 195.9853556598569924 ) ) ;
#85046 = CARTESIAN_POINT ( 'NONE',  ( 16.48525259900869955, 1431.535382936039923, 217.4038343007140099 ) ) ;
#85047 = ORIENTED_EDGE ( 'NONE', *, *, #59839, .T. ) ;
#85048 = CARTESIAN_POINT ( 'NONE',  ( 4.487249066482500659, 1509.038643261319976, 206.6339218291419968 ) ) ;
#85049 = CARTESIAN_POINT ( 'NONE',  ( 5.866456971857230585, 1434.780192336125992, 202.9178924053972253 ) ) ;
#85050 = CARTESIAN_POINT ( 'NONE',  ( -4.932890325499830197, 1508.551704408389924, 212.1343244586070114 ) ) ;
#85051 = CARTESIAN_POINT ( 'NONE',  ( -1.544830625875079910, 1421.730119690919992, 228.2386301722320070 ) ) ;
#85052 = CARTESIAN_POINT ( 'NONE',  ( 7.345629923129999739, 1422.263538441430001, 195.5717800564989943 ) ) ;
#85053 = CARTESIAN_POINT ( 'NONE',  ( -2.901039365278310189, 1433.100862733600252, 218.2186568973889962 ) ) ;
#85054 = CARTESIAN_POINT ( 'NONE',  ( 17.22592482065188335, 1443.913060387329779, 162.9227486220069352 ) ) ;
#85055 = CARTESIAN_POINT ( 'NONE',  ( 1.014329838393059902, 1408.948481565789962, 186.6702704748330177 ) ) ;
#85057 = LINE ( 'NONE', #101288, #84830 ) ;
#85056 = CARTESIAN_POINT ( 'NONE',  ( 1.220948355079999992, 1416.360244924329891, 233.1251597269979925 ) ) ;
#85058 = CARTESIAN_POINT ( 'NONE',  ( 12.86744022639999940, 1409.362401301430054, 227.0135731152979872 ) ) ;
#85059 = CARTESIAN_POINT ( 'NONE',  ( -13.71395948329999825, 1379.587229639339967, 211.8543337660190105 ) ) ;
#85060 = CARTESIAN_POINT ( 'NONE',  ( 2.570808432944288846, 1525.317359687841190, 241.4588331507368650 ) ) ;
#85061 = ORIENTED_EDGE ( 'NONE', *, *, #20027, .T. ) ;
#85062 = CARTESIAN_POINT ( 'NONE',  ( -32.23393008293517425, 1523.462669333491021, 201.4036600224246740 ) ) ;
#85063 = CARTESIAN_POINT ( 'NONE',  ( 11.81416765884010012, 1432.336398938299908, 150.4603274062260141 ) ) ;
#85064 = CARTESIAN_POINT ( 'NONE',  ( 31.63978151511877357, 1525.343710797494396, 202.0582079856336577 ) ) ;
#85065 = ADVANCED_FACE ( 'NONE', ( #102956 ), #24185, .T. ) ;
#85066 = AXIS2_PLACEMENT_3D ( 'NONE', #82898, #13467, #47112 ) ;
#85067 = CARTESIAN_POINT ( 'NONE',  ( -12.29063212139999983, 1392.314905091580158, 209.7402030487879756 ) ) ;
#85068 = CARTESIAN_POINT ( 'NONE',  ( 8.758531138563899532, 1427.348527690079891, 211.4847147330029884 ) ) ;
#85069 = CARTESIAN_POINT ( 'NONE',  ( 1.598766419041605991, 1421.472867901786003, 193.7976631032935870 ) ) ;
#85070 = DIRECTION ( 'NONE',  ( 0.000000000000000000, -6.123233995736769734E-17, -1.000000000000000000 ) ) ;
#85071 = CARTESIAN_POINT ( 'NONE',  ( -10.04572263370000051, 1464.202968133530021, 255.3819207742980097 ) ) ;
#85072 = CARTESIAN_POINT ( 'NONE',  ( -21.03123196678649975, 1507.789098018889945, 192.1781278620359785 ) ) ;
#85073 = CARTESIAN_POINT ( 'NONE',  ( 11.91160370939999957, 1433.398298247449929, 150.1562357106980130 ) ) ;
#85074 = CARTESIAN_POINT ( 'NONE',  ( 4.540901341789999712, 1462.614442898930065, 248.0989693021979861 ) ) ;
#85075 = CARTESIAN_POINT ( 'NONE',  ( 12.87618670774100060, 1416.835419214280137, 196.3099906520550064 ) ) ;
#85076 = AXIS2_PLACEMENT_3D ( 'NONE', #64862, #81075, #106820 ) ;
#85077 = CARTESIAN_POINT ( 'NONE',  ( -16.83242346257729949, 1420.442304662440165, 203.3407665278299703 ) ) ;
#85078 = CARTESIAN_POINT ( 'NONE',  ( -17.17241001986462123, 1512.187213306747481, 237.6251415217917895 ) ) ;
#85079 = CARTESIAN_POINT ( 'NONE',  ( 7.695203452936191013, 1464.811393429670034, 216.0057213840310055 ) ) ;
#85080 = EDGE_CURVE ( 'NONE', #4206, #36027, #51758, .T. ) ;
#85081 = DIRECTION ( 'NONE',  ( -0.9996573249755689172, 0.02617694830742899742, -1.602875797806941519E-18 ) ) ;
#85082 = B_SPLINE_CURVE_WITH_KNOTS ( 'NONE', 5,
 ( #49291, #100757, #48190, #107522, #22947, #30813 ),
 .UNSPECIFIED., .F., .F.,
 ( 6, 6 ),
 ( 302.8993106099999864, 307.9376145470000097 ),
 .UNSPECIFIED. ) ;
#85083 = CARTESIAN_POINT ( 'NONE',  ( 12.78677686703885996, 1398.292081298729045, 206.7702702667238555 ) ) ;
#85084 = CARTESIAN_POINT ( 'NONE',  ( -7.510707159466901039, 1509.188756966919982, 238.7243973511239972 ) ) ;
#85085 = CARTESIAN_POINT ( 'NONE',  ( 24.18568768079999742, 1430.355574605830043, 212.4850587644480129 ) ) ;
#85086 = CARTESIAN_POINT ( 'NONE',  ( 0.1128880363801176290, 1477.705586754096430, 198.7092162523474599 ) ) ;
#85087 = DIRECTION ( 'NONE',  ( 1.755985294532469921E-16, -1.000000000000000000, 1.338183447452831989E-16 ) ) ;
#85088 = CARTESIAN_POINT ( 'NONE',  ( -12.38799748877169904, 1383.860969130600097, 218.8265414708790217 ) ) ;
#85089 = CARTESIAN_POINT ( 'NONE',  ( 12.73796549575709847, 1426.755042289380071, 204.5610647559049937 ) ) ;
#85090 = CARTESIAN_POINT ( 'NONE',  ( -5.221955725866830100, 1489.269540765400052, 185.8916489472570106 ) ) ;
#85091 = CARTESIAN_POINT ( 'NONE',  ( 5.785582913545000316, 1516.981965530290154, 213.1542438721070027 ) ) ;
#85092 = B_SPLINE_CURVE_WITH_KNOTS ( 'NONE', 3,
 ( #95743, #60507, #55833, #78395 ),
 .UNSPECIFIED., .F., .F.,
 ( 4, 4 ),
 ( 0.000000000000000000, 1.000000000000000000 ),
 .UNSPECIFIED. ) ;
#85093 = CARTESIAN_POINT ( 'NONE',  ( -12.46613533405179908, 1422.637669668850094, 203.9783536675730033 ) ) ;
#85094 = CARTESIAN_POINT ( 'NONE',  ( 0.2056537491783179961, 1459.797042805989804, 182.9617855128460064 ) ) ;
#85096 = ORIENTED_EDGE ( 'NONE', *, *, #9303, .T. ) ;
#85095 = CARTESIAN_POINT ( 'NONE',  ( -2.822331109926550230, 1407.946699431110119, 222.3121693578910083 ) ) ;
#85097 = CARTESIAN_POINT ( 'NONE',  ( -13.35741048202589809, 1443.913060387329324, 164.9741927960640453 ) ) ;
#85098 = B_SPLINE_CURVE_WITH_KNOTS ( 'NONE', 3,
 ( #99542, #34006, #31802, #41859, #82761, #84947, #42407, #83857, #66542, #14983 ),
 .UNSPECIFIED., .F., .F.,
 ( 4, 2, 2, 2, 4 ),
 ( 0.000000000000000000, 0.2500000000000000000, 0.5000000000000000000, 0.7500000000000000000, 1.000000000000000000 ),
 .UNSPECIFIED. ) ;
#85099 = EDGE_CURVE ( 'NONE', #98856, #61659, #17281, .T. ) ;
#85100 = CARTESIAN_POINT ( 'NONE',  ( 23.59335433453006559, 1517.051704408389924, 208.3625261891680793 ) ) ;
#85101 = CARTESIAN_POINT ( 'NONE',  ( 13.50072690200000025, 1434.968958840149980, 149.8854961322979875 ) ) ;
#85102 = CARTESIAN_POINT ( 'NONE',  ( -40.14707100610610269, 1448.397814784289949, 134.0999999982449822 ) ) ;
#85103 = CARTESIAN_POINT ( 'NONE',  ( -109.3502800569999920, 1384.878668106390023, 297.1387558422589450 ) ) ;
#85104 = ORIENTED_EDGE ( 'NONE', *, *, #14108, .T. ) ;
#85105 = CARTESIAN_POINT ( 'NONE',  ( -5.858855997865759946, 1391.912605642699873, 203.1598715823440102 ) ) ;
#85106 = CYLINDRICAL_SURFACE ( 'NONE', #108236, 1.455175085939995450 ) ;
#85107 = CARTESIAN_POINT ( 'NONE',  ( -16.09868638649999895, 1415.425582719929707, 216.6834975185180099 ) ) ;
#85108 = EDGE_CURVE ( 'NONE', #31779, #63901, #73241, .T. ) ;
#85109 = B_SPLINE_CURVE_WITH_KNOTS ( 'NONE', 3,
 ( #8723, #42903, #77060, #34493, #23863, #102771, #60259, #83241, #40686, #74859 ),
 .UNSPECIFIED., .F., .F.,
 ( 4, 2, 2, 2, 4 ),
 ( 3.469446951953614189E-18, 0.0007403986298595378662, 0.001480797259719072263, 0.002221195889578606551, 0.002961594519438141056 ),
 .UNSPECIFIED. ) ;
#85110 = CARTESIAN_POINT ( 'NONE',  ( -3.967003077310200077, 1433.325234434820004, 217.0778631506990166 ) ) ;
#85111 = CARTESIAN_POINT ( 'NONE',  ( -25.62237252300000279, 1435.677407238350042, 212.3102753037179866 ) ) ;
#85112 = CARTESIAN_POINT ( 'NONE',  ( -16.20017219800000063, 1416.460102861859923, 208.9420928254820069 ) ) ;
#85113 = CARTESIAN_POINT ( 'NONE',  ( -22.57319772750419773, 1409.701314710050156, 209.4509374963450057 ) ) ;
#85114 = CARTESIAN_POINT ( 'NONE',  ( -11.07587008949999863, 1391.913060426370066, 205.3995214137289906 ) ) ;
#85115 = CARTESIAN_POINT ( 'NONE',  ( -73.07129608938419096, 1385.127337429350064, 271.9867951422679653 ) ) ;
#85116 = CARTESIAN_POINT ( 'NONE',  ( -10.28246376656830030, 1391.913060387289988, 213.9844737885490247 ) ) ;
#85117 = CARTESIAN_POINT ( 'NONE',  ( 10.17807908018379770, 1423.278369623310027, 208.7639352597529978 ) ) ;
#85118 = ORIENTED_EDGE ( 'NONE', *, *, #28769, .T. ) ;
#85119 = CARTESIAN_POINT ( 'NONE',  ( -29.80701679760000289, 1450.584075178780267, 136.3662129318980192 ) ) ;
#85120 = CARTESIAN_POINT ( 'NONE',  ( -15.69056619607619929, 1410.711084544529967, 226.7224086681349888 ) ) ;
#85121 = AXIS2_PLACEMENT_3D ( 'NONE', #74391, #21170, #43194 ) ;
#85123 = ORIENTED_EDGE ( 'NONE', *, *, #33786, .T. ) ;
#85122 = CARTESIAN_POINT ( 'NONE',  ( 8.598096571001718758, 1427.995879741943554, 134.0999999980979567 ) ) ;
#85124 = CARTESIAN_POINT ( 'NONE',  ( 2.587119683470000098, 1473.233209539489962, 219.0154824371090001 ) ) ;
#85125 = CARTESIAN_POINT ( 'NONE',  ( 5.871367194876985884, 1422.630051726727743, 194.8466533618984897 ) ) ;
#85126 = CARTESIAN_POINT ( 'NONE',  ( -7.592149787973779596, 1361.964468435450044, 210.6218459616987957 ) ) ;
#85127 = FACE_OUTER_BOUND ( 'NONE', #40449, .T. ) ;
#85128 = EDGE_CURVE ( 'NONE', #22898, #8871, #101824, .T. ) ;
#85129 = CARTESIAN_POINT ( 'NONE',  ( 41.26946182738182500, 1446.774783179103224, 269.6336529072985400 ) ) ;
#85130 = CARTESIAN_POINT ( 'NONE',  ( 22.12673984907599944, 1409.685743169220132, 208.3470065775269973 ) ) ;
#85131 = CARTESIAN_POINT ( 'NONE',  ( 14.45242834458300862, 1430.060838702070441, 220.7992783074957401 ) ) ;
#85132 = CARTESIAN_POINT ( 'NONE',  ( 9079.130222195200986, 5181.793945261120825, 1985.491949542980137 ) ) ;
#85133 = CARTESIAN_POINT ( 'NONE',  ( 8.789267444210000946, 1449.799573326989957, 205.7427481119990205 ) ) ;
#85134 = CARTESIAN_POINT ( 'NONE',  ( -119.3423021147299607, 1306.483669372790018, 300.9755515165832662 ) ) ;
#85135 = EDGE_CURVE ( 'NONE', #60389, #8432, #543, .T. ) ;
#85136 = CARTESIAN_POINT ( 'NONE',  ( -7.811405798920000088, 1367.739269854440181, 207.6218459616989946 ) ) ;
#85137 = CARTESIAN_POINT ( 'NONE',  ( -29.33952678943212433, 1526.382868172864164, 217.1408869592854671 ) ) ;
#85138 = EDGE_CURVE ( 'NONE', #41237, #13558, #100068, .T. ) ;
#85139 = CARTESIAN_POINT ( 'NONE',  ( 6.546951682585000043, 1516.606339319019980, 206.2472570094369928 ) ) ;
#85140 = CARTESIAN_POINT ( 'NONE',  ( 3.654206554840000010, 1446.297061077269973, 167.4573428069980139 ) ) ;
#85141 = CARTESIAN_POINT ( 'NONE',  ( -31.63978151511851777, 1525.343710797494396, 216.1854839377624842 ) ) ;
#85142 = CARTESIAN_POINT ( 'NONE',  ( -1.954686510389999965, 1496.240076336090169, 197.3202119613989964 ) ) ;
#85144 = ORIENTED_EDGE ( 'NONE', *, *, #58223, .T. ) ;
#85143 = CARTESIAN_POINT ( 'NONE',  ( -0.1165868996460010104, 1494.887927287289813, 220.3098612586990157 ) ) ;
#85145 = EDGE_CURVE ( 'NONE', #91418, #105869, #9179, .T. ) ;
#85146 = CIRCLE ( 'NONE', #99449, 3.500000000000003109 ) ;
#85147 = CARTESIAN_POINT ( 'NONE',  ( 3.055333763765900386E-13, 1547.913060387330006, 209.1218459616979999 ) ) ;
#85148 = VERTEX_POINT ( 'NONE', #69963 ) ;
#85149 = DIRECTION ( 'NONE',  ( 1.000000000000000000, 0.000000000000000000, 0.000000000000000000 ) ) ;
#85150 = CARTESIAN_POINT ( 'NONE',  ( -23.95220588849999999, 1410.918936088230112, 208.0890925629879860 ) ) ;
#85152 = CARTESIAN_POINT ( 'NONE',  ( 17.08463325386040310, 1410.592669789649790, 192.1150242963900325 ) ) ;
#85151 = CARTESIAN_POINT ( 'NONE',  ( -10.59742304113489908, 1425.359664718739850, 108.4540387853830055 ) ) ;
#85153 = CARTESIAN_POINT ( 'NONE',  ( -4.026614517785000125, 1516.699825673279975, 210.8361802174170236 ) ) ;
#85154 = CARTESIAN_POINT ( 'NONE',  ( 28.52891198672809736, 1510.020576512638172, 199.8347506128769169 ) ) ;
#85155 = CARTESIAN_POINT ( 'NONE',  ( 1.532290126919999995, 1453.146242306529984, 188.6114051259980045 ) ) ;
#85156 = CARTESIAN_POINT ( 'NONE',  ( -11.73700276120000119, 1426.696009609329849, 144.1682878321979899 ) ) ;
#85157 = CARTESIAN_POINT ( 'NONE',  ( -13.44717672499990080, 1379.564256771150212, 208.3953959236740161 ) ) ;
#85158 = CARTESIAN_POINT ( 'NONE',  ( 12.75179305369680804, 1463.394816282316242, 231.2017325377458405 ) ) ;
#85159 = SHAPE_DEFINITION_REPRESENTATION ( #72391, #110199 ) ;
#85160 = CARTESIAN_POINT ( 'NONE',  ( 2.927652146237840203, 1508.551704408389924, 214.0699139930379715 ) ) ;
#85161 = CARTESIAN_POINT ( 'NONE',  ( -34.83764231434859937, 1437.110286233230227, 136.5404629688219984 ) ) ;
#85162 = ORIENTED_EDGE ( 'NONE', *, *, #55850, .F. ) ;
#85163 = CARTESIAN_POINT ( 'NONE',  ( 8.897827345618869899, 1398.177211024679991, 219.0743639419499971 ) ) ;
#85164 = CARTESIAN_POINT ( 'NONE',  ( 10.92858942872100059, 1460.889019201350038, 208.5050433691779972 ) ) ;
#85165 = ADVANCED_FACE ( 'NONE', ( #104077 ), #32614, .T. ) ;
#85166 = CARTESIAN_POINT ( 'NONE',  ( 38.10537780832439836, 1442.926987427690165, 137.1117395883970005 ) ) ;
#85167 = ORIENTED_EDGE ( 'NONE', *, *, #62384, .F. ) ;
#85168 = ORIENTED_EDGE ( 'NONE', *, *, #65995, .F. ) ;
#85169 = CARTESIAN_POINT ( 'NONE',  ( -0.5481912525510364009, 1370.039449668079669, 211.2584053860457232 ) ) ;
#85170 = CARTESIAN_POINT ( 'NONE',  ( 9.018703368920000685, 1425.148033156689962, 195.5914714850989924 ) ) ;
#85171 = CARTESIAN_POINT ( 'NONE',  ( -14.18336309970609932, 1380.133888219859955, 210.8530608805870088 ) ) ;
#85172 = CARTESIAN_POINT ( 'NONE',  ( -13.71322468297814723, 1416.698495194484849, 202.0650518266237725 ) ) ;
#85173 = EDGE_CURVE ( 'NONE', #96209, #89343, #44640, .T. ) ;
#85174 = CARTESIAN_POINT ( 'NONE',  ( 4.123250153539999907, 1515.545045452190152, 209.8706226742160084 ) ) ;
#85175 = CARTESIAN_POINT ( 'NONE',  ( -2.470955850358403705, 1523.580204110582144, 242.8749759455149615 ) ) ;
#85176 = CARTESIAN_POINT ( 'NONE',  ( 27.06966409833973941, 1508.822567037296949, 206.2042575372482816 ) ) ;
#85177 = CARTESIAN_POINT ( 'NONE',  ( 4.327793175846784024, 1516.734711358257528, 215.2529812453810223 ) ) ;
#85178 = CARTESIAN_POINT ( 'NONE',  ( 9.246914999585321482, 1451.227871316439860, 209.6132637504499883 ) ) ;
#85179 = CARTESIAN_POINT ( 'NONE',  ( -10.33117234729999900, 1391.913060387289988, 214.5016767380689942 ) ) ;
#85180 = CARTESIAN_POINT ( 'NONE',  ( -90.34139317962680593, 1384.840033543810023, 292.7666966122710051 ) ) ;
#85181 = VERTEX_POINT ( 'NONE', #110088 ) ;
#85182 = CARTESIAN_POINT ( 'NONE',  ( -3.262264688434999726, 1516.633288330999903, 202.5742890007669814 ) ) ;
#85183 = CARTESIAN_POINT ( 'NONE',  ( 1.133653140995000141, 1516.978425811520083, 209.8592968530090275 ) ) ;
#85184 = EDGE_LOOP ( 'NONE', ( #17072, #75119, #99010, #67336 ) ) ;
#85185 = CARTESIAN_POINT ( 'NONE',  ( 19.31456092990000073, 1455.192895371089890, 208.1952086544899885 ) ) ;
#85186 = CARTESIAN_POINT ( 'NONE',  ( 19.70018007940000260, 1487.524873918330059, 228.1714004993980041 ) ) ;
#85187 = ORIENTED_EDGE ( 'NONE', *, *, #18261, .T. ) ;
#85188 = CARTESIAN_POINT ( 'NONE',  ( -13.76682154080000053, 1416.274718422629803, 221.8364419309980065 ) ) ;
#85189 = CARTESIAN_POINT ( 'NONE',  ( -11.13648087572960144, 1432.345323104730141, 151.6342752581680031 ) ) ;
#85190 = DIRECTION ( 'NONE',  ( 1.755985294532464991E-16, -1.000000000000000000, 1.338183447452830017E-16 ) ) ;
#85191 = CARTESIAN_POINT ( 'NONE',  ( -3.624924048459783776, 1488.770799682897859, 219.3952194504361159 ) ) ;
#85192 = CARTESIAN_POINT ( 'NONE',  ( -4.848112173330000552, 1424.812407234129978, 186.1231568304979760 ) ) ;
#85193 = CARTESIAN_POINT ( 'NONE',  ( -7.632823605539153178, 1446.706720026436187, 154.1366947371981837 ) ) ;
#85194 = DIRECTION ( 'NONE',  ( 1.755985294532464991E-16, -1.000000000000000000, 1.338183447452830017E-16 ) ) ;
#85195 = CARTESIAN_POINT ( 'NONE',  ( 6.042689891000001090, 1492.864352563789907, 218.4381426803390127 ) ) ;
#85196 = CARTESIAN_POINT ( 'NONE',  ( -50.59433295680000242, 1379.743302990699931, 241.3342481622590014 ) ) ;
#85197 = CARTESIAN_POINT ( 'NONE',  ( 24.02067050899190193, 1444.215366903609947, 206.2118375416320077 ) ) ;
#85199 = CARTESIAN_POINT ( 'NONE',  ( -1.757532416683340148, 1451.933574871519795, 184.1885909450070073 ) ) ;
#85198 = CARTESIAN_POINT ( 'NONE',  ( 18.07930019940000221, 1457.670260863829981, 229.7183053948980103 ) ) ;
#85200 = CARTESIAN_POINT ( 'NONE',  ( -4.804557508719293324, 1423.543705180204142, 184.5808143603345002 ) ) ;
#85201 = CARTESIAN_POINT ( 'NONE',  ( -13.96269180912499941, 1502.379650475309973, 226.3091602680140113 ) ) ;
#85202 = ORIENTED_EDGE ( 'NONE', *, *, #55265, .T. ) ;
#85203 = CARTESIAN_POINT ( 'NONE',  ( 18.08636941810240018, 1424.496041336439930, 224.1297234290499887 ) ) ;
#85204 = CARTESIAN_POINT ( 'NONE',  ( 0.7899257907088232944, 1516.710726079306141, 216.8354974527231036 ) ) ;
#85205 = CARTESIAN_POINT ( 'NONE',  ( -2.915526101786688251, 1484.840208661149063, 183.2060714930112511 ) ) ;
#85206 = CARTESIAN_POINT ( 'NONE',  ( -9.047070658296459234E-06, 1407.650947979230068, 270.1377427408980338 ) ) ;
#85208 = ORIENTED_EDGE ( 'NONE', *, *, #10863, .T. ) ;
#85207 = CARTESIAN_POINT ( 'NONE',  ( 4.159841809088510978, 1508.728286212990042, 213.5483455248779876 ) ) ;
#85209 = FACE_OUTER_BOUND ( 'NONE', #110019, .T. ) ;
#85210 = CARTESIAN_POINT ( 'NONE',  ( -0.3329474806990009861, 1507.873469256489898, 221.0089344693989801 ) ) ;
#85211 = CARTESIAN_POINT ( 'NONE',  ( -11.80513488090000074, 1428.473324687329978, 148.4494227052980193 ) ) ;
#85212 = CARTESIAN_POINT ( 'NONE',  ( -14.87168881317970026, 1430.147188212150240, 221.8136313441650032 ) ) ;
#85213 = CARTESIAN_POINT ( 'NONE',  ( -10.77150947492019917, 1461.758312437779978, 211.3157053564689818 ) ) ;
#85214 = CARTESIAN_POINT ( 'NONE',  ( -4.367937192439999450, 1447.898255911189835, 190.6350925615990093 ) ) ;
#85215 = CARTESIAN_POINT ( 'NONE',  ( -4.030172342475210279, 1428.333731443729903, 200.6736590918410172 ) ) ;
#85216 = CARTESIAN_POINT ( 'NONE',  ( 2.896431327470000205, 1410.394954567630066, 231.6349568340980056 ) ) ;
#85218 = CARTESIAN_POINT ( 'NONE',  ( -10.47826420840229922, 1480.900688901569993, 207.8449939762269878 ) ) ;
#85217 = CARTESIAN_POINT ( 'NONE',  ( -20.47759437099999857, 1470.086929132030036, 225.5303694363980185 ) ) ;
#85219 = CARTESIAN_POINT ( 'NONE',  ( -0.9205759414320010547, 1469.929133752490088, 216.3346150940489849 ) ) ;
#85220 = ORIENTED_EDGE ( 'NONE', *, *, #67976, .T. ) ;
#85221 = CARTESIAN_POINT ( 'NONE',  ( 4.996642160164999957, 1516.697242742309982, 206.2447328616370044 ) ) ;
#85222 = CARTESIAN_POINT ( 'NONE',  ( 18.31222429210000158, 1408.824700350729927, 268.9136943074980195 ) ) ;
#85223 = CARTESIAN_POINT ( 'NONE',  ( -21.38516915557942255, 1524.726013923371283, 237.8497028174240029 ) ) ;
#85224 = CARTESIAN_POINT ( 'NONE',  ( 21.87475989109999830, 1430.294660538329936, 199.6850607904279968 ) ) ;
#85225 = VECTOR ( 'NONE', #6811, 1000.000000000000000 ) ;
#85226 = CARTESIAN_POINT ( 'NONE',  ( 4.329448776040000446, 1515.064792882589927, 209.0973262533439936 ) ) ;
#85227 = CARTESIAN_POINT ( 'NONE',  ( 4.144002508462048873, 1453.992169703209811, 217.5342908371910084 ) ) ;
#85228 = CARTESIAN_POINT ( 'NONE',  ( -1.275176580349999922, 1451.321844197929977, 183.5437223828979825 ) ) ;
#85229 = DIRECTION ( 'NONE',  ( -1.755985294532469921E-16, 1.000000000000000000, -1.338183447452831989E-16 ) ) ;
#85230 = CARTESIAN_POINT ( 'NONE',  ( -14.62060631049999770, 1416.594821258409866, 204.2386896224389830 ) ) ;
#85231 = CARTESIAN_POINT ( 'NONE',  ( -14.28540945339999979, 1444.019357213639978, 188.7049663577979857 ) ) ;
#85232 = CARTESIAN_POINT ( 'NONE',  ( -18.07642520410000131, 1475.513060387329915, 220.4627547701979893 ) ) ;
#85233 = CARTESIAN_POINT ( 'NONE',  ( -16.18859208205868683, 1419.742601152931002, 209.9822759361395015 ) ) ;
#85234 = CARTESIAN_POINT ( 'NONE',  ( -4.318206861440000210, 1497.528676090189947, 220.7835062296990145 ) ) ;
#85235 = ORIENTED_EDGE ( 'NONE', *, *, #89780, .T. ) ;
#85236 = CARTESIAN_POINT ( 'NONE',  ( 1.465037550250199994, 1491.117439488069977, 181.8109677011690053 ) ) ;
#85237 = CARTESIAN_POINT ( 'NONE',  ( -13.23418824936010019, 1409.375208424609809, 216.0505887701349934 ) ) ;
#85238 = CARTESIAN_POINT ( 'NONE',  ( -11.60674054546250034, 1507.508082460230071, 207.5537236852100023 ) ) ;
#85239 = CARTESIAN_POINT ( 'NONE',  ( -12.12980996005155276, 1377.655037718360973, 211.2214414945090937 ) ) ;
#85240 = CARTESIAN_POINT ( 'NONE',  ( -21.63439191490000368, 1471.040418176530011, 269.4983909155979518 ) ) ;
#85241 = CARTESIAN_POINT ( 'NONE',  ( -5.909698491649999497, 1449.521837735690042, 210.1656816284789784 ) ) ;
#85242 = CARTESIAN_POINT ( 'NONE',  ( -14.59144169897830956, 1514.407829430023639, 192.7405808733855395 ) ) ;
#85243 = CARTESIAN_POINT ( 'NONE',  ( -24.07534640571084950, 1444.393242560262479, 211.9935189188719278 ) ) ;
#85244 = CARTESIAN_POINT ( 'NONE',  ( -65.34430217836160182, 1384.676577935759951, 289.2243165953830157 ) ) ;
#85245 = CARTESIAN_POINT ( 'NONE',  ( -13.05275046466420008, 1384.938348676199894, 200.3351238176559832 ) ) ;
#85246 = CARTESIAN_POINT ( 'NONE',  ( 12.10884181136779958, 1416.007771869960152, 223.4226694167990104 ) ) ;
#85247 = CARTESIAN_POINT ( 'NONE',  ( -107.5335879240000025, 1378.913060387289988, 300.4967944802589841 ) ) ;
#85248 = DIRECTION ( 'NONE',  ( 0.08340294689805435868, -0.004098122787127734569, 0.9965074780644357366 ) ) ;
#85249 = CARTESIAN_POINT ( 'NONE',  ( -0.7910245917146945249, 1426.918876941764893, 137.0999999980979851 ) ) ;
#85250 = CARTESIAN_POINT ( 'NONE',  ( -22.94104396079999830, 1409.714179296030125, 208.0443976299279996 ) ) ;
#85251 = CARTESIAN_POINT ( 'NONE',  ( -8.374671775625037284, 1382.833066931880694, 199.9155290017601772 ) ) ;
#85252 = EDGE_CURVE ( 'NONE', #16145, #67278, #109336, .T. ) ;
#85253 = CARTESIAN_POINT ( 'NONE',  ( 3.933180850559999886, 1485.871275756990144, 219.1485422991989935 ) ) ;
#85254 = FACE_OUTER_BOUND ( 'NONE', #97303, .T. ) ;
#85255 = ADVANCED_FACE ( 'NONE', ( #38594 ), #94775, .T. ) ;
#85256 = CARTESIAN_POINT ( 'NONE',  ( -17.33962108957659964, 1446.210180764470124, 200.4727308985020215 ) ) ;
#85257 = CIRCLE ( 'NONE', #79935, 1.999999999999998668 ) ;
#85258 = CARTESIAN_POINT ( 'NONE',  ( 20.40402507730000181, 1433.421378987090065, 214.6266990018290244 ) ) ;
#85259 = CARTESIAN_POINT ( 'NONE',  ( 16.94363731710740595, 1525.231909165033585, 181.3784879451278584 ) ) ;
#85260 = CARTESIAN_POINT ( 'NONE',  ( -7.540514764990074781, 1385.122439251179685, 219.0844776276921380 ) ) ;
#85262 = CARTESIAN_POINT ( 'NONE',  ( -9.123736442209999353, 1384.508619151449921, 199.9712811190890136 ) ) ;
#85261 = CARTESIAN_POINT ( 'NONE',  ( -21.54410644429999877, 1409.665397162329782, 210.5639858174479855 ) ) ;
#85263 = CARTESIAN_POINT ( 'NONE',  ( 11.73645003660239894, 1426.696353566730068, 144.1286464700729937 ) ) ;
#85264 = CARTESIAN_POINT ( 'NONE',  ( 9.687311913827020504, 1436.266597529439878, 210.8265562985189945 ) ) ;
#85265 = DIRECTION ( 'NONE',  ( 1.000000000000000000, 0.000000000000000000, 0.000000000000000000 ) ) ;
#85266 = CARTESIAN_POINT ( 'NONE',  ( 5.304930756692599836, 1447.452529283679951, 200.4004275134280135 ) ) ;
#85267 = CARTESIAN_POINT ( 'NONE',  ( -0.06333887091406470438, 1408.725629457220066, 223.1955288070940071 ) ) ;
#85268 = CARTESIAN_POINT ( 'NONE',  ( -7.719392420504999741, 1516.929962200689943, 202.5670673984569703 ) ) ;
#85269 = CARTESIAN_POINT ( 'NONE',  ( -5.631861160212480399, 1398.080659042673688, 220.8446200131021726 ) ) ;
#85270 = FACE_BOUND ( 'NONE', #49251, .T. ) ;
#85271 = CARTESIAN_POINT ( 'NONE',  ( -17.64656215119999771, 1410.883670852830164, 194.5767827140980160 ) ) ;
#85272 = CARTESIAN_POINT ( 'NONE',  ( 10.86417644130879978, 1503.361827989980156, 213.1981603545889925 ) ) ;
#85274 = VERTEX_POINT ( 'NONE', #25507 ) ;
#85273 = CARTESIAN_POINT ( 'NONE',  ( -26.01288487611240186, 1379.670732920850014, 215.3165728412730004 ) ) ;
#85275 = ADVANCED_FACE ( 'NONE', ( #51850 ), #101867, .T. ) ;
#85276 = ORIENTED_EDGE ( 'NONE', *, *, #36996, .F. ) ;
#85277 = CARTESIAN_POINT ( 'NONE',  ( 11.89750062909999961, 1433.907086374190158, 150.7125587214979987 ) ) ;
#85278 = CARTESIAN_POINT ( 'NONE',  ( 28.15435480200000029, 1509.896243100630045, 217.4028989878879941 ) ) ;
#85279 = EDGE_LOOP ( 'NONE', ( #93593, #50738, #101409, #79374, #90831 ) ) ;
#85280 = CARTESIAN_POINT ( 'NONE',  ( -0.0002535134715325740242, 1396.409806809705060, 221.4414762769463039 ) ) ;
#85281 = CARTESIAN_POINT ( 'NONE',  ( -23.95032396419999898, 1509.749424129729960, 192.7253573581980106 ) ) ;
#85282 = CARTESIAN_POINT ( 'NONE',  ( -4.408349274510000804, 1512.051704408390151, 206.7128113371389873 ) ) ;
#85284 = CARTESIAN_POINT ( 'NONE',  ( 18.02057538510000256, 1424.315176607929743, 225.5995559224980127 ) ) ;
#85283 = CARTESIAN_POINT ( 'NONE',  ( -11.75869035857540013, 1522.051704408389924, 190.9442076533970010 ) ) ;
#85285 = CARTESIAN_POINT ( 'NONE',  ( 14.93738999439999837, 1507.809955652629924, 232.3150682984980051 ) ) ;
#85286 = CARTESIAN_POINT ( 'NONE',  ( 3.193178223990000397, 1449.236852389319893, 184.0465812473979952 ) ) ;
#85287 = CARTESIAN_POINT ( 'NONE',  ( 3.401541474679999677, 1468.225229937389940, 218.5224292272789910 ) ) ;
#85288 = CARTESIAN_POINT ( 'NONE',  ( 15.52863166319999877, 1409.957043847029809, 226.9582993814979943 ) ) ;
#85289 =( NAMED_UNIT ( * ) SI_UNIT ( $, .STERADIAN. ) SOLID_ANGLE_UNIT ( ) );
#85290 = CARTESIAN_POINT ( 'NONE',  ( 14.79681306129999996, 1434.437610817989935, 221.1969614931990122 ) ) ;
#85291 = CARTESIAN_POINT ( 'NONE',  ( 13.40958089240390017, 1414.996442620800053, 197.9133050684260127 ) ) ;
#85292 = CARTESIAN_POINT ( 'NONE',  ( 11.28450772929999957, 1431.049583972360097, 151.4082744405979781 ) ) ;
#85293 = CARTESIAN_POINT ( 'NONE',  ( 1.657820374930000007, 1433.671037157990213, 203.5362873279890152 ) ) ;
#85294 = ORIENTED_EDGE ( 'NONE', *, *, #15165, .F. ) ;
#85295 = CARTESIAN_POINT ( 'NONE',  ( 13.55393066989770112, 1434.957539567609956, 148.7506260606290027 ) ) ;
#85296 = ORIENTED_EDGE ( 'NONE', *, *, #37848, .T. ) ;
#85297 = ORIENTED_EDGE ( 'NONE', *, *, #77435, .F. ) ;
#85298 = CARTESIAN_POINT ( 'NONE',  ( 13.26721377506743238, 1444.631487620105418, 169.3823617746430443 ) ) ;
#85299 = CARTESIAN_POINT ( 'NONE',  ( -6.765101722839999887, 1464.003571155029931, 235.1670121008980345 ) ) ;
#85300 = CARTESIAN_POINT ( 'NONE',  ( -13.97867491850210087, 1429.402194067919709, 222.2970902837259928 ) ) ;
#85301 = AXIS2_PLACEMENT_3D ( 'NONE', #87711, #97743, #78743 ) ;
#85302 = CARTESIAN_POINT ( 'NONE',  ( -4.035536263215000474, 1517.086065052259983, 216.8453260496270047 ) ) ;
#85303 = CARTESIAN_POINT ( 'NONE',  ( -8.003699198419786498, 1511.683921177773755, 212.5077785452298826 ) ) ;
#85304 = EDGE_CURVE ( 'NONE', #56530, #22078, #30735, .T. ) ;
#85305 = CARTESIAN_POINT ( 'NONE',  ( -18.97979506072560341, 1443.417780829110598, 211.6816736686500633 ) ) ;
#85306 = CARTESIAN_POINT ( 'NONE',  ( -1.793335950739999962, 1419.496365638530051, 185.6406336190979971 ) ) ;
#85307 = CARTESIAN_POINT ( 'NONE',  ( -11.64847922969999949, 1377.842188321789990, 206.5023625028690049 ) ) ;
#85308 = EDGE_CURVE ( 'NONE', #94675, #35766, #8495, .T. ) ;
#85309 = EDGE_LOOP ( 'NONE', ( #57659, #77517, #52000, #63182 ) ) ;
#85310 = CARTESIAN_POINT ( 'NONE',  ( 4.027051405805000428, 1516.733363207009916, 206.6306575737070261 ) ) ;
#85311 = ORIENTED_EDGE ( 'NONE', *, *, #50403, .F. ) ;
#85312 = CARTESIAN_POINT ( 'NONE',  ( 19.96317061269749971, 1440.913060387330006, 216.1997736411760229 ) ) ;
#85313 = CARTESIAN_POINT ( 'NONE',  ( -19.60066770079999898, 1508.321169291629985, 229.5156755424980020 ) ) ;
#85314 = CARTESIAN_POINT ( 'NONE',  ( -8.768908993999998458, 1409.219277437030087, 189.4712383907980211 ) ) ;
#85315 = CARTESIAN_POINT ( 'NONE',  ( 7.469619891705000292, 1513.342361861140034, 216.8722327131270049 ) ) ;
#85317 = ORIENTED_EDGE ( 'NONE', *, *, #66723, .T. ) ;
#85316 = CARTESIAN_POINT ( 'NONE',  ( -4.175281431485900363, 1433.777855993409958, 217.7638082317450028 ) ) ;
#85318 = CARTESIAN_POINT ( 'NONE',  ( 23.67158291440000184, 1434.407285501780052, 214.7094373112279868 ) ) ;
#85320 = B_SPLINE_CURVE_WITH_KNOTS ( 'NONE', 5,
 ( #82645, #56348, #13205, #91028, #20503, #89390 ),
 .UNSPECIFIED., .F., .F.,
 ( 6, 6 ),
 ( 4.250950522260000142, 7.082025451739999866 ),
 .UNSPECIFIED. ) ;
#85319 = CARTESIAN_POINT ( 'NONE',  ( -13.94448290884199970, 1508.551704408389924, 210.3470438395370081 ) ) ;
#85321 = CARTESIAN_POINT ( 'NONE',  ( -6.372167638625000130, 1511.069621805459974, 201.7253008890070021 ) ) ;
#85322 = CARTESIAN_POINT ( 'NONE',  ( 5.386185205460879644, 1432.347042709529887, 154.6076275981190236 ) ) ;
#85323 = CARTESIAN_POINT ( 'NONE',  ( 21.41029105012001921, 1526.329757971583831, 184.2230555347920529 ) ) ;
#85324 = AXIS2_PLACEMENT_3D ( 'NONE', #77794, #95696, #10592 ) ;
#85325 = CARTESIAN_POINT ( 'NONE',  ( -2.868433836634999512, 1517.020727862619879, 214.1341630384669941 ) ) ;
#85326 = CARTESIAN_POINT ( 'NONE',  ( -3.292573594295789885, 1428.757065012120165, 200.3549139475240111 ) ) ;
#85327 = CARTESIAN_POINT ( 'NONE',  ( 22.80370854688087690, 1409.709376451625985, 209.3213601526881575 ) ) ;
#85328 = CARTESIAN_POINT ( 'NONE',  ( 5.513240537208758951, 1508.551563895499839, 216.2888651833050062 ) ) ;
#85329 = CARTESIAN_POINT ( 'NONE',  ( 2.493699768634999536, 1516.858326417339867, 211.5985794462469869 ) ) ;
#85330 = CARTESIAN_POINT ( 'NONE',  ( 14.33610687090000013, 1409.413688268130045, 192.4637013132980030 ) ) ;
#85331 = CARTESIAN_POINT ( 'NONE',  ( 29.70307915522525732, 1525.408327360769590, 221.9454130908924583 ) ) ;
#85333 = ORIENTED_EDGE ( 'NONE', *, *, #79994, .F. ) ;
#85332 = CARTESIAN_POINT ( 'NONE',  ( -73.21223786119999488, 1390.654864019360048, 287.6042314150589618 ) ) ;
#85334 = CARTESIAN_POINT ( 'NONE',  ( -65.00424250889579980, 1385.043326950109986, 288.7494347189460200 ) ) ;
#85335 = CARTESIAN_POINT ( 'NONE',  ( -2.370583552050000338E-08, 1473.529262908829878, 262.4990046775979522 ) ) ;
#85336 = CARTESIAN_POINT ( 'NONE',  ( 10.67800209769209907, 1490.926871433870247, 211.7224831522450188 ) ) ;
#85337 = CARTESIAN_POINT ( 'NONE',  ( -28.95199422474000173, 1509.924086303959939, 213.9638677111150002 ) ) ;
#85338 = B_SPLINE_CURVE_WITH_KNOTS ( 'NONE', 3,
 ( #94582, #1112, #35241, #26845, #61032, #87308, #71656, #37455, #104100, #87876, #105775, #10601 ),
 .UNSPECIFIED., .F., .F.,
 ( 4, 2, 2, 2, 2, 4 ),
 ( -0.1123552056311339920, -0.09789079770760569787, -0.08345975727310689374, -0.05408602631436299629, -0.02844277166354580721, 1.387778780781445676E-17 ),
 .UNSPECIFIED. ) ;
#85339 = CARTESIAN_POINT ( 'NONE',  ( -2.757035807209109901, 1508.901542382500111, 238.0815734855640073 ) ) ;
#85340 = CARTESIAN_POINT ( 'NONE',  ( -0.8597107444419990196, 1463.363299253190007, 202.2013017319989956 ) ) ;
#85341 = CARTESIAN_POINT ( 'NONE',  ( -31.34137657934000387, 1523.382868172864164, 221.9025654077414345 ) ) ;
#85342 = CIRCLE ( 'NONE', #31722, 1.000000000000000888 ) ;
#85344 = CARTESIAN_POINT ( 'NONE',  ( 17.94190076916380150, 1410.493024420959955, 222.9337422920199856 ) ) ;
#85343 = CARTESIAN_POINT ( 'NONE',  ( -0.02955819112566620069, 1517.051704408389924, 225.0080808726450243 ) ) ;
#85345 = CARTESIAN_POINT ( 'NONE',  ( 32.78250617288044566, 1511.187213306747708, 218.3079823578266314 ) ) ;
#85346 = CARTESIAN_POINT ( 'NONE',  ( -109.1575033200779927, 1383.485187780409888, 311.0614977769220673 ) ) ;
#85347 = ORIENTED_EDGE ( 'NONE', *, *, #75456, .F. ) ;
#85348 = CARTESIAN_POINT ( 'NONE',  ( 3.451033388965000004, 1517.025653221279981, 203.3353183697670090 ) ) ;
#85349 = CARTESIAN_POINT ( 'NONE',  ( -11.29483889965070098, 1508.440183434380060, 218.1662304949769862 ) ) ;
#85350 = CARTESIAN_POINT ( 'NONE',  ( 29.15071166469999753, 1509.931025669929795, 206.3815615989880143 ) ) ;
#85351 = AXIS2_PLACEMENT_3D ( 'NONE', #76588, #110739, #16644 ) ;
#85352 = FACE_OUTER_BOUND ( 'NONE', #29112, .T. ) ;
#85353 = CARTESIAN_POINT ( 'NONE',  ( -13.41054182479114054, 1504.856770982285980, 208.9138911101860288 ) ) ;
#85354 =( BOUNDED_SURFACE ( )  B_SPLINE_SURFACE ( 3, 2, ( 
 ( #431, #74510, #108640 ),
 ( #101738, #34550, #59228 ),
 ( #103961, #88274, #37874 ),
 ( #105637, #12664, #95565 ) ),
 .UNSPECIFIED., .F., .F., .F. ) 
 B_SPLINE_SURFACE_WITH_KNOTS ( ( 4, 4 ),
 ( 3, 3 ),
 ( 0.000000000000000000, 0.0002960034161023848394 ),
 ( 0.000000000000000000, 1.000000000000000000 ),
 .UNSPECIFIED. ) 
 GEOMETRIC_REPRESENTATION_ITEM ( )  RATIONAL_B_SPLINE_SURFACE ( (
 ( 1.000000000000000000, 0.8070209408750156355, 1.000000000000000000),
 ( 1.000000000000000000, 0.8071723757218154383, 1.000000000000000000),
 ( 1.000000000000000000, 0.8072480346917759730, 1.000000000000000000),
 ( 1.000000000000000000, 0.8072480644198091193, 1.000000000000000000) ) ) 
 REPRESENTATION_ITEM ( '' )  SURFACE ( )  );
#85355 = CARTESIAN_POINT ( 'NONE',  ( 3.691669781079999879, 1467.622943078690014, 218.3869275675289998 ) ) ;
#85356 = CARTESIAN_POINT ( 'NONE',  ( 24.59498489902570029, 1440.913044926110160, 213.3385239659299941 ) ) ;
#85357 = CARTESIAN_POINT ( 'NONE',  ( 32.64372457531959526, 1436.966666287780072, 136.6006212270859805 ) ) ;
#85358 = CARTESIAN_POINT ( 'NONE',  ( -38.63560630069969903, 1444.097728792060025, 137.1726987393469983 ) ) ;
#85359 = CARTESIAN_POINT ( 'NONE',  ( 3.996802888650000299E-15, 1464.864131489809779, 254.9666375976830182 ) ) ;
#85360 = DIRECTION ( 'NONE',  ( -0.05752486295818490941, -0.9969860201949397593, 0.05205540968523030693 ) ) ;
#85361 = CARTESIAN_POINT ( 'NONE',  ( -16.86767980680000178, 1410.829200352329963, 226.4168310385980192 ) ) ;
#85362 = CARTESIAN_POINT ( 'NONE',  ( 11.55216494016860018, 1480.217685936279850, 211.4791692585090175 ) ) ;
#85363 = CARTESIAN_POINT ( 'NONE',  ( -21.42853521715671761, 1524.678541297860875, 184.2223151939084005 ) ) ;
#85364 = FACE_OUTER_BOUND ( 'NONE', #64739, .T. ) ;
#85365 = ORIENTED_EDGE ( 'NONE', *, *, #31306, .T. ) ;
#85366 = CARTESIAN_POINT ( 'NONE',  ( -40.73184307449999864, 1436.263014496689948, 268.3665355199980240 ) ) ;
#85367 = CARTESIAN_POINT ( 'NONE',  ( 2.407076450357060082, 1456.389291684359932, 219.4682715861369786 ) ) ;
#85368 = CARTESIAN_POINT ( 'NONE',  ( 11.40561765973709996, 1470.999254084470067, 209.2195126300399863 ) ) ;
#85369 = CARTESIAN_POINT ( 'NONE',  ( 15.14272559822449793, 1450.983108074159873, 189.8671428218680148 ) ) ;
#85370 = CARTESIAN_POINT ( 'NONE',  ( 11.41065117167780762, 1425.709223140004497, 138.9050562313533419 ) ) ;
#85373 = DIRECTION ( 'NONE',  ( -0.5877852522924746914, 0.000000000000000000, -0.8090169943749463410 ) ) ;
#85372 = VECTOR ( 'NONE', #56183, 1000.000000000000114 ) ;
#85371 = CARTESIAN_POINT ( 'NONE',  ( 11.44311708750000101, 1501.817457268189855, 208.4257042509889857 ) ) ;
#85374 = FACE_OUTER_BOUND ( 'NONE', #77754, .T. ) ;
#85375 = CARTESIAN_POINT ( 'NONE',  ( 7.236738478339999503, 1426.973880016789963, 212.3972659138590018 ) ) ;
#85376 = CARTESIAN_POINT ( 'NONE',  ( -3.912776123225929936, 1515.493282983300105, 212.5868990599399808 ) ) ;
#85377 = FACE_OUTER_BOUND ( 'NONE', #46361, .T. ) ;
#85378 = CARTESIAN_POINT ( 'NONE',  ( -19.32265508015788669, 1451.005352466662998, 146.2743915447199186 ) ) ;
#85379 = CARTESIAN_POINT ( 'NONE',  ( -16.67301258007090325, 1414.971349104640012, 209.3683847725079943 ) ) ;
#85380 = CARTESIAN_POINT ( 'NONE',  ( 24.29594634020000044, 1435.420522265349973, 137.1129172815979871 ) ) ;
#85381 = CARTESIAN_POINT ( 'NONE',  ( -10.28643981572550103, 1396.272270782580108, 205.0450038041399807 ) ) ;
#85382 = ORIENTED_EDGE ( 'NONE', *, *, #59619, .T. ) ;
#85383 = CARTESIAN_POINT ( 'NONE',  ( 1.711055448681089940E-31, 1424.874073124720098, 209.1218459616989946 ) ) ;
#85384 = CARTESIAN_POINT ( 'NONE',  ( -1.953612668519999707, 1408.981282045029957, 231.3328323811979885 ) ) ;
#85385 = EDGE_LOOP ( 'NONE', ( #90950, #35677, #104451, #82085, #99914 ) ) ;
#85386 = ORIENTED_EDGE ( 'NONE', *, *, #100031, .T. ) ;
#85387 = CARTESIAN_POINT ( 'NONE',  ( -4.313829138780000072, 1500.726371502089933, 230.0083276664990137 ) ) ;
#85388 = CARTESIAN_POINT ( 'NONE',  ( -15.56794941087492390, 1415.969174529124075, 207.8815349042810112 ) ) ;
#85390 = CARTESIAN_POINT ( 'NONE',  ( 1.111422967361669789, 1456.698882163199869, 219.6849870739549999 ) ) ;
#85389 = CARTESIAN_POINT ( 'NONE',  ( 11.02768931129999963, 1426.931661410030074, 92.69464464869780329 ) ) ;
#85391 = CARTESIAN_POINT ( 'NONE',  ( 23.34379457190000196, 1410.649718844729932, 212.3615055056179983 ) ) ;
#85392 = CARTESIAN_POINT ( 'NONE',  ( 4.156515053869860310, 1424.245343161929895, 184.5679882677330284 ) ) ;
#85393 = CARTESIAN_POINT ( 'NONE',  ( -41.40570855549999862, 1380.117442312619914, 227.6002677670589947 ) ) ;
#85394 = CARTESIAN_POINT ( 'NONE',  ( -2.843812590201006518, 1419.747894056850782, 186.1690033552606849 ) ) ;
#85395 = CARTESIAN_POINT ( 'NONE',  ( 7.890413475299999924, 1422.993678601120109, 213.8680409669790095 ) ) ;
#85396 = CARTESIAN_POINT ( 'NONE',  ( -2.515613294380000031, 1448.349718812090032, 188.5842421506989979 ) ) ;
#85397 = CARTESIAN_POINT ( 'NONE',  ( 8.664649168559998671, 1509.043694294030047, 182.0634189174980122 ) ) ;
#85398 = CARTESIAN_POINT ( 'NONE',  ( -101.5349560225229908, 1377.092447604730069, 306.6887311473950035 ) ) ;
#85399 = CARTESIAN_POINT ( 'NONE',  ( 9.454737631267599696, 1363.431170718773956, 210.6218459616987957 ) ) ;
#85401 = ORIENTED_EDGE ( 'NONE', *, *, #110557, .T. ) ;
#85400 = CARTESIAN_POINT ( 'NONE',  ( -4.363122647530000009, 1423.854802298929826, 172.2701767054979882 ) ) ;
#85402 = ORIENTED_EDGE ( 'NONE', *, *, #45616, .F. ) ;
#85403 = EDGE_CURVE ( 'NONE', #13291, #43055, #39258, .T. ) ;
#85404 = CARTESIAN_POINT ( 'NONE',  ( -11.81903391593660047, 1429.240617403939950, 149.0414667438120091 ) ) ;
#85405 = CARTESIAN_POINT ( 'NONE',  ( 1.847634001515719993, 1478.089546411300262, 198.8590795898780073 ) ) ;
#85406 = CARTESIAN_POINT ( 'NONE',  ( -0.4918994192140000443, 1474.175172928430129, 270.1377426665980011 ) ) ;
#85407 = CARTESIAN_POINT ( 'NONE',  ( 9.407330927246226437, 1500.876264887889647, 202.6219334492917596 ) ) ;
#85408 = CARTESIAN_POINT ( 'NONE',  ( -107.3060007717225375, 1358.631207110789546, 307.5510129087674045 ) ) ;
#85409 = CARTESIAN_POINT ( 'NONE',  ( 2.596261494520237800, 1525.907212628473644, 240.7735774411711702 ) ) ;
#85410 = CARTESIAN_POINT ( 'NONE',  ( -7.983409256419999878, 1384.364947284539767, 199.5220205512890175 ) ) ;
#85411 = EDGE_CURVE ( 'NONE', #38088, #2271, #18454, .T. ) ;
#85412 = CARTESIAN_POINT ( 'NONE',  ( 22.77127579980000149, 1411.073674597329955, 206.9287118965879984 ) ) ;
#85413 = CARTESIAN_POINT ( 'NONE',  ( -22.90620825977149977, 1507.562497965029934, 208.0767490477490185 ) ) ;
#85414 = CARTESIAN_POINT ( 'NONE',  ( 3.756023522790000069, 1369.098589419769951, 207.6218459616989946 ) ) ;
#85415 = CARTESIAN_POINT ( 'NONE',  ( 10.10010064645940098, 1409.265763673950005, 197.6200419344060037 ) ) ;
#85416 = CARTESIAN_POINT ( 'NONE',  ( -15.54429786038520156, 1407.696428880429949, 267.7515575858669763 ) ) ;
#85417 = CARTESIAN_POINT ( 'NONE',  ( -113.4000000000000057, 1384.913060387289988, 304.2218459572590064 ) ) ;
#85418 = ORIENTED_EDGE ( 'NONE', *, *, #52429, .F. ) ;
#85419 = FACE_OUTER_BOUND ( 'NONE', #9837, .T. ) ;
#85420 = CARTESIAN_POINT ( 'NONE',  ( 13.77182695930000023, 1443.992469818299924, 189.0025103208980113 ) ) ;
#85421 = EDGE_LOOP ( 'NONE', ( #89522, #29674, #1754, #96143, #95907 ) ) ;
#85422 = VERTEX_POINT ( 'NONE', #38551 ) ;
#85423 = CARTESIAN_POINT ( 'NONE',  ( 4.653692642196047835, 1422.133935384945516, 184.1087935189646885 ) ) ;
#85424 = CARTESIAN_POINT ( 'NONE',  ( 14.91143818900724405, 1416.177402202029953, 209.1063111766177940 ) ) ;
#85425 = CARTESIAN_POINT ( 'NONE',  ( -2.479246885834999858, 1516.983612918759945, 213.1658362778269691 ) ) ;
#85426 = CARTESIAN_POINT ( 'NONE',  ( -16.93220803830000065, 1485.485519723529933, 188.1884812454979965 ) ) ;
#85427 = CIRCLE ( 'NONE', #62218, 1.000000000000000000 ) ;
#85428 = CARTESIAN_POINT ( 'NONE',  ( -10.50234776566190043, 1470.323106409019829, 212.1315068601290079 ) ) ;
#85429 = EDGE_LOOP ( 'NONE', ( #79691, #100307, #91872 ) ) ;
#85430 = CARTESIAN_POINT ( 'NONE',  ( -113.4000000000000057, 1374.413060387289988, 304.2218459572590064 ) ) ;
#85431 = CIRCLE ( 'NONE', #21088, 1.999994602351862438 ) ;
#85432 = CARTESIAN_POINT ( 'NONE',  ( -5.363939304704870459, 1424.918647691059959, 151.3386706125469914 ) ) ;
#85433 = CARTESIAN_POINT ( 'NONE',  ( -2.877113108595000135, 1516.697242742309982, 204.1252037719370094 ) ) ;
#85434 = CARTESIAN_POINT ( 'NONE',  ( -26.55602695130000157, 1507.993014311030038, 202.0788793302480144 ) ) ;
#85435 = CARTESIAN_POINT ( 'NONE',  ( -0.5846039405770000474, 1467.892742173730085, 230.0195927640980074 ) ) ;
#85436 = CARTESIAN_POINT ( 'NONE',  ( -45.26921098079020567, 1384.600480252990110, 218.6804048096429938 ) ) ;
#85437 = CARTESIAN_POINT ( 'NONE',  ( -2.930050900409999937, 1409.015380019430040, 194.3093250809980077 ) ) ;
#85438 = CARTESIAN_POINT ( 'NONE',  ( -103.5806803890000083, 1389.940350142260058, 304.1776731731589507 ) ) ;
#85440 = ORIENTED_EDGE ( 'NONE', *, *, #72432, .T. ) ;
#85439 = CARTESIAN_POINT ( 'NONE',  ( -6.153783059604999828, 1516.954809569559984, 216.8418890038570055 ) ) ;
#85441 = CARTESIAN_POINT ( 'NONE',  ( -28.15858260011039960, 1508.155820277190060, 209.9842769292959872 ) ) ;
#85442 = CARTESIAN_POINT ( 'NONE',  ( 26.83695571220000176, 1488.686901729329747, 212.2842936355180257 ) ) ;
#85443 = CARTESIAN_POINT ( 'NONE',  ( -66.48613725193760615, 1379.743195139351428, 277.3348019686743555 ) ) ;
#85444 = LINE ( 'NONE', #102258, #94961 ) ;
#85445 = CARTESIAN_POINT ( 'NONE',  ( -23.77853211389999899, 1435.327860087930048, 137.1324111805979840 ) ) ;
#85446 = AXIS2_PLACEMENT_3D ( 'NONE', #64235, #19997, #63691 ) ;
#85447 = CARTESIAN_POINT ( 'NONE',  ( -4.995994825704999975, 1516.665179208830068, 211.6114635085770033 ) ) ;
#85448 = CARTESIAN_POINT ( 'NONE',  ( -68.72596496900000318, 1379.747818773470044, 280.0427953276590074 ) ) ;
#85449 = CARTESIAN_POINT ( 'NONE',  ( 8.832258665910320161, 1437.105706114509985, 211.2299904616040180 ) ) ;
#85450 = CARTESIAN_POINT ( 'NONE',  ( 5.702926893268910113, 1484.838078577319948, 214.7898773046569829 ) ) ;
#85451 = CARTESIAN_POINT ( 'NONE',  ( -6.562094107424999656, 1517.122674412569950, 208.3832410274270046 ) ) ;
#85452 = ORIENTED_EDGE ( 'NONE', *, *, #73055, .F. ) ;
#85453 = CARTESIAN_POINT ( 'NONE',  ( -36.37832876739999932, 1451.642701153929920, 134.0999999898979809 ) ) ;
#85454 = CARTESIAN_POINT ( 'NONE',  ( 3.013238820032960064, 1440.805531895070089, 157.2037823681930320 ) ) ;
#85455 = CARTESIAN_POINT ( 'NONE',  ( -8.743385264969999682, 1384.893486076239924, 218.5827849380889916 ) ) ;
#85456 = ORIENTED_EDGE ( 'NONE', *, *, #70207, .F. ) ;
#85457 = CARTESIAN_POINT ( 'NONE',  ( -9.272580261226769593, 1385.313636453000072, 218.6819139582640048 ) ) ;
#85458 = CARTESIAN_POINT ( 'NONE',  ( -11.67167393029579969, 1491.623603738560178, 205.3077603581180028 ) ) ;
#85459 = CARTESIAN_POINT ( 'NONE',  ( 12.28148677300000102, 1434.518492997930025, 150.4836546675979889 ) ) ;
#85460 = CARTESIAN_POINT ( 'NONE',  ( -4.191720384344816530, 1441.591968528253801, 183.6965429472514302 ) ) ;
#85461 = CARTESIAN_POINT ( 'NONE',  ( -22.75670083784289943, 1508.433586079999941, 224.9338270191400113 ) ) ;
#85462 = CARTESIAN_POINT ( 'NONE',  ( -17.03788438627360691, 1524.775785348137561, 237.1518578317898118 ) ) ;
#85463 = CARTESIAN_POINT ( 'NONE',  ( -2.671306766649999886, 1410.383647693430021, 186.5757153796980106 ) ) ;
#85464 = CARTESIAN_POINT ( 'NONE',  ( 4.617112521066619735, 1430.220117714789922, 217.4127892114239842 ) ) ;
#85465 = CARTESIAN_POINT ( 'NONE',  ( 9.831195291770230327, 1461.796653735920017, 208.3421129756590062 ) ) ;
#85466 = AXIS2_PLACEMENT_3D ( 'NONE', #32803, #110072, #58582 ) ;
#85468 = CARTESIAN_POINT ( 'NONE',  ( 7.599227146160510316, 1512.341036968809931, 206.8869228877400133 ) ) ;
#85467 = CARTESIAN_POINT ( 'NONE',  ( 5.782749401605000727, 1516.858301627840092, 214.8983370654769942 ) ) ;
#85469 = CARTESIAN_POINT ( 'NONE',  ( 21.19481749090000022, 1509.644157120430236, 188.6018308473980198 ) ) ;
#85470 = DIRECTION ( 'NONE',  ( -1.000000000000000000, 0.000000000000000000, 0.000000000000000000 ) ) ;
#85471 = ORIENTED_EDGE ( 'NONE', *, *, #72894, .F. ) ;
#85472 = CARTESIAN_POINT ( 'NONE',  ( -12.61594209390000110, 1416.825532216630108, 194.9200742095979706 ) ) ;
#85473 = CARTESIAN_POINT ( 'NONE',  ( -16.72711410799999854, 1420.480869615339998, 203.4938400411990074 ) ) ;
#85474 = VERTEX_POINT ( 'NONE', #88421 ) ;
#85475 = CARTESIAN_POINT ( 'NONE',  ( 7.450245527241210475, 1489.014956828029881, 206.3621210875100189 ) ) ;
#85476 = B_SPLINE_CURVE_WITH_KNOTS ( 'NONE', 5,
 ( #70262, #20352, #54556, #69137, #103240, #5217, #13041, #73546, #65140, #74093, #23103, #47778, #47230, #39371, #39924, #4670, #22532, #55649, #72445, #3598, #108222 ),
 .UNSPECIFIED., .F., .F.,
 ( 6, 3, 3, 3, 3, 3, 6 ),
 ( -12.02704502919999996, -11.38341475070000008, -10.53188235890000080, -9.802594204569999192, -8.789679567349999445, -5.488753621229999879, 1.776356839400250465E-15 ),
 .UNSPECIFIED. ) ;
#85477 = CARTESIAN_POINT ( 'NONE',  ( -8.655671105859999770, 1512.830360918489987, 210.0583268009119990 ) ) ;
#85478 = CARTESIAN_POINT ( 'NONE',  ( 2.708816481117918507, 1524.478200376951463, 176.2954886323626056 ) ) ;
#85479 = CARTESIAN_POINT ( 'NONE',  ( 0.9134330820525868866, 1423.706385267109908, 191.2040966441970227 ) ) ;
#85480 = CARTESIAN_POINT ( 'NONE',  ( 8.578717400394859958E-16, 1374.913060387289988, 209.1218459616989946 ) ) ;
#85481 = CARTESIAN_POINT ( 'NONE',  ( -4.462107437047291292, 1508.188283896733537, 220.5629211818961721 ) ) ;
#85482 = CARTESIAN_POINT ( 'NONE',  ( 18.96271086799999850, 1416.819756528530206, 210.2433118287679861 ) ) ;
#85483 = CARTESIAN_POINT ( 'NONE',  ( -3.271538019026510202, 1454.292002138270163, 199.1638778078030043 ) ) ;
#85484 = CARTESIAN_POINT ( 'NONE',  ( 11.86716023049999968, 1432.353341358199941, 147.6509521729980179 ) ) ;
#85485 = CYLINDRICAL_SURFACE ( 'NONE', #2075, 2.000000000000006217 ) ;
#85487 = ADVANCED_FACE ( 'NONE', ( #20633 ), #25895, .F. ) ;
#85486 = CARTESIAN_POINT ( 'NONE',  ( 37.12039286075560085, 1440.913060386880034, 254.8318130490980309 ) ) ;
#85489 = CARTESIAN_POINT ( 'NONE',  ( -22.91663120903140083, 1507.606285602550088, 207.6071078552859888 ) ) ;
#85488 = CARTESIAN_POINT ( 'NONE',  ( -4.727379727993030301, 1421.625110441430024, 193.4326326425589855 ) ) ;
#85490 = CARTESIAN_POINT ( 'NONE',  ( 10.89381921772500839, 1427.223731764126796, 149.7143491514381708 ) ) ;
#85491 = ORIENTED_EDGE ( 'NONE', *, *, #20683, .F. ) ;
#85492 = CARTESIAN_POINT ( 'NONE',  ( 28.70874162694008547, 1526.306647125542668, 220.3434987316592526 ) ) ;
#85493 = AXIS2_PLACEMENT_3D ( 'NONE', #7677, #110139, #41833 ) ;
#85494 = CARTESIAN_POINT ( 'NONE',  ( -4.038582018749999669, 1515.598601288590089, 209.1218459616989946 ) ) ;
#85495 = CARTESIAN_POINT ( 'NONE',  ( 11.75869035672759999, 1519.551704408389924, 227.2994842695800060 ) ) ;
#85496 = CARTESIAN_POINT ( 'NONE',  ( 9.321267295856701551, 1447.491614812988928, 186.3095919917775518 ) ) ;
#85497 = CIRCLE ( 'NONE', #74827, 1.999999999999999556 ) ;
#85498 = CARTESIAN_POINT ( 'NONE',  ( -4.146782895030730387, 1426.018316030089863, 186.1121555109529879 ) ) ;
#85499 = DIRECTION ( 'NONE',  ( -0.9455185755993178454, 0.000000000000000000, 0.3255681544571537578 ) ) ;
#85500 = VECTOR ( 'NONE', #95309, 1000.000000000000114 ) ;
#85501 = CARTESIAN_POINT ( 'NONE',  ( 2.855157077230529694, 1508.551704408389924, 219.4496006082999884 ) ) ;
#85502 = CARTESIAN_POINT ( 'NONE',  ( 12.98226561589999939, 1414.913060387329779, 198.3280246956980193 ) ) ;
#85503 = CARTESIAN_POINT ( 'NONE',  ( -72.62010951785889290, 1383.782830401899901, 297.5846722543229816 ) ) ;
#85504 = CIRCLE ( 'NONE', #76572, 2.000000000000002665 ) ;
#85505 = CARTESIAN_POINT ( 'NONE',  ( 21.89882296440000076, 1452.148336636630120, 141.7804002450980079 ) ) ;
#85506 = DIRECTION ( 'NONE',  ( 0.000000000000000000, 0.000000000000000000, -1.000000000000000000 ) ) ;
#85507 = CARTESIAN_POINT ( 'NONE',  ( -2.048720034851359895, 1516.528429087750055, 201.4129680643380027 ) ) ;
#85509 = EDGE_LOOP ( 'NONE', ( #60575, #54824, #22537, #79707, #20443 ) ) ;
#85508 = CARTESIAN_POINT ( 'NONE',  ( 10.38805000968689995, 1451.723873411300019, 207.4476418283009878 ) ) ;
#85510 = AXIS2_PLACEMENT_3D ( 'NONE', #20021, #81037, #3261 ) ;
#85511 = CARTESIAN_POINT ( 'NONE',  ( -1.556370308520000023, 1414.996442553830093, 226.5294865815980074 ) ) ;
#85512 = CARTESIAN_POINT ( 'NONE',  ( -58.17684086589999737, 1383.136550875339935, 240.1300462906590099 ) ) ;
#85513 = CARTESIAN_POINT ( 'NONE',  ( 4.987078438843329131, 1508.551704408389924, 206.5718281456429963 ) ) ;
#85514 = ORIENTED_EDGE ( 'NONE', *, *, #109332, .T. ) ;
#85515 = ORIENTED_EDGE ( 'NONE', *, *, #94927, .T. ) ;
#85516 = CARTESIAN_POINT ( 'NONE',  ( 19.16562477733859993, 1509.252401821619969, 230.4506081681080047 ) ) ;
#85517 = CARTESIAN_POINT ( 'NONE',  ( -5.513264357029999729, 1374.913060387289988, 209.1218459572589836 ) ) ;
#85518 = CARTESIAN_POINT ( 'NONE',  ( 36.70747090514399957, 1437.748585611690032, 136.5500148930220234 ) ) ;
#85520 = CARTESIAN_POINT ( 'NONE',  ( 4.500000000000000000, 1448.210448412289907, 182.3842140122979743 ) ) ;
#85519 = CARTESIAN_POINT ( 'NONE',  ( 18.85453636469999950, 1434.822352678469997, 208.8963608210670202 ) ) ;
#85521 = B_SPLINE_CURVE_WITH_KNOTS ( 'NONE', 5,
 ( #67064, #16062, #58107, #58653, #49708, #93334 ),
 .UNSPECIFIED., .F., .F.,
 ( 6, 6 ),
 ( -107.6663712510000011, -41.52559413485549555 ),
 .UNSPECIFIED. ) ;
#85522 = CARTESIAN_POINT ( 'NONE',  ( 11.77118616850890120, 1479.407637630939917, 208.8749157105980032 ) ) ;
#85523 = B_SPLINE_CURVE_WITH_KNOTS ( 'NONE', 5,
 ( #33329, #7042, #102195, #110605, #14875, #101625, #51251, #17054, #57474, #108402, #6491, #24914, #23823, #85384, #66970, #49067, #99986, #15969 ),
 .UNSPECIFIED., .F., .F.,
 ( 6, 3, 3, 3, 3, 6 ),
 ( 30.30137870641080156, 39.81263101060000054, 43.27628380800000230, 45.00811020669999607, 46.73993660539999695, 49.32388343160000233 ),
 .UNSPECIFIED. ) ;
#85524 = CARTESIAN_POINT ( 'NONE',  ( -108.3070719650000058, 1383.318204079829911, 297.4475841893589632 ) ) ;
#85525 = CARTESIAN_POINT ( 'NONE',  ( -0.3328314641405109575, 1452.976685807730291, 183.2631399573310205 ) ) ;
#85526 = LINE ( 'NONE', #45227, #4878 ) ;
#85527 = CARTESIAN_POINT ( 'NONE',  ( 2.555976562930000195, 1409.169953449729974, 186.1677122907980220 ) ) ;
#85528 = CARTESIAN_POINT ( 'NONE',  ( 11.22085815260450126, 1416.913060341609935, 197.6243702213470215 ) ) ;
#85529 = CARTESIAN_POINT ( 'NONE',  ( 40.27219824716285501, 1443.778079288244953, 137.1299607049654128 ) ) ;
#85530 = CARTESIAN_POINT ( 'NONE',  ( -9.205625138637591576, 1450.204495207709897, 208.8293812459489800 ) ) ;
#85531 = CARTESIAN_POINT ( 'NONE',  ( -14.53343879676760153, 1421.577982565850107, 203.5955589198449900 ) ) ;
#85532 = CARTESIAN_POINT ( 'NONE',  ( -2.383806472443930069, 1450.585402367019924, 184.2442155348799986 ) ) ;
#85533 = CARTESIAN_POINT ( 'NONE',  ( 1.578863831189999845, 1464.872486508430029, 236.9579546960979997 ) ) ;
#85534 = ORIENTED_EDGE ( 'NONE', *, *, #75423, .T. ) ;
#85535 = CARTESIAN_POINT ( 'NONE',  ( 4.694859187580000537, 1472.563992416889960, 187.6273510758990142 ) ) ;
#85536 = CARTESIAN_POINT ( 'NONE',  ( -43.71744118499999843, 1445.751715858400075, 270.2202180345980196 ) ) ;
#85537 = DIRECTION ( 'NONE',  ( -1.000000000000000000, 0.000000000000000000, 0.000000000000000000 ) ) ;
#85538 = CARTESIAN_POINT ( 'NONE',  ( 21.97938480441199971, 1506.433683733499947, 208.7396655020440051 ) ) ;
#85539 = CARTESIAN_POINT ( 'NONE',  ( 15.68240438299999973, 1430.131679172730173, 190.9216979817980189 ) ) ;
#85540 = CARTESIAN_POINT ( 'NONE',  ( -1.174542368893330082E-08, 1473.852152221930055, 263.0553943314729963 ) ) ;
#85541 = CARTESIAN_POINT ( 'NONE',  ( 10.41177329615350011, 1460.024665156439823, 205.9063136364349873 ) ) ;
#85543 = EDGE_CURVE ( 'NONE', #78370, #87307, #105379, .T. ) ;
#85542 = CARTESIAN_POINT ( 'NONE',  ( -1.350316101520000256, 1416.274718424630009, 228.0027273083979935 ) ) ;
#85544 = CARTESIAN_POINT ( 'NONE',  ( -4.956485740179999766, 1416.161662173230070, 232.1584812440979988 ) ) ;
#85545 = CARTESIAN_POINT ( 'NONE',  ( -1.993348244980000183, 1477.149067790089930, 198.9137608980990137 ) ) ;
#85546 = CARTESIAN_POINT ( 'NONE',  ( -108.1994964509999875, 1388.325478153710037, 310.2320290272589887 ) ) ;
#85547 = CARTESIAN_POINT ( 'NONE',  ( -0.7507406189636354199, 1485.270421196727966, 181.9807069647154378 ) ) ;
#85548 = CARTESIAN_POINT ( 'NONE',  ( -6.608559145320131556, 1359.356750036984067, 209.6218459617033432 ) ) ;
#85549 = CARTESIAN_POINT ( 'NONE',  ( -45.48544670104310228, 1437.736077969160078, 266.1937296958689672 ) ) ;
#85550 = CARTESIAN_POINT ( 'NONE',  ( 13.91486264393430083, 1509.328966950709855, 234.3828252105219860 ) ) ;
#85551 = CYLINDRICAL_SURFACE ( 'NONE', #105665, 1.999999999999999556 ) ;
#85552 = ORIENTED_EDGE ( 'NONE', *, *, #76033, .T. ) ;
#85553 = CARTESIAN_POINT ( 'NONE',  ( -3.261652325025000021, 1516.939580991450157, 209.1351299096569960 ) ) ;
#85554 = CARTESIAN_POINT ( 'NONE',  ( -5.397656279289999581, 1433.838088931449875, 154.6405518360980125 ) ) ;
#85555 = B_SPLINE_CURVE_WITH_KNOTS ( 'NONE', 3,
 ( #1379, #52897, #44491, #71384 ),
 .UNSPECIFIED., .F., .F.,
 ( 4, 4 ),
 ( 0.000000000000000000, 1.000000000000000000 ),
 .UNSPECIFIED. ) ;
#85556 = CARTESIAN_POINT ( 'NONE',  ( -26.46631751370579977, 1441.292691208669794, 137.7246565571259964 ) ) ;
#85557 = CARTESIAN_POINT ( 'NONE',  ( 7.367553984658170130, 1426.317790364889788, 212.6468799033240202 ) ) ;
#85558 = CARTESIAN_POINT ( 'NONE',  ( -26.62761621350209751, 1450.720643774079917, 136.4854395823020070 ) ) ;
#85559 = ORIENTED_EDGE ( 'NONE', *, *, #106208, .T. ) ;
#85560 = CARTESIAN_POINT ( 'NONE',  ( 23.84883432139999826, 1428.816474285830054, 231.9514347523980291 ) ) ;
#85562 = CYLINDRICAL_SURFACE ( 'NONE', #83892, 1.999999999999996225 ) ;
#85561 = CARTESIAN_POINT ( 'NONE',  ( -11.18131722815940066, 1491.896203582180078, 207.0175328158499610 ) ) ;
#85563 = CARTESIAN_POINT ( 'NONE',  ( 5.004475574535000248, 1517.026025493960105, 201.3999380438669959 ) ) ;
#85564 = CARTESIAN_POINT ( 'NONE',  ( -22.15139830485364669, 1451.884836739148795, 222.5180298453051364 ) ) ;
#85565 = CARTESIAN_POINT ( 'NONE',  ( 8.413970532630001387, 1428.089005924990033, 212.8939830477889927 ) ) ;
#85566 = CARTESIAN_POINT ( 'NONE',  ( -3.852420766530000318, 1461.443526049990169, 228.3501068971989980 ) ) ;
#85567 = CARTESIAN_POINT ( 'NONE',  ( 20.92767404034498568, 1511.187213306747708, 182.8548762971663848 ) ) ;
#85568 = VERTEX_POINT ( 'NONE', #4952 ) ;
#85569 = CARTESIAN_POINT ( 'NONE',  ( -8.632231662151090390, 1408.838363546260098, 270.3814370203099884 ) ) ;
#85570 = CARTESIAN_POINT ( 'NONE',  ( 9.106286253189209035, 1419.188153054899885, 232.8697977723819861 ) ) ;
#85571 = DIRECTION ( 'NONE',  ( -1.305148739725796033E-31, 1.000000000000000000, -1.836970198721029688E-16 ) ) ;
#85573 = ORIENTED_EDGE ( 'NONE', *, *, #39109, .F. ) ;
#85572 = CARTESIAN_POINT ( 'NONE',  ( -31.23437356469453263, 1523.382868172864164, 195.3468678195118287 ) ) ;
#85574 = ORIENTED_EDGE ( 'NONE', *, *, #81471, .T. ) ;
#85575 = CARTESIAN_POINT ( 'NONE',  ( -23.11517254792869736, 1409.837221116860064, 209.7713657907539755 ) ) ;
#85576 = ADVANCED_FACE ( 'NONE', ( #13334 ), #58982, .T. ) ;
#85577 = CARTESIAN_POINT ( 'NONE',  ( -0.8766014945788880297, 1410.319220143099983, 185.2092218620130097 ) ) ;
#85578 = CARTESIAN_POINT ( 'NONE',  ( -103.9363405334299983, 1366.350733876289951, 309.3918666868790410 ) ) ;
#85579 = CARTESIAN_POINT ( 'NONE',  ( -4.418986906789999836, 1428.481734779130193, 91.31218443469779800 ) ) ;
#85580 = AXIS2_PLACEMENT_3D ( 'NONE', #86111, #69337, #9953 ) ;
#85581 = AXIS2_PLACEMENT_3D ( 'NONE', #59666, #33886, #25473 ) ;
#85582 = CARTESIAN_POINT ( 'NONE',  ( -19.36527534830760189, 1454.515909355379790, 193.8667981925449908 ) ) ;
#85583 = CARTESIAN_POINT ( 'NONE',  ( -19.03679519810000187, 1420.834773504230043, 223.8082884180979875 ) ) ;
#85584 = CARTESIAN_POINT ( 'NONE',  ( 41.21152668593589397, 1456.890786767240115, 267.1395868360899613 ) ) ;
#85585 = CARTESIAN_POINT ( 'NONE',  ( -2.807011052872784962, 1466.843255166033032, 235.0768055671881029 ) ) ;
#85586 = CARTESIAN_POINT ( 'NONE',  ( -4.979428188690000034, 1427.783661369190213, 201.1078272686790172 ) ) ;
#85587 = CARTESIAN_POINT ( 'NONE',  ( 7.322105067625000352, 1516.572193931679976, 206.2485165713470110 ) ) ;
#85588 = EDGE_LOOP ( 'NONE', ( #69761, #59120, #63463, #59145 ) ) ;
#85589 = CARTESIAN_POINT ( 'NONE',  ( -11.39963766959999880, 1433.910854737510135, 151.4262557347980191 ) ) ;
#85590 = CARTESIAN_POINT ( 'NONE',  ( 15.16689668216860021, 1513.426431439620046, 194.7669068285340188 ) ) ;
#85591 = DIRECTION ( 'NONE',  ( 0.1196801093690024326, -0.9928125056733640985, 0.000000000000000000 ) ) ;
#85592 = VERTEX_POINT ( 'NONE', #109091 ) ;
#85593 = CARTESIAN_POINT ( 'NONE',  ( 4.544860949943270612, 1508.551704410290085, 205.1599016910289777 ) ) ;
#85594 = CARTESIAN_POINT ( 'NONE',  ( 25.81862830083710136, 1451.947416646700049, 135.6228482220020055 ) ) ;
#85595 = CARTESIAN_POINT ( 'NONE',  ( -14.81380081930790027, 1513.941944658620059, 194.2161487120590095 ) ) ;
#85596 = FACE_OUTER_BOUND ( 'NONE', #105859, .T. ) ;
#85597 = CARTESIAN_POINT ( 'NONE',  ( 7.854071199910000800, 1421.721864916329878, 195.9105866898989916 ) ) ;
#85598 = CARTESIAN_POINT ( 'NONE',  ( 18.67334359839999891, 1410.488446969229926, 194.6898139266980081 ) ) ;
#85599 = CARTESIAN_POINT ( 'NONE',  ( -3.589794993429999970, 1496.402118238189814, 198.3466359645990167 ) ) ;
#85600 = CARTESIAN_POINT ( 'NONE',  ( 0.3071698501290910377, 1408.923786994839929, 186.4998763197650078 ) ) ;
#85602 = DIRECTION ( 'NONE',  ( -0.5877852522924629231, 0.000000000000000000, 0.8090169943749548898 ) ) ;
#85601 = CARTESIAN_POINT ( 'NONE',  ( 1.113930986489999775, 1416.316097248230108, 233.2037843969979747 ) ) ;
#85603 = CARTESIAN_POINT ( 'NONE',  ( -16.54106930751559190, 1524.860077346004800, 180.8551645285683662 ) ) ;
#85604 = CARTESIAN_POINT ( 'NONE',  ( 10.96947504439999932, 1432.347663815810165, 151.7701302545979729 ) ) ;
#85605 = AXIS2_PLACEMENT_3D ( 'NONE', #76239, #40425, #110386 ) ;
#85606 = CARTESIAN_POINT ( 'NONE',  ( -13.29669133360000188, 1379.596949712730066, 212.3329758012989714 ) ) ;
#85607 = CARTESIAN_POINT ( 'NONE',  ( 3.410069871122496821, 1417.828849658407762, 234.2623983030260320 ) ) ;
#85608 = VERTEX_POINT ( 'NONE', #108521 ) ;
#85609 = CARTESIAN_POINT ( 'NONE',  ( 12.18581614772429944, 1415.088012641449950, 220.9247406374639979 ) ) ;
#85610 = B_SPLINE_CURVE_WITH_KNOTS ( 'NONE', 5,
 ( #102506, #25796, #59995, #94673, #43185, #77337, #34768, #80078, #72794 ),
 .UNSPECIFIED., .F., .F.,
 ( 6, 3, 6 ),
 ( 234.3510616479999840, 237.3878297990000021, 239.1631355520000000 ),
 .UNSPECIFIED. ) ;
#85611 = LINE ( 'NONE', #66652, #26611 ) ;
#85612 = DIRECTION ( 'NONE',  ( 0.000000000000000000, 1.000000000000000000, 0.000000000000000000 ) ) ;
#85613 = EDGE_CURVE ( 'NONE', #41682, #102562, #48153, .T. ) ;
#85614 = CARTESIAN_POINT ( 'NONE',  ( -11.73166134470000088, 1389.808667801499951, 203.8872188440389834 ) ) ;
#85615 = CARTESIAN_POINT ( 'NONE',  ( 9.936711670530231189, 1422.499099451789789, 212.2361507557569951 ) ) ;
#85616 = CARTESIAN_POINT ( 'NONE',  ( -34.03169827300909844, 1450.436082776269814, 136.2420522946879942 ) ) ;
#85617 = EDGE_CURVE ( 'NONE', #98935, #84728, #53526, .T. ) ;
#85618 = CARTESIAN_POINT ( 'NONE',  ( -10.97606361528359997, 1462.640992382440118, 207.8491965332009954 ) ) ;
#85619 = CARTESIAN_POINT ( 'NONE',  ( -28.52406121949999829, 1451.758636109829922, 255.3819207742980097 ) ) ;
#85620 = CARTESIAN_POINT ( 'NONE',  ( -8.860022299467271267, 1384.827477254669930, 218.6840310215359864 ) ) ;
#85621 = ADVANCED_FACE ( 'NONE', ( #49189 ), #67948, .T. ) ;
#85622 = CARTESIAN_POINT ( 'NONE',  ( 11.92834938799999911, 1433.441347791240105, 150.0273619249979902 ) ) ;
#85623 = CARTESIAN_POINT ( 'NONE',  ( 20.41675352909999930, 1443.170379823910025, 219.6133835466979747 ) ) ;
#85625 = EDGE_CURVE ( 'NONE', #7502, #89045, #98593, .T. ) ;
#85624 = CARTESIAN_POINT ( 'NONE',  ( -9.850099335591719907, 1461.427211915769931, 209.3139255674489903 ) ) ;
#85626 = CARTESIAN_POINT ( 'NONE',  ( 18.29793613913720307, 1429.923626251509859, 201.0778461450230168 ) ) ;
#85627 = CARTESIAN_POINT ( 'NONE',  ( 11.99876342961469966, 1425.975962788000288, 199.1838357467620142 ) ) ;
#85628 = CARTESIAN_POINT ( 'NONE',  ( 9.503369802446668402, 1463.703997095049999, 211.5558214296420090 ) ) ;
#85629 = EDGE_CURVE ( 'NONE', #44333, #65430, #35122, .T. ) ;
#85630 = CARTESIAN_POINT ( 'NONE',  ( -3.497240116209999972, 1486.046665812830042, 182.0896961123980020 ) ) ;
#85631 = CARTESIAN_POINT ( 'NONE',  ( 8.792013403107649339, 1398.173719835249358, 218.8041918917098769 ) ) ;
#85632 = CARTESIAN_POINT ( 'NONE',  ( -30.28584401579999863, 1510.098977584829981, 208.7842246005000106 ) ) ;
#85633 = AXIS2_PLACEMENT_3D ( 'NONE', #7853, #16776, #92961 ) ;
#85634 = CARTESIAN_POINT ( 'NONE',  ( 23.30790377549999803, 1410.912174208729766, 212.5128193344479826 ) ) ;
#85635 = PLANE ( 'NONE',  #52085 ) ;
#85636 = CARTESIAN_POINT ( 'NONE',  ( 2.310235562019999888E-16, 1426.500992774829911, 146.0666368882980066 ) ) ;
#85637 = CARTESIAN_POINT ( 'NONE',  ( -9.129808743239919977, 1383.863787745319996, 218.5279288296370055 ) ) ;
#85638 = CARTESIAN_POINT ( 'NONE',  ( 11.62179174939422666, 1434.999149959319766, 151.3709551977956380 ) ) ;
#85639 = CARTESIAN_POINT ( 'NONE',  ( 5.076283936602980162, 1469.790178403189884, 187.8425608794819937 ) ) ;
#85640 = CARTESIAN_POINT ( 'NONE',  ( -6.936398393775000670, 1516.667393516340098, 213.1585948090369698 ) ) ;
#85641 = ADVANCED_FACE ( 'NONE', ( #86625 ), #42983, .F. ) ;
#85642 = CARTESIAN_POINT ( 'NONE',  ( -16.44758872147649953, 1420.160613029469914, 207.7350616873459899 ) ) ;
#85643 = CARTESIAN_POINT ( 'NONE',  ( 0.1730928914583289846, 1478.515575105890093, 182.1581534200829822 ) ) ;
#85645 = ORIENTED_EDGE ( 'NONE', *, *, #2971, .T. ) ;
#85644 = CARTESIAN_POINT ( 'NONE',  ( 3.775107361939999961, 1441.398020315490157, 217.5130260360689931 ) ) ;
#85646 = CARTESIAN_POINT ( 'NONE',  ( -1.546896711300000060, 1416.831925149330118, 228.0210885246980297 ) ) ;
#85647 = AXIS2_PLACEMENT_3D ( 'NONE', #24310, #13500, #91881 ) ;
#85648 = CARTESIAN_POINT ( 'NONE',  ( -38.51626067329515735, 1444.740067931809563, 136.9078731636151360 ) ) ;
#85649 = CARTESIAN_POINT ( 'NONE',  ( 3.347801439296141268, 1512.187213306747481, 176.1543725841967500 ) ) ;
#85650 = CARTESIAN_POINT ( 'NONE',  ( -109.7178215300000090, 1384.906467897089897, 297.0861894953589513 ) ) ;
#85651 = ORIENTED_EDGE ( 'NONE', *, *, #100040, .T. ) ;
#85652 = B_SPLINE_SURFACE_WITH_KNOTS ( 'NONE', 5, 5, ( 
 ( #85238, #94756, #33187, #58960, #76305, #60632 ),
 ( #76864, #50563, #42708, #175, #84689, #67378 ),
 ( #9636, #101476, #18033, #86353, #7988, #68478 ),
 ( #42154, #58412, #102579, #25877, #60077, #92538 ),
 ( #94193, #17463, #43810, #43265, #77412, #34847 ),
 ( #69036, #32648, #27555, #62869, #79635, #2392 ),
 ( #62294, #52771, #53903, #88038, #69592, #79085 ),
 ( #10199, #37612, #88580, #80165, #70704, #78519 ),
 ( #44938, #36510, #105935, #104816, #11322, #12401 ) ),
 .UNSPECIFIED., .F., .F., .F.,
 ( 6, 3, 6 ),
 ( 6, 6 ),
 ( -9.415047822849649119E-06, 2.934247638910000067, 4.839418697517819723 ),
 ( 0.000000000000000000, 1.000009415047820038 ),
 .UNSPECIFIED. ) ;
#85654 = ADVANCED_FACE ( 'NONE', ( #77142 ), #8796, .T. ) ;
#85653 = DIRECTION ( 'NONE',  ( 1.000000000000000000, 0.000000000000000000, 1.989556701369999986E-13 ) ) ;
#85655 = CARTESIAN_POINT ( 'NONE',  ( -14.24367202074330052, 1390.369523491529890, 210.8398262857290035 ) ) ;
#85656 = CARTESIAN_POINT ( 'NONE',  ( -17.27701495550000033, 1415.425644477229980, 211.8855821374380071 ) ) ;
#85657 = CYLINDRICAL_SURFACE ( 'NONE', #49937, 2.999999999999999556 ) ;
#85658 = ADVANCED_FACE ( 'NONE', ( #8802 ), #48199, .T. ) ;
#85659 = CARTESIAN_POINT ( 'NONE',  ( -6.958135218038119518, 1434.179671701880125, 214.2270546061249945 ) ) ;
#85660 = DIRECTION ( 'NONE',  ( -5.980589973904019347E-17, 1.000000000000000000, -1.736889445713099699E-16 ) ) ;
#85661 = DIRECTION ( 'NONE',  ( -1.987898964669120000E-13, 0.000000000000000000, 1.000000000000000000 ) ) ;
#85662 = DIRECTION ( 'NONE',  ( 0.000000000000000000, 1.000000000000000000, 0.000000000000000000 ) ) ;
#85663 = CARTESIAN_POINT ( 'NONE',  ( -10.54817843220000029, 1391.913060387289988, 204.8953073741390085 ) ) ;
#85664 = B_SPLINE_SURFACE_WITH_KNOTS ( 'NONE', 5, 5, ( 
 ( #29116, #63302, #97420, #38607, #72786, #54887 ),
 ( #12301, #3940, #55435, #63845, #72245, #30201 ),
 ( #64392, #98513, #55983, #90106, #13389, #47577 ),
 ( #81701, #49240, #64940, #75547, #5571, #6663 ),
 ( #109144, #66051, #50352, #109683, #48692, #82816 ),
 ( #23990, #84477, #39722, #49788, #41383, #31310 ) ),
 .UNSPECIFIED., .F., .F., .F.,
 ( 6, 6 ),
 ( 6, 6 ),
 ( 8.912615240089998281, 11.89398684980000098 ),
 ( 0.000000000000000000, 1.457234320079999979 ),
 .UNSPECIFIED. ) ;
#85665 = CARTESIAN_POINT ( 'NONE',  ( -75.33569739729779258, 1385.137803142289840, 276.0448183544650647 ) ) ;
#85666 = CARTESIAN_POINT ( 'NONE',  ( 13.01671764799699993, 1416.842625005220043, 196.3343525426479914 ) ) ;
#85667 = CARTESIAN_POINT ( 'NONE',  ( 11.27279626876990015, 1426.317628015930040, 206.4670722515049874 ) ) ;
#85668 = EDGE_LOOP ( 'NONE', ( #18642, #82148, #10954, #21177 ) ) ;
#85669 = CIRCLE ( 'NONE', #108949, 0.9999999999998898659 ) ;
#85670 = ADVANCED_FACE ( 'NONE', ( #3213 ), #54717, .F. ) ;
#85671 = DIRECTION ( 'NONE',  ( -1.000000000000000000, 0.000000000000000000, 0.000000000000000000 ) ) ;
#85673 = EDGE_LOOP ( 'NONE', ( #83653, #46549 ) ) ;
#85672 = CARTESIAN_POINT ( 'NONE',  ( 5.508554876272072853, 1427.333971811663332, 137.0999999980980135 ) ) ;
#85674 = CARTESIAN_POINT ( 'NONE',  ( 4.889046445280000874, 1473.841289047790042, 218.9857726612289923 ) ) ;
#85675 = AXIS2_PLACEMENT_3D ( 'NONE', #38949, #23255, #57454 ) ;
#85676 = ORIENTED_EDGE ( 'NONE', *, *, #94494, .F. ) ;
#85677 =( BOUNDED_SURFACE ( )  B_SPLINE_SURFACE ( 3, 2, ( 
 ( #49566, #64729, #56304 ),
 ( #90434, #66379, #83695 ),
 ( #13712, #47898, #31636 ),
 ( #74225, #41146, #6448 ) ),
 .UNSPECIFIED., .F., .F., .T. ) 
 B_SPLINE_SURFACE_WITH_KNOTS ( ( 4, 4 ),
 ( 3, 3 ),
 ( 0.000000000000000000, 0.0002960034161023845684 ),
 ( 0.000000000000000000, 1.000000000000000000 ),
 .UNSPECIFIED. ) 
 GEOMETRIC_REPRESENTATION_ITEM ( )  RATIONAL_B_SPLINE_SURFACE ( (
 ( 1.000000000000000000, 0.8070209408749979829, 1.000000000000000000),
 ( 1.000000000000000000, 0.8071723757218428608, 1.000000000000000000),
 ( 1.000000000000000000, 0.8072480346917620952, 1.000000000000000000),
 ( 1.000000000000000000, 0.8072480644198127830, 1.000000000000000000) ) ) 
 REPRESENTATION_ITEM ( '' )  SURFACE ( )  );
#85678 = CARTESIAN_POINT ( 'NONE',  ( -17.84338787571902074, 1512.187213306747481, 237.8836641337663309 ) ) ;
#85679 = CARTESIAN_POINT ( 'NONE',  ( -7.482952933474933843, 1364.121751949525560, 208.3718459617061285 ) ) ;
#85680 = CARTESIAN_POINT ( 'NONE',  ( -10.94209233289999972, 1492.979988313090189, 207.3926202980489961 ) ) ;
#85681 = CARTESIAN_POINT ( 'NONE',  ( 38.96090183549657127, 1452.356242234835236, 269.5922817352261518 ) ) ;
#85682 = CARTESIAN_POINT ( 'NONE',  ( -11.60004869885203682, 1428.983126981193436, 134.0999999980979851 ) ) ;
#85683 = CARTESIAN_POINT ( 'NONE',  ( 13.40566205669149902, 1429.098591087019940, 222.0107402452829888 ) ) ;
#85684 = CARTESIAN_POINT ( 'NONE',  ( -1778.930368298719941, -2340.220200558880151, 9317.326275786501355 ) ) ;
#85685 = CARTESIAN_POINT ( 'NONE',  ( 5.296871147660000112, 1447.430519322290138, 200.3058700119589730 ) ) ;
#85686 = DIRECTION ( 'NONE',  ( -5.980589973904019347E-17, 1.000000000000000000, -1.736889445713099699E-16 ) ) ;
#85687 = CARTESIAN_POINT ( 'NONE',  ( -10.56833826840790813, 1367.981913465304388, 208.3718459617010978 ) ) ;
#85688 = CARTESIAN_POINT ( 'NONE',  ( -2.124993027169999493, 1455.769608825389923, 199.7713323867489805 ) ) ;
#85689 = CARTESIAN_POINT ( 'NONE',  ( 3.253141137235000091, 1516.858171774179937, 205.8542424163969997 ) ) ;
#85690 = AXIS2_PLACEMENT_3D ( 'NONE', #62143, #2241, #79478 ) ;
#85691 = DIRECTION ( 'NONE',  ( 0.000000000000000000, 1.000000000000000000, 0.000000000000000000 ) ) ;
#85692 = B_SPLINE_SURFACE_WITH_KNOTS ( 'NONE', 5, 5, ( 
 ( #86489, #77553, #76436, #95452, #856, #78093, #34983, #110589, #103267 ),
 ( #97654, #36104, #97109, #98193, #27695, #96560, #20375, #11995, #105513 ),
 ( #104400, #4159, #70845, #12546, #87614, #104954, #54580, #3624, #38286 ),
 ( #88715, #61881, #71947, #46725, #55128, #19832, #45630, #21466, #46178 ),
 ( #72468, #80858, #80308, #106598, #88166, #37754, #47254, #36647, #70290 ),
 ( #28804, #79217, #95997, #106059, #55676, #29337, #63001, #63538, #29883 ),
 ( #89796, #28244, #20924, #89250, #64074, #11454, #45075, #13068, #62434 ),
 ( #71397, #1968, #3076, #19266, #53469, #10902, #2525, #54037, #79769 ),
 ( #37203, #82510, #14737, #40493, #98746, #107147, #75221, #15274, #30440 ),
 ( #73574, #64626, #92540, #99280, #22006, #23128, #73011, #74120, #66285 ),
 ( #13615, #107705, #56203, #109373, #99836, #57333, #41043, #6886, #49467 ),
 ( #15806, #91459, #32650, #58414, #48925, #56760, #57870, #108249, #47803 ),
 ( #83053, #24228, #6346, #31539, #65715, #83587, #4693, #100933, #30990 ),
 ( #74671, #108804, #90897, #81938, #66827, #39397, #14181, #39948, #92000 ),
 ( #32098, #81378, #100402, #38833, #90335, #5241, #65165, #48367, #5808 ),
 ( #23685, #22556, #75762, #43812, #94759, #109909, #24765, #42156, #33190 ),
 ( #67930, #67380, #102581, #41608, #42710, #34849, #60079, #93095, #76308 ),
 ( #77959, #68480, #69038, #110458, #51116, #1267, #50565, #16367, #103140 ),
 ( #86355, #85803, #9101, #50012, #94195, #102037, #84691, #7990, #25324 ),
 ( #101478, #59520, #58962, #18035, #26440, #33735, #93632, #35405, #17465 ),
 ( #25879, #69594, #60634, #16911, #52227, #84145, #34298, #103712, #85240 ),
 ( #7445, #43268, #8536, #9638, #76865, #51666, #177, #27013, #61202 ),
 ( #95317, #77414, #719, #4031, #10769, #105937, #80167, #11324, #54991 ),
 ( #2395, #72340, #46588, #29754, #53905, #63405, #1833, #11865, #38159 ),
 ( #29215, #3485, #45495, #89114, #97520, #36512, #106469, #20246, #20790 ),
 ( #37614, #71255, #63944, #37060, #12403, #18578, #28666, #104819, #80723 ),
 ( #95863, #86911, #54447, #52773, #96983, #79637, #2940, #10202, #44378 ),
 ( #44940, #88583, #46038, #71816, #28106, #61740, #78521, #87480, #62296 ),
 ( #35967, #19702, #62871, #70158, #104268, #27557, #19130, #53332, #79087 ),
 ( #88040, #70706, #96423, #105377, #12945, #91865, #31957, #47126, #72878 ) ),
 .UNSPECIFIED., .F., .F., .F.,
 ( 6, 3, 3, 3, 3, 3, 3, 3, 3, 6 ),
 ( 6, 3, 6 ),
 ( 24.21110745940000086, 25.10805053119999997, 26.03075347299999720, 28.79941466429999863, 31.56807585549999828, 38.94969915669999949, 55.51300259679999982, 72.07630603690000726, 88.69360427520000201, 143.4983655759999976 ),
 ( 0.000000000000000000, 1.000000000000000000, 2.000000000000000000 ),
 .UNSPECIFIED. ) ;
#85693 = CARTESIAN_POINT ( 'NONE',  ( -15.79903022766779941, 1414.763965172529879, 226.8475472940190230 ) ) ;
#85694 = CARTESIAN_POINT ( 'NONE',  ( 16.81223453394349932, 1414.913060391199906, 210.6693087035600058 ) ) ;
#85696 = ORIENTED_EDGE ( 'NONE', *, *, #98574, .T. ) ;
#85695 = CARTESIAN_POINT ( 'NONE',  ( -3.355411835910000029, 1495.471247818590200, 219.8040188672989927 ) ) ;
#85697 = EDGE_CURVE ( 'NONE', #69449, #82812, #75011, .T. ) ;
#85698 = CARTESIAN_POINT ( 'NONE',  ( 0.000000000000000000, 1408.913060387329779, 217.9908631324380224 ) ) ;
#85699 = ORIENTED_EDGE ( 'NONE', *, *, #88708, .F. ) ;
#85700 = CARTESIAN_POINT ( 'NONE',  ( -16.78028220709281726, 1513.363094763815525, 221.9574106988646065 ) ) ;
#85701 = CARTESIAN_POINT ( 'NONE',  ( -24.38832783710000029, 1430.357083412530073, 206.4809742753880073 ) ) ;
#85703 = CARTESIAN_POINT ( 'NONE',  ( 17.38138781036309766, 1410.742412905310175, 192.4657863012999712 ) ) ;
#85702 = CARTESIAN_POINT ( 'NONE',  ( -10.94965103403530016, 1425.287425078169917, 130.8065909167059999 ) ) ;
#85704 = CARTESIAN_POINT ( 'NONE',  ( 3.462948796544999652, 1516.956048353049937, 211.4063724288770061 ) ) ;
#85705 = ADVANCED_FACE ( 'NONE', ( #23817 ), #55816, .F. ) ;
#85706 = CARTESIAN_POINT ( 'NONE',  ( 28.64565192311250286, 1510.024564594433514, 200.2014960864728437 ) ) ;
#85707 = CARTESIAN_POINT ( 'NONE',  ( 21.53712143570577453, 1523.621879633029039, 234.3036048850995883 ) ) ;
#85708 = CARTESIAN_POINT ( 'NONE',  ( -11.43729524049999924, 1425.481262536329950, 144.1593964292979990 ) ) ;
#85709 = CARTESIAN_POINT ( 'NONE',  ( -13.00682114438060033, 1379.342060573179879, 208.5822149791590334 ) ) ;
#85710 = CARTESIAN_POINT ( 'NONE',  ( 17.11935957328527991, 1460.306514732013738, 228.6623330438524420 ) ) ;
#85711 = CARTESIAN_POINT ( 'NONE',  ( 3.096514233597529753, 1508.551704408389924, 214.0351581889520105 ) ) ;
#85712 = CARTESIAN_POINT ( 'NONE',  ( -36.44137682827670233, 1437.619458494599712, 136.5441383857150015 ) ) ;
#85713 = EDGE_LOOP ( 'NONE', ( #51513, #64016, #29976, #66687 ) ) ;
#85714 = CARTESIAN_POINT ( 'NONE',  ( 7.050167510270000548, 1396.339668515729954, 198.4643683982980065 ) ) ;
#85715 = CARTESIAN_POINT ( 'NONE',  ( 9.655324750296419012, 1461.352300578269933, 207.1780675101539941 ) ) ;
#85716 = CARTESIAN_POINT ( 'NONE',  ( -16.48650050839999892, 1458.966229476530089, 230.7111281069979896 ) ) ;
#85717 = ORIENTED_EDGE ( 'NONE', *, *, #53861, .F. ) ;
#85718 = VERTEX_POINT ( 'NONE', #6485 ) ;
#85719 = CARTESIAN_POINT ( 'NONE',  ( 8.916387934133441107, 1452.089085741889903, 211.7557271715180320 ) ) ;
#85720 = CARTESIAN_POINT ( 'NONE',  ( -1.910237665331893986, 1487.499208352387313, 219.7920233817232543 ) ) ;
#85721 = EDGE_CURVE ( 'NONE', #23359, #21788, #103690, .T. ) ;
#85722 = CARTESIAN_POINT ( 'NONE',  ( -14.21053568732289918, 1380.204026121820107, 210.6677758705890255 ) ) ;
#85723 = CARTESIAN_POINT ( 'NONE',  ( -14.74124171903659963, 1508.249207875330058, 209.5562123098220013 ) ) ;
#85724 = CARTESIAN_POINT ( 'NONE',  ( -19.34729233231120205, 1486.470064436709890, 189.5887045964369975 ) ) ;
#85725 = AXIS2_PLACEMENT_3D ( 'NONE', #39349, #49417, #108200 ) ;
#85726 = CARTESIAN_POINT ( 'NONE',  ( 27.36889244077043415, 1509.257027140795799, 206.1683652123398645 ) ) ;
#85727 = CARTESIAN_POINT ( 'NONE',  ( 1.026021462112689964, 1420.779496623759997, 182.9306845227040128 ) ) ;
#85728 = CARTESIAN_POINT ( 'NONE',  ( 10.48352362072680144, 1451.966107083780116, 207.9936217224200163 ) ) ;
#85729 = CARTESIAN_POINT ( 'NONE',  ( -5.144873395449999443, 1502.885538352589947, 229.8910404859989853 ) ) ;
#85730 = CARTESIAN_POINT ( 'NONE',  ( -106.3822989043390095, 1384.893588603729995, 297.0069513608490297 ) ) ;
#85731 = ORIENTED_EDGE ( 'NONE', *, *, #39288, .T. ) ;
#85732 = CARTESIAN_POINT ( 'NONE',  ( 1.706797785944999868, 1517.164987839469859, 203.3324512698969784 ) ) ;
#85733 = CARTESIAN_POINT ( 'NONE',  ( -7.332063977575000280, 1516.939491476980038, 209.1325772641960157 ) ) ;
#85734 = ORIENTED_EDGE ( 'NONE', *, *, #80239, .T. ) ;
#85735 = CARTESIAN_POINT ( 'NONE',  ( 11.78683996080030028, 1427.664868936200037, 147.4634367502030159 ) ) ;
#85736 = CIRCLE ( 'NONE', #64343, 1.999999999999999556 ) ;
#85737 = EDGE_CURVE ( 'NONE', #9923, #95978, #108954, .T. ) ;
#85738 = CARTESIAN_POINT ( 'NONE',  ( 2.968351152030138440, 1512.111360402368518, 217.0109328861994982 ) ) ;
#85739 = ORIENTED_EDGE ( 'NONE', *, *, #58216, .T. ) ;
#85740 = CARTESIAN_POINT ( 'NONE',  ( -13.79047275900000002, 1415.263254653229978, 220.8845754465980065 ) ) ;
#85741 = CARTESIAN_POINT ( 'NONE',  ( -12.53676446056685378, 1442.773887286369018, 169.5333422587011114 ) ) ;
#85742 = CARTESIAN_POINT ( 'NONE',  ( -16.99050533527280038, 1420.323706995179919, 203.8408272025779979 ) ) ;
#85743 = CARTESIAN_POINT ( 'NONE',  ( -3.378218165227587555, 1488.703315969531104, 219.4764361902140877 ) ) ;
#85744 = CARTESIAN_POINT ( 'NONE',  ( -5.441602405930001218, 1420.475810304129936, 186.6133007815980136 ) ) ;
#85745 = VECTOR ( 'NONE', #11770, 1000.000000000000000 ) ;
#85746 = EDGE_CURVE ( 'NONE', #50492, #86906, #105150, .T. ) ;
#85747 = CARTESIAN_POINT ( 'NONE',  ( 10.58168742575649901, 1469.969853788360069, 207.1021894818239844 ) ) ;
#85748 = DIRECTION ( 'NONE',  ( -0.9942586961433764747, -0.000000000000000000, -0.1070030146457237041 ) ) ;
#85749 = CARTESIAN_POINT ( 'NONE',  ( 6.225972109890000716, 1494.795958560490135, 219.7811165620990153 ) ) ;
#85750 = CARTESIAN_POINT ( 'NONE',  ( -30.49138227950000157, 1379.618898258369882, 214.1838697673789795 ) ) ;
#85751 = FACE_OUTER_BOUND ( 'NONE', #2292, .T. ) ;
#85753 = CARTESIAN_POINT ( 'NONE',  ( 4.601013853250220720, 1466.751833711500012, 199.0309000631700087 ) ) ;
#85752 = CARTESIAN_POINT ( 'NONE',  ( 17.95976239040000166, 1458.835784221629865, 228.1005955696979868 ) ) ;
#85754 = B_SPLINE_CURVE_WITH_KNOTS ( 'NONE', 3,
 ( #103660, #61148, #55478, #38104, #14541, #71760, #90700, #21820, #20732, #38648, #13426, #73370, #64435, #5048, #65532, #3428, #63883, #82312, #89603, #107508, #30798, #5610, #72823, #12896, #97998, #90143, #39763, #47073, #97463, #106956, #29157, #106415, #99639, #81741, #91262, #54927, #47616 ),
 .UNSPECIFIED., .F., .F.,
 ( 4, 3, 3, 3, 3, 3, 3, 3, 3, 3, 3, 3, 4 ),
 ( -13.29188980189490010, -13.07961419483339860, -12.37600827227140066, -11.63118760886860059, -10.84675077014980005, -10.00729710514400139, -9.011581114248389923, -8.034184604791839490, -7.287185506055469553, -6.316933981596370096, -5.489728945046230102, -4.759576170441491172, -4.070471747090000036 ),
 .UNSPECIFIED. ) ;
#85755 = CARTESIAN_POINT ( 'NONE',  ( 15.52481336237690179, 1507.483737832699944, 225.9069234557499897 ) ) ;
#85756 = CARTESIAN_POINT ( 'NONE',  ( -20.86258279118739978, 1504.682079557240058, 214.2158750867690173 ) ) ;
#85757 = EDGE_LOOP ( 'NONE', ( #64867, #92957, #106179, #54628 ) ) ;
#85758 = AXIS2_PLACEMENT_3D ( 'NONE', #56450, #82185, #38528 ) ;
#85759 = CARTESIAN_POINT ( 'NONE',  ( -4.487358994564536907, 1509.034509900238845, 205.3201110865223029 ) ) ;
#85760 = CARTESIAN_POINT ( 'NONE',  ( -20.53760542139741929, 1525.821544997590081, 233.5223198772807791 ) ) ;
#85761 = EDGE_CURVE ( 'NONE', #37407, #38555, #24994, .T. ) ;
#85762 = CARTESIAN_POINT ( 'NONE',  ( -2.925857677911992027, 1485.016887262468117, 183.1345334478515099 ) ) ;
#85763 = CARTESIAN_POINT ( 'NONE',  ( -14.29558945610000009, 1415.677402202029953, 213.3792774005289914 ) ) ;
#85765 = ORIENTED_EDGE ( 'NONE', *, *, #107050, .T. ) ;
#85764 = CARTESIAN_POINT ( 'NONE',  ( -0.4393421190897080497, 1515.147356017569791, 204.7945591776110064 ) ) ;
#85766 = CARTESIAN_POINT ( 'NONE',  ( -9.095046486179999334, 1384.897268781169942, 199.9428014140690095 ) ) ;
#85767 = CARTESIAN_POINT ( 'NONE',  ( 0.000000000000000000, 1397.913060387289988, 209.1218459616989946 ) ) ;
#85768 = ADVANCED_FACE ( 'NONE', ( #38969 ), #66117, .T. ) ;
#85769 = CARTESIAN_POINT ( 'NONE',  ( -11.27131388419999958, 1430.079666422429909, 151.1567905714979929 ) ) ;
#85770 = CARTESIAN_POINT ( 'NONE',  ( -21.12212911287052464, 1511.187213306747708, 182.4210318429776692 ) ) ;
#85771 = CARTESIAN_POINT ( 'NONE',  ( -11.02705047837450181, 1462.270517538050171, 209.4579406216429902 ) ) ;
#85772 = CARTESIAN_POINT ( 'NONE',  ( -3.696522336499820760, 1396.042145791810071, 198.5686952443658697 ) ) ;
#85773 = CARTESIAN_POINT ( 'NONE',  ( 9.258462863084998773, 1517.051704408389924, 196.7308630447670055 ) ) ;
#85774 = CARTESIAN_POINT ( 'NONE',  ( -15.29601662286500030, 1513.169116394660023, 223.2466004030669922 ) ) ;
#85775 = CARTESIAN_POINT ( 'NONE',  ( 13.11746251490000148, 1410.400218127729886, 228.4678513248979925 ) ) ;
#85776 = EDGE_CURVE ( 'NONE', #56530, #110307, #50697, .T. ) ;
#85778 = CARTESIAN_POINT ( 'NONE',  ( -9.845631732519999346, 1478.475703631090028, 212.8873760790889946 ) ) ;
#85777 = CARTESIAN_POINT ( 'NONE',  ( 0.4151546846821903003, 1522.382868172863937, 244.9330574173806951 ) ) ;
#85779 = CARTESIAN_POINT ( 'NONE',  ( -16.96848018825399862, 1460.581442102934261, 228.2620679135440014 ) ) ;
#85780 = VECTOR ( 'NONE', #39559, 1000.000000000000000 ) ;
#85781 = CARTESIAN_POINT ( 'NONE',  ( 1.701729820345000199, 1516.969638403840008, 206.2395199527169893 ) ) ;
#85782 = CARTESIAN_POINT ( 'NONE',  ( 23.45810927580000183, 1411.272422073929874, 269.3038011074980318 ) ) ;
#85783 = DIRECTION ( 'NONE',  ( 0.000000000000000000, 0.000000000000000000, 1.000000000000000000 ) ) ;
#85784 = B_SPLINE_SURFACE_WITH_KNOTS ( 'NONE', 5, 5, ( 
 ( #77916, #19649, #71764, #27505, #61692, #88527 ),
 ( #87989, #11277, #54395, #45440, #79583, #62813 ),
 ( #96929, #60588, #1223, #20196, #11812, #35358 ),
 ( #45982, #3433, #37564, #26393, #17984, #95270 ),
 ( #52180, #86311, #106419, #48735, #39768, #82317 ),
 ( #5615, #64981, #5053, #20737, #21825, #91268 ) ),
 .UNSPECIFIED., .F., .F., .F.,
 ( 6, 6 ),
 ( 6, 6 ),
 ( 29.50720980499999868, 158.0245753780000086 ),
 ( 0.000000000000000000, 1.000000000000000000 ),
 .UNSPECIFIED. ) ;
#85785 = CARTESIAN_POINT ( 'NONE',  ( 21.04775274920000072, 1430.296917575329871, 197.6394114472979879 ) ) ;
#85786 = EDGE_CURVE ( 'NONE', #10258, #1893, #74423, .T. ) ;
#85787 = EDGE_CURVE ( 'NONE', #38170, #56464, #99397, .T. ) ;
#85788 = CARTESIAN_POINT ( 'NONE',  ( -0.1600598377913609871, 1508.974959163609810, 238.8730780788579864 ) ) ;
#85789 = CARTESIAN_POINT ( 'NONE',  ( 32.38845792001180968, 1523.456924617338473, 216.1254071227668589 ) ) ;
#85790 = CARTESIAN_POINT ( 'NONE',  ( -41.66194398591169801, 1443.744947597720056, 136.1277479405200097 ) ) ;
#85791 = CARTESIAN_POINT ( 'NONE',  ( -1.906499846882070084E-08, 1516.801704408389924, 209.1218459511669892 ) ) ;
#85792 = CARTESIAN_POINT ( 'NONE',  ( -16.50171772879999921, 1417.502270639089829, 205.9476994086790000 ) ) ;
#85793 = AXIS2_PLACEMENT_3D ( 'NONE', #102313, #86079, #25600 ) ;
#85794 = CARTESIAN_POINT ( 'NONE',  ( -14.01419671689999902, 1443.250645178179866, 188.5336382816979892 ) ) ;
#85795 = CARTESIAN_POINT ( 'NONE',  ( -4.413317922511070357, 1485.124240097989968, 198.0652374695790172 ) ) ;
#85796 = CARTESIAN_POINT ( 'NONE',  ( -8.629049563562299241, 1437.597470000089970, 208.3922918523649912 ) ) ;
#85797 = CARTESIAN_POINT ( 'NONE',  ( -5.486708004948176232, 1457.204336652478105, 228.5178868769606595 ) ) ;
#85798 = ORIENTED_EDGE ( 'NONE', *, *, #82880, .F. ) ;
#85799 = CARTESIAN_POINT ( 'NONE',  ( -2.841932056525000139, 1512.089957059379913, 201.3490862420470080 ) ) ;
#85800 = CARTESIAN_POINT ( 'NONE',  ( -11.72950371754490106, 1409.322663682899929, 199.8602493023269915 ) ) ;
#85801 = CARTESIAN_POINT ( 'NONE',  ( -113.4235965852909089, 1381.413060387289988, 305.2215675190763591 ) ) ;
#85802 = CARTESIAN_POINT ( 'NONE',  ( -15.05358279999999915, 1410.831827720429828, 226.7261506157979909 ) ) ;
#85803 = CARTESIAN_POINT ( 'NONE',  ( -14.61105931230000010, 1474.212000672530166, 267.1471378767980127 ) ) ;
#85804 = CARTESIAN_POINT ( 'NONE',  ( 30.29107790644764009, 1523.847233649538339, 195.7510835363660533 ) ) ;
#85805 = CARTESIAN_POINT ( 'NONE',  ( -14.31745300034082291, 1514.209337176663212, 192.5996944249964429 ) ) ;
#85806 = EDGE_CURVE ( 'NONE', #40123, #74608, #73022, .T. ) ;
#85807 = CARTESIAN_POINT ( 'NONE',  ( -24.07979781585164503, 1444.275408748464088, 212.4814690993878230 ) ) ;
#85808 = CARTESIAN_POINT ( 'NONE',  ( -81.83957670781239813, 1384.634800382709955, 305.0019059595069848 ) ) ;
#85809 = CARTESIAN_POINT ( 'NONE',  ( -19.40613836968019967, 1384.949689164209985, 201.5054105275870029 ) ) ;
#85810 = CARTESIAN_POINT ( 'NONE',  ( -13.96307519100000150, 1409.400661718330184, 225.8965666933980003 ) ) ;
#85811 = CARTESIAN_POINT ( 'NONE',  ( 11.61894910093169919, 1415.258594622810051, 222.9409272062040088 ) ) ;
#85812 = B_SPLINE_SURFACE_WITH_KNOTS ( 'NONE', 5, 1, ( 
 ( #45897, #87901 ),
 ( #28527, #11727 ),
 ( #19560, #54307 ),
 ( #12818, #21743 ),
 ( #38565, #44796 ),
 ( #55396, #78949 ),
 ( #20115, #96283 ),
 ( #98474, #79493 ),
 ( #71682, #106333 ) ),
 .UNSPECIFIED., .F., .F., .F.,
 ( 6, 3, 6 ),
 ( 2, 2 ),
 ( 0.000000000000000000, 3.905343215419999847, 7.794752761919999884 ),
 ( 0.000000000000000000, 14.00000000000000000 ),
 .UNSPECIFIED. ) ;
#85813 = CARTESIAN_POINT ( 'NONE',  ( -6.184151071931365706, 1496.325375897394451, 199.7106397341868274 ) ) ;
#85814 = CARTESIAN_POINT ( 'NONE',  ( -16.66231036550682987, 1523.604703353109699, 237.7554842931448036 ) ) ;
#85815 = DIRECTION ( 'NONE',  ( 0.03489949670247352587, -0.9993908270190967613, -1.907370177224992791E-14 ) ) ;
#85816 = CARTESIAN_POINT ( 'NONE',  ( -23.38374426929999927, 1411.089939434129974, 205.9489912828279898 ) ) ;
#85817 = CARTESIAN_POINT ( 'NONE',  ( -1.465793917108519917, 1484.360957496709943, 182.4810413606819850 ) ) ;
#85818 = CARTESIAN_POINT ( 'NONE',  ( 16.66700976312913696, 1523.530935881284904, 180.4846138748685007 ) ) ;
#85819 = VECTOR ( 'NONE', #33808, 1000.000000000000227 ) ;
#85820 = CARTESIAN_POINT ( 'NONE',  ( 10.46985159624440165, 1480.586287654560010, 207.8944363599310066 ) ) ;
#85821 = B_SPLINE_SURFACE_WITH_KNOTS ( 'NONE', 5, 5, ( 
 ( #28826, #105539, #36672, #70310, #37227, #96020, #70865, #72489, #78674, #46199, #104977, #27716, #37779, #3650, #28267, #45653, #63024, #106080, #53491, #20946, #12018, #62460, #3097, #71423, #80333, #55152, #63559, #1991, #61355, #96583, #10923, #45099, #89273 ),
 ( #52935, #44528, #12570, #19855, #79239, #46750, #95474, #18741, #80881, #2547, #4177, #87071, #98770, #91482, #5831, #30465, #64097, #73598, #22579, #4712, #90921, #13637, #6916, #106618, #73034, #22032, #39421, #107728, #57895, #55700, #5266, #108828, #47277 ),
 ( #31013, #82536, #15302, #66310, #65193, #41072, #29904, #14761, #98218, #49494, #89821, #99305, #39972, #38855, #56229, #107173, #6373, #92030, #90359, #83618, #40519, #48949, #21488, #83080, #64651, #32125, #56783, #14207, #48393, #13093, #81400, #74147, #47826 ),
 ( #108278, #100427, #31565, #65741, #23156, #81960, #99859, #57358, #74696, #23710, #52260, #32675, #93126, #34878, #50044, #101506, #109399, #66854, #94789, #50588, #84719, #100963, #84172, #16393, #8565, #75788, #69067, #207, #103167, #8018, #42185, #59546, #85268 ),
 ( #76898, #42737, #76335, #7471, #34331, #109940, #110485, #86385, #15839, #94222, #33764, #41633, #85835, #51694, #67961, #93659, #68508, #9135, #33218, #26468, #25907, #102071, #60663, #18066, #24260, #58440, #25353, #92567, #43298, #9673, #58998, #67407, #24793 ),
 ( #16940, #102607, #51142, #60105, #17496, #77447, #75250, #748, #29244, #54479, #28697, #1294, #97013, #78548, #80201, #87509, #28138, #36541, #97552, #103744, #53934, #61232, #27046, #70189, #20275, #37089, #69622, #104298, #88615, #37644, #55021, #95347, #71292 ),
 ( #2972, #1864, #89148, #27587, #19733, #88068, #11896, #77989, #53363, #35998, #20825, #10230, #35435, #45526, #43843, #18608, #52807, #105405, #86939, #62903, #46070, #3519, #44407, #79667, #11356, #10799, #61770, #71850, #95896, #44969, #19157, #79116, #105966 ),
 ( #63434, #2424, #70738, #104850, #62328, #96453, #6233, #57772, #21360, #98088, #90231, #12433, #5136, #38188, #29788, #82942, #56102, #55566, #81832, #46623, #23582, #23021, #81282, #74563, #99175, #4598, #108142, #22456, #47156, #80755, #13515, #39291, #89692 ),
 ( #100298, #12973, #31435, #65616, #48819, #48263, #82406, #4063, #56657, #64523, #38732, #72370, #72908, #90791, #14073, #91353, #106500, #21905, #107047, #63975, #30333, #98638, #5702, #66179, #47703, #73465, #39847, #107598, #74010, #57224, #14633, #30881, #99729 ),
 ( #65061, #40386, #108698, #31989, #16262, #40939, #103032, #84589, #67272, #85689, #24115, #26329, #50465, #42050, #109264, #8987, #91891, #100827, #66724, #58856, #15166, #7880, #6776, #32549, #51554, #24655, #58307, #76201, #49354, #83482, #102484, #49906, #43158 ),
 ( #25773, #75117, #110346, #85139, #84041, #33621, #92428, #67816, #59972, #68932, #15704, #61, #34192, #17358, #16803, #51006, #7339, #25217, #33083, #41504, #34742, #59421, #92987, #101930, #612, #77314, #93533, #75662, #109805, #76750, #101365, #8425, #42596 ),
 ( #68376, #94088, #103604, #71140, #45921, #86802, #80055, #105260, #45382, #17919, #2825, #95208, #96871, #104156, #44828, #53224, #3376, #9536, #70588, #77857, #43704, #10093, #36943, #53793, #86245, #44267, #28554, #54334, #71709, #1166, #87930, #62753, #37503 ),
 ( #20140, #11219, #105827, #26903, #61625, #35861, #88466, #60524, #52116, #78409, #11750, #35296, #1721, #94646, #69481, #61092, #70045, #27443, #18469, #52666, #95757, #104704, #19022, #87364, #96310, #10659, #78981, #2285, #36397, #27999, #62184, #19589, #79520 ),
 ( #48121, #21769, #20677, #64379, #89000, #40255, #55970, #4464, #22876, #72235, #74437, #98501, #90094, #46481, #57086, #29105, #38057, #3928, #106900, #63291, #13377, #54876, #80614, #99593, #72772, #106360, #47565, #97406, #12287, #39711, #97944, #91209, #4995 ),
 ( #29646, #81689, #22320, #21213, #39140, #63833, #73316, #108003, #6100, #55421, #82260, #5560, #65484, #64929, #99042, #89555, #107453, #81151, #12844, #82807, #30748, #30186, #56522, #48683, #14491, #90649, #47025, #38593, #13933, #73875, #31300, #91756, #7215 ),
 ( #109674, #76621, #23983, #23448, #92860, #93962, #57643, #92306, #41921, #41373, #75539, #76077, #100163, #110773, #66597, #8301, #32418, #50876, #15032, #68256, #8850, #110217, #102363, #50343, #24537, #93412, #66040, #17227, #49230, #32950, #33490, #6654, #58178 ),
 ( #83355, #16136, #51423, #40807, #15576, #67692, #67139, #101237, #101800, #74986, #34063, #100701, #42462, #49778, #85006, #109134, #25648, #43032, #25090, #59838, #84468, #58725, #59295, #85553, #83909, #7756, #16678, #108563, #31853, #34617, #95083, #36831, #51985 ),
 ( #10524, #45258, #493, #86673, #69352, #54215, #43583, #68802, #78846, #20019, #102903, #60390, #70464, #86126, #36274, #11091, #79393, #77732, #2157, #44699, #9969, #9420, #87235, #1045, #44140, #88340, #17785, #96186, #78274, #35167, #87805, #53661, #1588 ),
 ( #94511, #71021, #11631, #103462, #26769, #35725, #77190, #69913, #26202, #60956, #105141, #104026, #18349, #27321, #52541, #61503, #2706, #95632, #28431, #53096, #18901, #62061, #104585, #27880, #19462, #62631, #96748, #54758, #30068, #63716, #56951, #45809, #12173 ),
 ( #81569, #4873, #79942, #89982, #97826, #46363, #99469, #13256, #46913, #21654, #65362, #5431, #81035, #91080, #3258, #37944, #22748, #80498, #37385, #47445, #71586, #105707, #28989, #39015, #88888, #73193, #90529, #47991, #3814, #107338, #30633, #55306, #72124 ),
 ( #89440, #63177, #97283, #64821, #12731, #106240, #56397, #22201, #4345, #64259, #98929, #13805, #29526, #39588, #82129, #38475, #72652, #98383, #73760, #107883, #55862, #20554, #21104, #106778, #31173, #23320, #9160, #108443, #18089, #85859, #91637, #60690, #27071 ),
 ( #6532, #75411, #65909, #109551, #94813, #103769, #14913, #34901, #69088, #52284, #51724, #43324, #14363, #60128, #66470, #49105, #69648, #94246, #15461, #102630, #35458, #86409, #49654, #61255, #48555, #773, #82692, #5982, #31724, #23861, #17520, #57512, #40684 ),
 ( #40130, #34355, #1317, #74313, #109001, #77471, #58054, #92189, #103189, #100028, #9698, #83239, #26494, #74857, #43866, #32286, #78010, #100579, #83789, #7084, #68532, #41239, #25930, #29262, #70213, #36562, #44990, #11915, #63455, #52830, #10820, #80224, #36022 ),
 ( #45547, #46092, #95370, #2446, #19179, #70759, #104871, #105987, #44427, #28160, #3541, #104317, #97573, #71871, #10251, #78571, #62349, #1886, #37665, #20845, #79137, #95917, #27611, #79686, #88637, #88088, #18634, #96473, #86960, #19753, #53383, #97034, #61796 ),
 ( #87532, #11375, #53954, #2992, #37112, #71312, #105427, #28716, #62923, #20297, #54501, #101883, #67770, #16, #26856, #77814, #110302, #34150, #61043, #78366, #95715, #33578, #1123, #95167, #61582, #43662, #8383, #18980, #68335, #60477, #17873, #52623, #7838 ),
 ( #42006, #93490, #102442, #52071, #85091, #44222, #9495, #1673, #25728, #51508, #68889, #94595, #84549, #94047, #76155, #50964, #42551, #103553, #77273, #25174, #8940, #59378, #16761, #571, #59930, #35814, #76703, #17313, #43114, #34697, #85640, #69997, #102991 ),
 ( #26288, #86204, #35254, #69438, #104111, #18423, #86761, #10049, #27399, #42947, #17698, #68714, #16057, #9340, #33978, #50260, #77106, #68173, #92781, #15504, #25009, #84921, #67059, #42379, #75988, #69265, #58102, #24459, #59210, #43502, #7134, #67607, #60302 ),
 ( #86042, #83832, #41289, #101716, #75463, #102819, #77646, #41832, #84389, #109597, #102280, #26113, #110686, #960, #93329, #94422, #7676, #32869, #76535, #35084, #101165, #110138, #25561, #16592, #50789, #59754, #49703, #51902, #33411, #103371, #8214, #414, #58648 ),
 ( #93875, #34532, #51332, #17141, #85467, #92233, #8766, #37855, #86591, #54130, #37305, #3725, #96662, #61423, #72041, #87149, #2621, #70940, #105619, #60874, #36198, #18819, #26675, #103944, #95000, #28346, #80411, #18268, #9883, #19933, #35633, #88258, #71500 ),
 ( #70382, #52461, #27242, #95546, #45727, #19370, #44051, #61979, #78190, #1502, #53573, #2067, #20468, #69827, #53014, #96094, #87720, #10438, #62541, #79863, #11550, #104499, #10998, #45170, #105056, #54679, #36747, #44610, #3173, #78752, #27792, #79311, #28903 ),
 ( #88805, #63098, #97195, #12088, #46283, #29984, #63634, #73111, #22112, #4257, #90443, #13168, #6454, #106158, #72566, #98297, #38931, #39506, #47357, #106693, #49026, #73679, #107252, #82041, #14837, #65824, #30546, #40602, #29435, #90995, #97748, #83161, #89353 ),
 ( #38390, #21573, #64176, #5904, #91561, #55782, #21019, #40050, #14285, #55223, #48475, #89897, #31643, #64735, #13720, #98849, #12648, #46826, #5346, #80956, #81484, #4785, #82613, #99387, #56310, #47905, #74231, #99942, #107806, #31093, #22665, #108362, #65275 ),
 ( #23237, #56865, #57436, #108913, #66386, #94298, #50126, #84255, #32205, #83703, #92650, #8092, #75331, #34409, #110562, #102686, #15925, #41705, #59081, #84794, #74772, #7551, #100505, #41156, #109472, #93735, #67484, #23784, #110015, #57973, #85914, #101587, #75865 ) ),
 .UNSPECIFIED., .F., .F., .F.,
 ( 6, 3, 3, 3, 3, 3, 3, 3, 3, 3, 6 ),
 ( 6, 3, 3, 3, 3, 3, 3, 3, 3, 3, 6 ),
 ( 0.000000000000000000, 1.936717162300000128, 3.873434324599999812, 4.841792905749999321, 5.810151486899999718, 7.746868649199999624, 9.683585811500000418, 10.65194439270000082, 11.62030297379999944, 13.55702013610000023, 15.49373729840000102 ),
 ( 0.000000000000000000, 1.936717162300000128, 3.873434324599999812, 4.841792905749999321, 5.810151486899999718, 7.746868649199999624, 9.683585811500000418, 10.65194439270000082, 11.62030297379999944, 13.55702013610000023, 15.49373729840000102 ),
 .UNSPECIFIED. ) ;
#85822 = CARTESIAN_POINT ( 'NONE',  ( 2.461716435160000049, 1435.943783413959864, 150.4083956814980070 ) ) ;
#85823 = CARTESIAN_POINT ( 'NONE',  ( -19.86654541609999924, 1443.778853391489974, 213.2156533979290032 ) ) ;
#85824 = CARTESIAN_POINT ( 'NONE',  ( -4.038582018736554424, 1515.598601288560985, 209.4326227434377472 ) ) ;
#85825 = CARTESIAN_POINT ( 'NONE',  ( -4.705736654693100540, 1479.984769896650278, 230.9466533013020069 ) ) ;
#85826 =( BOUNDED_CURVE ( )  B_SPLINE_CURVE ( 3, ( #11412, #1921, #55078, #61832 ),
 .UNSPECIFIED., .F., .T. ) 
 B_SPLINE_CURVE_WITH_KNOTS ( ( 4, 4 ),
 ( 5.447131836145489459, 6.315249268837946239 ),
 .UNSPECIFIED. ) 
 CURVE ( )  GEOMETRIC_REPRESENTATION_ITEM ( )  RATIONAL_B_SPLINE_CURVE ( ( 1.000000000000000000, 0.9381775381419560356, 0.9381775381419560356, 1.000000000000000000 ) ) 
 REPRESENTATION_ITEM ( '' )  );
#85828 = CARTESIAN_POINT ( 'NONE',  ( -10.06333680959999910, 1381.959595553830241, 201.2992880703589833 ) ) ;
#85827 = CARTESIAN_POINT ( 'NONE',  ( -22.63947967940000083, 1410.626538670930131, 211.5335619545579959 ) ) ;
#85829 = DIRECTION ( 'NONE',  ( 1.836970198721029688E-16, 1.000000000000000000, 0.000000000000000000 ) ) ;
#85830 = DIRECTION ( 'NONE',  ( 1.000000000000000000, 0.000000000000000000, 0.000000000000000000 ) ) ;
#85831 = VECTOR ( 'NONE', #97300, 1000.000000000000114 ) ;
#85832 = CARTESIAN_POINT ( 'NONE',  ( -11.12609309039999950, 1491.160357135190225, 209.7795743302380060 ) ) ;
#85833 = CARTESIAN_POINT ( 'NONE',  ( 9.406850844429460068, 1450.347115270439872, 204.6358555677470008 ) ) ;
#85834 = CARTESIAN_POINT ( 'NONE',  ( -0.5941431873634029914, 1420.625254382509866, 182.8568024079209806 ) ) ;
#85835 = CARTESIAN_POINT ( 'NONE',  ( 2.288357407604999949, 1517.116049120239950, 203.3334095979369920 ) ) ;
#85836 = CARTESIAN_POINT ( 'NONE',  ( -8.704519340914814052, 1398.171442848455627, 218.7793260591613489 ) ) ;
#85837 = CARTESIAN_POINT ( 'NONE',  ( -4.283857371189049523, 1440.956241081810049, 155.9231041381889895 ) ) ;
#85838 = CARTESIAN_POINT ( 'NONE',  ( 4.208240993269999564, 1434.939300248989866, 227.0651965576989824 ) ) ;
#85839 = FACE_OUTER_BOUND ( 'NONE', #20053, .T. ) ;
#85840 = AXIS2_PLACEMENT_3D ( 'NONE', #107979, #31276, #90069 ) ;
#85841 = SURFACE_STYLE_USAGE ( .BOTH. , #51700 ) ;
#85842 = CARTESIAN_POINT ( 'NONE',  ( 40.44627699776750518, 1447.230319210510061, 136.4061566910979764 ) ) ;
#85844 = VERTEX_POINT ( 'NONE', #5252 ) ;
#85843 = CARTESIAN_POINT ( 'NONE',  ( -66.98815419365290325, 1379.745645132190020, 277.9424776583130097 ) ) ;
#85845 = ORIENTED_EDGE ( 'NONE', *, *, #9926, .F. ) ;
#85846 = CARTESIAN_POINT ( 'NONE',  ( 11.83189171497950021, 1433.731675027539950, 150.7538201803880042 ) ) ;
#85847 = CARTESIAN_POINT ( 'NONE',  ( 28.41776274690000292, 1509.905438290129950, 216.6186804979880094 ) ) ;
#85848 = ORIENTED_EDGE ( 'NONE', *, *, #27154, .F. ) ;
#85849 = CARTESIAN_POINT ( 'NONE',  ( -107.8262839200000087, 1378.913060387289988, 308.7442743352589787 ) ) ;
#85850 = CARTESIAN_POINT ( 'NONE',  ( -10.36562125464200079, 1447.972358732529983, 209.1898071262730241 ) ) ;
#85851 = CARTESIAN_POINT ( 'NONE',  ( 3.586360116007059506, 1515.071395204220153, 205.0390662864990077 ) ) ;
#85853 = CARTESIAN_POINT ( 'NONE',  ( 0.8262468554639167406, 1416.839570625587157, 190.2114392743267501 ) ) ;
#85852 = DIRECTION ( 'NONE',  ( 0.000000000000000000, 0.000000000000000000, -1.000000000000000000 ) ) ;
#85854 = CARTESIAN_POINT ( 'NONE',  ( 2.893254755770000131, 1507.808732218230034, 235.9747248503979904 ) ) ;
#85855 = CARTESIAN_POINT ( 'NONE',  ( 3.328465976629999989, 1507.639111981630094, 181.4822836926979903 ) ) ;
#85856 = CARTESIAN_POINT ( 'NONE',  ( -2.857575698580000267, 1416.519106787730152, 191.2889195365980015 ) ) ;
#85857 = CARTESIAN_POINT ( 'NONE',  ( -24.09999474531229779, 1444.794386359630153, 211.7658029478569972 ) ) ;
#85858 = SURFACE_STYLE_USAGE ( .BOTH. , #68531 ) ;
#85859 = CARTESIAN_POINT ( 'NONE',  ( -6.546039433425000276, 1516.565291103010168, 211.4147861392469849 ) ) ;
#85860 = CARTESIAN_POINT ( 'NONE',  ( 35.52558520626859462, 1435.900183204529867, 134.0999999974749812 ) ) ;
#85861 = CARTESIAN_POINT ( 'NONE',  ( 11.30119660309999929, 1432.297823534569943, 151.5221481425980130 ) ) ;
#85862 = CARTESIAN_POINT ( 'NONE',  ( 6.563811411605000146, 1514.071098020780028, 201.4679970645470064 ) ) ;
#85863 = ORIENTED_EDGE ( 'NONE', *, *, #93216, .F. ) ;
#85864 = CARTESIAN_POINT ( 'NONE',  ( 13.67949770404189991, 1434.971884691610285, 148.6456809700089821 ) ) ;
#85865 = ORIENTED_EDGE ( 'NONE', *, *, #103228, .T. ) ;
#85866 = VERTEX_POINT ( 'NONE', #107715 ) ;
#85867 = CARTESIAN_POINT ( 'NONE',  ( 12.96754954602891452, 1444.896177199393605, 169.4263590215614386 ) ) ;
#85868 = CARTESIAN_POINT ( 'NONE',  ( -1.124593200380000102, 1465.369077680330065, 236.1474170825979968 ) ) ;
#85869 = AXIS2_PLACEMENT_3D ( 'NONE', #33199, #25889, #186 ) ;
#85870 = CARTESIAN_POINT ( 'NONE',  ( -12.20493911282916422, 1503.566106373808225, 208.5052164380747115 ) ) ;
#85871 = CARTESIAN_POINT ( 'NONE',  ( -2.484577695354999616, 1517.170512887980067, 216.4602579296269766 ) ) ;
#85872 = CARTESIAN_POINT ( 'NONE',  ( -7.932506210237777466, 1511.860476874699089, 212.2635995054286582 ) ) ;
#85873 = CARTESIAN_POINT ( 'NONE',  ( -19.07346239651989350, 1442.276001358560052, 210.5561030354247976 ) ) ;
#85874 = CARTESIAN_POINT ( 'NONE',  ( -59.11633403356870531, 1379.721728728080507, 259.3841856975482187 ) ) ;
#85875 = CARTESIAN_POINT ( 'NONE',  ( -3.771520285720000309, 1375.389610323599982, 209.1218458698340044 ) ) ;
#85876 = B_SPLINE_CURVE_WITH_KNOTS ( 'NONE', 3,
 ( #15811, #92543, #5245, #39400, #31542, #73578, #32653, #50015, #48370, #99283, #30993, #74674, #100937, #100405, #84147, #49470, #58417, #39951, #7448, #48929, #41611 ),
 .UNSPECIFIED., .F., .F.,
 ( 4, 2, 2, 2, 1, 1, 1, 1, 1, 2, 2, 2, 4 ),
 ( 0.000000000000000000, 0.2499999999998419042, 0.3749999999997623013, 0.4374999999997226108, 0.4687499999997017941, 0.4843749999996903588, 0.4921874999996844746, 0.4960937499996817546, 0.4980468749996803668, 0.4990234374996797007, 0.4999999999996790345, 0.7499999999998394618, 1.000000000000000000 ),
 .UNSPECIFIED. ) ;
#85877 = EDGE_LOOP ( 'NONE', ( #1750, #84867, #106738, #79333 ) ) ;
#85878 = CARTESIAN_POINT ( 'NONE',  ( 2.477373605864999995, 1516.891731298979948, 206.2406231745169976 ) ) ;
#85879 = EDGE_LOOP ( 'NONE', ( #99557, #106433, #97260, #107318, #71696 ) ) ;
#85880 = CARTESIAN_POINT ( 'NONE',  ( -105.3976796612010105, 1378.878460358250095, 305.0048818320939858 ) ) ;
#85881 = EDGE_CURVE ( 'NONE', #96030, #27055, #45085, .T. ) ;
#85882 = DIRECTION ( 'NONE',  ( -1.000000000000000000, 0.000000000000000000, 0.000000000000000000 ) ) ;
#85883 = ORIENTED_EDGE ( 'NONE', *, *, #97392, .F. ) ;
#85884 = CARTESIAN_POINT ( 'NONE',  ( -10.88545445589999972, 1409.460139157529966, 189.3640148419979994 ) ) ;
#85885 = CARTESIAN_POINT ( 'NONE',  ( 7.170545778634999756, 1512.974587999920004, 216.1941441599169877 ) ) ;
#85887 = VERTEX_POINT ( 'NONE', #108259 ) ;
#85886 = CARTESIAN_POINT ( 'NONE',  ( -11.60004869885203682, 1428.983126981193436, 137.0999999980979851 ) ) ;
#85888 = B_SPLINE_CURVE_WITH_KNOTS ( 'NONE', 3,
 ( #39311, #100315, #107618, #65079, #90809, #26921, #103623, #60545, #53242, #26347, #1739, #95773, #17938, #94106, #95225, #34761, #85157, #76221, #9552, #61643, #35314, #68394, #25790, #85709, #103049, #101948, #94666, #19039, #42070, #8443, #42616, #61110, #59989, #18487, #82, #67837, #25235, #52134, #52684, #43721, #102500, #27458, #7898, #93549, #9004, #43178 ),
 .UNSPECIFIED., .F., .F.,
 ( 4, 3, 3, 3, 3, 3, 3, 3, 3, 3, 3, 3, 3, 3, 3, 4 ),
 ( -2.000000000000000000, -1.899921065871490011, -1.768492324960689865, -1.635042478424219903, -1.500382481119959976, -1.363810208304299998, -1.226238695583030003, -1.087938997751350056, -0.9492313653944000063, -0.8106048422210849758, -0.6725266165283070308, -0.5353410715184310220, -0.3993255339347789867, -0.2646837051581960587, -0.1315499660857459840, 0.000000000000000000 ),
 .UNSPECIFIED. ) ;
#85889 = CARTESIAN_POINT ( 'NONE',  ( 22.58319838150000081, 1431.951323673850084, 217.9369709904979970 ) ) ;
#85890 = CARTESIAN_POINT ( 'NONE',  ( -13.82318464736509966, 1508.551704408389924, 210.3452327715689876 ) ) ;
#85891 = CYLINDRICAL_SURFACE ( 'NONE', #27028, 2.000000000000001332 ) ;
#85892 = DIRECTION ( 'NONE',  ( -0.000000000000000000, -1.000000000000000000, -0.000000000000000000 ) ) ;
#85893 = DIRECTION ( 'NONE',  ( 1.000000000000000000, 2.249639673992789970E-32, 1.224646799147350002E-16 ) ) ;
#85894 = CARTESIAN_POINT ( 'NONE',  ( -5.000083865865000199, 1516.858456333729919, 214.1306941701269864 ) ) ;
#85895 = CARTESIAN_POINT ( 'NONE',  ( -2.569297563752009683, 1429.158925392049923, 200.1088665598680052 ) ) ;
#85896 = CARTESIAN_POINT ( 'NONE',  ( -20.59664500279999899, 1507.763472350329948, 190.3621299396980078 ) ) ;
#85897 = CARTESIAN_POINT ( 'NONE',  ( -7.720817095325030799, 1516.984411380829897, 208.9454551635660380 ) ) ;
#85898 = CARTESIAN_POINT ( 'NONE',  ( -2.282915221395000138, 1516.876240617270014, 211.6158662526670184 ) ) ;
#85899 = CARTESIAN_POINT ( 'NONE',  ( 14.79761690939999852, 1410.816705308729979, 191.5180088111980012 ) ) ;
#85900 = CARTESIAN_POINT ( 'NONE',  ( -16.14808375428494003, 1486.096392924785732, 187.0799805905815845 ) ) ;
#85902 = ORIENTED_EDGE ( 'NONE', *, *, #32569, .T. ) ;
#85901 = CARTESIAN_POINT ( 'NONE',  ( -94.50571792069999333, 1385.206310935810052, 294.8715553429590273 ) ) ;
#85903 = CARTESIAN_POINT ( 'NONE',  ( -58.94950924095840605, 1385.071407265270182, 279.1407438311780425 ) ) ;
#85904 = CIRCLE ( 'NONE', #109173, 2.000000000000006661 ) ;
#85905 = CARTESIAN_POINT ( 'NONE',  ( 40.44441459949999285, 1454.056682589430011, 264.0386555474980241 ) ) ;
#85906 = EDGE_CURVE ( 'NONE', #56028, #73491, #57195, .T. ) ;
#85907 = CARTESIAN_POINT ( 'NONE',  ( 3.406945355383976359, 1451.023871256067878, 184.0267942193613919 ) ) ;
#85908 = FACE_OUTER_BOUND ( 'NONE', #49422, .T. ) ;
#85909 = CARTESIAN_POINT ( 'NONE',  ( -7.877053409569999332, 1508.178149367029846, 235.5567789369980005 ) ) ;
#85910 = EDGE_CURVE ( 'NONE', #62647, #41404, #8941, .T. ) ;
#85911 = VECTOR ( 'NONE', #100291, 1000.000000000000000 ) ;
#85912 = CARTESIAN_POINT ( 'NONE',  ( -23.83018590009999826, 1446.211104711980170, 214.0005792661480086 ) ) ;
#85913 = EDGE_CURVE ( 'NONE', #53799, #56488, #37504, .T. ) ;
#85915 = CARTESIAN_POINT ( 'NONE',  ( 19.02906815400000440, 1456.981079902029933, 225.9142998226980126 ) ) ;
#85914 = CARTESIAN_POINT ( 'NONE',  ( -6.942354311545000378, 1516.905946377369901, 216.8406094761369900 ) ) ;
#85916 = CARTESIAN_POINT ( 'NONE',  ( -10.36432893639859998, 1448.249851073609989, 208.5380077942650132 ) ) ;
#85917 = CARTESIAN_POINT ( 'NONE',  ( -107.5108399970000050, 1380.713577291549882, 309.5364694182589460 ) ) ;
#85918 = EDGE_LOOP ( 'NONE', ( #88727, #36257, #110534, #76906 ) ) ;
#85919 = CARTESIAN_POINT ( 'NONE',  ( -6.559168674874999105, 1516.960844870249957, 204.1192525727769862 ) ) ;
#85920 = CARTESIAN_POINT ( 'NONE',  ( -12.99645283652920114, 1508.444770402639961, 217.1333260180389857 ) ) ;
#85921 = AXIS2_PLACEMENT_3D ( 'NONE', #45127, #35590, #63053 ) ;
#85922 = CARTESIAN_POINT ( 'NONE',  ( 1.393816646507353596, 1512.187213306747481, 175.1051575864439656 ) ) ;
#85923 = EDGE_CURVE ( 'NONE', #53131, #51303, #10342, .T. ) ;
#85924 = CARTESIAN_POINT ( 'NONE',  ( 12.36417386409999963, 1419.802638387629941, 223.6718635272980009 ) ) ;
#85925 = CARTESIAN_POINT ( 'NONE',  ( -8.099005836065213515, 1461.719615227744953, 203.7568343392296129 ) ) ;
#85926 = LINE ( 'NONE', #9229, #41453 ) ;
#85927 = CARTESIAN_POINT ( 'NONE',  ( 2.016490277786251450, 1468.747382109811042, 218.9369546187164417 ) ) ;
#85928 = B_SPLINE_CURVE_WITH_KNOTS ( 'NONE', 5,
 ( #100755, #93462, #57703, #77249, #15096, #68311 ),
 .UNSPECIFIED., .F., .F.,
 ( 6, 6 ),
 ( -167.5214209060000030, -95.54118702129999008 ),
 .UNSPECIFIED. ) ;
#85929 = CARTESIAN_POINT ( 'NONE',  ( 32.64372691405990423, 1435.637504776599826, 135.1055159787700006 ) ) ;
#85930 = CARTESIAN_POINT ( 'NONE',  ( -27.58798392020000279, 1447.300859615939999, 137.0122922810979844 ) ) ;
#85931 = CARTESIAN_POINT ( 'NONE',  ( -40.44671179960830187, 1456.761851024655243, 269.1171488671376437 ) ) ;
#85932 = CARTESIAN_POINT ( 'NONE',  ( -109.6086437639999929, 1385.304251137460142, 297.1179079228590467 ) ) ;
#85933 = CARTESIAN_POINT ( 'NONE',  ( 10.77478558037159928, 1480.716566089449998, 211.2105078800119884 ) ) ;
#85934 = CARTESIAN_POINT ( 'NONE',  ( 4.836622313100200188, 1506.975876971950129, 219.7632233975940323 ) ) ;
#85935 = DIRECTION ( 'NONE',  ( 1.000000000000000000, 2.249639673992789970E-32, 1.224646799147350002E-16 ) ) ;
#85936 = VERTEX_POINT ( 'NONE', #67941 ) ;
#85937 = CARTESIAN_POINT ( 'NONE',  ( 2.409586283469999923, 1426.663880916129983, 144.1938086916980239 ) ) ;
#85938 = CARTESIAN_POINT ( 'NONE',  ( 2.982880056400492030, 1425.995092949923674, 184.8396490932583163 ) ) ;
#85939 = CARTESIAN_POINT ( 'NONE',  ( -4.364199128832369823, 1509.032029411810072, 213.2377089278639914 ) ) ;
#85940 = CARTESIAN_POINT ( 'NONE',  ( 14.54091120785239788, 1432.075290591040130, 190.4591005668110029 ) ) ;
#85941 = AXIS2_PLACEMENT_3D ( 'NONE', #62683, #69972, #3316 ) ;
#85942 = CARTESIAN_POINT ( 'NONE',  ( 11.43996310808473638, 1425.781067050057572, 139.0083090113801063 ) ) ;
#85943 = B_SPLINE_CURVE_WITH_KNOTS ( 'NONE', 5,
 ( #37741, #12538, #65157, #80847, #99271, #72461 ),
 .UNSPECIFIED., .F., .F.,
 ( 6, 6 ),
 ( -41.05058650750000027, -28.72930409989999845 ),
 .UNSPECIFIED. ) ;
#85945 = CARTESIAN_POINT ( 'NONE',  ( 33.93019615849225801, 1522.906561336852519, 197.6607374646082178 ) ) ;
#85944 = CARTESIAN_POINT ( 'NONE',  ( 11.54017902740000068, 1501.914511391590167, 210.4796054250789723 ) ) ;
#85946 = CARTESIAN_POINT ( 'NONE',  ( -13.00518750807362167, 1444.872235629844454, 186.2927087732988412 ) ) ;
#85947 = EDGE_CURVE ( 'NONE', #7508, #98070, #26794, .T. ) ;
#85948 = CARTESIAN_POINT ( 'NONE',  ( 20.79738390328738973, 1511.187213306747708, 237.0406858230487899 ) ) ;
#85949 = CARTESIAN_POINT ( 'NONE',  ( -14.00956919615309992, 1384.879701807039964, 219.2459905235510007 ) ) ;
#85950 = CARTESIAN_POINT ( 'NONE',  ( -14.16989796120989986, 1420.440730658529901, 227.4201728071160176 ) ) ;
#85951 = CARTESIAN_POINT ( 'NONE',  ( -24.22787522506175506, 1450.838946662983972, 139.9861787190485529 ) ) ;
#85952 = CARTESIAN_POINT ( 'NONE',  ( -7.844819027749999840, 1484.029266062490024, 200.6142659637689860 ) ) ;
#85953 = CARTESIAN_POINT ( 'NONE',  ( 25.42198949309999989, 1436.467254550020016, 137.2714020107979991 ) ) ;
#85955 = ADVANCED_FACE ( 'NONE', ( #41617 ), #24775, .T. ) ;
#85954 = CARTESIAN_POINT ( 'NONE',  ( -9.150759623799741505, 1396.232611956530036, 202.9140964477350053 ) ) ;
#85956 = VERTEX_POINT ( 'NONE', #102048 ) ;
#85957 = CARTESIAN_POINT ( 'NONE',  ( -16.27483966040009733, 1409.481380779909841, 225.0625982544499948 ) ) ;
#85958 = CARTESIAN_POINT ( 'NONE',  ( 19.63722818192610120, 1519.551704408389924, 218.2362632616380154 ) ) ;
#85959 = EDGE_LOOP ( 'NONE', ( #11798, #4473, #44288, #22305 ) ) ;
#85960 = ORIENTED_EDGE ( 'NONE', *, *, #72139, .F. ) ;
#85961 = CARTESIAN_POINT ( 'NONE',  ( -0.2280590849522179941, 1435.891982273890108, 227.5921632324569828 ) ) ;
#85962 = CARTESIAN_POINT ( 'NONE',  ( -14.93183294469202949, 1416.109101684369762, 205.2149106319410237 ) ) ;
#85964 = CARTESIAN_POINT ( 'NONE',  ( -9.788466504199840656, 1438.420938493939957, 210.7573931614269895 ) ) ;
#85963 = CARTESIAN_POINT ( 'NONE',  ( 10.73151125300000075, 1425.688082741829930, 96.53145859069789481 ) ) ;
#85965 = CARTESIAN_POINT ( 'NONE',  ( -11.16575615629999874, 1433.014654777279929, 151.6208054879980125 ) ) ;
#85966 = CARTESIAN_POINT ( 'NONE',  ( -2.829822254990304042, 1419.790776434859481, 186.1587357482032985 ) ) ;
#85967 = CARTESIAN_POINT ( 'NONE',  ( -2.745154014197499937, 1419.769956470485113, 137.0999999980979851 ) ) ;
#85968 = CARTESIAN_POINT ( 'NONE',  ( -19.86464710129999744, 1441.435714617490021, 212.6459466283089910 ) ) ;
#85969 = CARTESIAN_POINT ( 'NONE',  ( 7.812988826530000708, 1507.598641535930028, 182.8715579098980015 ) ) ;
#85970 = CARTESIAN_POINT ( 'NONE',  ( 3.237924447490000190, 1448.965650011070238, 183.9353614378979955 ) ) ;
#85971 = CARTESIAN_POINT ( 'NONE',  ( 7.985371214169377119, 1364.849800335405234, 209.6218459617148824 ) ) ;
#85973 = ORIENTED_EDGE ( 'NONE', *, *, #71079, .F. ) ;
#85972 = CARTESIAN_POINT ( 'NONE',  ( 5.920481487290000011, 1454.372615866290062, 216.6343245259689922 ) ) ;
#85974 = ORIENTED_EDGE ( 'NONE', *, *, #68866, .F. ) ;
#85975 = CARTESIAN_POINT ( 'NONE',  ( -41.66043499930000138, 1443.874479658190012, 136.1362231440980111 ) ) ;
#85976 = CARTESIAN_POINT ( 'NONE',  ( 7.545803617137186947, 1510.531931299321286, 203.4140010686424773 ) ) ;
#85977 = CARTESIAN_POINT ( 'NONE',  ( -1.408322393329999977, 1471.421866497730207, 269.3348812650980335 ) ) ;
#85978 = CARTESIAN_POINT ( 'NONE',  ( -11.60004869885203682, 1428.983126981193436, 137.0999999980979851 ) ) ;
#85979 = DIRECTION ( 'NONE',  ( 0.9455185755993178454, 0.000000000000000000, -0.3255681544571537578 ) ) ;
#85980 = AXIS2_PLACEMENT_3D ( 'NONE', #106359, #82805, #22875 ) ;
#85981 = CARTESIAN_POINT ( 'NONE',  ( -32.48455292688703366, 1524.659148609483054, 201.1731995520806038 ) ) ;
#85982 = CARTESIAN_POINT ( 'NONE',  ( 1.810149460082830064, 1476.164246713959983, 197.7790825785519928 ) ) ;
#85983 = CARTESIAN_POINT ( 'NONE',  ( 22.15124694530000227, 1409.851347014229987, 206.9300461489279996 ) ) ;
#85984 = CARTESIAN_POINT ( 'NONE',  ( -20.59684415639999955, 1507.762623716630060, 190.3921826403979765 ) ) ;
#85985 = CARTESIAN_POINT ( 'NONE',  ( -15.96958168569999970, 1519.913060387329779, 193.1522642759980215 ) ) ;
#85986 = CARTESIAN_POINT ( 'NONE',  ( 10.25488443387654591, 1368.282720929027164, 208.3718459617010978 ) ) ;
#85987 = CARTESIAN_POINT ( 'NONE',  ( 6.251338861372889966, 1407.163727730510118, 197.0599927605450148 ) ) ;
#85988 = CARTESIAN_POINT ( 'NONE',  ( -15.50363298934050071, 1407.833641513950170, 267.1365089329019611 ) ) ;
#85989 = CARTESIAN_POINT ( 'NONE',  ( -14.45330220633330143, 1435.576072362619925, 149.6094451218459938 ) ) ;
#85990 = VERTEX_POINT ( 'NONE', #6897 ) ;
#85991 = CARTESIAN_POINT ( 'NONE',  ( -11.86629849080000021, 1432.349867597430148, 149.9824147457980246 ) ) ;
#85992 = CARTESIAN_POINT ( 'NONE',  ( 13.48364811319999923, 1443.577837597139933, 188.2168391137979881 ) ) ;
#85993 = VERTEX_POINT ( 'NONE', #9113 ) ;
#85994 = VERTEX_POINT ( 'NONE', #7454 ) ;
#85995 = DIRECTION ( 'NONE',  ( -0.02616798426453448984, 0.9993150019883495494, -0.02616798426619649023 ) ) ;
#85996 = CARTESIAN_POINT ( 'NONE',  ( -7.592149787980000397, 1361.964468435470053, 207.6218459616989946 ) ) ;
#85997 = CARTESIAN_POINT ( 'NONE',  ( 5.009478067315000338, 1516.886345593249871, 213.7343532441369973 ) ) ;
#85998 = CARTESIAN_POINT ( 'NONE',  ( -17.86906774540000242, 1470.472114943930137, 189.5573397613979978 ) ) ;
#85999 = CIRCLE ( 'NONE', #53823, 22.86690257359991207 ) ;
#86000 = ORIENTED_EDGE ( 'NONE', *, *, #59785, .T. ) ;
#86001 = CARTESIAN_POINT ( 'NONE',  ( -105.7397521540000014, 1379.153471392710117, 302.6503159780590408 ) ) ;
#86002 = CLOSED_SHELL ( 'NONE', ( #48619, #80105, #17848, #73671, #19683, #13688, #11151, #35039, #8423, #65922, #100749, #48302, #6414, #807, #33664, #59168, #12083, #92443, #73292, #86052, #57726, #71274, #15693, #64961 ) ) ;
#86003 = CARTESIAN_POINT ( 'NONE',  ( 11.74107766989999924, 1415.088275290230058, 222.6191883478979889 ) ) ;
#86004 = CARTESIAN_POINT ( 'NONE',  ( 7.712490952985000980, 1516.666407245520077, 204.5049844236870058 ) ) ;
#86005 = CARTESIAN_POINT ( 'NONE',  ( -26.80691778309999762, 1509.168223069730175, 201.9730100476380130 ) ) ;
#86006 = CARTESIAN_POINT ( 'NONE',  ( 0.8350686643532192477, 1526.382868172863937, 240.9330574173806951 ) ) ;
#86007 = CARTESIAN_POINT ( 'NONE',  ( -25.90756897309999829, 1384.546519395709765, 203.4684288897289832 ) ) ;
#86008 = CARTESIAN_POINT ( 'NONE',  ( -64.27641931829590760, 1384.700183869020066, 253.4426907645700453 ) ) ;
#86009 = CARTESIAN_POINT ( 'NONE',  ( -7.121584090669999867, 1409.161751583729938, 195.9581075241979988 ) ) ;
#86010 = AXIS2_PLACEMENT_3D ( 'NONE', #23794, #92119, #94308 ) ;
#86011 = CARTESIAN_POINT ( 'NONE',  ( -6.445219260712940823, 1513.425324099833460, 216.7494849698516362 ) ) ;
#86013 = VERTEX_POINT ( 'NONE', #58972 ) ;
#86012 = CARTESIAN_POINT ( 'NONE',  ( -5.782709728270000404, 1448.056422632139856, 185.4008468919979862 ) ) ;
#86014 = CARTESIAN_POINT ( 'NONE',  ( -28.30909971437809958, 1508.149945971400030, 209.2281912400019905 ) ) ;
#86015 = CARTESIAN_POINT ( 'NONE',  ( 26.60955424469999997, 1469.249567702030163, 209.2992017010270160 ) ) ;
#86016 = CARTESIAN_POINT ( 'NONE',  ( 20.01352635799040058, 1487.439253770349978, 226.1235325421299933 ) ) ;
#86017 = CARTESIAN_POINT ( 'NONE',  ( -25.50964525599999888, 1435.388358958310164, 135.5743256029979875 ) ) ;
#86018 = AXIS2_PLACEMENT_3D ( 'NONE', #110314, #26869, #94610 ) ;
#86019 = CARTESIAN_POINT ( 'NONE',  ( -5.771797464315000070, 1516.647618671360078, 211.9976960644470125 ) ) ;
#86020 = CARTESIAN_POINT ( 'NONE',  ( -68.45122535890000393, 1379.747412755049936, 279.4374878893589766 ) ) ;
#86021 = CARTESIAN_POINT ( 'NONE',  ( -14.77492012620000139, 1418.010700285029998, 226.9887921092979752 ) ) ;
#86022 = CARTESIAN_POINT ( 'NONE',  ( -30.01482722727578434, 1525.231909165033585, 221.6074739429450915 ) ) ;
#86023 = CARTESIAN_POINT ( 'NONE',  ( -4.042388539304999640, 1517.045004075700035, 208.3857484934819979 ) ) ;
#86024 = VERTEX_POINT ( 'NONE', #60088 ) ;
#86025 = FACE_OUTER_BOUND ( 'NONE', #33928, .T. ) ;
#86026 = CARTESIAN_POINT ( 'NONE',  ( -1.731016753280000042, 1412.842784831929976, 232.9829570279979976 ) ) ;
#86027 =( BOUNDED_CURVE ( )  B_SPLINE_CURVE ( 3, ( #78420, #52675, #3386, #70054 ),
 .UNSPECIFIED., .F., .T. ) 
 B_SPLINE_CURVE_WITH_KNOTS ( ( 4, 4 ),
 ( 1.997881027491174929E-12, 0.4510268114855899291 ),
 .UNSPECIFIED. ) 
 CURVE ( )  GEOMETRIC_REPRESENTATION_ITEM ( )  RATIONAL_B_SPLINE_CURVE ( ( 1.000000000000000000, 0.9831196230105693212, 0.9831196230105693212, 1.000000000000000000 ) ) 
 REPRESENTATION_ITEM ( '' )  );
#86028 = CARTESIAN_POINT ( 'NONE',  ( -49.58513492879999518, 1384.996931083360096, 260.9114759950589928 ) ) ;
#86029 = VERTEX_POINT ( 'NONE', #25890 ) ;
#86031 = CIRCLE ( 'NONE', #55617, 3.000000000000002665 ) ;
#86030 = CARTESIAN_POINT ( 'NONE',  ( -16.54629027219139914, 1385.289268194029773, 219.7699943765580031 ) ) ;
#86033 = VERTEX_POINT ( 'NONE', #84700 ) ;
#86032 = CARTESIAN_POINT ( 'NONE',  ( -10.30791481292679990, 1492.690696011769887, 202.4224590082119732 ) ) ;
#86034 = CARTESIAN_POINT ( 'NONE',  ( 12.28522815033359983, 1434.206584240389930, 149.6310126879850202 ) ) ;
#86035 = EDGE_CURVE ( 'NONE', #81793, #21520, #50022, .T. ) ;
#86036 = CARTESIAN_POINT ( 'NONE',  ( -4.072211398493276846, 1441.024307978096203, 184.8826053890980177 ) ) ;
#86037 = B_SPLINE_CURVE_WITH_KNOTS ( 'NONE', 3,
 ( #100015, #31159, #74299, #89970 ),
 .UNSPECIFIED., .F., .F.,
 ( 4, 4 ),
 ( 0.08090687173989799530, 0.08222331860531204017 ),
 .UNSPECIFIED. ) ;
#86038 = CARTESIAN_POINT ( 'NONE',  ( -21.27928666812490022, 1509.330136533530094, 228.3541946679790158 ) ) ;
#86039 = CARTESIAN_POINT ( 'NONE',  ( 3.629223372069999787, 1485.493217076989822, 199.0019188288989938 ) ) ;
#86040 = CARTESIAN_POINT ( 'NONE',  ( 3.084333964535199701, 1430.771674455919992, 218.0971261273060122 ) ) ;
#86041 = CARTESIAN_POINT ( 'NONE',  ( 4.221485129053400343, 1441.604895247859986, 169.6123329709060101 ) ) ;
#86043 = CARTESIAN_POINT ( 'NONE',  ( -3.550567568200000412, 1421.681120215429701, 184.9649535313980095 ) ) ;
#86042 = CARTESIAN_POINT ( 'NONE',  ( 7.721907888235000073, 1517.026025493960105, 214.1263215447669950 ) ) ;
#86044 = CARTESIAN_POINT ( 'NONE',  ( 20.52130897869999870, 1509.391296556930001, 188.5276697472980061 ) ) ;
#86045 = CARTESIAN_POINT ( 'NONE',  ( -5.779627092215000594, 1516.977993847330026, 216.8424961055369806 ) ) ;
#86046 = ORIENTED_EDGE ( 'NONE', *, *, #55579, .F. ) ;
#86047 = CARTESIAN_POINT ( 'NONE',  ( 7.722102888894769812, 1517.033472268840114, 209.4823235324890334 ) ) ;
#86048 = DIRECTION ( 'NONE',  ( -0.6736849260863841948, 0.000000000000000000, 0.7390186874254148774 ) ) ;
#86049 = ORIENTED_EDGE ( 'NONE', *, *, #19250, .F. ) ;
#86050 = VECTOR ( 'NONE', #99509, 1000.000000000000000 ) ;
#86051 = CARTESIAN_POINT ( 'NONE',  ( 9.803834995107230554, 1517.151704408390060, 221.6221720662910002 ) ) ;
#86052 = ADVANCED_FACE ( 'NONE', ( #24239 ), #105467, .F. ) ;
#86053 = DIRECTION ( 'NONE',  ( 0.8775825618903687619, 0.000000000000000000, 0.4794255386042102218 ) ) ;
#86054 = CARTESIAN_POINT ( 'NONE',  ( 2.273033093151346939, 1525.821544997590308, 177.3097463090895189 ) ) ;
#86055 = PRODUCT_DEFINITION_CONTEXT ( 'detailed design', #97107, 'design' ) ;
#86056 = CARTESIAN_POINT ( 'NONE',  ( 5.128935729357530171, 1424.665416358850052, 191.8839303524709976 ) ) ;
#86057 = CARTESIAN_POINT ( 'NONE',  ( -31.97190655716365626, 1524.330813522192102, 201.5540712235616638 ) ) ;
#86058 = CARTESIAN_POINT ( 'NONE',  ( -2.188078410709979771, 1508.020976590390092, 220.9453026643990086 ) ) ;
#86059 = CARTESIAN_POINT ( 'NONE',  ( 15.10371960350000009, 1409.440493898030127, 192.9533952332979823 ) ) ;
#86060 = CARTESIAN_POINT ( 'NONE',  ( 17.33159144739991575, 1507.668180251339209, 230.9408620993981458 ) ) ;
#86061 = CARTESIAN_POINT ( 'NONE',  ( -6.628886050447888145, 1457.835213357252087, 215.9907006640574423 ) ) ;
#86062 = EDGE_CURVE ( 'NONE', #101516, #4376, #110505, .T. ) ;
#86063 = CARTESIAN_POINT ( 'NONE',  ( -2.500000000000000000, 1443.913060387330006, 150.6726614421979775 ) ) ;
#86064 = CARTESIAN_POINT ( 'NONE',  ( 38.99928884940030116, 1440.913060375190071, 257.8291480320509663 ) ) ;
#86066 = LINE ( 'NONE', #78774, #60521 ) ;
#86065 = CARTESIAN_POINT ( 'NONE',  ( -14.20525606923979822, 1416.383994347770113, 203.1489080140429735 ) ) ;
#86067 = ORIENTED_EDGE ( 'NONE', *, *, #12530, .T. ) ;
#86068 = CARTESIAN_POINT ( 'NONE',  ( -7.649964371800000329, 1508.551704408389924, 219.0282674226889981 ) ) ;
#86069 = CARTESIAN_POINT ( 'NONE',  ( 24.65551417620000407, 1449.825726189819989, 207.1786036389680135 ) ) ;
#86070 = LINE ( 'NONE', #58127, #77084 ) ;
#86071 = DIRECTION ( 'NONE',  ( 0.9455185755993178454, 0.000000000000000000, -0.3255681544571537578 ) ) ;
#86072 = CARTESIAN_POINT ( 'NONE',  ( -4.059748297103329406, 1426.017828923427942, 186.0954046221966109 ) ) ;
#86073 = CARTESIAN_POINT ( 'NONE',  ( -19.53786426059057746, 1511.187213306747708, 180.5239794925695946 ) ) ;
#86074 = CARTESIAN_POINT ( 'NONE',  ( -22.91361795061149920, 1509.842955864680107, 188.6798147461790052 ) ) ;
#86075 = CARTESIAN_POINT ( 'NONE',  ( -1.530900592538410043, 1457.980095062469900, 229.8454460011110143 ) ) ;
#86076 = CARTESIAN_POINT ( 'NONE',  ( -4.038581993089999322, 1515.598601291389969, 208.7452962358790103 ) ) ;
#86077 = CARTESIAN_POINT ( 'NONE',  ( -64.82673933009961331, 1383.790673287549907, 288.1958069606300228 ) ) ;
#86078 = CARTESIAN_POINT ( 'NONE',  ( 24.10320139190000432, 1451.260843396730024, 140.0407038608980201 ) ) ;
#86079 = DIRECTION ( 'NONE',  ( 1.755985294532464991E-16, -1.000000000000000000, 1.338183447452830017E-16 ) ) ;
#86082 = ADVANCED_FACE ( 'NONE', ( #51678 ), #109056, .T. ) ;
#86081 = AXIS2_PLACEMENT_3D ( 'NONE', #8686, #18737, #44524 ) ;
#86080 = CARTESIAN_POINT ( 'NONE',  ( -1.856688514214469787, 1516.535411464260051, 201.4127852243740051 ) ) ;
#86084 = ORIENTED_EDGE ( 'NONE', *, *, #84265, .T. ) ;
#86083 = CARTESIAN_POINT ( 'NONE',  ( 10.45300839642550095, 1451.886422029280084, 207.8125584717180061 ) ) ;
#86085 = CARTESIAN_POINT ( 'NONE',  ( -17.29937165656953013, 1460.725061093811519, 228.2665015787683274 ) ) ;
#86086 = CARTESIAN_POINT ( 'NONE',  ( -78.60087703010000837, 1380.062901053669975, 298.2649052036589978 ) ) ;
#86087 = CARTESIAN_POINT ( 'NONE',  ( 20.25449715238289627, 1509.423786278329999, 230.0845035740109950 ) ) ;
#86088 = EDGE_LOOP ( 'NONE', ( #97156, #87703, #58711, #42863, #3384, #106883 ) ) ;
#86089 = ORIENTED_EDGE ( 'NONE', *, *, #46735, .F. ) ;
#86090 = CARTESIAN_POINT ( 'NONE',  ( -7.756928808066270165, 1508.430203411700177, 219.4938965895260026 ) ) ;
#86091 = DIRECTION ( 'NONE',  ( 6.938893903907222067E-15, 0.000000000000000000, 1.000000000000000000 ) ) ;
#86092 = CARTESIAN_POINT ( 'NONE',  ( 40.24658834409459729, 1443.000124224550063, 137.0450759061350254 ) ) ;
#86094 = CARTESIAN_POINT ( 'NONE',  ( -38.63859217040000260, 1453.572267226629947, 261.7057268775980106 ) ) ;
#86093 = CARTESIAN_POINT ( 'NONE',  ( 20.60842128290000019, 1470.808655614429881, 209.2898127946290003 ) ) ;
#86095 = CARTESIAN_POINT ( 'NONE',  ( 8.743403136036231871, 1436.332529221019968, 208.7150008048009795 ) ) ;
#86096 = CARTESIAN_POINT ( 'NONE',  ( -109.9794884180000167, 1384.897685350450047, 296.9898195259589784 ) ) ;
#86097 = AXIS2_PLACEMENT_3D ( 'NONE', #74416, #13911, #40233 ) ;
#86098 = CARTESIAN_POINT ( 'NONE',  ( -11.51430234028174659, 1434.846150746961939, 151.4276967473332718 ) ) ;
#86099 = LINE ( 'NONE', #44670, #83518 ) ;
#86100 = CARTESIAN_POINT ( 'NONE',  ( 3.859899927900000360, 1409.047851062930022, 187.4971536713979958 ) ) ;
#86101 = CARTESIAN_POINT ( 'NONE',  ( 3.535327672168380175, 1487.160996015089950, 197.6951163816430039 ) ) ;
#86102 = CARTESIAN_POINT ( 'NONE',  ( -6.907297315470000143, 1441.639242787609874, 154.4648440498980051 ) ) ;
#86103 = CARTESIAN_POINT ( 'NONE',  ( 9.005225986101351054, 1434.097730569279975, 205.2808843445390039 ) ) ;
#86104 = CARTESIAN_POINT ( 'NONE',  ( -11.82672180567140074, 1422.987463746610047, 204.1159878212820047 ) ) ;
#86105 = CARTESIAN_POINT ( 'NONE',  ( -23.98473687499999940, 1450.847192898529784, 140.5494830415979948 ) ) ;
#86106 = CARTESIAN_POINT ( 'NONE',  ( 0.3198754856440000349, 1465.430268038429858, 236.3116685324980040 ) ) ;
#86107 = EDGE_LOOP ( 'NONE', ( #105234, #60881, #85167, #96337 ) ) ;
#86108 = CARTESIAN_POINT ( 'NONE',  ( -12.92111071619999940, 1506.047764528690095, 209.0897718066489688 ) ) ;
#86109 = CARTESIAN_POINT ( 'NONE',  ( -3.219437420819999840, 1471.841586492590068, 187.3725962029989773 ) ) ;
#86110 = CARTESIAN_POINT ( 'NONE',  ( -44.13010932679999598, 1442.529835151319958, 270.2165850160980085 ) ) ;
#86111 = CARTESIAN_POINT ( 'NONE',  ( 4.500000000000000000, 1448.210448412289907, 182.3842140122979743 ) ) ;
#86112 = CARTESIAN_POINT ( 'NONE',  ( 17.99954499820000109, 1410.904693969529944, 222.9872228725980108 ) ) ;
#86113 = CARTESIAN_POINT ( 'NONE',  ( 16.31021256559999699, 1449.492267977409711, 190.3239795148979852 ) ) ;
#86114 = AXIS2_PLACEMENT_3D ( 'NONE', #99513, #81616, #30676 ) ;
#86115 = CARTESIAN_POINT ( 'NONE',  ( 0.9796450454589999968, 1519.913060387329779, 185.5578019107980197 ) ) ;
#86116 = CARTESIAN_POINT ( 'NONE',  ( 2.877037746629070192, 1409.300644392530103, 231.0559814730769972 ) ) ;
#86117 = CARTESIAN_POINT ( 'NONE',  ( -11.77719994004817039, 1507.564759764977225, 208.2431318170986572 ) ) ;
#86118 = CARTESIAN_POINT ( 'NONE',  ( -5.334367723879999801, 1417.997726539230143, 234.5082296770980008 ) ) ;
#86119 = CARTESIAN_POINT ( 'NONE',  ( -105.5485668489999966, 1388.544618357170066, 309.1779867852590655 ) ) ;
#86120 = CARTESIAN_POINT ( 'NONE',  ( -0.3233743197617713894, 1485.844240999069598, 181.8492774525526272 ) ) ;
#86121 = CARTESIAN_POINT ( 'NONE',  ( -4.209351669747369407, 1359.579323995338200, 210.6218459617030021 ) ) ;
#86122 = CARTESIAN_POINT ( 'NONE',  ( -45.41124627136969849, 1437.168790165909968, 266.1958325039140618 ) ) ;
#86123 = CARTESIAN_POINT ( 'NONE',  ( -5.864566082395450408, 1517.151704408390060, 192.0899093523580063 ) ) ;
#86124 = CARTESIAN_POINT ( 'NONE',  ( -7.990476243889999886, 1424.874074065990271, 210.4763446083090059 ) ) ;
#86125 = ORIENTED_EDGE ( 'NONE', *, *, #22334, .T. ) ;
#86126 = CARTESIAN_POINT ( 'NONE',  ( 1.715109447055000125, 1516.963431999339946, 209.8570730874349977 ) ) ;
#86127 = CARTESIAN_POINT ( 'NONE',  ( -10.77443953700000101, 1387.520226337789836, 201.1700256806890081 ) ) ;
#86128 = CARTESIAN_POINT ( 'NONE',  ( -33.13357216314891929, 1523.313115944345554, 200.8872321731306272 ) ) ;
#86129 = CARTESIAN_POINT ( 'NONE',  ( 7.326032238172809130, 1426.385876809990123, 212.7391182884030059 ) ) ;
#86130 = VECTOR ( 'NONE', #32746, 1000.000000000000000 ) ;
#86131 = CARTESIAN_POINT ( 'NONE',  ( -26.88813706803909653, 1450.873201854049967, 136.4178382659040096 ) ) ;
#86132 = VERTEX_POINT ( 'NONE', #33746 ) ;
#86133 = CARTESIAN_POINT ( 'NONE',  ( -16.27487920219974171, 1409.481386702927466, 225.0626368816978982 ) ) ;
#86135 = CARTESIAN_POINT ( 'NONE',  ( -15.31201882530910119, 1512.804203059170050, 222.7675833470860027 ) ) ;
#86134 = CARTESIAN_POINT ( 'NONE',  ( -2.214867471995963566, 1525.730671948510917, 176.6953685902578570 ) ) ;
#86136 = CARTESIAN_POINT ( 'NONE',  ( 1.798881530780000126, 1414.793106040730208, 232.3921639753980344 ) ) ;
#86137 = CARTESIAN_POINT ( 'NONE',  ( 3.451191875628176753, 1523.678648413191695, 243.0729557893954791 ) ) ;
#86138 = CARTESIAN_POINT ( 'NONE',  ( -0.3143867530260010534, 1455.265365023490176, 215.8131651789690011 ) ) ;
#86139 = CARTESIAN_POINT ( 'NONE',  ( -25.55352470659999753, 1439.395922612140112, 138.2402125053979773 ) ) ;
#86140 = ORIENTED_EDGE ( 'NONE', *, *, #52178, .T. ) ;
#86141 = CARTESIAN_POINT ( 'NONE',  ( -3.047457018506829485, 1409.276789394889875, 270.3711182856380333 ) ) ;
#86142 = CARTESIAN_POINT ( 'NONE',  ( -2.297629659184999618, 1516.970035769810011, 208.3868227339359862 ) ) ;
#86143 = CARTESIAN_POINT ( 'NONE',  ( 4.825278127329029942, 1416.231055590679944, 231.5676602141780052 ) ) ;
#86144 = LINE ( 'NONE', #42481, #37558 ) ;
#86146 = ORIENTED_EDGE ( 'NONE', *, *, #100152, .F. ) ;
#86145 = CARTESIAN_POINT ( 'NONE',  ( -7.850666375130202823, 1365.384408210369429, 208.3718459617061285 ) ) ;
#86147 = EDGE_LOOP ( 'NONE', ( #87241, #62636, #39123, #103646 ) ) ;
#86148 = CARTESIAN_POINT ( 'NONE',  ( -23.73482365112180048, 1410.983419591109850, 210.2719065163740026 ) ) ;
#86149 = CARTESIAN_POINT ( 'NONE',  ( -0.5842822571356600658, 1410.310976816329912, 185.0864727095799935 ) ) ;
#86150 = CARTESIAN_POINT ( 'NONE',  ( 3.637347128655072481, 1424.394824945528399, 184.3428791968424036 ) ) ;
#86151 = CARTESIAN_POINT ( 'NONE',  ( -11.59417695439999996, 1428.981093279630159, 133.6118001900980232 ) ) ;
#86152 = B_SPLINE_CURVE_WITH_KNOTS ( 'NONE', 3,
 ( #90810, #82425, #31451, #74030, #108162, #97032, #88635, #46090, #4081, #71869, #105986, #55040, #93550, #75680, #50484, #91910, #40957, #108717, #6797, #57790, #101384, #67292, #15187, #76222, #16281, #101949, #66197, #25236, #110365, #32008, #42617, #49375, #14653, #59440 ),
 .UNSPECIFIED., .F., .F.,
 ( 4, 3, 3, 3, 3, 3, 3, 3, 3, 3, 3, 4 ),
 ( -7.942685506149999242, -7.854675769405689678, -7.548843613729729896, -7.215342110406210097, -6.846990903797389727, -6.377391753856749723, -5.953803517216489816, -5.599849543008009967, -5.359340702741580031, -4.827138227139039728, -4.194202119578910093, -3.257013150989999772 ),
 .UNSPECIFIED. ) ;
#86153 =( GEOMETRIC_REPRESENTATION_CONTEXT ( 3 ) GLOBAL_UNCERTAINTY_ASSIGNED_CONTEXT ( ( #93887 ) ) GLOBAL_UNIT_ASSIGNED_CONTEXT ( ( #41656, #109963, #84197 ) ) REPRESENTATION_CONTEXT ( 'NONE', 'WORKASPACE' ) );
#86154 = CARTESIAN_POINT ( 'NONE',  ( -19.58644262093049804, 1461.583877449769943, 193.6422725452479767 ) ) ;
#86155 = CARTESIAN_POINT ( 'NONE',  ( -20.42850894749999924, 1420.829206022629933, 220.9923232775979898 ) ) ;
#86156 = CARTESIAN_POINT ( 'NONE',  ( 41.14170836581870105, 1456.835253165500035, 268.3722864362400173 ) ) ;
#86157 = CARTESIAN_POINT ( 'NONE',  ( -11.42304708970420002, 1391.913060387289988, 207.3451802848499881 ) ) ;
#86158 = CARTESIAN_POINT ( 'NONE',  ( -16.94780996901901204, 1421.954292645319583, 226.8349865805433296 ) ) ;
#86159 = CARTESIAN_POINT ( 'NONE',  ( -2.492130661305000050, 1516.778761582560037, 205.6761608547170113 ) ) ;
#86160 = ORIENTED_EDGE ( 'NONE', *, *, #97844, .F. ) ;
#86161 = DIRECTION ( 'NONE',  ( 0.8386695113602913310, -0.4884709562387192228, -0.2408932868012753081 ) ) ;
#86162 = CARTESIAN_POINT ( 'NONE',  ( 1.525475311809489920, 1454.505970651009875, 183.4105038380650115 ) ) ;
#86163 = CARTESIAN_POINT ( 'NONE',  ( 23.39550544339999760, 1409.988940844130184, 208.4616023169569985 ) ) ;
#86164 = ORIENTED_EDGE ( 'NONE', *, *, #105580, .F. ) ;
#86165 = CARTESIAN_POINT ( 'NONE',  ( 3.744311016462700259, 1509.032041868229953, 204.8808983862890045 ) ) ;
#86166 = CARTESIAN_POINT ( 'NONE',  ( 25.40507033939829995, 1452.020727665570121, 135.4560029008310096 ) ) ;
#86167 = CARTESIAN_POINT ( 'NONE',  ( -3.053241897311849584, 1508.551704408389924, 214.0456212180230011 ) ) ;
#86168 = CARTESIAN_POINT ( 'NONE',  ( -3.078458355219999998, 1384.919541752539999, 199.6700055799090023 ) ) ;
#86169 = CARTESIAN_POINT ( 'NONE',  ( 7.526678075229999543, 1423.047586979970220, 195.6744525590990236 ) ) ;
#86170 = CARTESIAN_POINT ( 'NONE',  ( 18.51573764629999630, 1410.055922931730038, 194.7836524695979961 ) ) ;
#86171 = CARTESIAN_POINT ( 'NONE',  ( 20.24673233129999872, 1443.913060387330006, 162.1129423953979938 ) ) ;
#86172 = CARTESIAN_POINT ( 'NONE',  ( -4.500000000000000000, 1425.929641636930000, 184.1455913746980002 ) ) ;
#86174 = CARTESIAN_POINT ( 'NONE',  ( -22.68797206934306487, 1432.005947149859367, 215.9728551277908650 ) ) ;
#86173 = CARTESIAN_POINT ( 'NONE',  ( 30.25956561551600998, 1524.775785348137788, 196.4597071787796665 ) ) ;
#86175 = CARTESIAN_POINT ( 'NONE',  ( 6.936014448009999889, 1409.155271349029817, 229.3511990319979930 ) ) ;
#86176 = AXIS2_PLACEMENT_3D ( 'NONE', #52112, #58, #67813 ) ;
#86177 = CARTESIAN_POINT ( 'NONE',  ( 19.53757103644559834, 1500.216194704430109, 229.0545849299770111 ) ) ;
#86178 = CARTESIAN_POINT ( 'NONE',  ( 27.68516842258932087, 1508.595246554458527, 207.6423249480233437 ) ) ;
#86179 = DIRECTION ( 'NONE',  ( -1.755985294532469921E-16, 1.000000000000000000, -1.338183447452831989E-16 ) ) ;
#86180 = ORIENTED_EDGE ( 'NONE', *, *, #84890, .T. ) ;
#86181 = CARTESIAN_POINT ( 'NONE',  ( -2.038646110889675178, 1525.960063244516959, 177.0579350083066004 ) ) ;
#86182 = CARTESIAN_POINT ( 'NONE',  ( 11.40717599968280105, 1432.341607277799994, 151.3374035920139988 ) ) ;
#86183 = CARTESIAN_POINT ( 'NONE',  ( -6.504448388238199819, 1484.623890501229880, 199.1483530729989866 ) ) ;
#86184 = CARTESIAN_POINT ( 'NONE',  ( -12.11107905609999946, 1390.909553154740024, 205.6216718233689846 ) ) ;
#86185 = CARTESIAN_POINT ( 'NONE',  ( 12.67629937430701936, 1426.478869958664063, 202.7079000866955028 ) ) ;
#86186 = CARTESIAN_POINT ( 'NONE',  ( 0.1166470182406819933, 1506.491018773052474, 231.1523900923795907 ) ) ;
#86187 = CARTESIAN_POINT ( 'NONE',  ( -19.47651265109999841, 1455.559577374430091, 243.9198229294980251 ) ) ;
#86188 = CARTESIAN_POINT ( 'NONE',  ( -8.893072318575100610, 1384.473093328959976, 218.6576864550619916 ) ) ;
#86189 = CARTESIAN_POINT ( 'NONE',  ( 11.52617294090000044, 1433.738990838459813, 151.2724044377980022 ) ) ;
#86190 = CARTESIAN_POINT ( 'NONE',  ( 20.63825565839999854, 1456.438754565230056, 248.0989693098979956 ) ) ;
#86191 = CARTESIAN_POINT ( 'NONE',  ( 12.73594778886240064, 1416.524489948229984, 196.2724390681139823 ) ) ;
#86192 = CARTESIAN_POINT ( 'NONE',  ( -17.59937028154769934, 1418.719235195160081, 207.0514148608630194 ) ) ;
#86193 = CARTESIAN_POINT ( 'NONE',  ( -1.842962214296178569, 1515.219201590507282, 213.4472514034267761 ) ) ;
#86194 = CARTESIAN_POINT ( 'NONE',  ( 19.70594995229999924, 1434.992946305079840, 210.6610983617879924 ) ) ;
#86195 = CARTESIAN_POINT ( 'NONE',  ( -13.58259380279999995, 1486.033890773129997, 185.4071426780979834 ) ) ;
#86196 = CARTESIAN_POINT ( 'NONE',  ( -14.04637195990000009, 1416.570631226729802, 227.2989283747980096 ) ) ;
#86197 = CARTESIAN_POINT ( 'NONE',  ( 18.19590854888164699, 1512.187213306747481, 238.2026672068774644 ) ) ;
#86198 = AXIS2_PLACEMENT_3D ( 'NONE', #62814, #4521, #46538 ) ;
#86199 = CARTESIAN_POINT ( 'NONE',  ( 22.66911695310000141, 1410.908238429030007, 214.4050216980779737 ) ) ;
#86200 = CARTESIAN_POINT ( 'NONE',  ( 2.572472979250941538, 1447.610664903252655, 170.5280182008338272 ) ) ;
#86201 = CARTESIAN_POINT ( 'NONE',  ( 26.23841509872854161, 1436.700912505007864, 136.8690137196103933 ) ) ;
#86202 = CARTESIAN_POINT ( 'NONE',  ( -11.80945589138680063, 1383.861482993130039, 218.7560470375080115 ) ) ;
#86203 = CARTESIAN_POINT ( 'NONE',  ( -16.53114555299940136, 1465.611457094120169, 220.7423133389369809 ) ) ;
#86204 = CARTESIAN_POINT ( 'NONE',  ( 7.334957356574999920, 1517.030858226499959, 213.7381182667970165 ) ) ;
#86205 = CARTESIAN_POINT ( 'NONE',  ( -20.36885094410000008, 1418.422628033280034, 210.1555047974290176 ) ) ;
#86206 = CARTESIAN_POINT ( 'NONE',  ( 9.008848419482919923, 1451.404950095520007, 211.2754342882610104 ) ) ;
#86208 = VERTEX_POINT ( 'NONE', #59529 ) ;
#86207 = CARTESIAN_POINT ( 'NONE',  ( 3.711571330249999967, 1441.008188660590122, 218.3178908880789777 ) ) ;
#86209 = CARTESIAN_POINT ( 'NONE',  ( 16.81223453394349932, 1414.913060391199906, 210.6693087035600058 ) ) ;
#86210 = CARTESIAN_POINT ( 'NONE',  ( 22.86388144384979881, 1435.295931049420005, 134.1000000033949959 ) ) ;
#86211 = CARTESIAN_POINT ( 'NONE',  ( 13.80504973719999917, 1434.979586003610166, 149.9810039891980011 ) ) ;
#86212 = CARTESIAN_POINT ( 'NONE',  ( -31.75407494088130278, 1525.055427061272439, 216.6568988463208996 ) ) ;
#86213 = CARTESIAN_POINT ( 'NONE',  ( -8.627785716502410551, 1437.492545073600013, 228.3379458911339839 ) ) ;
#86214 = ORIENTED_EDGE ( 'NONE', *, *, #73558, .F. ) ;
#86215 = CARTESIAN_POINT ( 'NONE',  ( -5.663447254089099658, 1391.839989632750076, 203.2423981696859983 ) ) ;
#86216 = CARTESIAN_POINT ( 'NONE',  ( -14.48038155212669942, 1380.012369224539952, 208.7075723164790304 ) ) ;
#86217 = CARTESIAN_POINT ( 'NONE',  ( 6.326340444085493786, 1446.650791557884077, 202.6322225399144372 ) ) ;
#86218 = CARTESIAN_POINT ( 'NONE',  ( 11.59121695358153303, 1426.214086040526126, 138.6115839517644304 ) ) ;
#86219 = EDGE_CURVE ( 'NONE', #1439, #77110, #99769, .T. ) ;
#86220 = CARTESIAN_POINT ( 'NONE',  ( 25.78167222729700114, 1509.813387082529971, 195.1140727163279962 ) ) ;
#86221 = CARTESIAN_POINT ( 'NONE',  ( 0.4435022289555869968, 1418.672171135500093, 184.7048927309859891 ) ) ;
#86222 = CARTESIAN_POINT ( 'NONE',  ( 14.25613302710000063, 1464.413060387330006, 224.0689215379980226 ) ) ;
#86223 = CARTESIAN_POINT ( 'NONE',  ( 0.000000000000000000, 1523.051704408389696, 209.1218459616979999 ) ) ;
#86224 = CARTESIAN_POINT ( 'NONE',  ( -11.84218506250000047, 1391.913060323489844, 208.2592681188410211 ) ) ;
#86225 = CARTESIAN_POINT ( 'NONE',  ( -69.05597640560989703, 1385.107553815650135, 263.9271920575239392 ) ) ;
#86226 = CARTESIAN_POINT ( 'NONE',  ( -9.809994025999090539, 1391.913060387289988, 214.8154631801960193 ) ) ;
#86227 = CARTESIAN_POINT ( 'NONE',  ( -16.79549422457180796, 1379.712786052571118, 208.6606538604273453 ) ) ;
#86228 = VERTEX_POINT ( 'NONE', #729 ) ;
#86229 = CARTESIAN_POINT ( 'NONE',  ( -15.72121095137550206, 1409.846661881940008, 226.2995151419540036 ) ) ;
#86231 = VERTEX_POINT ( 'NONE', #93641 ) ;
#86230 = CARTESIAN_POINT ( 'NONE',  ( 2.253566441613126910E-10, 1426.918876941764893, 137.0999999980979851 ) ) ;
#86232 = CARTESIAN_POINT ( 'NONE',  ( 5.864566082395450408, 1522.051704408389924, 226.1537825710409777 ) ) ;
#86233 = ORIENTED_EDGE ( 'NONE', *, *, #81571, .T. ) ;
#86234 = CARTESIAN_POINT ( 'NONE',  ( 5.145309177750649887, 1422.426130283250131, 194.5914460530619863 ) ) ;
#86235 = CARTESIAN_POINT ( 'NONE',  ( -7.562440734658915531, 1363.099625272887806, 207.6218459616988241 ) ) ;
#86236 = CARTESIAN_POINT ( 'NONE',  ( -12.02051099930000078, 1491.153688734890011, 206.6632163140190244 ) ) ;
#86237 = CARTESIAN_POINT ( 'NONE',  ( 38.91493664412075049, 1452.437576044287198, 269.5915040112719225 ) ) ;
#86238 = CARTESIAN_POINT ( 'NONE',  ( 15.18044682235556664, 1511.791180387471059, 197.3654389570463081 ) ) ;
#86239 = CARTESIAN_POINT ( 'NONE',  ( 15.14181670882874187, 1430.803132298357241, 219.9013560687592985 ) ) ;
#86240 = CARTESIAN_POINT ( 'NONE',  ( -7329.274061526074547, -2340.220200558883789, -10678.01295216180006 ) ) ;
#86241 = CARTESIAN_POINT ( 'NONE',  ( -7.002187114500163290, 1516.573284371974751, 211.8084850268393495 ) ) ;
#86242 = CARTESIAN_POINT ( 'NONE',  ( -11.81780673814840021, 1517.051704408389924, 222.7166774759110126 ) ) ;
#86243 = CARTESIAN_POINT ( 'NONE',  ( -9.232879690934204575, 1367.985994792911470, 207.6218459616987673 ) ) ;
#86244 = CARTESIAN_POINT ( 'NONE',  ( 10.78522152235938947, 1424.939302195395612, 142.2917100169879348 ) ) ;
#86245 = CARTESIAN_POINT ( 'NONE',  ( -3.462620856235000044, 1516.938330505699923, 206.6435391121569864 ) ) ;
#86246 = CARTESIAN_POINT ( 'NONE',  ( 3.709912251430000030, 1447.069506931650039, 154.3963888670980111 ) ) ;
#86247 = CARTESIAN_POINT ( 'NONE',  ( -2.500000000000000000, 1432.302173844710069, 157.4936352153980010 ) ) ;
#86248 = CARTESIAN_POINT ( 'NONE',  ( -3.490463098060000213, 1496.905315118289991, 198.4270279902989955 ) ) ;
#86250 = ORIENTED_EDGE ( 'NONE', *, *, #90736, .F. ) ;
#86249 = CARTESIAN_POINT ( 'NONE',  ( -2.215101663730000059, 1496.819187201989962, 221.3100143584990178 ) ) ;
#86251 = CARTESIAN_POINT ( 'NONE',  ( -33.91369110859999836, 1435.681798638700002, 135.0664268289980043 ) ) ;
#86252 = EDGE_LOOP ( 'NONE', ( #67192, #78437, #45909, #45369 ) ) ;
#86253 = CARTESIAN_POINT ( 'NONE',  ( 35.51625767599999506, 1423.702336106529856, 261.8360507833979796 ) ) ;
#86254 = ADVANCED_FACE ( 'NONE', ( #104281 ), #8923, .F. ) ;
#86255 = CARTESIAN_POINT ( 'NONE',  ( -25.05872055609999904, 1449.799157997629891, 205.7769664646480123 ) ) ;
#86257 = CARTESIAN_POINT ( 'NONE',  ( 17.16028268420890157, 1410.456713703000105, 192.2572872432389772 ) ) ;
#86256 = CARTESIAN_POINT ( 'NONE',  ( -11.50904860320000012, 1426.838353685629954, 127.8453462649979997 ) ) ;
#86258 = EDGE_CURVE ( 'NONE', #1945, #43546, #78673, .T. ) ;
#86259 = CARTESIAN_POINT ( 'NONE',  ( -6.546001388695000145, 1516.557392317769882, 210.8318505190270002 ) ) ;
#86260 = CARTESIAN_POINT ( 'NONE',  ( 4.034101557127501181, 1509.184792326690058, 179.3359848413445832 ) ) ;
#86261 = ADVANCED_FACE ( 'NONE', ( #86368 ), #49117, .F. ) ;
#86262 = CARTESIAN_POINT ( 'NONE',  ( -18.90776566690000138, 1416.839648768930147, 208.2177105294629769 ) ) ;
#86263 = CARTESIAN_POINT ( 'NONE',  ( -27.41409751149999963, 1415.612339528129951, 262.1295707058980042 ) ) ;
#86264 = CARTESIAN_POINT ( 'NONE',  ( 18.98069862813439812, 1509.597656182110086, 231.8600174792910025 ) ) ;
#86265 = EDGE_CURVE ( 'NONE', #43307, #6784, #91133, .T. ) ;
#86266 = CARTESIAN_POINT ( 'NONE',  ( 17.44123683046308315, 1460.026124469276283, 228.4392115393495715 ) ) ;
#86267 = EDGE_CURVE ( 'NONE', #86906, #41878, #75808, .T. ) ;
#86268 = CARTESIAN_POINT ( 'NONE',  ( -4.995284487919999350, 1391.732982292789984, 214.7012254044889801 ) ) ;
#86269 = CARTESIAN_POINT ( 'NONE',  ( -34.95989591692970322, 1437.134820888970125, 136.5390585529150087 ) ) ;
#86270 = ORIENTED_EDGE ( 'NONE', *, *, #18154, .F. ) ;
#86271 = CARTESIAN_POINT ( 'NONE',  ( 6.016803703712399809, 1396.654461611120041, 220.0432444583680081 ) ) ;
#86272 = CARTESIAN_POINT ( 'NONE',  ( 10.84791127679310030, 1460.615700148999849, 207.7176790179939871 ) ) ;
#86273 = CARTESIAN_POINT ( 'NONE',  ( -17.31269850480000017, 1460.709739774729996, 228.2660248434980019 ) ) ;
#86274 = ORIENTED_EDGE ( 'NONE', *, *, #110461, .F. ) ;
#86275 = ORIENTED_EDGE ( 'NONE', *, *, #1250, .T. ) ;
#86276 = CARTESIAN_POINT ( 'NONE',  ( 9.296700322752400325, 1453.078792441659971, 212.1083447425310169 ) ) ;
#86277 = FACE_OUTER_BOUND ( 'NONE', #106506, .T. ) ;
#86279 = ORIENTED_EDGE ( 'NONE', *, *, #35986, .T. ) ;
#86278 = B_SPLINE_CURVE_WITH_KNOTS ( 'NONE', 3,
 ( #91297, #6732, #48768, #40338, #31937, #41457, #56607, #58262, #74519, #31384, #30834, #92383, #100778, #5652, #22405, #66131, #15655, #91842 ),
 .UNSPECIFIED., .F., .F.,
 ( 4, 2, 2, 2, 2, 2, 2, 2, 4 ),
 ( 1.993915778357750142E-11, 0.07958679707882590493, 0.1577458553287279797, 0.2359250188071150001, 0.2750929174303070046, 0.2946670492092580140, 0.3044529509164879966, 0.3142986040616189691, 0.3151139619271109971 ),
 .UNSPECIFIED. ) ;
#86280 = DIRECTION ( 'NONE',  ( 5.980589973904019347E-17, -1.000000000000000000, 1.736889445713099699E-16 ) ) ;
#86281 = CARTESIAN_POINT ( 'NONE',  ( -9.418564982631906446, 1418.460837828868989, 196.9369629217839872 ) ) ;
#86283 = CARTESIAN_POINT ( 'NONE',  ( -19.54170600522309797, 1486.310841334699035, 189.8199399202851225 ) ) ;
#86282 = VECTOR ( 'NONE', #23385, 1000.000000000000000 ) ;
#86284 = CARTESIAN_POINT ( 'NONE',  ( 27.12970368896878171, 1508.933966457487031, 206.1969555583084457 ) ) ;
#86285 = DIRECTION ( 'NONE',  ( 0.3090169943749447312, 0.000000000000000000, -0.9510565162951544194 ) ) ;
#86286 = CARTESIAN_POINT ( 'NONE',  ( 9.216280896211529239, 1450.783082650540109, 209.7718718314580144 ) ) ;
#86287 = CARTESIAN_POINT ( 'NONE',  ( 6.063466849340000131, 1461.859068790690117, 206.6237464808990012 ) ) ;
#86288 = EDGE_CURVE ( 'NONE', #437, #39065, #87636, .T. ) ;
#86289 = CARTESIAN_POINT ( 'NONE',  ( -95.37154346148018647, 1384.858690459429909, 295.0689016550999781 ) ) ;
#86290 = ORIENTED_EDGE ( 'NONE', *, *, #89272, .T. ) ;
#86291 = CARTESIAN_POINT ( 'NONE',  ( 2.289624432225000117, 1517.154223579619838, 202.5582500624169882 ) ) ;
#86292 = CARTESIAN_POINT ( 'NONE',  ( 5.781585778145000631, 1516.939646076049939, 209.1093989964429909 ) ) ;
#86293 = VERTEX_POINT ( 'NONE', #55004 ) ;
#86294 = CARTESIAN_POINT ( 'NONE',  ( 31.23437356469446158, 1523.382868172864164, 222.8968241038843416 ) ) ;
#86295 = CARTESIAN_POINT ( 'NONE',  ( 3.208451221193931779, 1511.804171812530058, 217.0732872714422115 ) ) ;
#86296 = ORIENTED_EDGE ( 'NONE', *, *, #60329, .T. ) ;
#86297 = CARTESIAN_POINT ( 'NONE',  ( -1.443364724936080146, 1457.295864005700196, 183.6403006531590165 ) ) ;
#86298 = CARTESIAN_POINT ( 'NONE',  ( -7.170583105241029820, 1508.384145562859885, 219.7141895747710123 ) ) ;
#86299 = CARTESIAN_POINT ( 'NONE',  ( 8.935643129749999858, 1508.218061432530021, 235.0249814686980017 ) ) ;
#86300 = EDGE_CURVE ( 'NONE', #82949, #59940, #80440, .T. ) ;
#86301 = DIRECTION ( 'NONE',  ( -0.000000000000000000, 1.000000000000000000, -0.000000000000000000 ) ) ;
#86302 = CARTESIAN_POINT ( 'NONE',  ( -4.997848117199999329, 1422.516530880429855, 184.8641170294979759 ) ) ;
#86303 = CARTESIAN_POINT ( 'NONE',  ( 2.328498457451699810, 1407.969193676269924, 270.2917565518350216 ) ) ;
#86304 = CARTESIAN_POINT ( 'NONE',  ( -103.5806803890000083, 1389.940350142260058, 304.1776731731589507 ) ) ;
#86305 = CARTESIAN_POINT ( 'NONE',  ( -12.72940262790820043, 1502.367719156869953, 210.1495042875829995 ) ) ;
#86306 = EDGE_CURVE ( 'NONE', #50150, #24414, #17811, .T. ) ;
#86307 = CARTESIAN_POINT ( 'NONE',  ( -16.66966706706500290, 1516.995662938509895, 194.6788146269670108 ) ) ;
#86308 = CARTESIAN_POINT ( 'NONE',  ( -44.16865037990000076, 1379.703007072680066, 229.5410392623589928 ) ) ;
#86309 = CARTESIAN_POINT ( 'NONE',  ( 8.400941578297418388, 1424.507064994723351, 195.7368743825176125 ) ) ;
#86311 = CARTESIAN_POINT ( 'NONE',  ( 16.60581947120000024, 1489.466620109829819, 194.3878554425980099 ) ) ;
#86310 = CARTESIAN_POINT ( 'NONE',  ( -4.171844745047410541, 1497.126029642969797, 198.6588305097009766 ) ) ;
#86312 = DIRECTION ( 'NONE',  ( -0.9942586961433749204, -0.000000000000000000, 0.1070030146457375819 ) ) ;
#86313 = CARTESIAN_POINT ( 'NONE',  ( 17.93975917528049990, 1421.697473349219990, 225.1225136664709794 ) ) ;
#86314 = CARTESIAN_POINT ( 'NONE',  ( -5.547914922874206844, 1506.428740433108715, 187.8549363882322893 ) ) ;
#86315 = ORIENTED_EDGE ( 'NONE', *, *, #47763, .F. ) ;
#86316 = CARTESIAN_POINT ( 'NONE',  ( 18.39213345135680200, 1424.508846254459968, 223.4664176072620023 ) ) ;
#86317 = CARTESIAN_POINT ( 'NONE',  ( -21.45464262047638115, 1525.320827368860591, 233.4406584548679859 ) ) ;
#86318 = CARTESIAN_POINT ( 'NONE',  ( -2.994403857541957592, 1485.695008466471108, 182.6247529937351146 ) ) ;
#86319 = CARTESIAN_POINT ( 'NONE',  ( -14.85992380390000100, 1416.181292664740113, 213.2198171372490094 ) ) ;
#86321 = ORIENTED_EDGE ( 'NONE', *, *, #238, .F. ) ;
#86320 = CARTESIAN_POINT ( 'NONE',  ( -0.1141777317403989966, 1515.158022524200078, 204.7948384897389928 ) ) ;
#86322 = CARTESIAN_POINT ( 'NONE',  ( 17.11711237140000108, 1414.913528139930122, 210.6775764032980192 ) ) ;
#86323 = CARTESIAN_POINT ( 'NONE',  ( -24.55197755740000076, 1443.533885484360098, 210.8939174055780086 ) ) ;
#86324 = CARTESIAN_POINT ( 'NONE',  ( -11.71200338719999934, 1428.227207751029937, 149.3442601595979795 ) ) ;
#86325 = CARTESIAN_POINT ( 'NONE',  ( 19.44117294853580091, 1456.941945407359981, 224.4539793896520052 ) ) ;
#86326 = CARTESIAN_POINT ( 'NONE',  ( -10.98329405719170104, 1462.122223828419919, 210.0364276692640146 ) ) ;
#86327 = DIRECTION ( 'NONE',  ( 0.01430194279835390707, 0.9998977151197045998, -0.0001171775870170530692 ) ) ;
#86328 = DIRECTION ( 'NONE',  ( 0.7071067811865474617, -3.909376183068731469E-17, -0.7071067811865474617 ) ) ;
#86329 = CARTESIAN_POINT ( 'NONE',  ( -16.51584608446500013, 1514.088841912139969, 223.6140043943670150 ) ) ;
#86330 = CARTESIAN_POINT ( 'NONE',  ( 15.87811701990000302, 1410.407893985029887, 226.9632077383980118 ) ) ;
#86331 = CARTESIAN_POINT ( 'NONE',  ( -10.44853431733320015, 1480.978285847389998, 207.5981847469569743 ) ) ;
#86332 = CARTESIAN_POINT ( 'NONE',  ( -16.12591782766000037, 1459.081375581680049, 229.9878571019870037 ) ) ;
#86333 = CARTESIAN_POINT ( 'NONE',  ( 0.7351097711180020200, 1516.977504706749869, 206.6301902066870184 ) ) ;
#86334 = CARTESIAN_POINT ( 'NONE',  ( 31.62445009409999841, 1415.432857817130071, 268.6459320787980118 ) ) ;
#86335 = CARTESIAN_POINT ( 'NONE',  ( 24.45980407890000308, 1436.162459971299768, 138.9323611871980120 ) ) ;
#86336 = CARTESIAN_POINT ( 'NONE',  ( 19.47832335489999878, 1430.302475234229860, 194.3997851820979861 ) ) ;
#86337 = PRODUCT_RELATED_PRODUCT_CATEGORY ( 'part', '', ( #105426 ) ) ;
#86338 = CARTESIAN_POINT ( 'NONE',  ( -20.74894096239999897, 1428.237764131229824, 223.0444765198980122 ) ) ;
#86339 = CARTESIAN_POINT ( 'NONE',  ( 19.66678637211940028, 1521.951704408389787, 202.3500283489059939 ) ) ;
#86340 = CARTESIAN_POINT ( 'NONE',  ( 32.38114538885255200, 1523.604703353109699, 216.1203639561429100 ) ) ;
#86341 =( BOUNDED_CURVE ( )  B_SPLINE_CURVE ( 3, ( #73860, #73300, #107435, #37489 ),
 .UNSPECIFIED., .F., .F. ) 
 B_SPLINE_CURVE_WITH_KNOTS ( ( 4, 4 ),
 ( 6.175716230969100273, 6.483011094422519882 ),
 .UNSPECIFIED. ) 
 CURVE ( )  GEOMETRIC_REPRESENTATION_ITEM ( )  RATIONAL_B_SPLINE_CURVE ( ( 1.000000000000000000, 0.9921462910537798274, 0.9921462910537798274, 1.000000000000000000 ) ) 
 REPRESENTATION_ITEM ( '' )  );
#86342 = CARTESIAN_POINT ( 'NONE',  ( -41.15112175996920740, 1443.645559826710041, 136.9181504865389911 ) ) ;
#86343 = CARTESIAN_POINT ( 'NONE',  ( 3.827327206003189985, 1424.046157813739910, 172.2701767048200168 ) ) ;
#86344 = CARTESIAN_POINT ( 'NONE',  ( -18.34777493720000408, 1415.426952350729835, 207.7346860995480142 ) ) ;
#86345 = CARTESIAN_POINT ( 'NONE',  ( -16.89684486387019291, 1409.672993099775113, 193.4350317905646364 ) ) ;
#86346 = CARTESIAN_POINT ( 'NONE',  ( -18.48114474329999979, 1431.113060387329824, 212.6089797988180123 ) ) ;
#86347 = CARTESIAN_POINT ( 'NONE',  ( -32.74366472130000716, 1435.640891862840135, 135.1028903260980201 ) ) ;
#86348 = LINE ( 'NONE', #20239, #81830 ) ;
#86349 = VERTEX_POINT ( 'NONE', #6217 ) ;
#86350 = CARTESIAN_POINT ( 'NONE',  ( -2.541812797074999963, 1512.177707669779920, 201.4966559065569811 ) ) ;
#86351 = CARTESIAN_POINT ( 'NONE',  ( -14.93123092370299965, 1409.434470460630109, 208.8274998085580023 ) ) ;
#86352 = ADVANCED_FACE ( 'NONE', ( #30316 ), #75057, .F. ) ;
#86353 = CARTESIAN_POINT ( 'NONE',  ( -11.43249851594280031, 1508.430448985320027, 208.4158283025909952 ) ) ;
#86354 = CARTESIAN_POINT ( 'NONE',  ( -3.014945144310587022, 1420.039793247956595, 137.0999999980981272 ) ) ;
#86355 = CARTESIAN_POINT ( 'NONE',  ( -14.57206770570000032, 1474.063984277629970, 266.8771244472980015 ) ) ;
#86356 = DIRECTION ( 'NONE',  ( 0.000000000000000000, 1.000000000000000000, 0.000000000000000000 ) ) ;
#86357 = CARTESIAN_POINT ( 'NONE',  ( 0.2861219874754159509, 1419.391003853660095, 184.4958517824849764 ) ) ;
#86358 = EDGE_CURVE ( 'NONE', #8084, #52143, #76842, .T. ) ;
#86359 = CARTESIAN_POINT ( 'NONE',  ( 17.92086665490029773, 1421.088564386509915, 224.2530476824699974 ) ) ;
#86360 = CARTESIAN_POINT ( 'NONE',  ( -67.08513696692429562, 1384.671056508349920, 291.5503426151730650 ) ) ;
#86361 = B_SPLINE_SURFACE_WITH_KNOTS ( 'NONE', 5, 5, ( 
 ( #90217, #89678, #12961, #4585, #98625, #13502, #47691, #73452, #107584 ),
 ( #19719, #43562, #30870, #34044, #77714, #5690, #68234, #6223, #82392 ),
 ( #59274, #39834, #67673, #94489, #86106, #65603, #25627, #16657, #102342 ),
 ( #101780, #73997, #22442, #50855, #17204, #473, #59819, #25071, #40375 ),
 ( #42443, #34597, #74554, #48248, #93392, #90778, #57212, #17761, #93938 ),
 ( #108127, #76601, #31979, #65047, #51401, #110753, #85533, #8828, #108686 ),
 ( #31421, #99162, #99716, #56644, #43013, #14061, #77170, #68783, #91337 ),
 ( #23009, #14621, #48808, #82931, #84983, #8279, #102882, #26180, #60368 ),
 ( #51965, #9400, #53640, #46345, #70445, #11064, #61483, #78255, #20536 ) ),
 .UNSPECIFIED., .F., .F., .F.,
 ( 6, 3, 6 ),
 ( 6, 3, 6 ),
 ( 2.710078270099999909, 5.432775312530000456, 8.155472354960000558 ),
 ( 0.000000000000000000, 1.000000000000000000, 2.000000000000000000 ),
 .UNSPECIFIED. ) ;
#86362 = DIRECTION ( 'NONE',  ( -0.1528503721702839657, -0.4524026203659298195, -0.8786174553316397073 ) ) ;
#86363 = CARTESIAN_POINT ( 'NONE',  ( 17.96129668646389632, 1424.685407009209939, 227.4171637106319963 ) ) ;
#86364 = CARTESIAN_POINT ( 'NONE',  ( 22.52609269710000106, 1509.699688877929930, 227.7124812497979747 ) ) ;
#86365 = CARTESIAN_POINT ( 'NONE',  ( 11.20854089337319870, 1414.996442620860080, 222.5314268542019818 ) ) ;
#86366 = CYLINDRICAL_SURFACE ( 'NONE', #82079, 0.9999999999999569233 ) ;
#86367 = CARTESIAN_POINT ( 'NONE',  ( -11.21032122992201607, 1522.051704408389924, 229.8720270527158220 ) ) ;
#86368 = FACE_OUTER_BOUND ( 'NONE', #85877, .T. ) ;
#86369 = CARTESIAN_POINT ( 'NONE',  ( -23.03736570619999924, 1410.638942846430155, 204.9276098081979853 ) ) ;
#86370 = CARTESIAN_POINT ( 'NONE',  ( 15.65413380780000097, 1416.520322350429979, 199.0527707490979878 ) ) ;
#86371 = CARTESIAN_POINT ( 'NONE',  ( 3.939553394270000286, 1484.542612446990006, 220.2950041541989776 ) ) ;
#86372 = ADVANCED_FACE ( 'NONE', ( #24102 ), #102784, .F. ) ;
#86373 = CARTESIAN_POINT ( 'NONE',  ( 11.30263822180440059, 1479.449500025850057, 208.3515620824809957 ) ) ;
#86374 = CARTESIAN_POINT ( 'NONE',  ( -4.122931283589999374E-15, 1438.194204504490017, 150.6035180695979818 ) ) ;
#86375 = CARTESIAN_POINT ( 'NONE',  ( 8.316512080489999903, 1462.697935791190048, 228.8554007396989789 ) ) ;
#86376 = CARTESIAN_POINT ( 'NONE',  ( -5.513258784733920059, 1508.551704615640119, 216.1343122518819939 ) ) ;
#86377 = CARTESIAN_POINT ( 'NONE',  ( 18.46110511457829872, 1471.786120933839811, 195.2229451478879980 ) ) ;
#86379 = CARTESIAN_POINT ( 'NONE',  ( -8.219561042539998752, 1383.199823560049936, 199.7615019773890026 ) ) ;
#86378 = FACE_OUTER_BOUND ( 'NONE', #43604, .T. ) ;
#86380 = CARTESIAN_POINT ( 'NONE',  ( 0.3144575102820000301, 1415.740843721930105, 233.4848348588980116 ) ) ;
#86381 = CARTESIAN_POINT ( 'NONE',  ( 2.475018616569089946, 1497.111080321040163, 196.9667222483770104 ) ) ;
#86382 = CARTESIAN_POINT ( 'NONE',  ( -14.77932465454309963, 1420.552195126709876, 212.5457007543760142 ) ) ;
#86383 = CARTESIAN_POINT ( 'NONE',  ( 7.882146126611630166, 1449.075262138320113, 202.4510296736249870 ) ) ;
#86384 = CARTESIAN_POINT ( 'NONE',  ( 10.78159844869479933, 1461.896569297480028, 211.1674770051990038 ) ) ;
#86385 = CARTESIAN_POINT ( 'NONE',  ( 4.032397901875000024, 1516.981965530290154, 203.3362630185569913 ) ) ;
#86386 = CARTESIAN_POINT ( 'NONE',  ( -4.219709396322937955, 1398.038964707169271, 221.4179454279745869 ) ) ;
#86387 = CARTESIAN_POINT ( 'NONE',  ( -3.210056062782554065, 1440.596314194909610, 157.0444588582195422 ) ) ;
#86388 = FACE_BOUND ( 'NONE', #20258, .T. ) ;
#86389 = LINE ( 'NONE', #110491, #3692 ) ;
#86390 = SURFACE_STYLE_FILL_AREA ( #94796 ) ;
#86391 = CARTESIAN_POINT ( 'NONE',  ( 41.08515758954219876, 1445.199432839919837, 136.7286086285029967 ) ) ;
#86393 = ORIENTED_EDGE ( 'NONE', *, *, #1250, .F. ) ;
#86392 = CARTESIAN_POINT ( 'NONE',  ( -66.40710909386241667, 1379.744920543010039, 277.0421639454029901 ) ) ;
#86394 = ORIENTED_EDGE ( 'NONE', *, *, #17853, .T. ) ;
#86395 = CARTESIAN_POINT ( 'NONE',  ( 11.92740228873420172, 1433.690821784659875, 150.4649736788460075 ) ) ;
#86396 = CARTESIAN_POINT ( 'NONE',  ( 21.48632729253213114, 1524.478200376968971, 184.1569673976052570 ) ) ;
#86397 = ORIENTED_EDGE ( 'NONE', *, *, #56592, .T. ) ;
#86398 = CARTESIAN_POINT ( 'NONE',  ( -2.571036083430311869, 1463.062948214519793, 199.6378877115486148 ) ) ;
#86399 = EDGE_CURVE ( 'NONE', #75960, #54639, #7133, .T. ) ;
#86400 = CARTESIAN_POINT ( 'NONE',  ( -3.487592469735000478, 1508.551704408389924, 214.1089243866569802 ) ) ;
#86401 = CARTESIAN_POINT ( 'NONE',  ( -4.832616806509495433, 1508.551704408389924, 211.6097810599876254 ) ) ;
#86403 = CARTESIAN_POINT ( 'NONE',  ( 8.828869558830000130, 1428.756629641229893, 91.31218443469779800 ) ) ;
#86402 = CARTESIAN_POINT ( 'NONE',  ( -4.363122647530000009, 1418.913060387330006, 172.2701767054979882 ) ) ;
#86404 = CARTESIAN_POINT ( 'NONE',  ( 6.486837805662870160, 1498.104514242190135, 235.0024069431659939 ) ) ;
#86405 = EDGE_CURVE ( 'NONE', #56812, #109512, #69363, .T. ) ;
#86406 = CARTESIAN_POINT ( 'NONE',  ( 9.868861043749999951, 1507.633046480430039, 183.6677869673980013 ) ) ;
#86407 = CARTESIAN_POINT ( 'NONE',  ( -2.525974214079999669, 1414.913060387329779, 193.2525438407980118 ) ) ;
#86408 = DIRECTION ( 'NONE',  ( 0.000000000000000000, 0.000000000000000000, -1.000000000000000000 ) ) ;
#86409 = CARTESIAN_POINT ( 'NONE',  ( -2.476733514145000203, 1516.858326417339867, 211.6155457388669845 ) ) ;
#86410 = CARTESIAN_POINT ( 'NONE',  ( 37.09403179586560384, 1436.457961864639856, 134.0999999968530005 ) ) ;
#86411 = CARTESIAN_POINT ( 'NONE',  ( -5.292247061280000331, 1391.913060387289988, 203.8075142969990168 ) ) ;
#86412 = CARTESIAN_POINT ( 'NONE',  ( 7.014484243095000515, 1513.886778333999928, 201.4788231846570170 ) ) ;
#86413 = ORIENTED_EDGE ( 'NONE', *, *, #66461, .F. ) ;
#86414 = CARTESIAN_POINT ( 'NONE',  ( 14.06373079481629951, 1435.540244135899911, 149.8224532940170093 ) ) ;
#86415 = CARTESIAN_POINT ( 'NONE',  ( -14.52721453695589915, 1441.419400887780057, 221.0377524652309944 ) ) ;
#86416 = ORIENTED_EDGE ( 'NONE', *, *, #61737, .T. ) ;
#86417 = EDGE_LOOP ( 'NONE', ( #54441, #6676, #36294, #18956 ) ) ;
#86418 = ADVANCED_FACE ( 'NONE', ( #35283 ), #97800, .F. ) ;
#86419 = DIRECTION ( 'NONE',  ( 0.9942586961433758086, -0.000000000000000000, 0.1070030146457303932 ) ) ;
#86420 = CARTESIAN_POINT ( 'NONE',  ( 16.59156834624142718, 1513.042027792519093, 197.1096995654986301 ) ) ;
#86421 = LINE ( 'NONE', #41667, #36666 ) ;
#86422 = CARTESIAN_POINT ( 'NONE',  ( -5.004475612664999851, 1517.026025493960105, 216.8437538584669824 ) ) ;
#86423 = CARTESIAN_POINT ( 'NONE',  ( 10.49215165150000040, 1461.076717947590168, 208.4970850545110181 ) ) ;
#86424 = EDGE_CURVE ( 'NONE', #103193, #106306, #51828, .T. ) ;
#86425 = CARTESIAN_POINT ( 'NONE',  ( -18.98057761230930396, 1443.411275185286968, 211.6743897324382147 ) ) ;
#86426 = CARTESIAN_POINT ( 'NONE',  ( -29.97702574129686681, 1379.627454049267953, 213.8718541879157442 ) ) ;
#86427 = FACE_OUTER_BOUND ( 'NONE', #13841, .T. ) ;
#86428 = CARTESIAN_POINT ( 'NONE',  ( 0.8791005338980000250, 1507.105016923229869, 237.2044774393979765 ) ) ;
#86429 = ORIENTED_EDGE ( 'NONE', *, *, #85787, .F. ) ;
#86430 = CARTESIAN_POINT ( 'NONE',  ( -1.136547623115000016, 1516.839862955080207, 206.6438706166370025 ) ) ;
#86431 = VERTEX_POINT ( 'NONE', #53208 ) ;
#86432 = CARTESIAN_POINT ( 'NONE',  ( 22.67290673576669846, 1440.913060387330006, 230.3840297054860002 ) ) ;
#86433 = CARTESIAN_POINT ( 'NONE',  ( -20.30888048250000111, 1509.664622658930057, 230.8524508361979883 ) ) ;
#86434 = ORIENTED_EDGE ( 'NONE', *, *, #25586, .F. ) ;
#86435 = CARTESIAN_POINT ( 'NONE',  ( -7.096089203739619933, 1508.610128855429821, 202.4734964306379936 ) ) ;
#86436 = CARTESIAN_POINT ( 'NONE',  ( -15.37265973589999923, 1410.381991858130050, 190.9834082127980253 ) ) ;
#86437 = FACE_OUTER_BOUND ( 'NONE', #30356, .T. ) ;
#86439 = ORIENTED_EDGE ( 'NONE', *, *, #5732, .T. ) ;
#86438 = CARTESIAN_POINT ( 'NONE',  ( -11.33192160890000011, 1414.988015876730060, 195.9133765198980086 ) ) ;
#86440 = CARTESIAN_POINT ( 'NONE',  ( -6.003588571597879842, 1511.304111283970087, 201.4516922765099878 ) ) ;
#86441 = CARTESIAN_POINT ( 'NONE',  ( -11.93874601188699636, 1433.484590485582430, 147.6230866160556729 ) ) ;
#86442 = EDGE_CURVE ( 'NONE', #84984, #33852, #21421, .T. ) ;
#86443 = DIRECTION ( 'NONE',  ( -0.6736849260863840838, 0.000000000000000000, 0.7390186874254150995 ) ) ;
#86444 = CYLINDRICAL_SURFACE ( 'NONE', #28436, 1.999999999999997335 ) ;
#86446 = CARTESIAN_POINT ( 'NONE',  ( -2.482751378362429762, 1484.258609237499968, 183.2201431065910242 ) ) ;
#86445 = CARTESIAN_POINT ( 'NONE',  ( 22.69876404239850132, 1522.861859112239472, 181.3483716558253036 ) ) ;
#86447 = ADVANCED_FACE ( 'NONE', ( #21077 ), #89384, .T. ) ;
#86448 = CARTESIAN_POINT ( 'NONE',  ( 1.711311228545000063, 1516.591755933730155, 214.8926661113670207 ) ) ;
#86449 = CARTESIAN_POINT ( 'NONE',  ( -2.518237780042220209, 1429.186867776430063, 200.0939789790910197 ) ) ;
#86450 = CARTESIAN_POINT ( 'NONE',  ( 22.90250767448596037, 1409.721554337538237, 209.3445789366613496 ) ) ;
#86451 = CARTESIAN_POINT ( 'NONE',  ( 28.13497766429999913, 1508.084884363030142, 208.3112646548739804 ) ) ;
#86452 = CARTESIAN_POINT ( 'NONE',  ( 6.951175128784999657, 1517.170721208160103, 211.4121022339570004 ) ) ;
#86453 = CARTESIAN_POINT ( 'NONE',  ( -11.86162332674610020, 1482.094478540630007, 208.3237497903899964 ) ) ;
#86454 = CARTESIAN_POINT ( 'NONE',  ( 30.41961987998531569, 1524.374578187333100, 221.8533450253357842 ) ) ;
#86456 = ORIENTED_EDGE ( 'NONE', *, *, #57636, .F. ) ;
#86455 = CARTESIAN_POINT ( 'NONE',  ( -89.65022158889999560, 1384.970293222339933, 308.7482827413589348 ) ) ;
#86457 = CARTESIAN_POINT ( 'NONE',  ( 41.56056515450000433, 1443.484422632850055, 261.5690365361979275 ) ) ;
#86458 = CARTESIAN_POINT ( 'NONE',  ( 10.46269364489999987, 1491.122602117189899, 212.5073291737689942 ) ) ;
#86459 = CARTESIAN_POINT ( 'NONE',  ( -28.36642185875479782, 1509.903637666350050, 216.6464846185489819 ) ) ;
#86460 = CARTESIAN_POINT ( 'NONE',  ( -7.846811853963729710, 1509.181123880980067, 237.0925084584870035 ) ) ;
#86461 = CARTESIAN_POINT ( 'NONE',  ( -20.96815884289999943, 1453.795197786730114, 223.9293672322979774 ) ) ;
#86463 = CARTESIAN_POINT ( 'NONE',  ( 16.91835387501690136, 1409.503862420059932, 222.1480345199989870 ) ) ;
#86462 = CARTESIAN_POINT ( 'NONE',  ( 11.86735446070000144, 1432.439707097380051, 150.3969702326980098 ) ) ;
#86464 = CARTESIAN_POINT ( 'NONE',  ( -9.157365711123761187, 1450.019713085520152, 208.1727642848220228 ) ) ;
#86465 = CARTESIAN_POINT ( 'NONE',  ( -109.2031378463979934, 1382.831926674700071, 310.9887859676099993 ) ) ;
#86466 = VERTEX_POINT ( 'NONE', #4316 ) ;
#86467 = CARTESIAN_POINT ( 'NONE',  ( 4.999456390405000228, 1516.830644417779922, 204.5005780481670001 ) ) ;
#86468 = CARTESIAN_POINT ( 'NONE',  ( 0.3381086166239999358, 1406.067103787530186, 269.0456609344980166 ) ) ;
#86469 = DIRECTION ( 'NONE',  ( 0.5412924984493711067, 0.1391731009598990432, -0.8292365640103210866 ) ) ;
#86470 = CARTESIAN_POINT ( 'NONE',  ( -5.013001780754789585E-06, 1474.175194961529996, 270.1377298905089788 ) ) ;
#86471 = CYLINDRICAL_SURFACE ( 'NONE', #93117, 1.000000000000000888 ) ;
#86472 = CARTESIAN_POINT ( 'NONE',  ( -39.52868828463210349, 1448.959389328290172, 136.3024939181339903 ) ) ;
#86473 = CARTESIAN_POINT ( 'NONE',  ( 4.760896992130000172, 1449.971761959190189, 190.6385172635989704 ) ) ;
#86474 = CARTESIAN_POINT ( 'NONE',  ( -40.91681241450080364, 1440.913060407800003, 260.5474447294020024 ) ) ;
#86475 = CARTESIAN_POINT ( 'NONE',  ( 34.49674184778439923, 1450.393187712189956, 136.2329864103040222 ) ) ;
#86476 = DIRECTION ( 'NONE',  ( 0.000000000000000000, 1.000000000000000000, 0.000000000000000000 ) ) ;
#86477 = CARTESIAN_POINT ( 'NONE',  ( -2.018623677739999955, 1430.846887013590049, 200.9911499127990169 ) ) ;
#86478 = CARTESIAN_POINT ( 'NONE',  ( 8.126234247455000670, 1514.923664147150021, 215.2485921136969864 ) ) ;
#86479 = CARTESIAN_POINT ( 'NONE',  ( -1.049859350909999822, 1507.477610268389981, 221.1890539870990153 ) ) ;
#86480 =( BOUNDED_CURVE ( )  B_SPLINE_CURVE ( 3, ( #95857, #96417, #4561, #64486 ),
 .UNSPECIFIED., .F., .T. ) 
 B_SPLINE_CURVE_WITH_KNOTS ( ( 4, 4 ),
 ( 0.9877503981440959313, 2.153842406702509926 ),
 .UNSPECIFIED. ) 
 CURVE ( )  GEOMETRIC_REPRESENTATION_ITEM ( )  RATIONAL_B_SPLINE_CURVE ( ( 1.000000000000000000, 0.8898596592221782453, 0.8898596592221782453, 1.000000000000000000 ) ) 
 REPRESENTATION_ITEM ( '' )  );
#86481 = CARTESIAN_POINT ( 'NONE',  ( -4.026786250540000722, 1418.591992575429913, 166.2922546441980103 ) ) ;
#86482 = ORIENTED_EDGE ( 'NONE', *, *, #31692, .F. ) ;
#86483 = CARTESIAN_POINT ( 'NONE',  ( 2.541163892419999737, 1448.917481751670039, 182.8661774463979839 ) ) ;
#86484 = CARTESIAN_POINT ( 'NONE',  ( 13.19903007109999926, 1434.900407346980046, 146.9206655066979863 ) ) ;
#86485 = AXIS2_PLACEMENT_3D ( 'NONE', #104320, #19182, #2449 ) ;
#86486 = EDGE_CURVE ( 'NONE', #16730, #54104, #42871, .T. ) ;
#86487 = CARTESIAN_POINT ( 'NONE',  ( 0.2004702986640009843, 1484.367984788590093, 198.3959036849990127 ) ) ;
#86488 = FACE_OUTER_BOUND ( 'NONE', #52024, .T. ) ;
#86489 = CARTESIAN_POINT ( 'NONE',  ( -2.816489208520000235E-09, 1475.837061348030147, 266.9611530681980298 ) ) ;
#86490 = CARTESIAN_POINT ( 'NONE',  ( 11.46077257159999974, 1502.847332571289826, 210.2224670152189958 ) ) ;
#86491 = CARTESIAN_POINT ( 'NONE',  ( -33.93019615848960768, 1522.382868172863937, 197.6607374646000892 ) ) ;
#86492 = CARTESIAN_POINT ( 'NONE',  ( 8.778597385549998577, 1422.758389211139956, 213.4479247216190174 ) ) ;
#86493 = CARTESIAN_POINT ( 'NONE',  ( -17.86631035801030265, 1384.868769857020197, 220.1729067581420054 ) ) ;
#86494 = AXIS2_PLACEMENT_3D ( 'NONE', #105420, #104865, #70208 ) ;
#86495 = CARTESIAN_POINT ( 'NONE',  ( -18.88088134670000073, 1416.274718424630009, 207.7715298601779921 ) ) ;
#86496 = CARTESIAN_POINT ( 'NONE',  ( -6.025150679499999384, 1484.743688571590155, 198.8560548609989951 ) ) ;
#86497 = CARTESIAN_POINT ( 'NONE',  ( 26.81151128603429967, 1435.638944777679853, 136.0785659481259984 ) ) ;
#86498 = CARTESIAN_POINT ( 'NONE',  ( -13.42972542437900252, 1443.473990538164571, 169.3652351402658383 ) ) ;
#86500 = ORIENTED_EDGE ( 'NONE', *, *, #3139, .T. ) ;
#86499 = B_SPLINE_CURVE_WITH_KNOTS ( 'NONE', 3,
 ( #51829, #9266, #43426, #61903, #36126, #20398, #10357, #29358, #97129, #104423, #71968, #38310, #11477, #54603, #19292, #88185 ),
 .UNSPECIFIED., .F., .F.,
 ( 4, 3, 3, 3, 3, 4 ),
 ( -3.958893044225889835, -3.921419384640000061, -3.778841049641950001, -3.535848525436170231, -3.369511780086619890, -3.112795738848540328 ),
 .UNSPECIFIED. ) ;
#86501 = EDGE_CURVE ( 'NONE', #22363, #110093, #93028, .T. ) ;
#86502 = CARTESIAN_POINT ( 'NONE',  ( -16.37287785862759648, 1409.509946165770089, 225.2661112220829693 ) ) ;
#86503 = DIRECTION ( 'NONE',  ( -0.6736849260863841948, 0.000000000000000000, 0.7390186874254148774 ) ) ;
#86504 = ORIENTED_EDGE ( 'NONE', *, *, #97588, .T. ) ;
#86505 = ORIENTED_EDGE ( 'NONE', *, *, #38378, .T. ) ;
#86506 = CARTESIAN_POINT ( 'NONE',  ( 0.6226065275839990365, 1494.171460328590001, 217.4567746792189666 ) ) ;
#86507 = CARTESIAN_POINT ( 'NONE',  ( -14.92639605204266928, 1416.110071989740163, 205.1965795451626775 ) ) ;
#86509 = CARTESIAN_POINT ( 'NONE',  ( 0.6804202724532750768, 1456.809669822820069, 219.7230711736309843 ) ) ;
#86508 = CARTESIAN_POINT ( 'NONE',  ( 10.34843157210000086, 1425.420399904829992, 92.68902548569779754 ) ) ;
#86510 = VECTOR ( 'NONE', #83254, 1000.000000000000114 ) ;
#86511 = CARTESIAN_POINT ( 'NONE',  ( 0.9523195296171770297, 1507.123350973060269, 181.0287246982449858 ) ) ;
#86512 = EDGE_CURVE ( 'NONE', #77650, #87081, #85092, .T. ) ;
#86513 = B_SPLINE_CURVE_WITH_KNOTS ( 'NONE', 5,
 ( #70341, #69216, #1446, #79824, #51860, #60830, #10956, #78144, #71457, #87101, #103326, #43458, #36157, #36702, #19884, #45128, #10388, #27201, #69783, #61937, #54091, #11510, #913, #88216, #61383, #97158, #105573, #63054, #52419, #35591, #53525, #9840, #85996, #104453, #78709, #44559, #96616, #3130, #26633, #95502, #70896, #9295, #45685, #105012, #103901, #52969, #94954, #2022, #44007, #87667, #37260, #77605, #86546, #27745, #96054, #18224, #19324, #79270, #2580, #28301, #62495, #28860, #80367, #89309, #22065, #97707, #81432, #4743, #39458, #74182, #46234, #21522, #107761, #99338, #106649, #5863, #56262, #29389 ),
 .UNSPECIFIED., .F., .F.,
 ( 6, 3, 3, 3, 3, 3, 3, 3, 3, 3, 3, 3, 3, 3, 3, 3, 3, 3, 3, 3, 3, 3, 3, 3, 3, 6 ),
 ( 0.03051383316132079068, 3.902585213099999617, 6.240861926939999194, 6.790072646649998767, 8.377982366400001268, 8.928580102349998882, 10.97133995140000096, 12.98949692180000071, 13.60228008900000063, 15.24737252870000148, 15.86745694640000082, 18.51059426890000026, 22.57641725190000415, 26.75087197450000076, 31.16005629229999840, 33.90953505430000092, 34.60237748540000524, 36.31249047570000243, 36.97255805550000218, 38.99052022429999909, 41.04947707190000017, 41.62972334149999654, 43.19545136810000230, 43.76106149099999953, 46.17824368760000198, 50.04091111600000374 ),
 .UNSPECIFIED. ) ;
#86514 = CARTESIAN_POINT ( 'NONE',  ( 4.146638837207450301, 1424.545683129910230, 184.9058648655890238 ) ) ;
#86515 = CARTESIAN_POINT ( 'NONE',  ( -2.580094527846787056, 1420.665232545646859, 185.6742284517313237 ) ) ;
#86516 = CARTESIAN_POINT ( 'NONE',  ( 7.630837923450000559, 1424.601304396760042, 212.1062089104590029 ) ) ;
#86517 = CARTESIAN_POINT ( 'NONE',  ( -18.47518245119999847, 1466.235720591789914, 200.8822878489689856 ) ) ;
#86518 = CARTESIAN_POINT ( 'NONE',  ( 0.000000000000000000, 1526.382868172863937, 209.1218459616979999 ) ) ;
#86519 = CARTESIAN_POINT ( 'NONE',  ( -105.6049799648840093, 1378.109173369829932, 306.7703173994800068 ) ) ;
#86520 = CARTESIAN_POINT ( 'NONE',  ( 8.916609868645085868, 1365.352032791107831, 207.6218459616988241 ) ) ;
#86522 = EDGE_LOOP ( 'NONE', ( #46721, #22523, #1611, #61983, #108961 ) ) ;
#86521 = CARTESIAN_POINT ( 'NONE',  ( 5.355729600950000169, 1454.568469885690092, 217.0404969026290019 ) ) ;
#86523 = ORIENTED_EDGE ( 'NONE', *, *, #45214, .F. ) ;
#86524 = CARTESIAN_POINT ( 'NONE',  ( 2.500000000000000000, 1440.913060387330006, 209.1218459616979999 ) ) ;
#86525 = CARTESIAN_POINT ( 'NONE',  ( 7.542447022002694013, 1510.549724834208519, 203.3709729786484672 ) ) ;
#86526 = CARTESIAN_POINT ( 'NONE',  ( -0.9912863951520000105, 1474.170141985030114, 270.1376065698979687 ) ) ;
#86527 = CARTESIAN_POINT ( 'NONE',  ( 7.534083176413666649, 1500.276886300912111, 200.5709797116870163 ) ) ;
#86528 = CARTESIAN_POINT ( 'NONE',  ( -1.315440798330000050, 1486.372475699629831, 181.7057967760979977 ) ) ;
#86529 = CARTESIAN_POINT ( 'NONE',  ( -32.13446200735376834, 1525.163457223744444, 201.2154439896625888 ) ) ;
#86530 = EDGE_CURVE ( 'NONE', #43306, #37624, #50423, .T. ) ;
#86531 = CARTESIAN_POINT ( 'NONE',  ( 0.1665620115664219747, 1475.825097533989947, 197.6600777373799929 ) ) ;
#86532 = DIRECTION ( 'NONE',  ( 0.9786619618251657382, 0.000000000000000000, 0.2054769195713184449 ) ) ;
#86533 = CARTESIAN_POINT ( 'NONE',  ( -2.500000000000000000, 1448.240815252059747, 166.0716893801519802 ) ) ;
#86534 = CARTESIAN_POINT ( 'NONE',  ( 8.726849315034220567, 1367.111769039812089, 210.6218459616991936 ) ) ;
#86535 = CARTESIAN_POINT ( 'NONE',  ( 15.58731231540000017, 1409.457381327729991, 212.3362532563479874 ) ) ;
#86536 = CARTESIAN_POINT ( 'NONE',  ( -3.834048154244769968, 1405.884165538340085, 268.4780263706620076 ) ) ;
#86537 = ADVANCED_FACE ( 'NONE', ( #5400 ), #8875, .F. ) ;
#86538 = CARTESIAN_POINT ( 'NONE',  ( -5.343479917770609156, 1396.099658817820000, 199.4684377796870081 ) ) ;
#86539 = VERTEX_POINT ( 'NONE', #7055 ) ;
#86540 = DIRECTION ( 'NONE',  ( 5.980589973904019347E-17, -1.000000000000000000, 1.736889445713099699E-16 ) ) ;
#86541 = CARTESIAN_POINT ( 'NONE',  ( 14.14641573409999964, 1442.793379590060113, 189.5788793805980106 ) ) ;
#86542 = ORIENTED_EDGE ( 'NONE', *, *, #56468, .F. ) ;
#86543 = EDGE_LOOP ( 'NONE', ( #78180, #54883, #87256, #51204 ) ) ;
#86544 = EDGE_CURVE ( 'NONE', #107607, #21616, #75382, .T. ) ;
#86545 = CARTESIAN_POINT ( 'NONE',  ( -4.523943953710000798, 1455.378620544990099, 200.8408221482090141 ) ) ;
#86546 = CARTESIAN_POINT ( 'NONE',  ( 9.454737631249999552, 1363.431170718789872, 207.6218459616989946 ) ) ;
#86547 = CARTESIAN_POINT ( 'NONE',  ( -2.480187054844999572, 1517.025470194390209, 213.7472054950769973 ) ) ;
#86548 = CARTESIAN_POINT ( 'NONE',  ( 2.549111447265000052, 1512.332007210709889, 216.7517165153469989 ) ) ;
#86549 = EDGE_CURVE ( 'NONE', #71414, #108462, #80794, .T. ) ;
#86550 = ORIENTED_EDGE ( 'NONE', *, *, #93352, .T. ) ;
#86551 = CARTESIAN_POINT ( 'NONE',  ( -78.82321741190000353, 1375.585673336139962, 290.9639565911590466 ) ) ;
#86552 = CARTESIAN_POINT ( 'NONE',  ( 12.26359346369999948, 1416.522662137829911, 223.5679345147979973 ) ) ;
#86553 = CARTESIAN_POINT ( 'NONE',  ( -4.038637500854999729, 1516.734985836460055, 203.3481771172569950 ) ) ;
#86554 = CARTESIAN_POINT ( 'NONE',  ( -28.49954575200000306, 1509.595654374630158, 206.6884919356779733 ) ) ;
#86555 = CARTESIAN_POINT ( 'NONE',  ( -1.117992221519999996, 1457.942518689430244, 229.8927423682980020 ) ) ;
#86556 = CARTESIAN_POINT ( 'NONE',  ( -85.86261655710001151, 1384.821806127680020, 289.6800030968590249 ) ) ;
#86557 = CARTESIAN_POINT ( 'NONE',  ( -56.35913123646120226, 1384.651571263749929, 236.4900000120020138 ) ) ;
#86558 = CARTESIAN_POINT ( 'NONE',  ( 9.695068361086670805, 1462.695882120360011, 208.0360144262189976 ) ) ;
#86559 = CARTESIAN_POINT ( 'NONE',  ( -106.7877995600000105, 1387.660326901150029, 310.1072176132589675 ) ) ;
#86561 = ORIENTED_EDGE ( 'NONE', *, *, #31314, .F. ) ;
#86560 = CARTESIAN_POINT ( 'NONE',  ( -12.02002183159999937, 1447.120369466030070, 187.5076504508980122 ) ) ;
#86562 = EDGE_CURVE ( 'NONE', #74812, #53095, #22171, .T. ) ;
#86563 = CARTESIAN_POINT ( 'NONE',  ( 7.330468880873466375, 1514.095142040203882, 201.0173238986526201 ) ) ;
#86564 = CARTESIAN_POINT ( 'NONE',  ( 28.00748489079999715, 1508.132844955729752, 210.8183952993380217 ) ) ;
#86565 = CIRCLE ( 'NONE', #90146, 1.000000000000000888 ) ;
#86566 = FACE_OUTER_BOUND ( 'NONE', #34572, .T. ) ;
#86567 = CARTESIAN_POINT ( 'NONE',  ( -24.67107306660000177, 1435.359038600570102, 135.9357527513979846 ) ) ;
#86568 = EDGE_CURVE ( 'NONE', #71251, #85568, #109120, .T. ) ;
#86569 = CARTESIAN_POINT ( 'NONE',  ( -3.445685115514999897, 1516.778761582560037, 211.6139765934069885 ) ) ;
#86570 = CARTESIAN_POINT ( 'NONE',  ( -68.11985932390000187, 1379.748509173530010, 278.8066904925590279 ) ) ;
#86571 = AXIS2_PLACEMENT_3D ( 'NONE', #40912, #42027, #5675 ) ;
#86572 = CARTESIAN_POINT ( 'NONE',  ( 9.561971226590548767, 1436.616785344690015, 211.5587197113850095 ) ) ;
#86573 = CARTESIAN_POINT ( 'NONE',  ( -29.22959469711409852, 1509.933780326070064, 211.7723416727030212 ) ) ;
#86574 = CARTESIAN_POINT ( 'NONE',  ( -5.221927606092449992, 1489.269388166920180, 185.8916506247110192 ) ) ;
#86575 = CARTESIAN_POINT ( 'NONE',  ( -7.726684725664999753, 1517.208444099459939, 207.9957078235169945 ) ) ;
#86576 = EDGE_CURVE ( 'NONE', #37815, #87917, #71890, .T. ) ;
#86577 = EDGE_LOOP ( 'NONE', ( #93899, #18501, #3255, #108981, #80045 ) ) ;
#86578 = CARTESIAN_POINT ( 'NONE',  ( 2.500000000000000000, 1433.033616087690007, 157.5151964473980115 ) ) ;
#86579 = CARTESIAN_POINT ( 'NONE',  ( 3.313501335607582643, 1397.551704408390151, 215.1871694724064810 ) ) ;
#86580 = CARTESIAN_POINT ( 'NONE',  ( -19.17386968219999943, 1384.864972699589771, 220.5237385319589976 ) ) ;
#86581 = EDGE_LOOP ( 'NONE', ( #37544, #87916, #59576, #102343, #13941 ) ) ;
#86582 = CARTESIAN_POINT ( 'NONE',  ( -3.171072485709999889, 1451.871858332230204, 182.7750508701979868 ) ) ;
#86583 = CARTESIAN_POINT ( 'NONE',  ( -3.531493108469999864, 1429.908133670090137, 201.5805818289689739 ) ) ;
#86584 = CARTESIAN_POINT ( 'NONE',  ( 11.69975092292400021, 1434.958819240250023, 151.3101301185499779 ) ) ;
#86585 = B_SPLINE_SURFACE_WITH_KNOTS ( 'NONE', 5, 1, ( 
 ( #94152, #85756 ),
 ( #51074, #677 ),
 ( #18535, #134 ),
 ( #70108, #85201 ),
 ( #104221, #68995 ),
 ( #103096, #34255 ) ),
 .UNSPECIFIED., .F., .F., .F.,
 ( 6, 6 ),
 ( 2, 2 ),
 ( -3.220373955451920388E-05, 18.01490009493960187 ),
 ( 0.000000000000000000, 14.00003220373960033 ),
 .UNSPECIFIED. ) ;
#86586 = CARTESIAN_POINT ( 'NONE',  ( 17.89184398620259842, 1478.710743812830060, 229.0921243387979871 ) ) ;
#86587 = CARTESIAN_POINT ( 'NONE',  ( -24.34268787264259970, 1442.549328851149994, 212.2035684885649687 ) ) ;
#86588 = CARTESIAN_POINT ( 'NONE',  ( -2.196220669999999764, 1409.923853725629897, 186.4038509670979806 ) ) ;
#86589 = CARTESIAN_POINT ( 'NONE',  ( 12.67630892740000093, 1426.478874823920023, 202.7079035067189920 ) ) ;
#86590 = CARTESIAN_POINT ( 'NONE',  ( -0.1500423873502870209, 1420.467040554029836, 182.7481543114539875 ) ) ;
#86592 = DIRECTION ( 'NONE',  ( -0.9455185755993178454, 0.000000000000000000, 0.3255681544571539243 ) ) ;
#86591 = CARTESIAN_POINT ( 'NONE',  ( 3.457266605394999637, 1516.691414181030041, 214.8945738789770132 ) ) ;
#86593 = CARTESIAN_POINT ( 'NONE',  ( -8.871221972256710941, 1385.201631638590015, 218.6720694474429934 ) ) ;
#86594 = CARTESIAN_POINT ( 'NONE',  ( 18.52345746076924016, 1425.819856484418779, 224.6762942409735899 ) ) ;
#86595 = ORIENTED_EDGE ( 'NONE', *, *, #66480, .T. ) ;
#86596 = CARTESIAN_POINT ( 'NONE',  ( -11.01105141468870130, 1414.913060387399810, 197.2110468686490208 ) ) ;
#86597 = DIRECTION ( 'NONE',  ( -0.9996573249755517088, -0.02617694830808747070, 0.000000000000000000 ) ) ;
#86598 = ORIENTED_EDGE ( 'NONE', *, *, #95268, .T. ) ;
#86599 = CARTESIAN_POINT ( 'NONE',  ( 3.462763369819999770, 1420.996806472229991, 185.1667669751979872 ) ) ;
#86600 = CARTESIAN_POINT ( 'NONE',  ( -121.3977480003905782, 1384.926148861439970, 304.3966123716357401 ) ) ;
#86601 = CARTESIAN_POINT ( 'NONE',  ( 8.473110443205881026, 1511.778877376279979, 203.0322686476939964 ) ) ;
#86602 = CARTESIAN_POINT ( 'NONE',  ( 2.973593887119999835, 1441.553271505090152, 218.1843342212790162 ) ) ;
#86603 = DIRECTION ( 'NONE',  ( 3.828568698926945984E-16, 0.000000000000000000, -1.000000000000000000 ) ) ;
#86604 = DIRECTION ( 'NONE',  ( 5.525335831609270812E-11, 0.9712045719081587869, 0.2382470975787324696 ) ) ;
#86605 = CARTESIAN_POINT ( 'NONE',  ( -3.692944113110000259, 1446.771170833259930, 157.7765974131980045 ) ) ;
#86606 = CARTESIAN_POINT ( 'NONE',  ( -18.06991754140000239, 1424.836194406330151, 226.5046235209979955 ) ) ;
#86607 = CARTESIAN_POINT ( 'NONE',  ( -9.078760040516870689, 1459.398684262878078, 212.3905513612093046 ) ) ;
#86608 = CARTESIAN_POINT ( 'NONE',  ( 16.71292568740000206, 1489.452917662229993, 194.5586640803979890 ) ) ;
#86609 = CARTESIAN_POINT ( 'NONE',  ( 17.94562356750000021, 1438.546729650309999, 191.2321735587979958 ) ) ;
#86611 = DIRECTION ( 'NONE',  ( 5.980589973904019347E-17, -1.000000000000000000, 1.736889445713099699E-16 ) ) ;
#86610 = CARTESIAN_POINT ( 'NONE',  ( -13.87318377641789979, 1417.128397284559924, 202.3536462288429902 ) ) ;
#86612 = CARTESIAN_POINT ( 'NONE',  ( 10.92532341640084326, 1429.179526204826971, 151.1050430757466074 ) ) ;
#86613 = VERTEX_POINT ( 'NONE', #65333 ) ;
#86614 = CARTESIAN_POINT ( 'NONE',  ( 1.278193956753560068, 1507.616839952949931, 186.1818873165319985 ) ) ;
#86615 = CARTESIAN_POINT ( 'NONE',  ( 26.89254719910000091, 1508.005806001830024, 206.4982022804780115 ) ) ;
#86616 = CARTESIAN_POINT ( 'NONE',  ( -23.96906971290000143, 1437.223344794849936, 211.5767061028579974 ) ) ;
#86617 = CARTESIAN_POINT ( 'NONE',  ( 8.887359343084140662, 1425.078831941400040, 195.6980871684259853 ) ) ;
#86618 = CARTESIAN_POINT ( 'NONE',  ( -3.828803044467389949, 1426.014514409073172, 186.0276948169274931 ) ) ;
#86619 = B_SPLINE_SURFACE_WITH_KNOTS ( 'NONE', 5, 5, ( 
 ( #49133, #13282, #14938, #99493, #40159, #64843 ),
 ( #6561, #40712, #32847, #83813, #74342, #58629 ),
 ( #109034, #81596, #67039, #56425, #56982, #74884 ),
 ( #108469, #66500, #47473, #109577, #73785, #4900 ),
 ( #100605, #23887, #15486, #31753, #49684, #41267 ),
 ( #75441, #90555, #13835, #48020, #82157, #31205 ),
 ( #78167, #60282, #102261, #24987, #26655, #50767 ),
 ( #51311, #67588, #34513, #17122, #85448, #102796 ),
 ( #25541, #60854, #101695, #59731, #93851, #26093 ),
 ( #1480, #8746, #92760, #42929, #69807, #68691 ),
 ( #50238, #94402, #33958, #103925, #68153, #939 ),
 ( #17680, #59191, #84902, #93311, #9863, #395 ),
 ( #8194, #77086, #44031, #16571, #42360, #35063 ),
 ( #18247, #51884, #86020, #16038, #9320, #43484 ),
 ( #33392, #103353, #77627, #69244, #35612, #52442 ),
 ( #27224, #84366, #94979, #7655, #41811, #75968 ),
 ( #86570, #110120, #76515, #110665, #72545, #46807 ),
 ( #80937, #72021, #97178, #71479, #63614, #105038 ),
 ( #28328, #45707, #54112, #89333, #106676, #96642 ),
 ( #44587, #54660, #4235, #53551, #61962, #78732 ),
 ( #10978, #29414, #45152, #38369, #63079, #106137 ),
 ( #28883, #97730, #36727, #37287, #61404, #96076 ),
 ( #52994, #95526, #27770, #18798, #20451, #87127 ),
 ( #12630, #21001, #104477, #79845, #88240, #62520 ),
 ( #88789, #19351, #10417, #87698, #12070, #79292 ),
 ( #2602, #55205, #105600, #70922, #19911, #11532 ),
 ( #70363, #2047, #46262, #36180, #3154, #80391 ),
 ( #3705, #37835, #22091, #89879, #47334, #7397 ),
 ( #33140, #24718, #21551, #109863, #42110, #29966 ),
 ( #56290, #98832, #30524, #16863, #65254, #64159 ),
 ( #8483, #41562, #33685, #98277, #67329, #82022 ),
 ( #55763, #24176, #16319, #75717, #73094, #90418 ),
 ( #59476, #49960, #50520, #13698, #31073, #93586 ),
 ( #107233, #84644, #7941, #67880, #101426, #58915 ),
 ( #93046, #5326, #58364, #81462, #76257, #110406 ),
 ( #51066, #101989, #99366, #42657, #76811, #25275 ),
 ( #85196, #13149, #84096, #4768, #38911, #64715 ),
 ( #47884, #15759, #39486, #73657, #107788, #92490 ),
 ( #61689, #86308, #102535, #2339, #68989, #10717 ),
 ( #103090, #18528, #1781, #36451, #104767, #86859 ),
 ( #17417, #9046, #87986, #77369, #43762, #19646 ),
 ( #44888, #19078, #95811, #52724, #45436, #10151 ),
 ( #11274, #79038, #9591, #70649, #85750, #77914 ),
 ( #44324, #70101, #51615, #25827, #28051, #62241 ),
 ( #43220, #26390, #60028, #78468, #53282, #94146 ),
 ( #670, #103663, #87421, #35918, #34801, #60585 ),
 ( #96367, #104214, #53849, #94705, #1220, #127 ),
 ( #17981, #34250, #68433, #52176, #27501, #35355 ) ),
 .UNSPECIFIED., .F., .F., .F.,
 ( 6, 3, 3, 3, 3, 3, 3, 3, 3, 3, 3, 3, 3, 3, 3, 6 ),
 ( 6, 6 ),
 ( 182.2335547110000107, 182.4224514059999933, 182.6488836039999910, 182.8753158020000171, 183.5360872660000098, 184.5201209679999863, 185.9951582379999877, 188.2072972830000026, 191.5252565730000072, 196.5020170729999904, 209.5656953139999814, 231.9595200839999904, 250.6438719679999849, 278.7167119989999833, 297.4396013979999793, 313.5600086899999610 ),
 ( 0.000000000000000000, 0.5000000000000000000 ),
 .UNSPECIFIED. ) ;
#86620 = CARTESIAN_POINT ( 'NONE',  ( -9.845241469799999479, 1507.507259092430104, 182.3675330799979974 ) ) ;
#86621 = DIRECTION ( 'NONE',  ( 1.000000000000000000, 0.000000000000000000, 0.000000000000000000 ) ) ;
#86622 = CARTESIAN_POINT ( 'NONE',  ( 2.586839709529719755, 1508.551704408389924, 219.5247725683019837 ) ) ;
#86623 = CARTESIAN_POINT ( 'NONE',  ( 12.98226561589999939, 1414.913060387329779, 198.3280246956980193 ) ) ;
#86624 = CARTESIAN_POINT ( 'NONE',  ( -88.09424512964220355, 1383.771532610089935, 307.8360115022359764 ) ) ;
#86625 = FACE_OUTER_BOUND ( 'NONE', #6458, .T. ) ;
#86626 = CARTESIAN_POINT ( 'NONE',  ( -15.27152961130000008, 1506.433683729329914, 224.9338604266980326 ) ) ;
#86627 = DIRECTION ( 'NONE',  ( 0.7628756747269003213, -0.04363816414198476434, 0.6450708608674661226 ) ) ;
#86629 = VERTEX_POINT ( 'NONE', #108971 ) ;
#86628 = DIRECTION ( 'NONE',  ( -1.699538841806929935E-33, 1.000000000000000000, -1.698192320643030073E-16 ) ) ;
#86630 = CARTESIAN_POINT ( 'NONE',  ( -1.527505831896529997, 1414.913527275050001, 226.2323514033340075 ) ) ;
#86631 = CARTESIAN_POINT ( 'NONE',  ( -60.95159128010000416, 1380.984161914990182, 278.9881612236590058 ) ) ;
#86632 = CARTESIAN_POINT ( 'NONE',  ( 19.87374343083660122, 1508.662439912400032, 229.4870358833140074 ) ) ;
#86633 = ORIENTED_EDGE ( 'NONE', *, *, #12608, .F. ) ;
#86634 = ORIENTED_EDGE ( 'NONE', *, *, #99663, .F. ) ;
#86635 = CARTESIAN_POINT ( 'NONE',  ( 14.14641573409999964, 1442.793379590060113, 189.5788793805980106 ) ) ;
#86636 = LINE ( 'NONE', #103423, #77868 ) ;
#86637 = CARTESIAN_POINT ( 'NONE',  ( 37.57758922502669918, 1438.291453973320131, 136.5834610766669925 ) ) ;
#86639 = CARTESIAN_POINT ( 'NONE',  ( -45.31147984109999527, 1446.488572564270044, 266.2043212162980126 ) ) ;
#86638 = CARTESIAN_POINT ( 'NONE',  ( 21.99590692650000179, 1506.811133726529988, 208.7395957790290026 ) ) ;
#86640 = AXIS2_PLACEMENT_3D ( 'NONE', #62935, #104331, #54513 ) ;
#86641 = CARTESIAN_POINT ( 'NONE',  ( 8.629414813098978954, 1437.378993763129984, 209.7946259206210016 ) ) ;
#86642 = CARTESIAN_POINT ( 'NONE',  ( -109.8920056810000005, 1383.809063189439939, 297.0622304906589761 ) ) ;
#86643 = CARTESIAN_POINT ( 'NONE',  ( -12.82978874381982770, 1435.930450547085684, 150.8169046549416237 ) ) ;
#86644 = DIRECTION ( 'NONE',  ( 0.01243399051534999945, -0.9999091450434870465, -0.005205529585659179545 ) ) ;
#86645 = CARTESIAN_POINT ( 'NONE',  ( 2.669285241919999940, 1410.384145046430149, 185.6213876249979933 ) ) ;
#86646 = CARTESIAN_POINT ( 'NONE',  ( 4.902927094849999889, 1424.294896435129886, 185.5048746948980067 ) ) ;
#86648 = CARTESIAN_POINT ( 'NONE',  ( -12.48849034979999928, 1435.526019791340104, 150.8975384341979975 ) ) ;
#86647 = CIRCLE ( 'NONE', #100936, 0.4999999999999995559 ) ;
#86649 = CARTESIAN_POINT ( 'NONE',  ( 7.785771676495370386, 1435.464459252629922, 205.4398922123320119 ) ) ;
#86650 = FACE_OUTER_BOUND ( 'NONE', #97785, .T. ) ;
#86651 = CARTESIAN_POINT ( 'NONE',  ( -3.063989819839999740, 1452.806063505229986, 152.9802899940980296 ) ) ;
#86652 = DIRECTION ( 'NONE',  ( 0.8672669759446700599, -0.000000000000000000, 0.4978433412588614271 ) ) ;
#86653 = ORIENTED_EDGE ( 'NONE', *, *, #1011, .T. ) ;
#86654 = CARTESIAN_POINT ( 'NONE',  ( -26.35475552313950232, 1507.985742420310089, 201.5462045797129917 ) ) ;
#86655 =( BOUNDED_CURVE ( )  B_SPLINE_CURVE ( 3, ( #99278, #91998, #22554, #49465 ),
 .UNSPECIFIED., .F., .F. ) 
 B_SPLINE_CURVE_WITH_KNOTS ( ( 4, 4 ),
 ( 5.499719231641273964, 7.069826864254338261 ),
 .UNSPECIFIED. ) 
 CURVE ( )  GEOMETRIC_REPRESENTATION_ITEM ( )  RATIONAL_B_SPLINE_CURVE ( ( 1.000000000000000000, 0.8049001529481599748, 0.8049001529481599748, 1.000000000000000000 ) ) 
 REPRESENTATION_ITEM ( '' )  );
#86656 = CARTESIAN_POINT ( 'NONE',  ( -13.40940820319999993, 1470.117754583789974, 192.0205833154989818 ) ) ;
#86657 = CARTESIAN_POINT ( 'NONE',  ( -43.08606230889999722, 1445.624833271280295, 270.3368636273980314 ) ) ;
#86658 = CARTESIAN_POINT ( 'NONE',  ( -12.27010794651660497, 1416.835807151113613, 194.6641343636595138 ) ) ;
#86659 = CARTESIAN_POINT ( 'NONE',  ( 6.692947047070000544, 1442.760174925260117, 154.8612665581980252 ) ) ;
#86660 = DIRECTION ( 'NONE',  ( -1.755985294532469921E-16, 1.000000000000000000, -1.338183447452831989E-16 ) ) ;
#86661 = DIRECTION ( 'NONE',  ( 0.9942586961433756976, 0.000000000000000000, 0.1070030146457303794 ) ) ;
#86662 = EDGE_CURVE ( 'NONE', #28587, #36324, #32156, .T. ) ;
#86663 = CARTESIAN_POINT ( 'NONE',  ( 2.865137034695680374, 1409.233255452639924, 230.9592206399570102 ) ) ;
#86664 = DIRECTION ( 'NONE',  ( 0.000000000000000000, 1.000000000000000000, 0.000000000000000000 ) ) ;
#86665 = CARTESIAN_POINT ( 'NONE',  ( -4.309299583070000494, 1417.803906166430124, 233.7804493454979990 ) ) ;
#86666 = CARTESIAN_POINT ( 'NONE',  ( 4.026786250540000722, 1432.413060387330006, 146.1721969590979882 ) ) ;
#86667 = CARTESIAN_POINT ( 'NONE',  ( -7.673282386996102211, 1360.664745917332993, 210.6218459617030021 ) ) ;
#86668 = CARTESIAN_POINT ( 'NONE',  ( -46.22591519347989930, 1439.214963125549957, 267.5912708118539740 ) ) ;
#86669 = CARTESIAN_POINT ( 'NONE',  ( -2.500000000000000000, 1418.913060387330006, 172.2701767054979882 ) ) ;
#86670 = VERTEX_POINT ( 'NONE', #23833 ) ;
#86671 = CARTESIAN_POINT ( 'NONE',  ( -8.364654381539999406, 1423.448482863899926, 210.5916039729090130 ) ) ;
#86672 = ORIENTED_EDGE ( 'NONE', *, *, #60271, .T. ) ;
#86673 = CARTESIAN_POINT ( 'NONE',  ( 6.562094069294999166, 1517.122674412569950, 209.8604508749069737 ) ) ;
#86674 = DIRECTION ( 'NONE',  ( -1.836970198721029688E-16, -1.000000000000000000, 0.000000000000000000 ) ) ;
#86675 = CARTESIAN_POINT ( 'NONE',  ( 19.30779799461502932, 1456.580107245917134, 224.6839345049536121 ) ) ;
#86676 = CARTESIAN_POINT ( 'NONE',  ( 7.539467915018410515, 1425.654756675969793, 212.1861668026819814 ) ) ;
#86677 = B_SPLINE_CURVE_WITH_KNOTS ( 'NONE', 3,
 ( #98617, #107024, #22999, #73987, #81809, #74545 ),
 .UNSPECIFIED., .F., .F.,
 ( 4, 2, 4 ),
 ( -1.131363979615173359E-05, 0.001067788114096062746, 0.002146889867988277523 ),
 .UNSPECIFIED. ) ;
#86678 = CARTESIAN_POINT ( 'NONE',  ( -0.2833403650370509563, 1496.275355223149973, 221.4684270307890017 ) ) ;
#86679 = ORIENTED_EDGE ( 'NONE', *, *, #31652, .T. ) ;
#86680 = EDGE_CURVE ( 'NONE', #63865, #48606, #91845, .T. ) ;
#86681 = CARTESIAN_POINT ( 'NONE',  ( -15.16694981760000083, 1488.813684182929819, 194.2846367734980220 ) ) ;
#86683 = DIRECTION ( 'NONE',  ( -0.4090087482554183862, 0.000000000000000000, 0.9125304618754026542 ) ) ;
#86682 = CARTESIAN_POINT ( 'NONE',  ( -2.038646110889526852, 1525.960063244517187, 177.0579350083066856 ) ) ;
#86684 = CIRCLE ( 'NONE', #36656, 0.4999999999999996114 ) ;
#86685 =( BOUNDED_CURVE ( )  B_SPLINE_CURVE ( 3, ( #97175, #79288, #36723, #20448 ),
 .UNSPECIFIED., .F., .T. ) 
 B_SPLINE_CURVE_WITH_KNOTS ( ( 4, 4 ),
 ( 4.149166158125050075, 5.275619312941369543 ),
 .UNSPECIFIED. ) 
 CURVE ( )  GEOMETRIC_REPRESENTATION_ITEM ( )  RATIONAL_B_SPLINE_CURVE ( ( 1.000000000000000000, 0.8970245268685778095, 0.8970245268685778095, 1.000000000000000000 ) ) 
 REPRESENTATION_ITEM ( '' )  );
#86686 = CARTESIAN_POINT ( 'NONE',  ( 7.717505752974999744, 1516.857914730730045, 201.4043401791270185 ) ) ;
#86687 = CARTESIAN_POINT ( 'NONE',  ( -18.60629936281669927, 1508.494392593700013, 210.7647685123470183 ) ) ;
#86688 = CARTESIAN_POINT ( 'NONE',  ( 4.780307568339999591, 1467.625956517089890, 217.8721402715589761 ) ) ;
#86689 = CARTESIAN_POINT ( 'NONE',  ( -8.697277070075241312, 1440.006333808949876, 206.1599688172080107 ) ) ;
#86690 = VERTEX_POINT ( 'NONE', #77029 ) ;
#86691 = CARTESIAN_POINT ( 'NONE',  ( -4.798351648711870254, 1410.228040598270127, 269.8672392053869658 ) ) ;
#86692 = CARTESIAN_POINT ( 'NONE',  ( -6.563915562015000482, 1517.184063036290127, 207.9975562766469750 ) ) ;
#86693 = CARTESIAN_POINT ( 'NONE',  ( 6.381981878911410000, 1416.920506164580047, 231.2616950943009897 ) ) ;
#86694 = DIRECTION ( 'NONE',  ( -6.498030146439999846E-14, -1.000000000000000000, -7.271071663860000024E-13 ) ) ;
#86696 = ORIENTED_EDGE ( 'NONE', *, *, #102147, .F. ) ;
#86695 = CARTESIAN_POINT ( 'NONE',  ( -4.921072290514207026, 1367.614687051687270, 210.6218459617142003 ) ) ;
#86697 = EDGE_LOOP ( 'NONE', ( #11065, #93559, #108876, #53658 ) ) ;
#86698 = FACE_OUTER_BOUND ( 'NONE', #108525, .T. ) ;
#86699 = CARTESIAN_POINT ( 'NONE',  ( -4.400277592110000136, 1425.922606744830091, 186.1626553210980148 ) ) ;
#86700 = CARTESIAN_POINT ( 'NONE',  ( 3.627844022310690697, 1424.520533308087352, 184.5083861543649277 ) ) ;
#86701 = CARTESIAN_POINT ( 'NONE',  ( -0.01068885454432250137, 1408.933329768819704, 186.2235385012060078 ) ) ;
#86702 = ADVANCED_FACE ( 'NONE', ( #42308 ), #58575, .T. ) ;
#86703 = CARTESIAN_POINT ( 'NONE',  ( -20.08296050208739914, 1477.456190548399945, 193.1386059401030195 ) ) ;
#86704 = CARTESIAN_POINT ( 'NONE',  ( -18.89960126629999948, 1420.835424610929977, 224.0556394152980033 ) ) ;
#86705 = ORIENTED_EDGE ( 'NONE', *, *, #100921, .T. ) ;
#86706 = CARTESIAN_POINT ( 'NONE',  ( 39.30292780399409480, 1459.546458005919931, 267.2018548829190081 ) ) ;
#86707 = CARTESIAN_POINT ( 'NONE',  ( -5.924191439393101000, 1466.159508804048073, 234.1209534312763481 ) ) ;
#86708 = CARTESIAN_POINT ( 'NONE',  ( 8.813431017979999282, 1446.116337443820157, 185.6059072443980256 ) ) ;
#86709 = CARTESIAN_POINT ( 'NONE',  ( -5.011367984924999242, 1516.974592746400049, 205.6720686163770324 ) ) ;
#86710 = EDGE_CURVE ( 'NONE', #96052, #49801, #86499, .T. ) ;
#86711 = VERTEX_POINT ( 'NONE', #27170 ) ;
#86712 = CARTESIAN_POINT ( 'NONE',  ( 2.473110443770000000, 1437.362874199289763, 227.5249784694989899 ) ) ;
#86713 = CARTESIAN_POINT ( 'NONE',  ( 1.479066938756839811, 1478.749526688280184, 182.3503021183099975 ) ) ;
#86714 = CARTESIAN_POINT ( 'NONE',  ( 22.77629783569999944, 1409.717017837230060, 208.7225517380699955 ) ) ;
#86715 = EDGE_LOOP ( 'NONE', ( #70256, #48645, #80854 ) ) ;
#86716 = CARTESIAN_POINT ( 'NONE',  ( 4.058188250227919625, 1508.551704408389924, 204.4428604963009946 ) ) ;
#86717 = CARTESIAN_POINT ( 'NONE',  ( 26.22604730430230191, 1450.757778662670034, 136.6085202351380019 ) ) ;
#86718 = CARTESIAN_POINT ( 'NONE',  ( -113.4000000000000057, 1390.939237335599955, 304.2218459572590064 ) ) ;
#86719 = CARTESIAN_POINT ( 'NONE',  ( -17.53487789670000296, 1386.947750201170038, 219.7453638570590044 ) ) ;
#86720 = DIRECTION ( 'NONE',  ( 0.9455185755993178454, 0.000000000000000000, -0.3255681544571539243 ) ) ;
#86722 = B_SPLINE_SURFACE_WITH_KNOTS ( 'NONE', 2, 1, ( 
 ( #85886, #104905 ),
 ( #69115, #43351 ),
 ( #77499, #34928 ),
 ( #28193, #102657 ),
 ( #1918, #19785 ) ),
 .UNSPECIFIED., .F., .F., .F.,
 ( 3, 2, 3 ),
 ( 2, 2 ),
 ( 0.000000000000000000, 0.5000000000000000000, 1.000000000000000000 ),
 ( 0.000000000000000000, 1.000000000000000000 ),
 .UNSPECIFIED. ) ;
#86721 = CARTESIAN_POINT ( 'NONE',  ( 18.21434415869999768, 1409.713951146429963, 194.9538956094980335 ) ) ;
#86723 = CARTESIAN_POINT ( 'NONE',  ( 27.95977047539996718, 1444.740067931808653, 175.9996750486979238 ) ) ;
#86724 = AXIS2_PLACEMENT_3D ( 'NONE', #96899, #78443, #88495 ) ;
#86725 = CARTESIAN_POINT ( 'NONE',  ( 3.089875597163601828, 1439.679630760519331, 184.1893751638651509 ) ) ;
#86727 = CARTESIAN_POINT ( 'NONE',  ( -21.48378771895310990, 1429.065913162214201, 219.3372196911616356 ) ) ;
#86726 = CARTESIAN_POINT ( 'NONE',  ( -32.02808312589930040, 1512.187213306747481, 198.2787714533499752 ) ) ;
#86728 = CARTESIAN_POINT ( 'NONE',  ( 1.167028762698379962, 1450.781002157910052, 181.8366260879649872 ) ) ;
#86729 = CARTESIAN_POINT ( 'NONE',  ( -15.84432591830269743, 1419.853212859319910, 210.7451195136700051 ) ) ;
#86730 = CARTESIAN_POINT ( 'NONE',  ( -8.578849961799997814, 1381.727047392470013, 218.1308605599590180 ) ) ;
#86731 = CARTESIAN_POINT ( 'NONE',  ( 4.621897824414999967, 1516.858533673840157, 213.7337256555570093 ) ) ;
#86732 = AXIS2_PLACEMENT_3D ( 'NONE', #109756, #108092, #41459 ) ;
#86733 = CARTESIAN_POINT ( 'NONE',  ( 2.038646110889527296, 1525.960063244517187, 241.1857569150893141 ) ) ;
#86734 = ORIENTED_EDGE ( 'NONE', *, *, #13053, .T. ) ;
#86735 = CARTESIAN_POINT ( 'NONE',  ( -12.68810582867495640, 1464.870331481658241, 224.6384026358888377 ) ) ;
#86736 = CARTESIAN_POINT ( 'NONE',  ( 21.86721050905302377, 1523.611961620354123, 235.0400593884480713 ) ) ;
#86737 = CARTESIAN_POINT ( 'NONE',  ( -0.2964179489810150336, 1408.950247830049875, 232.0370909886389938 ) ) ;
#86738 = DIRECTION ( 'NONE',  ( 0.000000000000000000, 0.000000000000000000, -1.000000000000000000 ) ) ;
#86739 = CARTESIAN_POINT ( 'NONE',  ( 0.1794159432210164773, 1421.105753184904643, 193.7169311276417716 ) ) ;
#86740 = CARTESIAN_POINT ( 'NONE',  ( -4.328907235665659492, 1515.085473475149911, 207.8086220615720094 ) ) ;
#86741 = CARTESIAN_POINT ( 'NONE',  ( 1.332267629549999902E-15, 1453.913060387330006, 209.1218459616979999 ) ) ;
#86742 = DIRECTION ( 'NONE',  ( 1.755985294532469921E-16, -1.000000000000000000, 1.338183447452831989E-16 ) ) ;
#86743 = CARTESIAN_POINT ( 'NONE',  ( 11.89240926010000088, 1433.292849282470115, 150.1795062545980102 ) ) ;
#86744 = CARTESIAN_POINT ( 'NONE',  ( 23.42675388609999843, 1440.913060387330006, 234.3916895593979746 ) ) ;
#86745 = B_SPLINE_SURFACE_WITH_KNOTS ( 'NONE', 5, 5, ( 
 ( #74891, #109042, #57548, #75448, #91671, #14945 ),
 ( #109584, #67047, #7662, #83273, #101154, #6570 ),
 ( #32325, #66507, #58636, #92682, #83736, #75894 ),
 ( #14865, #32237, #58004, #47939, #57464, #74262 ),
 ( #108947, #24368, #49057, #49604, #23268, #91590 ),
 ( #40633, #83193, #41735, #91027, #93235, #6481 ),
 ( #73712, #23813, #65855, #32777, #92140, #110046 ),
 ( #22697, #107836, #65307, #7580, #74804, #33318 ),
 ( #7031, #100533, #58554, #5936, #67515, #15413 ) ),
 .UNSPECIFIED., .F., .F., .F.,
 ( 6, 3, 6 ),
 ( 6, 6 ),
 ( 2.948979317598059868, 5.061843608070000222, 7.174698196173030063 ),
 ( -0.0004176450428783939949, 2.000000000000000000 ),
 .UNSPECIFIED. ) ;
#86746 = B_SPLINE_CURVE_WITH_KNOTS ( 'NONE', 3,
 ( #29954, #37273, #80925, #20438, #72008, #53537 ),
 .UNSPECIFIED., .F., .F.,
 ( 4, 2, 4 ),
 ( 1.040834085586084257E-17, 0.001087661325621716189, 0.002175322651243421970 ),
 .UNSPECIFIED. ) ;
#86747 = CARTESIAN_POINT ( 'NONE',  ( 26.10499783855849998, 1440.913060396819901, 222.4284486497450075 ) ) ;
#86748 = CARTESIAN_POINT ( 'NONE',  ( -17.25816047809999887, 1421.803897450879958, 201.8596040855890124 ) ) ;
#86749 = CARTESIAN_POINT ( 'NONE',  ( 7.628773549489999972, 1416.913060387330006, 201.4930723711279938 ) ) ;
#86750 = CARTESIAN_POINT ( 'NONE',  ( 22.11554775090000291, 1489.452917662729988, 210.6419443847580055 ) ) ;
#86751 = CARTESIAN_POINT ( 'NONE',  ( -12.11110426309999966, 1485.984702322530211, 184.7620324990980123 ) ) ;
#86752 = DIRECTION ( 'NONE',  ( 1.755985294532469921E-16, -1.000000000000000000, 1.338183447452831989E-16 ) ) ;
#86753 = CARTESIAN_POINT ( 'NONE',  ( -25.60272812314580193, 1509.807125272330040, 193.2161752248550215 ) ) ;
#86754 = B_SPLINE_CURVE_WITH_KNOTS ( 'NONE', 5,
 ( #98195, #74673, #89798, #5244, #73576, #108251, #64628, #107707, #40495 ),
 .UNSPECIFIED., .F., .F.,
 ( 6, 3, 6 ),
 ( -133.6064266969999892, -37.05188947199999916, -29.74344005870001695 ),
 .UNSPECIFIED. ) ;
#86755 = CARTESIAN_POINT ( 'NONE',  ( 25.79285008279999758, 1449.806912616609907, 209.2669309290440083 ) ) ;
#86756 = CARTESIAN_POINT ( 'NONE',  ( 32.30068554584615725, 1526.382868172863937, 220.2363794648143198 ) ) ;
#86757 = CARTESIAN_POINT ( 'NONE',  ( 25.08533235215197621, 1436.600044169495050, 137.7642755019057859 ) ) ;
#86758 = CARTESIAN_POINT ( 'NONE',  ( -9.878584958427840235, 1383.863156290969982, 218.5760999266929900 ) ) ;
#86759 = AXIS2_PLACEMENT_3D ( 'NONE', #74383, #82757, #23929 ) ;
#86760 = CARTESIAN_POINT ( 'NONE',  ( 8.129468112789759004, 1461.711575812669935, 228.8738014183659857 ) ) ;
#86761 = CARTESIAN_POINT ( 'NONE',  ( 4.621897824414999967, 1516.858533673840157, 213.7337256555570093 ) ) ;
#86762 = CARTESIAN_POINT ( 'NONE',  ( 9.178714075745430634, 1450.974408660679956, 210.2178452082900151 ) ) ;
#86764 = ORIENTED_EDGE ( 'NONE', *, *, #50933, .T. ) ;
#86763 = CARTESIAN_POINT ( 'NONE',  ( 3.181164613930000051, 1442.605935617189971, 217.4126579123289957 ) ) ;
#86765 = CARTESIAN_POINT ( 'NONE',  ( 16.06428792994640276, 1414.913060387329779, 208.9262477894010033 ) ) ;
#86766 = CARTESIAN_POINT ( 'NONE',  ( -4.273368017822010083E-16, 1381.377992659140091, 201.0499806489090133 ) ) ;
#86767 = CARTESIAN_POINT ( 'NONE',  ( -5.429027349949509862, 1440.820888839999952, 154.8047238236129886 ) ) ;
#86769 = ORIENTED_EDGE ( 'NONE', *, *, #97876, .T. ) ;
#86768 = CARTESIAN_POINT ( 'NONE',  ( -36.53452253901330238, 1451.194196174219996, 134.0999999986999853 ) ) ;
#86770 = CARTESIAN_POINT ( 'NONE',  ( -17.65533568451049717, 1419.497303018139974, 207.2321751882169849 ) ) ;
#86771 = EDGE_LOOP ( 'NONE', ( #15663, #60572, #86634, #66632, #88798, #106796, #52576 ) ) ;
#86772 = AXIS2_PLACEMENT_3D ( 'NONE', #51567, #75671, #85149 ) ;
#86773 = DIRECTION ( 'NONE',  ( -0.7071067811865475727, -6.078560574715863648E-17, 0.7071067811865475727 ) ) ;
#86774 = CARTESIAN_POINT ( 'NONE',  ( -15.58852115169999841, 1416.217772598429974, 219.1616263515979881 ) ) ;
#86775 = CARTESIAN_POINT ( 'NONE',  ( -7.622164505680827595, 1509.179741253262137, 237.4777701423770111 ) ) ;
#86776 = CARTESIAN_POINT ( 'NONE',  ( -3.021015307306127884, 1369.102705570917351, 210.6218459617000462 ) ) ;
#86777 = CARTESIAN_POINT ( 'NONE',  ( -0.2632583344880010112, 1431.930419643889991, 218.6352234134390073 ) ) ;
#86778 = DIRECTION ( 'NONE',  ( 0.000000000000000000, 0.000000000000000000, 1.000000000000000000 ) ) ;
#86779 = CARTESIAN_POINT ( 'NONE',  ( 14.02074821061520105, 1409.402675702379838, 214.2751657983629912 ) ) ;
#86780 = CARTESIAN_POINT ( 'NONE',  ( -11.55178806880000053, 1391.830795966499863, 205.9355060421790142 ) ) ;
#86781 = CARTESIAN_POINT ( 'NONE',  ( -70.27838710172480319, 1385.113716173099874, 266.4821626989880201 ) ) ;
#86782 = CARTESIAN_POINT ( 'NONE',  ( 2.872763827723777919, 1464.652692434768142, 236.7382211450293426 ) ) ;
#86783 = CARTESIAN_POINT ( 'NONE',  ( -62.81000518919999109, 1379.749407722699971, 268.0377337381589768 ) ) ;
#86784 = ORIENTED_EDGE ( 'NONE', *, *, #56186, .T. ) ;
#86785 = CARTESIAN_POINT ( 'NONE',  ( 12.32884901062990046, 1491.954766579230181, 208.6881790030290063 ) ) ;
#86787 = EDGE_LOOP ( 'NONE', ( #103778, #3952, #86233, #104081, #17706 ) ) ;
#86786 = DIRECTION ( 'NONE',  ( 1.000000000000000000, 0.000000000000000000, 0.000000000000000000 ) ) ;
#86788 = CARTESIAN_POINT ( 'NONE',  ( -16.93884325354670040, 1507.634939694479954, 230.1482608329069990 ) ) ;
#86789 = ORIENTED_EDGE ( 'NONE', *, *, #95268, .F. ) ;
#86790 = CARTESIAN_POINT ( 'NONE',  ( 6.052710029050000884, 1450.431596175490085, 208.9426997230080190 ) ) ;
#86791 = CARTESIAN_POINT ( 'NONE',  ( -9.655745333040000489, 1363.739547551590022, 207.6218459616989946 ) ) ;
#86792 = CARTESIAN_POINT ( 'NONE',  ( -5.264764398929999700, 1496.215621365389779, 199.2138428350390029 ) ) ;
#86793 = CARTESIAN_POINT ( 'NONE',  ( 29.89039938633745308, 1462.329368749827381, 269.4696393147128219 ) ) ;
#86794 = CARTESIAN_POINT ( 'NONE',  ( 21.24668427616252586, 1409.655010951418035, 207.1560907808110699 ) ) ;
#86795 = CARTESIAN_POINT ( 'NONE',  ( -0.07152471987069999870, 1397.597829882229917, 222.1216538354979946 ) ) ;
#86796 = CARTESIAN_POINT ( 'NONE',  ( 22.62861454470000311, 1507.212883763329955, 209.7205631874760172 ) ) ;
#86797 = CARTESIAN_POINT ( 'NONE',  ( -7.054635634474425210, 1516.562299717372071, 211.6679574601893421 ) ) ;
#86798 = CARTESIAN_POINT ( 'NONE',  ( -22.73782204790000350, 1507.861822361731356, 224.9164116726981320 ) ) ;
#86799 = CARTESIAN_POINT ( 'NONE',  ( -9.354513558941972562, 1368.144804009614290, 210.6218459617030021 ) ) ;
#86800 = CARTESIAN_POINT ( 'NONE',  ( -4.363122647530000009, 1407.471318475729959, 121.6099336315979969 ) ) ;
#86801 = CARTESIAN_POINT ( 'NONE',  ( -15.74154698502330163, 1459.394320999469983, 230.7248352790539911 ) ) ;
#86802 = CARTESIAN_POINT ( 'NONE',  ( 4.995994787574999485, 1516.665179208830068, 206.6322283937570035 ) ) ;
#86803 = CARTESIAN_POINT ( 'NONE',  ( -2.472529913803023227, 1523.678648413191695, 175.3762130535718597 ) ) ;
#86804 = CARTESIAN_POINT ( 'NONE',  ( -2.500000000000000000, 1438.044549794279874, 157.6830143192980245 ) ) ;
#86805 = CARTESIAN_POINT ( 'NONE',  ( 14.35446001680000094, 1416.822692809430009, 196.6654167759980396 ) ) ;
#86807 = EDGE_LOOP ( 'NONE', ( #88644, #48992, #7079, #80097 ) ) ;
#86806 = CARTESIAN_POINT ( 'NONE',  ( -68.75512860862529863, 1379.747884653289930, 280.3306324661879785 ) ) ;
#86808 = DIRECTION ( 'NONE',  ( -1.065814103640000080E-14, -1.000000000000000000, -2.775557561560010037E-16 ) ) ;
#86809 = EDGE_LOOP ( 'NONE', ( #15527, #109425, #54525, #51381, #31875 ) ) ;
#86810 = EDGE_CURVE ( 'NONE', #39044, #23842, #38297, .T. ) ;
#86811 = DIRECTION ( 'NONE',  ( -1.000000000000000000, 0.000000000000000000, 0.000000000000000000 ) ) ;
#86812 = CARTESIAN_POINT ( 'NONE',  ( -24.22746707429999802, 1430.355866426629973, 205.9027524981279953 ) ) ;
#86815 = CARTESIAN_POINT ( 'NONE',  ( 16.96718384375279953, 1410.138872099130140, 192.2499806778830020 ) ) ;
#86814 = CIRCLE ( 'NONE', #95768, 2.000000000000003997 ) ;
#86813 = CARTESIAN_POINT ( 'NONE',  ( -11.01818088618090030, 1425.247880495119944, 135.2555266203450230 ) ) ;
#86816 = CARTESIAN_POINT ( 'NONE',  ( 6.562635822504999439, 1517.111322026010157, 211.9927976380170094 ) ) ;
#86817 = CARTESIAN_POINT ( 'NONE',  ( 2.070655153456132602, 1509.117836878747084, 179.1218456497088312 ) ) ;
#86818 = CARTESIAN_POINT ( 'NONE',  ( -19.76088122879999887, 1434.994518314420247, 207.7852199276980230 ) ) ;
#86819 = CARTESIAN_POINT ( 'NONE',  ( -34.21460435710000070, 1436.526926585939918, 250.0133502278980018 ) ) ;
#86820 = CARTESIAN_POINT ( 'NONE',  ( 14.64682994990399933, 1509.425018640689814, 234.5784246007609966 ) ) ;
#86821 = CARTESIAN_POINT ( 'NONE',  ( 28.46393112515930213, 1508.969040159859787, 209.4476463742820158 ) ) ;
#86822 = ADVANCED_FACE ( 'NONE', ( #87637 ), #85821, .F. ) ;
#86823 = CARTESIAN_POINT ( 'NONE',  ( 3.966481540897129232, 1508.551704408389924, 213.6259163359240176 ) ) ;
#86824 = CARTESIAN_POINT ( 'NONE',  ( 33.14938140729999816, 1451.300093685830007, 135.9684403000979955 ) ) ;
#86825 = ORIENTED_EDGE ( 'NONE', *, *, #107894, .T. ) ;
#86826 = CARTESIAN_POINT ( 'NONE',  ( 5.343474245058209782, 1396.099658619720003, 218.7752572416549981 ) ) ;
#86827 = CARTESIAN_POINT ( 'NONE',  ( 9.808454316486640678, 1461.705508564400134, 208.1084590643120009 ) ) ;
#86828 = CARTESIAN_POINT ( 'NONE',  ( -16.94140410150000164, 1460.101846531930050, 228.3559701019979968 ) ) ;
#86829 = VERTEX_POINT ( 'NONE', #76408 ) ;
#86830 = VERTEX_POINT ( 'NONE', #59624 ) ;
#86831 = CARTESIAN_POINT ( 'NONE',  ( 10.27958569201449990, 1453.357447123039947, 211.7732196989560123 ) ) ;
#86832 = CARTESIAN_POINT ( 'NONE',  ( -6.330596753318919134, 1422.104800618580157, 147.4057733953199829 ) ) ;
#86833 = ORIENTED_EDGE ( 'NONE', *, *, #35755, .F. ) ;
#86834 = CARTESIAN_POINT ( 'NONE',  ( 0.1127810345220000010, 1412.052416346030213, 184.9056086049980081 ) ) ;
#86835 = CARTESIAN_POINT ( 'NONE',  ( -10.15866205370000053, 1462.015553540890096, 208.6820378064900012 ) ) ;
#86836 = CARTESIAN_POINT ( 'NONE',  ( -12.10873113499999931, 1442.495059057370099, 187.0567141033980079 ) ) ;
#86837 = CARTESIAN_POINT ( 'NONE',  ( -11.61555427849999944, 1470.475265069229863, 231.8199702359979710 ) ) ;
#86838 = CARTESIAN_POINT ( 'NONE',  ( 7.444963621915969831, 1508.731180391410135, 203.6086381548180100 ) ) ;
#86839 = AXIS2_PLACEMENT_3D ( 'NONE', #16632, #50829, #34017 ) ;
#86840 = CARTESIAN_POINT ( 'NONE',  ( 10.57398797330110085, 1452.565052662689823, 209.4913240895520232 ) ) ;
#86841 = CARTESIAN_POINT ( 'NONE',  ( 4.329448776274299249, 1515.064792882709980, 211.4519800890089982 ) ) ;
#86842 = CARTESIAN_POINT ( 'NONE',  ( -95.64847269556051401, 1384.859662006189865, 295.1635381067140429 ) ) ;
#86843 = CARTESIAN_POINT ( 'NONE',  ( 4.033653264325000265, 1517.028034847769959, 202.5611037067669997 ) ) ;
#86844 = CARTESIAN_POINT ( 'NONE',  ( 1.127928333405000094, 1516.989863902050047, 209.1117210464550169 ) ) ;
#86845 = VERTEX_POINT ( 'NONE', #24873 ) ;
#86846 = CARTESIAN_POINT ( 'NONE',  ( 11.83078866654130046, 1429.952306642770054, 149.4451526254590021 ) ) ;
#86847 = CARTESIAN_POINT ( 'NONE',  ( 13.03352849233194632, 1444.854847888656423, 186.9825230085123167 ) ) ;
#86848 = ORIENTED_EDGE ( 'NONE', *, *, #108950, .T. ) ;
#86849 = DIRECTION ( 'NONE',  ( -0.5877852522924820189, 0.000000000000000000, -0.8090169943749410120 ) ) ;
#86850 = CARTESIAN_POINT ( 'NONE',  ( -7.723857300294940664, 1508.513725859440001, 219.3188919284999940 ) ) ;
#86851 = CARTESIAN_POINT ( 'NONE',  ( 8.903625402870000372, 1507.331954555630091, 234.8124830750979868 ) ) ;
#86852 = AXIS2_PLACEMENT_3D ( 'NONE', #33376, #59174, #102779 ) ;
#86853 = LINE ( 'NONE', #78462, #95457 ) ;
#86854 = CARTESIAN_POINT ( 'NONE',  ( -4.642209649809999839, 1422.070992366130213, 184.6618742118980094 ) ) ;
#86855 = CARTESIAN_POINT ( 'NONE',  ( 4.854327180553859478, 1409.980837898999880, 270.0724508720410313 ) ) ;
#86856 = DIRECTION ( 'NONE',  ( 0.4794255386042040046, -5.511896626706599255E-17, -0.8775825618903723147 ) ) ;
#86857 = CARTESIAN_POINT ( 'NONE',  ( -12.61701280676319925, 1502.098792127180104, 210.9886739834400089 ) ) ;
#86858 = CARTESIAN_POINT ( 'NONE',  ( 10.82744532179999908, 1493.119756917389850, 214.1919876165190146 ) ) ;
#86859 = CARTESIAN_POINT ( 'NONE',  ( -42.12884346819999593, 1379.660956442229917, 225.9714894042589890 ) ) ;
#86860 = CARTESIAN_POINT ( 'NONE',  ( 8.931923137804934854, 1424.999313002464532, 195.6482533560690058 ) ) ;
#86862 = CARTESIAN_POINT ( 'NONE',  ( 9.168936444336990732, 1468.675008117680136, 202.6297543281519893 ) ) ;
#86861 = CARTESIAN_POINT ( 'NONE',  ( -20.98459803374077026, 1517.151704408390060, 201.4854660376508377 ) ) ;
#86863 = CARTESIAN_POINT ( 'NONE',  ( -4.363123796622770278, 1423.854800546939941, 184.2546035468919854 ) ) ;
#86864 = DIRECTION ( 'NONE',  ( -0.6736849260863841948, 0.000000000000000000, 0.7390186874254148774 ) ) ;
#86865 = CARTESIAN_POINT ( 'NONE',  ( -2.499957339863959849, 1419.383168421049959, 144.0964016714840170 ) ) ;
#86866 = ORIENTED_EDGE ( 'NONE', *, *, #103365, .F. ) ;
#86867 = CARTESIAN_POINT ( 'NONE',  ( 31.32742178079999462, 1437.308404694980027, 255.3819207742980097 ) ) ;
#86868 = CARTESIAN_POINT ( 'NONE',  ( -0.4151546846821903003, 1522.382868172863937, 244.9330574173806951 ) ) ;
#86869 = CARTESIAN_POINT ( 'NONE',  ( -20.92528053747092542, 1525.790287071788953, 233.2531890063321498 ) ) ;
#86870 = CARTESIAN_POINT ( 'NONE',  ( 3.920837378839999943, 1505.974547704289989, 220.4971537480990094 ) ) ;
#86871 = FACE_OUTER_BOUND ( 'NONE', #102924, .T. ) ;
#86873 = VERTEX_POINT ( 'NONE', #92107 ) ;
#86872 = CARTESIAN_POINT ( 'NONE',  ( -0.8972167985107359911, 1515.116734647830071, 204.7937573286989732 ) ) ;
#86874 = CARTESIAN_POINT ( 'NONE',  ( 17.09240173490840320, 1414.913527292460003, 210.5647920935599871 ) ) ;
#86875 = CARTESIAN_POINT ( 'NONE',  ( -24.21003924839999755, 1443.294921534809873, 211.9567361259179847 ) ) ;
#86876 = CARTESIAN_POINT ( 'NONE',  ( -2.278072849319670468, 1449.813593373988624, 154.3981412275377068 ) ) ;
#86877 = CARTESIAN_POINT ( 'NONE',  ( 1.914156610164409855, 1431.087920293139859, 199.8421651263110164 ) ) ;
#86878 = CARTESIAN_POINT ( 'NONE',  ( -5.804923445810000082, 1441.820529667599885, 184.4027335045979896 ) ) ;
#86879 = CARTESIAN_POINT ( 'NONE',  ( -1.876662632594598978, 1395.978594890587374, 198.1101541364135130 ) ) ;
#86880 = CARTESIAN_POINT ( 'NONE',  ( -1.484157417262785383, 1526.349684470114653, 239.9035629046661597 ) ) ;
#86881 = CARTESIAN_POINT ( 'NONE',  ( -15.10381384906500202, 1513.853571676670072, 223.9969891008670118 ) ) ;
#86882 = CARTESIAN_POINT ( 'NONE',  ( 5.885111936350000406, 1415.073945855430111, 231.3228053793980052 ) ) ;
#86883 = CARTESIAN_POINT ( 'NONE',  ( 17.69622264849999738, 1430.679833671289771, 213.5595385020990022 ) ) ;
#86884 = CARTESIAN_POINT ( 'NONE',  ( -16.85240214550000104, 1460.648904765030011, 228.2641506848979986 ) ) ;
#86885 = CARTESIAN_POINT ( 'NONE',  ( -6.950214971414999887, 1517.129577905929864, 206.2502655435069983 ) ) ;
#86886 = CARTESIAN_POINT ( 'NONE',  ( 31.61313467960000168, 1415.423113773229716, 266.8259304570980248 ) ) ;
#86887 = CARTESIAN_POINT ( 'NONE',  ( 10.93677819324079969, 1460.929513094869890, 208.6200360033440120 ) ) ;
#86888 = CARTESIAN_POINT ( 'NONE',  ( -3.487592467065000257, 1509.038615934239942, 204.6345961781970004 ) ) ;
#86889 = CARTESIAN_POINT ( 'NONE',  ( 22.92537184140000051, 1488.580164505829998, 195.5505115141980070 ) ) ;
#86890 = CARTESIAN_POINT ( 'NONE',  ( -20.51879148909999984, 1428.070798452130020, 222.7953178437979886 ) ) ;
#86891 = AXIS2_PLACEMENT_3D ( 'NONE', #36428, #70621, #78444 ) ;
#86892 = CARTESIAN_POINT ( 'NONE',  ( -14.37880041125569974, 1379.596399452129845, 208.0441480758460102 ) ) ;
#86893 = TOROIDAL_SURFACE ( 'NONE', #43738, 11.26398391340000060, 1.000000000000000000 ) ;
#86894 = EDGE_CURVE ( 'NONE', #79854, #101117, #68581, .T. ) ;
#86895 = CARTESIAN_POINT ( 'NONE',  ( -11.25901873334290038, 1500.172003390719965, 210.8567363214919794 ) ) ;
#86896 = CARTESIAN_POINT ( 'NONE',  ( 15.17118851365313681, 1478.360907884334210, 223.3047515974349153 ) ) ;
#86897 = DIRECTION ( 'NONE',  ( 1.000000000000000000, 0.000000000000000000, 1.988211042460000085E-13 ) ) ;
#86898 = CARTESIAN_POINT ( 'NONE',  ( -16.79918157119999833, 1416.515139567399729, 209.6726229222840061 ) ) ;
#86899 = CARTESIAN_POINT ( 'NONE',  ( -12.64870551279999944, 1442.301404759220077, 187.5798431206980013 ) ) ;
#86900 = EDGE_CURVE ( 'NONE', #21931, #110691, #33291, .T. ) ;
#86901 = CARTESIAN_POINT ( 'NONE',  ( 22.03465957474571013, 1522.862737210650039, 235.4136513321629991 ) ) ;
#86902 = B_SPLINE_SURFACE_WITH_KNOTS ( 'NONE', 5, 5, ( 
 ( #44298, #95238, #95786, #1755, #10127, #53256 ),
 ( #78441, #86834, #12319, #52698, #19620, #96898 ),
 ( #105290, #54903, #20706, #105854, #80086, #97439 ),
 ( #11779, #2314, #19053, #70076, #89029, #10691 ),
 ( #3404, #29132, #18502, #63320, #35892, #104189 ),
 ( #80642, #27471, #2852, #70618, #3957, #20168 ) ),
 .UNSPECIFIED., .F., .F., .F.,
 ( 6, 6 ),
 ( 6, 6 ),
 ( 30.42592446739999801, 42.69308682570000002 ),
 ( 0.000000000000000000, 2.000000000000000000 ),
 .UNSPECIFIED. ) ;
#86903 = ADVANCED_FACE ( 'NONE', ( #102149 ), #15384, .F. ) ;
#86904 = CARTESIAN_POINT ( 'NONE',  ( -29.18328456680000116, 1435.993529926829979, 136.4438111567980059 ) ) ;
#86905 = CARTESIAN_POINT ( 'NONE',  ( 1.248319867352440049, 1432.832940376729994, 200.7627304351539976 ) ) ;
#86906 = VERTEX_POINT ( 'NONE', #16471 ) ;
#86907 = CARTESIAN_POINT ( 'NONE',  ( -3.049363967234999695, 1511.141271963170084, 201.5540345636269990 ) ) ;
#86908 = CARTESIAN_POINT ( 'NONE',  ( -11.93719948218080162, 1409.329916578820075, 200.1248561717409871 ) ) ;
#86909 = CARTESIAN_POINT ( 'NONE',  ( -4.885446997243459322, 1463.524418545851404, 200.4816647042127329 ) ) ;
#86910 = DIRECTION ( 'NONE',  ( -1.000000000000000000, 0.000000000000000000, 0.000000000000000000 ) ) ;
#86911 = CARTESIAN_POINT ( 'NONE',  ( -42.24861265719999892, 1455.960523536630035, 266.5276627523979869 ) ) ;
#86912 = CARTESIAN_POINT ( 'NONE',  ( -29.55269881708379742, 1525.821544997590308, 197.1295836072967234 ) ) ;
#86913 = CARTESIAN_POINT ( 'NONE',  ( 0.1664555413521620064, 1420.066918388370141, 183.9183786667229867 ) ) ;
#86914 = CARTESIAN_POINT ( 'NONE',  ( 17.81579863472509828, 1417.685313260180010, 224.1428778951429877 ) ) ;
#86915 = CARTESIAN_POINT ( 'NONE',  ( -68.14837186395048718, 1384.667842634059980, 292.8870578847530055 ) ) ;
#86916 = CARTESIAN_POINT ( 'NONE',  ( 17.59742321542820065, 1423.715947681140051, 226.4556487353030150 ) ) ;
#86917 = CARTESIAN_POINT ( 'NONE',  ( 17.05693858869999957, 1415.931669658029932, 215.3161187075879752 ) ) ;
#86918 = CARTESIAN_POINT ( 'NONE',  ( -28.27864386137849806, 1508.411229484100204, 208.8441910969250159 ) ) ;
#86919 = AXIS2_PLACEMENT_3D ( 'NONE', #34541, #77117, #86053 ) ;
#86920 = CARTESIAN_POINT ( 'NONE',  ( -26.30762031710139937, 1482.696347288150037, 210.8481448672619933 ) ) ;
#86921 = CARTESIAN_POINT ( 'NONE',  ( 4.325805437739999704, 1515.203925700790023, 207.6585595670590010 ) ) ;
#86922 = CARTESIAN_POINT ( 'NONE',  ( -7.779176540490000846, 1507.931165456829831, 181.6769597819979936 ) ) ;
#86923 = CARTESIAN_POINT ( 'NONE',  ( -22.57962297529999773, 1409.701558196430142, 208.4161775753709946 ) ) ;
#86924 = DIRECTION ( 'NONE',  ( -0.2254368866615512057, -0.7071067811873372744, 0.6702075873423324337 ) ) ;
#86925 = CARTESIAN_POINT ( 'NONE',  ( 3.499910042949999855, 1484.886116685890102, 220.0290872740989983 ) ) ;
#86926 = CARTESIAN_POINT ( 'NONE',  ( 4.423690678889999894, 1423.173374607840060, 194.1945114146989795 ) ) ;
#86927 = CARTESIAN_POINT ( 'NONE',  ( -11.97668390569999985, 1433.616603791269881, 149.8660147765980071 ) ) ;
#86928 = CARTESIAN_POINT ( 'NONE',  ( -2.809383017458359610, 1449.519851564760074, 188.5656358724000086 ) ) ;
#86929 = CARTESIAN_POINT ( 'NONE',  ( 18.19590854888166476, 1522.382868172863937, 238.2026672068774360 ) ) ;
#86930 = CARTESIAN_POINT ( 'NONE',  ( 22.24401671484320175, 1475.958684028669950, 209.7631754067580232 ) ) ;
#86932 = CARTESIAN_POINT ( 'NONE',  ( -8.988624297290000342, 1382.710527411900102, 200.4007720520790201 ) ) ;
#86931 = CARTESIAN_POINT ( 'NONE',  ( -16.82744758394869677, 1417.384158686259980, 208.0241611917670070 ) ) ;
#86933 = CARTESIAN_POINT ( 'NONE',  ( 1.356502502699999946, 1410.320696391030197, 232.6392733810980076 ) ) ;
#86934 = LINE ( 'NONE', #84714, #75487 ) ;
#86935 = CARTESIAN_POINT ( 'NONE',  ( -11.51646780219999933, 1489.881239353890123, 211.6099079467890078 ) ) ;
#86936 = CARTESIAN_POINT ( 'NONE',  ( -22.92154104720000163, 1411.040135743629889, 211.1056462352579786 ) ) ;
#86937 = B_SPLINE_CURVE_WITH_KNOTS ( 'NONE', 3,
 ( #78914, #104090, #94574, #87867, #86186, #61022, #45864, #9478, #52604, #27382, #61562 ),
 .UNSPECIFIED., .F., .F.,
 ( 4, 2, 1, 2, 2, 4 ),
 ( 0.000000000000000000, 0.2500000000001444955, 0.3750000000003331224, 0.4375000000002918221, 0.5000000000002505773, 1.000000000000000000 ),
 .UNSPECIFIED. ) ;
#86938 = CARTESIAN_POINT ( 'NONE',  ( 10.01433557240000027, 1462.389869715989789, 210.8954298964690111 ) ) ;
#86939 = CARTESIAN_POINT ( 'NONE',  ( -1.133517003235000153, 1516.713079096360161, 204.5117660986770147 ) ) ;
#86940 = CARTESIAN_POINT ( 'NONE',  ( -30.79916350759976851, 1526.104292489138288, 201.1259370313427439 ) ) ;
#86941 =( LENGTH_UNIT ( ) NAMED_UNIT ( * ) SI_UNIT ( .MILLI., .METRE. ) );
#86942 = CARTESIAN_POINT ( 'NONE',  ( -14.57927006065989950, 1484.949786830110043, 186.8775221956059909 ) ) ;
#86943 = CARTESIAN_POINT ( 'NONE',  ( -18.20429502950000256, 1430.266005493330113, 193.4350815501980208 ) ) ;
#86944 = CARTESIAN_POINT ( 'NONE',  ( 40.65306745188510007, 1445.156483018170093, 136.9198483831620194 ) ) ;
#86946 = ORIENTED_EDGE ( 'NONE', *, *, #9215, .F. ) ;
#86945 = CARTESIAN_POINT ( 'NONE',  ( -62.58397168594589743, 1379.733354689810085, 270.6756891441229982 ) ) ;
#86947 = VERTEX_POINT ( 'NONE', #17013 ) ;
#86948 = CARTESIAN_POINT ( 'NONE',  ( 11.23895917067440031, 1434.009643533409871, 151.5816975370499904 ) ) ;
#86949 = CARTESIAN_POINT ( 'NONE',  ( 20.92528053747592054, 1525.790287071777357, 184.9905029170446085 ) ) ;
#86950 = EDGE_LOOP ( 'NONE', ( #93514, #101519, #36830, #26358, #33888, #30491, #13521 ) ) ;
#86951 = CARTESIAN_POINT ( 'NONE',  ( 25.78167222729700114, 1509.813387082529971, 195.1140727163279962 ) ) ;
#86952 = CARTESIAN_POINT ( 'NONE',  ( -3.487592467601667856, 1508.909942010301620, 213.6124651694365184 ) ) ;
#86954 = CARTESIAN_POINT ( 'NONE',  ( 13.88894654940479967, 1452.878337568840152, 223.9947615367189826 ) ) ;
#86953 = FACE_OUTER_BOUND ( 'NONE', #53203, .T. ) ;
#86955 = CARTESIAN_POINT ( 'NONE',  ( 11.96519809220000141, 1440.444625599219989, 147.6189886498980002 ) ) ;
#86956 = CARTESIAN_POINT ( 'NONE',  ( 11.84776047779999963, 1488.164498195129909, 185.6409340852979994 ) ) ;
#86957 = CARTESIAN_POINT ( 'NONE',  ( -4.988720663300000524, 1414.971262582530017, 193.0978923767980007 ) ) ;
#86958 = CARTESIAN_POINT ( 'NONE',  ( -24.28150245826429909, 1444.786156486610025, 211.3238323467629982 ) ) ;
#86959 = EDGE_CURVE ( 'NONE', #97932, #50075, #66932, .T. ) ;
#86960 = CARTESIAN_POINT ( 'NONE',  ( -5.772403812434999892, 1516.676340709600026, 212.3853678745870184 ) ) ;
#86961 = FACE_OUTER_BOUND ( 'NONE', #19421, .T. ) ;
#86962 = CARTESIAN_POINT ( 'NONE',  ( -7.446477803703490217, 1423.701825524609831, 209.9841580610070082 ) ) ;
#86963 = CARTESIAN_POINT ( 'NONE',  ( 7.750386742905000403, 1513.342361861130030, 201.6522260404070153 ) ) ;
#86964 = EDGE_LOOP ( 'NONE', ( #18217, #34219, #103134, #42954 ) ) ;
#86965 = CARTESIAN_POINT ( 'NONE',  ( 14.04488167959519984, 1435.070998900880113, 149.0410152460709980 ) ) ;
#86966 = CARTESIAN_POINT ( 'NONE',  ( 1.234341273178619858, 1432.827581395659990, 200.7608884223369898 ) ) ;
#86967 = ORIENTED_EDGE ( 'NONE', *, *, #43589, .T. ) ;
#86968 = VERTEX_POINT ( 'NONE', #42260 ) ;
#86969 = ORIENTED_EDGE ( 'NONE', *, *, #15359, .F. ) ;
#86970 = CARTESIAN_POINT ( 'NONE',  ( -6.865869646824999784, 1512.784460098860109, 216.3356833388470193 ) ) ;
#86971 = CARTESIAN_POINT ( 'NONE',  ( 16.06220691697101799, 1512.836811624714528, 198.0093864833502550 ) ) ;
#86972 = CARTESIAN_POINT ( 'NONE',  ( 9.583090267181649580, 1451.335710444785946, 152.4223268313591859 ) ) ;
#86973 = CARTESIAN_POINT ( 'NONE',  ( -4.487357341475295414, 1509.034509733380446, 206.0057038257949671 ) ) ;
#86975 = CARTESIAN_POINT ( 'NONE',  ( 9.765834982210000348, 1462.985811087089814, 208.7590207740749975 ) ) ;
#86974 = B_SPLINE_CURVE_WITH_KNOTS ( 'NONE', 5,
 ( #21450, #73001, #82494, #5796, #108237, #31525, #106587, #47240, #81368, #88702, #107135, #11983 ),
 .UNSPECIFIED., .F., .F.,
 ( 6, 3, 3, 6 ),
 ( 13.14991324430000041, 14.22551365930000067, 16.37671448909999938, 17.67668238079999909 ),
 .UNSPECIFIED. ) ;
#86976 = PRODUCT_DEFINITION_FORMATION_WITH_SPECIFIED_SOURCE ( 'ANY', '', #105426, .NOT_KNOWN. ) ;
#86977 = CARTESIAN_POINT ( 'NONE',  ( 11.23571964750900065, 1422.131126052970103, 210.3743327618489900 ) ) ;
#86978 = CARTESIAN_POINT ( 'NONE',  ( -47.55859677702834176, 1379.679709275042569, 234.9829726369564469 ) ) ;
#86979 = CARTESIAN_POINT ( 'NONE',  ( 4.228534147342459804, 1446.279633625890028, 165.3434763453030030 ) ) ;
#86980 = CARTESIAN_POINT ( 'NONE',  ( 0.8620940066740000463, 1508.701006820629800, 238.1167471285979786 ) ) ;
#86981 = EDGE_LOOP ( 'NONE', ( #62170, #17115, #8307, #94720 ) ) ;
#86982 = CARTESIAN_POINT ( 'NONE',  ( -1.136004312195000088, 1516.815173273089840, 206.2562091229970065 ) ) ;
#86983 = VERTEX_POINT ( 'NONE', #51776 ) ;
#86984 = CARTESIAN_POINT ( 'NONE',  ( 31.37724852291990629, 1440.913060387330006, 254.8116090844129644 ) ) ;
#86985 = CARTESIAN_POINT ( 'NONE',  ( -20.13259487519999880, 1508.866008678130129, 188.8141320356980088 ) ) ;
#86986 = ORIENTED_EDGE ( 'NONE', *, *, #66493, .T. ) ;
#86987 = CARTESIAN_POINT ( 'NONE',  ( 25.55809122598300220, 1449.022359460670032, 137.9040320589840292 ) ) ;
#86988 = CARTESIAN_POINT ( 'NONE',  ( -14.18461090829999982, 1409.408397915129854, 191.4295514316980018 ) ) ;
#86989 = CARTESIAN_POINT ( 'NONE',  ( -24.89775034519999863, 1442.835538705840008, 210.5176537872779932 ) ) ;
#86990 = FACE_OUTER_BOUND ( 'NONE', #97991, .T. ) ;
#86991 = CARTESIAN_POINT ( 'NONE',  ( -0.6021969839118817003, 1455.373305037211594, 218.5407630597736954 ) ) ;
#86992 = CARTESIAN_POINT ( 'NONE',  ( -4.869818399669999742, 1491.215867106689984, 188.8099941780989752 ) ) ;
#86993 = CARTESIAN_POINT ( 'NONE',  ( -13.19837685220000090, 1434.900414701970021, 149.9808420605980075 ) ) ;
#86995 = ADVANCED_FACE ( 'NONE', ( #24340 ), #60181, .T. ) ;
#86994 = CARTESIAN_POINT ( 'NONE',  ( -2.244413514000000109, 1507.820143033590057, 221.0491532391990006 ) ) ;
#86997 = CARTESIAN_POINT ( 'NONE',  ( -2.541451598548929826E-15, 1375.913060387289988, 209.1218459572589836 ) ) ;
#86996 = CARTESIAN_POINT ( 'NONE',  ( 22.03465957474218229, 1522.644714754858796, 182.8300405912402766 ) ) ;
#86998 = CARTESIAN_POINT ( 'NONE',  ( 1.712644716155000024, 1516.636036526019780, 214.1174694231270053 ) ) ;
#86999 = CARTESIAN_POINT ( 'NONE',  ( 24.08426584000000048, 1411.115194200730002, 209.6325720084630007 ) ) ;
#87000 = CIRCLE ( 'NONE', #92334, 1.000000000000000888 ) ;
#87001 = CARTESIAN_POINT ( 'NONE',  ( 6.375350481660589708, 1511.068351247050032, 216.5169480941279971 ) ) ;
#87002 = FACE_OUTER_BOUND ( 'NONE', #29670, .T. ) ;
#87003 = CARTESIAN_POINT ( 'NONE',  ( -0.7353365779029981120, 1516.995911393979895, 212.0011643880069698 ) ) ;
#87004 = CARTESIAN_POINT ( 'NONE',  ( -11.77257222062089781, 1482.353834374220014, 207.3907860494599902 ) ) ;
#87005 =( BOUNDED_CURVE ( )  B_SPLINE_CURVE ( 3, ( #107412, #65443, #56480, #90052 ),
 .UNSPECIFIED., .F., .T. ) 
 B_SPLINE_CURVE_WITH_KNOTS ( ( 4, 4 ),
 ( 1.611169255404983236, 1.690789859815214458 ),
 .UNSPECIFIED. ) 
 CURVE ( )  GEOMETRIC_REPRESENTATION_ITEM ( )  RATIONAL_B_SPLINE_CURVE ( ( 1.000000000000000000, 0.9994717830474746378, 0.9994717830474746378, 1.000000000000000000 ) ) 
 REPRESENTATION_ITEM ( '' )  );
#87006 = CARTESIAN_POINT ( 'NONE',  ( -17.26876010021493713, 1486.136097085410938, 187.8972013554511875 ) ) ;
#87008 = EDGE_LOOP ( 'NONE', ( #90772, #7886 ) ) ;
#87007 = CARTESIAN_POINT ( 'NONE',  ( -94.13685229450000236, 1388.280613784919979, 295.9239280321589831 ) ) ;
#87009 = CARTESIAN_POINT ( 'NONE',  ( 26.69977470550000120, 1440.913060384380060, 225.7788486227980229 ) ) ;
#87010 = CARTESIAN_POINT ( 'NONE',  ( 30.90487439922551616, 1525.907212628473644, 216.4335774778779466 ) ) ;
#87011 = CARTESIAN_POINT ( 'NONE',  ( -7.563688229914999894, 1510.983859056260144, 212.0526840097969909 ) ) ;
#87013 = AXIS2_PLACEMENT_3D ( 'NONE', #7364, #40962, #25243 ) ;
#87012 = CARTESIAN_POINT ( 'NONE',  ( -3.979020191233149539, 1509.031297583600008, 238.1276855365710219 ) ) ;
#87014 = DIRECTION ( 'NONE',  ( -0.9233374271748948647, -0.3766813615418239114, -0.07455969048382228570 ) ) ;
#87016 = CARTESIAN_POINT ( 'NONE',  ( 17.36536559375440092, 1409.655994655129916, 222.4839180234889966 ) ) ;
#87015 = CARTESIAN_POINT ( 'NONE',  ( 11.77676742070000060, 1432.864137865029988, 150.8103446446980058 ) ) ;
#87017 = FACE_OUTER_BOUND ( 'NONE', #6639, .T. ) ;
#87018 = CARTESIAN_POINT ( 'NONE',  ( -108.4979148419599966, 1382.105573316219989, 310.5376726789369854 ) ) ;
#87019 = ORIENTED_EDGE ( 'NONE', *, *, #81853, .F. ) ;
#87020 = CARTESIAN_POINT ( 'NONE',  ( -0.01289782690309849988, 1516.939723362869927, 204.1155860834069813 ) ) ;
#87021 = EDGE_CURVE ( 'NONE', #90277, #8406, #64381, .T. ) ;
#87022 = CARTESIAN_POINT ( 'NONE',  ( 0.5579742739800001017, 1405.845050212329852, 267.2348424307979826 ) ) ;
#87023 = DIRECTION ( 'NONE',  ( -1.000000000000000000, 0.000000000000000000, 0.000000000000000000 ) ) ;
#87024 = B_SPLINE_CURVE_WITH_KNOTS ( 'NONE', 3,
 ( #52432, #86558, #9854, #72951, #56696, #2036, #28317, #45140, #56139, #61950, #98686, #47742, #53539, #79835, #36169, #107644 ),
 .UNSPECIFIED., .F., .F.,
 ( 4, 3, 3, 3, 3, 4 ),
 ( -7.359819276019999634, -7.224550556550780378, -6.183163466960579946, -5.141872062630270079, -4.100202402597499685, -3.013663444789999701 ),
 .UNSPECIFIED. ) ;
#87025 = EDGE_CURVE ( 'NONE', #88136, #31171, #42815, .T. ) ;
#87026 = CARTESIAN_POINT ( 'NONE',  ( 13.31649357393960109, 1472.985448371380016, 270.2713846310770123 ) ) ;
#87027 = DIRECTION ( 'NONE',  ( 0.9858563016923833633, 0.000000000000000000, 0.1675928173085483863 ) ) ;
#87028 = CARTESIAN_POINT ( 'NONE',  ( 20.49831092009999978, 1496.178973653789853, 204.1013708937389879 ) ) ;
#87029 = CARTESIAN_POINT ( 'NONE',  ( -0.7326187029203401480, 1469.562181525167944, 219.1516452693006727 ) ) ;
#87030 = EDGE_CURVE ( 'NONE', #36359, #80118, #283, .T. ) ;
#87031 = CARTESIAN_POINT ( 'NONE',  ( -15.46337563405010052, 1415.677402202039957, 209.5778891453549875 ) ) ;
#87032 = CARTESIAN_POINT ( 'NONE',  ( -27.15512466070000031, 1447.232094089440125, 137.0395159971979808 ) ) ;
#87033 = CARTESIAN_POINT ( 'NONE',  ( -30.31643683089974317, 1523.530935881284904, 222.4932308532208083 ) ) ;
#87034 = CARTESIAN_POINT ( 'NONE',  ( 0.2136919556920010010, 1431.040275962890064, 200.3703063552589754 ) ) ;
#87035 = EDGE_CURVE ( 'NONE', #18362, #22689, #10307, .T. ) ;
#87036 = CARTESIAN_POINT ( 'NONE',  ( -7.891238774805787060, 1519.551704408389924, 228.7291753150780380 ) ) ;
#87037 = EDGE_CURVE ( 'NONE', #87953, #64662, #12569, .T. ) ;
#87038 = CARTESIAN_POINT ( 'NONE',  ( 1.888458389810000027, 1506.668004227690062, 221.0469516508989898 ) ) ;
#87039 = CARTESIAN_POINT ( 'NONE',  ( -38.89334934265168187, 1452.475886767586871, 269.5913128745133349 ) ) ;
#87040 = ORIENTED_EDGE ( 'NONE', *, *, #40920, .T. ) ;
#87041 = CARTESIAN_POINT ( 'NONE',  ( 2.864767215090000096, 1448.949360505710047, 183.5737851087979777 ) ) ;
#87042 = ADVANCED_FACE ( 'NONE', ( #97088 ), #41060, .T. ) ;
#87043 = CARTESIAN_POINT ( 'NONE',  ( 3.511586131400000088, 1485.920068215290030, 198.9399327136989655 ) ) ;
#87044 = CARTESIAN_POINT ( 'NONE',  ( 3.350799455140170302, 1464.627286088550136, 199.8699596448449824 ) ) ;
#87045 = CARTESIAN_POINT ( 'NONE',  ( -0.4449673945539999731, 1417.362505061330012, 235.1883008639979948 ) ) ;
#87046 = CARTESIAN_POINT ( 'NONE',  ( 12.70729947579999930, 1500.570810271889968, 209.2766994282530106 ) ) ;
#87047 = CARTESIAN_POINT ( 'NONE',  ( -31.81407709660168948, 1522.644714754858114, 196.2902540610638766 ) ) ;
#87048 = CARTESIAN_POINT ( 'NONE',  ( 7.987775376090000101, 1423.444922220860008, 212.4896135368290118 ) ) ;
#87049 = CARTESIAN_POINT ( 'NONE',  ( -9.246645418283801376, 1384.892010108799923, 218.7062641367850233 ) ) ;
#87050 = CIRCLE ( 'NONE', #60211, 1.000000000000003775 ) ;
#87051 = FACE_OUTER_BOUND ( 'NONE', #70943, .T. ) ;
#87052 = CARTESIAN_POINT ( 'NONE',  ( -9.749017428870001112, 1483.358875000189983, 202.9209122778790118 ) ) ;
#87053 = CARTESIAN_POINT ( 'NONE',  ( 26.80685737241160282, 1436.288909910419989, 136.6593321135579799 ) ) ;
#87054 = B_SPLINE_CURVE_WITH_KNOTS ( 'NONE', 5,
 ( #99148, #48234, #65587, #91321, #81255, #14044 ),
 .UNSPECIFIED., .F., .F.,
 ( 6, 6 ),
 ( 0.000000000000000000, 1.000000000000000000 ),
 .UNSPECIFIED. ) ;
#87055 = CARTESIAN_POINT ( 'NONE',  ( -13.41929410752786822, 1443.449162763163940, 169.3662372747166387 ) ) ;
#87056 = EDGE_LOOP ( 'NONE', ( #39568, #15582, #40841, #103523 ) ) ;
#87057 = EDGE_CURVE ( 'NONE', #92171, #110603, #34125, .T. ) ;
#87058 = CARTESIAN_POINT ( 'NONE',  ( -16.29829464476939904, 1409.490388075790179, 225.2024797511170107 ) ) ;
#87059 = CARTESIAN_POINT ( 'NONE',  ( 7.467133905529999893, 1443.913060387330006, 149.7989312978980081 ) ) ;
#87060 = ORIENTED_EDGE ( 'NONE', *, *, #72151, .F. ) ;
#87061 = CARTESIAN_POINT ( 'NONE',  ( -11.34479132750911390, 1501.899302646182832, 207.4495276564311155 ) ) ;
#87063 = ADVANCED_FACE ( 'NONE', ( #3600 ), #100952, .F. ) ;
#87062 = CARTESIAN_POINT ( 'NONE',  ( 7.160751159672980926, 1516.545310091885540, 206.8877586002222131 ) ) ;
#87064 = CARTESIAN_POINT ( 'NONE',  ( -3.470364637360000337, 1448.107370639490000, 190.4136600830990176 ) ) ;
#87066 = CARTESIAN_POINT ( 'NONE',  ( -1.780593273166600099, 1457.520619209220058, 219.6239990789049727 ) ) ;
#87065 = CARTESIAN_POINT ( 'NONE',  ( 11.05993000279999983, 1426.915704966229896, 94.99998741569790184 ) ) ;
#87067 = CARTESIAN_POINT ( 'NONE',  ( 3.350338079455601026, 1523.604703353109699, 176.1628856388066708 ) ) ;
#87068 = B_SPLINE_CURVE_WITH_KNOTS ( 'NONE', 3,
 ( #108596, #31884, #107482, #65512 ),
 .UNSPECIFIED., .F., .F.,
 ( 4, 4 ),
 ( -128.3330504879999978, -82.60380882990649809 ),
 .UNSPECIFIED. ) ;
#87069 = EDGE_CURVE ( 'NONE', #68807, #83932, #103675, .T. ) ;
#87070 = CARTESIAN_POINT ( 'NONE',  ( -8.723783498850000484, 1451.961142758290180, 205.5456223906990090 ) ) ;
#87071 = CARTESIAN_POINT ( 'NONE',  ( 2.484577657225000014, 1517.170512887980067, 201.7834339727070017 ) ) ;
#87072 = CARTESIAN_POINT ( 'NONE',  ( 7.892648486029999688, 1424.312437875390060, 211.9575832887890101 ) ) ;
#87074 = CARTESIAN_POINT ( 'NONE',  ( -16.83568192250000095, 1418.884533543920043, 201.2565368162689765 ) ) ;
#87073 = AXIS2_PLACEMENT_3D ( 'NONE', #62955, #35487, #69681 ) ;
#87075 = CARTESIAN_POINT ( 'NONE',  ( -21.12854635009999882, 1507.715432716589703, 209.4790063781609888 ) ) ;
#87076 = CARTESIAN_POINT ( 'NONE',  ( 2.540129801540000010, 1449.030645993539792, 182.8575104869979953 ) ) ;
#87077 = ADVANCED_FACE ( 'NONE', ( #94171 ), #106304, .T. ) ;
#87078 = CARTESIAN_POINT ( 'NONE',  ( 8.770701337765752115, 1364.659332542723632, 210.6218459617142003 ) ) ;
#87080 = ORIENTED_EDGE ( 'NONE', *, *, #31652, .F. ) ;
#87079 = CARTESIAN_POINT ( 'NONE',  ( -4.730384201341079731, 1508.603735221695615, 205.6342535013503721 ) ) ;
#87081 = VERTEX_POINT ( 'NONE', #103116 ) ;
#87082 = CARTESIAN_POINT ( 'NONE',  ( -113.4000000000000057, 1310.214785017039958, 304.2218459572619622 ) ) ;
#87083 = CARTESIAN_POINT ( 'NONE',  ( -15.77403878809999860, 1409.463901959830082, 192.8704306968979836 ) ) ;
#87084 = CARTESIAN_POINT ( 'NONE',  ( -2.236976319609999653, 1471.546594272430184, 269.6154293286980419 ) ) ;
#87085 = CARTESIAN_POINT ( 'NONE',  ( 2.744925583754461940, 1499.105962719451554, 198.1014308731936069 ) ) ;
#87086 = CARTESIAN_POINT ( 'NONE',  ( 0.1582547704020000057, 1486.366246513129909, 181.8206974649980054 ) ) ;
#87087 = CARTESIAN_POINT ( 'NONE',  ( -31.75409331310280692, 1525.055402519434210, 201.5867938956818364 ) ) ;
#87088 = CARTESIAN_POINT ( 'NONE',  ( -1.841894009802319987, 1475.332893174979972, 197.8298818394579826 ) ) ;
#87089 = CARTESIAN_POINT ( 'NONE',  ( 12.63038619288439968, 1428.207532477410041, 223.9332333053530135 ) ) ;
#87090 = CARTESIAN_POINT ( 'NONE',  ( 33.92723937951050317, 1435.682267998569841, 135.5036483818229840 ) ) ;
#87091 = CARTESIAN_POINT ( 'NONE',  ( 7.079892945961029582, 1396.160295697190122, 217.6030398920230198 ) ) ;
#87092 = CARTESIAN_POINT ( 'NONE',  ( 10.31428324521939821, 1409.273243095039788, 197.3781550435539884 ) ) ;
#87093 = CARTESIAN_POINT ( 'NONE',  ( -2.300955939006319895, 1405.879429239740148, 267.2329980173330455 ) ) ;
#87094 = CARTESIAN_POINT ( 'NONE',  ( -14.58077760642500031, 1436.114534100510127, 149.8442496726960087 ) ) ;
#87095 = ORIENTED_EDGE ( 'NONE', *, *, #109812, .T. ) ;
#87096 = CARTESIAN_POINT ( 'NONE',  ( -18.64588652299999794, 1416.828040475229955, 208.5593769277110141 ) ) ;
#87097 = CARTESIAN_POINT ( 'NONE',  ( 14.25940458439999858, 1444.037519612920050, 189.5923944946979987 ) ) ;
#87098 = ORIENTED_EDGE ( 'NONE', *, *, #27274, .T. ) ;
#87099 = ORIENTED_EDGE ( 'NONE', *, *, #46651, .F. ) ;
#87100 = CARTESIAN_POINT ( 'NONE',  ( -3.637379841050000007, 1454.260016440290201, 199.7007646786289854 ) ) ;
#87101 = CARTESIAN_POINT ( 'NONE',  ( -8.696701630030000629, 1367.135748871429996, 207.6218459616989946 ) ) ;
#87102 = CIRCLE ( 'NONE', #13776, 2.000000000549930324 ) ;
#87103 = CARTESIAN_POINT ( 'NONE',  ( -4.030514550714999977, 1516.901952101700090, 213.7446888144170032 ) ) ;
#87104 = CARTESIAN_POINT ( 'NONE',  ( 2.766744922505000037, 1511.930588878439949, 216.8060890453470222 ) ) ;
#87105 = EDGE_CURVE ( 'NONE', #13404, #100973, #87873, .T. ) ;
#87106 = EDGE_LOOP ( 'NONE', ( #56837, #54593, #108267, #7104, #64425, #84670, #11507 ) ) ;
#87107 = CARTESIAN_POINT ( 'NONE',  ( -88.16707050029999948, 1379.270434038089888, 298.5681932088589861 ) ) ;
#87108 = ADVANCED_FACE ( 'NONE', ( #3328 ), #92932, .F. ) ;
#87109 = CARTESIAN_POINT ( 'NONE',  ( 7.561651663499999287, 1415.425582719929707, 225.2205323159980139 ) ) ;
#87110 = CARTESIAN_POINT ( 'NONE',  ( 1.705466410464999916, 1517.120861839400050, 204.1076508302870138 ) ) ;
#87111 = CARTESIAN_POINT ( 'NONE',  ( -28.09217120239999943, 1508.632189896530008, 207.7571593959380039 ) ) ;
#87112 = CARTESIAN_POINT ( 'NONE',  ( -0.9134622989720000419, 1487.754272106330063, 231.1436532359980163 ) ) ;
#87113 = CARTESIAN_POINT ( 'NONE',  ( -109.9987473180000137, 1385.244513981200043, 297.1847073398589600 ) ) ;
#87114 = CARTESIAN_POINT ( 'NONE',  ( -58.24002330138049643, 1384.662383407990092, 240.2918130150210061 ) ) ;
#87115 = CARTESIAN_POINT ( 'NONE',  ( 7.329930013194999816, 1516.881930554049859, 201.4037113026670056 ) ) ;
#87116 = CARTESIAN_POINT ( 'NONE',  ( -9.701291430620001321, 1409.251836952829990, 228.6783269308979811 ) ) ;
#87118 = EDGE_LOOP ( 'NONE', ( #79213, #30217 ) ) ;
#87117 = CARTESIAN_POINT ( 'NONE',  ( -4.118684918089999591, 1446.308391630630013, 183.7684684173979974 ) ) ;
#87119 = DIRECTION ( 'NONE',  ( -0.9455185755993178454, 0.000000000000000000, 0.3255681544571539243 ) ) ;
#87120 = CARTESIAN_POINT ( 'NONE',  ( 3.074703527060000052, 1441.333178254290033, 218.5515148082390056 ) ) ;
#87122 = CARTESIAN_POINT ( 'NONE',  ( -9.157150010547340457, 1440.811674898089223, 204.9830327270436499 ) ) ;
#87121 = TOROIDAL_SURFACE ( 'NONE', #105031, 1.000000000000000000, 1.000000000000000000 ) ;
#87124 = ADVANCED_FACE ( 'NONE', ( #57025 ), #49720, .F. ) ;
#87123 = CARTESIAN_POINT ( 'NONE',  ( -14.47420009890000081, 1416.181292664740113, 214.4142689833190047 ) ) ;
#87125 = CARTESIAN_POINT ( 'NONE',  ( -24.45522160929999700, 1435.370145036180020, 136.4741062850980029 ) ) ;
#87126 = CARTESIAN_POINT ( 'NONE',  ( 2.298369469825000344, 1516.779243033999819, 212.3734572960470075 ) ) ;
#87127 = CARTESIAN_POINT ( 'NONE',  ( -66.98943634389999602, 1379.744194872529988, 276.3872057256589869 ) ) ;
#87128 = CIRCLE ( 'NONE', #63896, 1.999999999999999556 ) ;
#87129 = CARTESIAN_POINT ( 'NONE',  ( -5.728574053214379624, 1424.937532576071590, 226.9478413594984545 ) ) ;
#87130 = CARTESIAN_POINT ( 'NONE',  ( -30.00906687502022407, 1525.856064936166604, 221.1186969528658608 ) ) ;
#87131 = CARTESIAN_POINT ( 'NONE',  ( -11.60004869885203682, 1423.973206102290760, 135.9381536961890617 ) ) ;
#87132 = CARTESIAN_POINT ( 'NONE',  ( -3.455495871984999745, 1516.939877939420057, 209.1351200182310208 ) ) ;
#87133 = ORIENTED_EDGE ( 'NONE', *, *, #66087, .T. ) ;
#87134 = CARTESIAN_POINT ( 'NONE',  ( -1.787767503901650068, 1451.934961237370089, 184.2182930155049974 ) ) ;
#87135 = CARTESIAN_POINT ( 'NONE',  ( -8.381285897630000647, 1412.830257829430138, 230.5949227061979911 ) ) ;
#87136 = CARTESIAN_POINT ( 'NONE',  ( -32.09787761819999474, 1385.089932967300001, 229.9554828700589724 ) ) ;
#87137 = ORIENTED_EDGE ( 'NONE', *, *, #22433, .F. ) ;
#87138 = CARTESIAN_POINT ( 'NONE',  ( -18.21948982384089888, 1385.283089966090074, 220.2654309255580074 ) ) ;
#87139 = ADVANCED_FACE ( 'NONE', ( #48058 ), #22818, .F. ) ;
#87140 = CARTESIAN_POINT ( 'NONE',  ( -2.451814761660000119, 1429.700538131990015, 200.7967561671190140 ) ) ;
#87141 = CARTESIAN_POINT ( 'NONE',  ( 12.49310090042409982, 1434.470230054580043, 149.8104293411710159 ) ) ;
#87142 = CARTESIAN_POINT ( 'NONE',  ( 6.375428557307381006, 1488.402514618529722, 234.5820377068529865 ) ) ;
#87143 =( BOUNDED_SURFACE ( )  B_SPLINE_SURFACE ( 3, 2, ( 
 ( #84653, #42119, #58375 ),
 ( #83550, #32615, #15768 ),
 ( #66791, #48887, #58924 ),
 ( #108764, #100891, #93055 ),
 ( #8493, #84106, #7406 ),
 ( #32057, #109871, #76267 ),
 ( #16328, #67890, #101998 ),
 ( #25284, #59484, #93595 ),
 ( #16872, #51077, #42665 ),
 ( #86317, #61161, #1229 ),
 ( #52734, #28622, #9059 ),
 ( #70663, #44899, #79591 ),
 ( #86869, #51624, #104778 ),
 ( #44336, #85760, #103101 ) ),
 .UNSPECIFIED., .F., .F., .F. ) 
 B_SPLINE_SURFACE_WITH_KNOTS ( ( 4, 2, 2, 2, 2, 2, 4 ),
 ( 3, 3 ),
 ( 0.000000000000000000, 0.0009440840677143813933, 0.001416126101571572090, 0.001888168135428762787, 0.002360210169285953483, 0.002832252203143144180, 0.003776336270857525573 ),
 ( 0.000000000000000000, 1.000000000000000000 ),
 .UNSPECIFIED. ) 
 GEOMETRIC_REPRESENTATION_ITEM ( )  RATIONAL_B_SPLINE_SURFACE ( (
 ( 1.000000000000000000, 0.8070209408750133040, 1.000000000000000000),
 ( 1.000000000000000000, 0.8215603905301913645, 1.000000000000000000),
 ( 1.000000000000000000, 0.8340988699037210630, 1.000000000000000000),
 ( 1.000000000000000000, 0.8516751610470432166, 1.000000000000000000),
 ( 1.000000000000000000, 0.8573697395158472734, 1.000000000000000000),
 ( 1.000000000000000000, 0.8683586635657976061, 1.000000000000000000),
 ( 1.000000000000000000, 0.8736518481707038486, 1.000000000000000000),
 ( 1.000000000000000000, 0.8840377753031671837, 1.000000000000000000),
 ( 1.000000000000000000, 0.8891294171305078597, 1.000000000000000000),
 ( 1.000000000000000000, 0.8992456600575245984, 1.000000000000000000),
 ( 1.000000000000000000, 0.9042785869232097262, 1.000000000000000000),
 ( 1.000000000000000000, 0.9189749222880136958, 1.000000000000000000),
 ( 1.000000000000000000, 0.9283978182317160766, 1.000000000000000000),
 ( 1.000000000000000000, 0.9376006582765968878, 1.000000000000000000) ) ) 
 REPRESENTATION_ITEM ( '' )  SURFACE ( )  );
#87144 = CARTESIAN_POINT ( 'NONE',  ( -23.30096132306110235, 1508.459748541459930, 223.9027429165689682 ) ) ;
#87145 = ADVANCED_FACE ( 'NONE', ( #82193 ), #109928, .T. ) ;
#87146 = CARTESIAN_POINT ( 'NONE',  ( -1.724134400390000099, 1408.973268486529832, 187.2669157652979948 ) ) ;
#87147 = CARTESIAN_POINT ( 'NONE',  ( 11.48577098159999998, 1425.717070342639772, 202.9081124425690064 ) ) ;
#87148 = DIRECTION ( 'NONE',  ( 0.9455185755993178454, 0.000000000000000000, -0.3255681544571537578 ) ) ;
#87150 = CARTESIAN_POINT ( 'NONE',  ( 16.08564639389649997, 1496.414352768219942, 193.8777386732119794 ) ) ;
#87149 = CARTESIAN_POINT ( 'NONE',  ( 0.7553264358530019651, 1516.745833913490060, 214.8974710475970085 ) ) ;
#87151 = CARTESIAN_POINT ( 'NONE',  ( -5.519031869190039963, 1391.701565166340060, 214.9395334166419786 ) ) ;
#87152 = CARTESIAN_POINT ( 'NONE',  ( -5.004475612664999851, 1517.026025493960105, 216.8437538584669824 ) ) ;
#87153 = EDGE_LOOP ( 'NONE', ( #7326, #37051 ) ) ;
#87154 = CARTESIAN_POINT ( 'NONE',  ( -12.21873817507669990, 1415.431750870129918, 196.1844242608510172 ) ) ;
#87155 = CARTESIAN_POINT ( 'NONE',  ( 12.39573405564623165, 1517.051704408389924, 218.5685989363918225 ) ) ;
#87156 = VERTEX_POINT ( 'NONE', #9360 ) ;
#87157 = CARTESIAN_POINT ( 'NONE',  ( 3.903606122229999809, 1420.588980623530006, 185.5382139491979956 ) ) ;
#87158 = ADVANCED_FACE ( 'NONE', ( #95019 ), #41992, .T. ) ;
#87159 = CARTESIAN_POINT ( 'NONE',  ( -17.21060100480000088, 1507.583332828389985, 209.3895586510680005 ) ) ;
#87160 = DIRECTION ( 'NONE',  ( -0.9455185755993178454, 0.000000000000000000, 0.3255681544571537578 ) ) ;
#87161 = CARTESIAN_POINT ( 'NONE',  ( 3.023734050500000325, 1442.695058689789903, 217.4756557394289871 ) ) ;
#87162 = DIRECTION ( 'NONE',  ( 0.9455185755993178454, 0.000000000000000000, -0.3255681544571539243 ) ) ;
#87163 = CARTESIAN_POINT ( 'NONE',  ( -20.49599333844833993, 1525.960063244516959, 233.8638087104925489 ) ) ;
#87164 = CARTESIAN_POINT ( 'NONE',  ( 17.64235773549999919, 1415.063410501330054, 210.6787325816779912 ) ) ;
#87166 = EDGE_CURVE ( 'NONE', #23656, #84410, #34993, .T. ) ;
#87165 = CARTESIAN_POINT ( 'NONE',  ( -28.44685754529687571, 1526.382868172863937, 219.8746262742137105 ) ) ;
#87167 = CARTESIAN_POINT ( 'NONE',  ( -14.03269008360000036, 1434.988272402140183, 148.9022108617980109 ) ) ;
#87168 = CARTESIAN_POINT ( 'NONE',  ( 33.93392607710000419, 1451.271780568129998, 135.9464999937979997 ) ) ;
#87169 = DIRECTION ( 'NONE',  ( 0.9455185755993178454, 0.000000000000000000, -0.3255681544571537578 ) ) ;
#87171 = CARTESIAN_POINT ( 'NONE',  ( -19.04163037422885552, 1439.995762762720460, 209.8507536649994165 ) ) ;
#87170 = FACE_OUTER_BOUND ( 'NONE', #34491, .T. ) ;
#87172 = CARTESIAN_POINT ( 'NONE',  ( 10.84538211560184351, 1425.248158932944079, 146.5362285467592756 ) ) ;
#87173 = ORIENTED_EDGE ( 'NONE', *, *, #81452, .F. ) ;
#87174 = CARTESIAN_POINT ( 'NONE',  ( 1.556610602838379931, 1415.059973079630026, 191.5211804267419780 ) ) ;
#87175 = CARTESIAN_POINT ( 'NONE',  ( -4.492641941105690151, 1508.880976867409800, 212.2392493694379993 ) ) ;
#87176 = EDGE_CURVE ( 'NONE', #72398, #90951, #19444, .T. ) ;
#87177 = AXIS2_PLACEMENT_3D ( 'NONE', #7845, #17322, #67233 ) ;
#87178 = CARTESIAN_POINT ( 'NONE',  ( -11.87550762067749943, 1433.043840718726415, 149.9802264065416750 ) ) ;
#87179 = CARTESIAN_POINT ( 'NONE',  ( -4.528990542849999024, 1484.552700007790008, 198.9721756806989958 ) ) ;
#87180 = CARTESIAN_POINT ( 'NONE',  ( -10.48842657476610185, 1479.773419084050147, 209.6713063323329891 ) ) ;
#87181 = CARTESIAN_POINT ( 'NONE',  ( -20.59684415639999955, 1507.762623717429960, 190.9355247910979756 ) ) ;
#87182 = CYLINDRICAL_SURFACE ( 'NONE', #43740, 1.999999999999999556 ) ;
#87183 = EDGE_CURVE ( 'NONE', #21410, #33283, #84883, .T. ) ;
#87184 = CARTESIAN_POINT ( 'NONE',  ( -10.05468035857399833, 1491.062548945049912, 213.6251199428619714 ) ) ;
#87185 = CARTESIAN_POINT ( 'NONE',  ( 13.25967441340000086, 1414.983771848829747, 197.8194332372980000 ) ) ;
#87186 = CARTESIAN_POINT ( 'NONE',  ( -90.09176604164480295, 1383.770261446130007, 308.5472844327179587 ) ) ;
#87187 = CARTESIAN_POINT ( 'NONE',  ( 1.106990746626510029E-15, 1390.939237335599955, 209.1218459572589836 ) ) ;
#87188 = PLANE ( 'NONE',  #48249 ) ;
#87189 = FACE_OUTER_BOUND ( 'NONE', #451, .T. ) ;
#87191 = ORIENTED_EDGE ( 'NONE', *, *, #79152, .F. ) ;
#87190 = CARTESIAN_POINT ( 'NONE',  ( 10.56624192506330040, 1452.381986011830122, 209.0163554798489827 ) ) ;
#87192 = CARTESIAN_POINT ( 'NONE',  ( -17.89145751773400761, 1459.891188655622500, 228.0875397610878963 ) ) ;
#87193 = CARTESIAN_POINT ( 'NONE',  ( -81.52042378539999845, 1379.302443467629928, 294.8143971615589862 ) ) ;
#87194 = CARTESIAN_POINT ( 'NONE',  ( 20.08991052607950323, 1509.197173136989932, 229.8362170949519907 ) ) ;
#87195 = ORIENTED_EDGE ( 'NONE', *, *, #87677, .T. ) ;
#87196 = ORIENTED_EDGE ( 'NONE', *, *, #57599, .T. ) ;
#87197 = CARTESIAN_POINT ( 'NONE',  ( 17.13546961575789851, 1509.208612314439961, 231.8360975173889926 ) ) ;
#87198 = CARTESIAN_POINT ( 'NONE',  ( 30.60906614450638230, 1526.073434386619738, 201.6841089170558519 ) ) ;
#87199 = CARTESIAN_POINT ( 'NONE',  ( 12.95646782890822024, 1442.923247039539092, 169.4280525748522450 ) ) ;
#87201 = CARTESIAN_POINT ( 'NONE',  ( -4.495633307820000005E-08, 1473.529235887330060, 262.4989462860979756 ) ) ;
#87200 = CARTESIAN_POINT ( 'NONE',  ( 20.46400528219999870, 1470.815019615230085, 209.0339138421799987 ) ) ;
#87202 = ADVANCED_FACE ( 'NONE', ( #3745 ), #54698, .T. ) ;
#87203 = CARTESIAN_POINT ( 'NONE',  ( -3.951796886255740215, 1495.396716508259942, 197.4422882964240102 ) ) ;
#87204 = CARTESIAN_POINT ( 'NONE',  ( -109.3876690420000131, 1382.506854422480046, 297.3616832378589834 ) ) ;
#87205 = CARTESIAN_POINT ( 'NONE',  ( 25.66085765329999901, 1508.559638121829948, 199.8979669743779937 ) ) ;
#87206 = CARTESIAN_POINT ( 'NONE',  ( -20.74297378600000030, 1486.050832587129889, 191.3292126814980065 ) ) ;
#87207 = CARTESIAN_POINT ( 'NONE',  ( -9.828024340748898524, 1446.801136768030119, 212.2328356403849909 ) ) ;
#87208 = CARTESIAN_POINT ( 'NONE',  ( 5.480463564019999900, 1422.526046715330040, 185.8321080085979986 ) ) ;
#87210 = EDGE_CURVE ( 'NONE', #17997, #91497, #18838, .T. ) ;
#87209 = CARTESIAN_POINT ( 'NONE',  ( -11.39453227890000164, 1435.362097301539961, 151.5417150060980020 ) ) ;
#87211 = CARTESIAN_POINT ( 'NONE',  ( 11.55343380559999922, 1436.871189967930150, 151.7006543630979820 ) ) ;
#87212 = CARTESIAN_POINT ( 'NONE',  ( -8.977835948444159442, 1424.635420156040027, 204.7825922023490079 ) ) ;
#87213 = AXIS2_PLACEMENT_3D ( 'NONE', #102734, #17059, #104418 ) ;
#87214 = CARTESIAN_POINT ( 'NONE',  ( 1.151838181399999828, 1507.064426625830038, 237.0475204680980141 ) ) ;
#87215 = LINE ( 'NONE', #35148, #31854 ) ;
#87216 = ORIENTED_EDGE ( 'NONE', *, *, #88299, .F. ) ;
#87217 = CARTESIAN_POINT ( 'NONE',  ( -3.865424752135750097, 1508.610338626970133, 213.5325984595829993 ) ) ;
#87218 = CARTESIAN_POINT ( 'NONE',  ( 18.37994959805489970, 1472.972861928199791, 195.0276218624729836 ) ) ;
#87219 = CARTESIAN_POINT ( 'NONE',  ( -42.45911994060000438, 1445.498763873839835, 270.1977472527979671 ) ) ;
#87220 = CARTESIAN_POINT ( 'NONE',  ( -23.70138498562419471, 1436.173432996585234, 212.0448533859750739 ) ) ;
#87221 = CARTESIAN_POINT ( 'NONE',  ( 17.67654200049999957, 1410.026337379229972, 223.0785978711979851 ) ) ;
#87222 = CARTESIAN_POINT ( 'NONE',  ( -14.72117515839999946, 1485.050094052629902, 224.1720311065980127 ) ) ;
#87223 = DIRECTION ( 'NONE',  ( -0.9510565162951566398, 0.000000000000000000, -0.3090169943749382919 ) ) ;
#87224 = CARTESIAN_POINT ( 'NONE',  ( 2.925928197532340125, 1410.286699746360227, 231.6216146004889822 ) ) ;
#87225 = CARTESIAN_POINT ( 'NONE',  ( -1.270728274629999932, 1414.996444518330009, 226.4582995714980029 ) ) ;
#87226 = CARTESIAN_POINT ( 'NONE',  ( -3.167625933140000072, 1417.589985715129842, 234.1420239621979817 ) ) ;
#87227 = DIRECTION ( 'NONE',  ( 1.000000000000000000, 3.152985556228405519E-15, -4.340229276715479857E-15 ) ) ;
#87228 = B_SPLINE_CURVE_WITH_KNOTS ( 'NONE', 3,
 ( #84487, #34637, #69932, #76096, #34083, #95651, #103482, #26787, #77209, #33508 ),
 .UNSPECIFIED., .F., .F.,
 ( 4, 2, 2, 2, 4 ),
 ( 0.000000000000000000, 0.2500000000000000000, 0.5000000000000000000, 0.7500000000000000000, 1.000000000000000000 ),
 .UNSPECIFIED. ) ;
#87229 = CARTESIAN_POINT ( 'NONE',  ( -3.982247585415259916, 1360.759224656435890, 210.6218459616991936 ) ) ;
#87230 = CARTESIAN_POINT ( 'NONE',  ( -43.73454037239169878, 1430.821798806799961, 266.2441235663050065 ) ) ;
#87231 = CARTESIAN_POINT ( 'NONE',  ( -4.146782939769999565, 1426.018316117329960, 186.1121555218979893 ) ) ;
#87232 = ORIENTED_EDGE ( 'NONE', *, *, #5421, .T. ) ;
#87233 = DIRECTION ( 'NONE',  ( 0.000000000000000000, 1.000000000000000000, 0.000000000000000000 ) ) ;
#87234 = EDGE_LOOP ( 'NONE', ( #78378, #91123, #79315, #22745 ) ) ;
#87235 = CARTESIAN_POINT ( 'NONE',  ( -2.868112169295000236, 1516.855632454399938, 209.8795095036720113 ) ) ;
#87236 = FACE_OUTER_BOUND ( 'NONE', #108570, .T. ) ;
#87237 = CIRCLE ( 'NONE', #55130, 0.9999999999998898659 ) ;
#87238 = CARTESIAN_POINT ( 'NONE',  ( -20.86054011779999939, 1508.959477709830026, 190.3575368027980232 ) ) ;
#87239 = CARTESIAN_POINT ( 'NONE',  ( -5.601667600379999890, 1410.392892709329772, 187.0683166722980104 ) ) ;
#87240 = FACE_OUTER_BOUND ( 'NONE', #90122, .T. ) ;
#87241 = ORIENTED_EDGE ( 'NONE', *, *, #109148, .F. ) ;
#87242 = CARTESIAN_POINT ( 'NONE',  ( 20.57759936150000257, 1430.447427346229915, 213.0442855874480017 ) ) ;
#87244 = CARTESIAN_POINT ( 'NONE',  ( 76.99707197884903564, 1524.382868172863937, 19.35599459046138193 ) ) ;
#87243 = DIRECTION ( 'NONE',  ( 0.02616798426500960631, -0.9993150019883683122, -0.02616798426500960631 ) ) ;
#87245 = CARTESIAN_POINT ( 'NONE',  ( 7.069913306463050162, 1426.666554464499995, 213.2414280066960259 ) ) ;
#87246 = DIRECTION ( 'NONE',  ( 3.331145804512843979E-08, 5.455889386854617429E-11, 0.9999999999999995559 ) ) ;
#87247 = CARTESIAN_POINT ( 'NONE',  ( 6.824562263029999798, 1471.929136523390071, 216.7044338043689891 ) ) ;
#87248 = CARTESIAN_POINT ( 'NONE',  ( -8.611006801263458854, 1438.354984712640089, 207.9016507195429995 ) ) ;
#87249 = ORIENTED_EDGE ( 'NONE', *, *, #33087, .T. ) ;
#87250 = CARTESIAN_POINT ( 'NONE',  ( -28.33587269610449866, 1415.670569832889896, 270.2700704253879849 ) ) ;
#87251 = CARTESIAN_POINT ( 'NONE',  ( -3.269025173884999802, 1517.026534522949987, 208.0024068424170025 ) ) ;
#87252 = CARTESIAN_POINT ( 'NONE',  ( 4.196431865958829555, 1416.112438447810064, 231.6845605219920117 ) ) ;
#87253 = DIRECTION ( 'NONE',  ( 0.000000000000000000, 1.000000000000000000, 0.000000000000000000 ) ) ;
#87255 = EDGE_LOOP ( 'NONE', ( #14640, #26790 ) ) ;
#87254 = CARTESIAN_POINT ( 'NONE',  ( -6.371134682390000137, 1368.423166410909971, 207.6218459616989946 ) ) ;
#87256 = ORIENTED_EDGE ( 'NONE', *, *, #102475, .F. ) ;
#87257 = CARTESIAN_POINT ( 'NONE',  ( -22.67952439726359870, 1409.704860892969918, 209.4938531156840043 ) ) ;
#87258 = CARTESIAN_POINT ( 'NONE',  ( -0.8807669020151700501, 1409.878743503689975, 185.2313411206270075 ) ) ;
#87259 = CARTESIAN_POINT ( 'NONE',  ( -20.06562366400000030, 1485.934169092390221, 214.0282076738189971 ) ) ;
#87260 = CIRCLE ( 'NONE', #62269, 0.9999999999999971134 ) ;
#87261 = CARTESIAN_POINT ( 'NONE',  ( 19.18645890815103883, 1474.831003437985828, 202.6579824388850568 ) ) ;
#87262 = CARTESIAN_POINT ( 'NONE',  ( -18.80861391721730058, 1416.321686226169959, 207.5736137325899904 ) ) ;
#87263 = CARTESIAN_POINT ( 'NONE',  ( -17.84981256740000077, 1425.821171079729993, 226.1975678583979743 ) ) ;
#87264 = CARTESIAN_POINT ( 'NONE',  ( 40.67628413852310132, 1456.517704155799947, 269.1116589114889734 ) ) ;
#87265 = CARTESIAN_POINT ( 'NONE',  ( -11.67377857781220030, 1391.913060387289988, 209.5093625368419907 ) ) ;
#87266 = CARTESIAN_POINT ( 'NONE',  ( 5.515204341519999609, 1447.426897563979992, 184.7404326633980247 ) ) ;
#87267 = CARTESIAN_POINT ( 'NONE',  ( -4.042417815834999928, 1516.904492006980036, 205.6736390534169914 ) ) ;
#87268 = VERTEX_POINT ( 'NONE', #78773 ) ;
#87269 = CARTESIAN_POINT ( 'NONE',  ( -3.806848320439999878, 1438.700957657089930, 227.3446634402990014 ) ) ;
#87271 = B_SPLINE_CURVE_WITH_KNOTS ( 'NONE', 3,
 ( #79543, #47587, #96890, #11772, #21236, #88487 ),
 .UNSPECIFIED., .F., .F.,
 ( 4, 2, 4 ),
 ( 0.000000000000000000, 0.5000000000000000000, 1.000000000000000000 ),
 .UNSPECIFIED. ) ;
#87270 = CARTESIAN_POINT ( 'NONE',  ( 1.490044353047579984, 1471.418353334920084, 182.6703762986020081 ) ) ;
#87272 = CARTESIAN_POINT ( 'NONE',  ( 23.47355847000000040, 1409.990881410429893, 208.6231098356030031 ) ) ;
#87273 = ORIENTED_EDGE ( 'NONE', *, *, #70687, .T. ) ;
#87274 = CARTESIAN_POINT ( 'NONE',  ( -1.530900592538410043, 1457.980095062469900, 229.8454460011110143 ) ) ;
#87275 = CARTESIAN_POINT ( 'NONE',  ( 25.68381050121670128, 1452.010962298709956, 135.3221168002480113 ) ) ;
#87276 = DIRECTION ( 'NONE',  ( 0.000000000000000000, -1.000000000000000000, 0.000000000000000000 ) ) ;
#87277 = CARTESIAN_POINT ( 'NONE',  ( -31.75214877180000528, 1390.937306157359899, 216.9912452226689936 ) ) ;
#87278 = CARTESIAN_POINT ( 'NONE',  ( -4.329448776040000446, 1515.064792882589927, 209.0973262533439936 ) ) ;
#87279 = CARTESIAN_POINT ( 'NONE',  ( 17.24303251159999917, 1409.680293628830213, 193.2722534259980307 ) ) ;
#87280 = CARTESIAN_POINT ( 'NONE',  ( 18.57285056714469107, 1444.740067931810245, 161.9794701184630696 ) ) ;
#87281 = FACE_OUTER_BOUND ( 'NONE', #78741, .T. ) ;
#87283 = CARTESIAN_POINT ( 'NONE',  ( -21.14513965206749901, 1428.384847628398347, 220.1321864412567209 ) ) ;
#87282 = CARTESIAN_POINT ( 'NONE',  ( -3.829620113920000346, 1515.551704408389924, 206.7917118429090237 ) ) ;
#87284 = CIRCLE ( 'NONE', #53329, 18.16666666670000296 ) ;
#87285 = CARTESIAN_POINT ( 'NONE',  ( 0.4493958440627169870, 1451.091564611090007, 182.2331086531640096 ) ) ;
#87286 = FACE_OUTER_BOUND ( 'NONE', #68957, .T. ) ;
#87287 = VECTOR ( 'NONE', #37074, 1000.000000000000000 ) ;
#87288 = CARTESIAN_POINT ( 'NONE',  ( -2.867803664234999772, 1516.994127245590107, 213.7465828294170080 ) ) ;
#87289 = CARTESIAN_POINT ( 'NONE',  ( 2.458536830555473340, 1524.871836253796118, 242.3417002918415903 ) ) ;
#87290 = VERTEX_POINT ( 'NONE', #70402 ) ;
#87291 = CARTESIAN_POINT ( 'NONE',  ( -45.63712966311000230, 1440.913059426480004, 268.9747523979869470 ) ) ;
#87292 = CARTESIAN_POINT ( 'NONE',  ( 22.69876404240100243, 1522.382868172863937, 236.8953202675778869 ) ) ;
#87293 = AXIS2_PLACEMENT_3D ( 'NONE', #67353, #67903, #101451 ) ;
#87294 = CARTESIAN_POINT ( 'NONE',  ( -0.5107086395123420219, 1409.923861741519886, 233.1022952685189864 ) ) ;
#87295 = VECTOR ( 'NONE', #30623, 1000.000000000000000 ) ;
#87296 = CYLINDRICAL_SURFACE ( 'NONE', #93125, 1.000000000000076383 ) ;
#87297 = CARTESIAN_POINT ( 'NONE',  ( 0.5152534324233022378, 1421.192241663663026, 193.7244559836547353 ) ) ;
#87298 = CARTESIAN_POINT ( 'NONE',  ( -10.69735147599770109, 1462.941248850579996, 206.3316273933290006 ) ) ;
#87299 = ADVANCED_FACE ( 'NONE', ( #87170 ), #24969, .F. ) ;
#87300 = CARTESIAN_POINT ( 'NONE',  ( -28.02005516190000023, 1440.913060387330006, 248.0989693021979861 ) ) ;
#87301 = DIRECTION ( 'NONE',  ( 1.755985294532469921E-16, -1.000000000000000000, 1.338183447452831989E-16 ) ) ;
#87303 = ADVANCED_FACE ( 'NONE', ( #73701 ), #8006, .F. ) ;
#87302 = CARTESIAN_POINT ( 'NONE',  ( -12.31857035642650011, 1378.312663573310147, 209.5823498162050100 ) ) ;
#87304 = CARTESIAN_POINT ( 'NONE',  ( 26.42714720800000094, 1440.913060387330006, 243.9198229517980110 ) ) ;
#87305 = CARTESIAN_POINT ( 'NONE',  ( -10.03542548471770068, 1461.476867323560100, 210.6072180941889940 ) ) ;
#87306 = CARTESIAN_POINT ( 'NONE',  ( -14.58152186650000104, 1423.117512814019847, 196.4410428726990006 ) ) ;
#87307 = VERTEX_POINT ( 'NONE', #107827 ) ;
#87308 = CARTESIAN_POINT ( 'NONE',  ( 22.92822468965760407, 1507.593738162489899, 210.2569774338279842 ) ) ;
#87309 = CARTESIAN_POINT ( 'NONE',  ( 17.17241001986483795, 1511.187213306747708, 181.6185504016043240 ) ) ;
#87310 = CARTESIAN_POINT ( 'NONE',  ( -5.846647695999999783, 1486.134888885630062, 182.3486960385980069 ) ) ;
#87311 = CARTESIAN_POINT ( 'NONE',  ( -1.191524307911306479, 1526.382868172864164, 239.2353018730791518 ) ) ;
#87312 = CARTESIAN_POINT ( 'NONE',  ( -27.94862287022959890, 1509.902053760850094, 222.3787653423719917 ) ) ;
#87313 = CARTESIAN_POINT ( 'NONE',  ( 25.57225985780000244, 1469.240968286530006, 213.7224825415979979 ) ) ;
#87314 = EDGE_CURVE ( 'NONE', #86690, #49508, #82061, .T. ) ;
#87315 = CARTESIAN_POINT ( 'NONE',  ( -16.38987313889203534, 1420.134888794942754, 208.8825633451824331 ) ) ;
#87316 = CARTESIAN_POINT ( 'NONE',  ( -15.94609539910000073, 1509.299602945830202, 232.2985042022980053 ) ) ;
#87317 = CARTESIAN_POINT ( 'NONE',  ( -34.02204320874939469, 1383.836828112509920, 232.5604475453570217 ) ) ;
#87318 =( BOUNDED_CURVE ( )  B_SPLINE_CURVE ( 3, ( #76289, #110439, #25858, #67911 ),
 .UNSPECIFIED., .F., .T. ) 
 B_SPLINE_CURVE_WITH_KNOTS ( ( 4, 4 ),
 ( 1.009533648558965879, 2.132059403723200131 ),
 .UNSPECIFIED. ) 
 CURVE ( )  GEOMETRIC_REPRESENTATION_ITEM ( )  RATIONAL_B_SPLINE_CURVE ( ( 1.000000000000000000, 0.8977224082826531504, 0.8977224082826531504, 1.000000000000000000 ) ) 
 REPRESENTATION_ITEM ( '' )  );
#87319 = CARTESIAN_POINT ( 'NONE',  ( 20.99597493542299986, 1506.660869835769972, 226.0298841686729929 ) ) ;
#87320 = CARTESIAN_POINT ( 'NONE',  ( 2.499940070885770194, 1420.000201147749976, 104.0331098325849979 ) ) ;
#87321 = DIRECTION ( 'NONE',  ( -0.6736849260863841948, 0.000000000000000000, 0.7390186874254148774 ) ) ;
#87322 = CARTESIAN_POINT ( 'NONE',  ( 0.1645172808354759819, 1483.564749894839906, 181.9412502021760076 ) ) ;
#87324 = ORIENTED_EDGE ( 'NONE', *, *, #72662, .F. ) ;
#87323 = CARTESIAN_POINT ( 'NONE',  ( 3.916630911069999943, 1442.176737572990078, 217.0733355794490080 ) ) ;
#87325 = DIRECTION ( 'NONE',  ( 0.02615379780595215864, -0.9996573249755578150, -0.001100673901560477895 ) ) ;
#87326 = CARTESIAN_POINT ( 'NONE',  ( -9.376059709543110700E-16, 1379.808971210409936, 214.0914956899389949 ) ) ;
#87327 = CARTESIAN_POINT ( 'NONE',  ( -20.59469742430000139, 1507.767255104930200, 190.2244918928979871 ) ) ;
#87329 = VERTEX_POINT ( 'NONE', #22686 ) ;
#87328 = FACE_OUTER_BOUND ( 'NONE', #875, .T. ) ;
#87330 = CARTESIAN_POINT ( 'NONE',  ( -6.473263611634259895, 1508.551704408380147, 219.3223280905850174 ) ) ;
#87331 = EDGE_LOOP ( 'NONE', ( #32167, #82064, #6528, #91002 ) ) ;
#87332 = CARTESIAN_POINT ( 'NONE',  ( -14.34064265566260055, 1380.320133270729912, 209.7503807163919873 ) ) ;
#87333 = CARTESIAN_POINT ( 'NONE',  ( -17.48265376240000180, 1415.426210663629945, 209.4361207452480187 ) ) ;
#87334 = CARTESIAN_POINT ( 'NONE',  ( 11.50644271998659285, 1425.933145223276142, 139.0407033083927786 ) ) ;
#87335 = CARTESIAN_POINT ( 'NONE',  ( 7.066689964004210012, 1470.190416163020245, 190.3198042189900150 ) ) ;
#87336 = CARTESIAN_POINT ( 'NONE',  ( -14.96589995520845129, 1420.088422609285089, 212.9477210871714874 ) ) ;
#87337 = CARTESIAN_POINT ( 'NONE',  ( -10.78537409608540010, 1471.596790556679935, 206.8701440394590065 ) ) ;
#87338 = CARTESIAN_POINT ( 'NONE',  ( 14.93195572412279937, 1409.434495771229876, 208.8832241306849937 ) ) ;
#87339 = CARTESIAN_POINT ( 'NONE',  ( -11.89096413900000115, 1391.913060356950155, 208.7476111290540075 ) ) ;
#87340 = CARTESIAN_POINT ( 'NONE',  ( -98.26796998229559676, 1385.216402604680070, 295.9131571092459581 ) ) ;
#87341 = ADVANCED_FACE ( 'NONE', ( #22133 ), #42202, .F. ) ;
#87342 = CARTESIAN_POINT ( 'NONE',  ( -17.09359705219999981, 1424.173446424729946, 191.3645022196980108 ) ) ;
#87343 = CARTESIAN_POINT ( 'NONE',  ( -63.89205165820000332, 1379.749420737849960, 270.3321189449590065 ) ) ;
#87344 = EDGE_LOOP ( 'NONE', ( #45455, #58929, #56971 ) ) ;
#87345 = CARTESIAN_POINT ( 'NONE',  ( 12.03443371747400015, 1491.353303888329947, 206.6665118833500117 ) ) ;
#87347 = ORIENTED_EDGE ( 'NONE', *, *, #104128, .F. ) ;
#87346 = CARTESIAN_POINT ( 'NONE',  ( -2.210067589258040144, 1438.358026146749808, 227.5735626261489983 ) ) ;
#87348 = DIRECTION ( 'NONE',  ( 0.9455185755993178454, 0.000000000000000000, -0.3255681544571539243 ) ) ;
#87349 = ORIENTED_EDGE ( 'NONE', *, *, #85252, .T. ) ;
#87350 = ADVANCED_FACE ( 'NONE', ( #34973 ), #26569, .T. ) ;
#87351 = CARTESIAN_POINT ( 'NONE',  ( -18.43163825505950015, 1441.474363498949970, 212.3696370042599995 ) ) ;
#87352 = CARTESIAN_POINT ( 'NONE',  ( -0.7212203791732667568, 1361.603923786195764, 210.6218459617142003 ) ) ;
#87353 = CARTESIAN_POINT ( 'NONE',  ( -11.73858749130000056, 1433.859640885310228, 151.0726002451980037 ) ) ;
#87354 = CARTESIAN_POINT ( 'NONE',  ( 29.48235791214129620, 1509.960495255634896, 211.9272200838070717 ) ) ;
#87355 = CARTESIAN_POINT ( 'NONE',  ( -33.82780500856123496, 1523.429859730330918, 220.5611772381400328 ) ) ;
#87356 = CARTESIAN_POINT ( 'NONE',  ( 1.244907802569999999, 1397.637435234229997, 222.1288968301979878 ) ) ;
#87357 = CARTESIAN_POINT ( 'NONE',  ( 32.13439773946879541, 1525.163527997504389, 201.2154464867858792 ) ) ;
#87358 = CARTESIAN_POINT ( 'NONE',  ( -6.056985123442561125, 1516.746171222724342, 213.5452912592785424 ) ) ;
#87359 = CARTESIAN_POINT ( 'NONE',  ( -1.200783037039999890, 1471.157679959530014, 182.7924989298979881 ) ) ;
#87360 = CARTESIAN_POINT ( 'NONE',  ( -5.728941678023104167, 1370.586255878621841, 208.3718459617010978 ) ) ;
#87361 = CARTESIAN_POINT ( 'NONE',  ( -18.34590456075780196, 1416.851343895820037, 208.8605686865189739 ) ) ;
#87362 = CARTESIAN_POINT ( 'NONE',  ( 21.33070998324595280, 1509.431296620648936, 227.6602567490701574 ) ) ;
#87363 = B_SPLINE_CURVE_WITH_KNOTS ( 'NONE', 5,
 ( #35896, #61127, #11252, #86836, #43739, #35330 ),
 .UNSPECIFIED., .F., .F.,
 ( 6, 6 ),
 ( 0.000000000000000000, 1.000000000000000000 ),
 .UNSPECIFIED. ) ;
#87364 = CARTESIAN_POINT ( 'NONE',  ( -3.269184946495000244, 1516.940296199220029, 206.8376465686969823 ) ) ;
#87365 = AXIS2_PLACEMENT_3D ( 'NONE', #26047, #93271, #60240 ) ;
#87366 = CARTESIAN_POINT ( 'NONE',  ( -2.493583506516910298, 1524.152349020271004, 175.5218085340932532 ) ) ;
#87367 = CARTESIAN_POINT ( 'NONE',  ( -15.91482500274329936, 1418.747949750289990, 226.9705446459220184 ) ) ;
#87368 = CARTESIAN_POINT ( 'NONE',  ( 19.90544086846439953, 1485.367507128069974, 226.9947249633279966 ) ) ;
#87371 = ORIENTED_EDGE ( 'NONE', *, *, #80486, .F. ) ;
#87370 = CARTESIAN_POINT ( 'NONE',  ( -1.029855757680000039, 1496.295066548290151, 221.0588599254990072 ) ) ;
#87369 = AXIS2_PLACEMENT_3D ( 'NONE', #92315, #58187, #23991 ) ;
#87372 = CARTESIAN_POINT ( 'NONE',  ( 12.84239221398829933, 1435.935692713660046, 150.8114773724069835 ) ) ;
#87373 = ORIENTED_EDGE ( 'NONE', *, *, #68587, .T. ) ;
#87374 = VECTOR ( 'NONE', #29849, 1000.000000000000114 ) ;
#87375 = CARTESIAN_POINT ( 'NONE',  ( 43.15848742349999867, 1435.559015236269943, 263.9122469287980266 ) ) ;
#87376 = CARTESIAN_POINT ( 'NONE',  ( -27.25446695549999987, 1488.690170598729765, 207.9119471468479787 ) ) ;
#87378 = CARTESIAN_POINT ( 'NONE',  ( 17.10041881072790204, 1410.877218605189910, 192.0891696896890153 ) ) ;
#87377 = CARTESIAN_POINT ( 'NONE',  ( -11.03966253259999952, 1426.925357892029979, 93.54906076669780646 ) ) ;
#87379 = CARTESIAN_POINT ( 'NONE',  ( -7.709681306425000713, 1516.559109716219837, 211.9945464874270158 ) ) ;
#87380 = CARTESIAN_POINT ( 'NONE',  ( 2.811464099758409940, 1396.011238877079904, 198.4687896839119787 ) ) ;
#87381 = CARTESIAN_POINT ( 'NONE',  ( -20.51078616439999891, 1453.154034703630032, 207.5895588249879893 ) ) ;
#87382 = CARTESIAN_POINT ( 'NONE',  ( -29.79081509929999783, 1435.029579668969973, 240.1465591147980092 ) ) ;
#87383 = CARTESIAN_POINT ( 'NONE',  ( -0.9775750227080020061, 1486.139233187990158, 221.0121526945989672 ) ) ;
#87384 = CARTESIAN_POINT ( 'NONE',  ( 28.81018896693269582, 1509.453431478040102, 209.5184652127150002 ) ) ;
#87385 = DIRECTION ( 'NONE',  ( 5.980589973904019347E-17, -1.000000000000000000, 1.736889445713099699E-16 ) ) ;
#87386 = CARTESIAN_POINT ( 'NONE',  ( 32.75710557470000595, 1451.313526626729981, 135.9801501586979953 ) ) ;
#87387 = ORIENTED_EDGE ( 'NONE', *, *, #26492, .F. ) ;
#87388 = CARTESIAN_POINT ( 'NONE',  ( 11.07094430326320023, 1396.299666280629935, 213.3550120317470089 ) ) ;
#87389 = CARTESIAN_POINT ( 'NONE',  ( 10.47311736184310149, 1460.984455949540006, 208.2454930404500146 ) ) ;
#87390 = CARTESIAN_POINT ( 'NONE',  ( 1.842962231260000028, 1515.064792882589927, 204.7923971856590128 ) ) ;
#87391 = ORIENTED_EDGE ( 'NONE', *, *, #77426, .F. ) ;
#87392 = VERTEX_POINT ( 'NONE', #83725 ) ;
#87393 = CARTESIAN_POINT ( 'NONE',  ( 10.21177956804319997, 1453.436188331060066, 212.0248552912580067 ) ) ;
#87394 = CARTESIAN_POINT ( 'NONE',  ( 7.276655529890000196, 1423.040021778160053, 195.5065388737989736 ) ) ;
#87395 = ORIENTED_EDGE ( 'NONE', *, *, #42858, .T. ) ;
#87396 = CARTESIAN_POINT ( 'NONE',  ( -17.27558692971449972, 1507.606285623229951, 224.2552697136770234 ) ) ;
#87397 = AXIS2_PLACEMENT_3D ( 'NONE', #39600, #82703, #74326 ) ;
#87398 = CARTESIAN_POINT ( 'NONE',  ( 8.683531591982326603, 1446.645667073313916, 153.8370100282342037 ) ) ;
#87399 = CYLINDRICAL_SURFACE ( 'NONE', #86891, 2.000000000000002220 ) ;
#87400 = CARTESIAN_POINT ( 'NONE',  ( 2.038646110889675178, 1525.960063244516959, 241.1857569150893994 ) ) ;
#87401 = CARTESIAN_POINT ( 'NONE',  ( 7.508704985173280555, 1508.884117426920056, 203.6086456676949865 ) ) ;
#87402 = CARTESIAN_POINT ( 'NONE',  ( 9.235753568799740520, 1451.320621426679963, 209.8280334265319880 ) ) ;
#87403 = CARTESIAN_POINT ( 'NONE',  ( -11.87928044310000075, 1391.913060387289988, 209.7224407804460213 ) ) ;
#87404 = CARTESIAN_POINT ( 'NONE',  ( 14.95878199090000038, 1496.663429984430195, 225.9504587705980043 ) ) ;
#87405 = EDGE_LOOP ( 'NONE', ( #35504, #38190 ) ) ;
#87406 = CARTESIAN_POINT ( 'NONE',  ( 6.552897366944999469, 1516.858146885269889, 202.5651945608169910 ) ) ;
#87407 = CARTESIAN_POINT ( 'NONE',  ( -2.865636847234999784, 1516.815173273089840, 210.2578502442970318 ) ) ;
#87408 = ORIENTED_EDGE ( 'NONE', *, *, #68595, .F. ) ;
#87409 = CARTESIAN_POINT ( 'NONE',  ( 11.86409049007759897, 1432.195540099199889, 149.9805507428490046 ) ) ;
#87410 = CARTESIAN_POINT ( 'NONE',  ( 12.89309554127431667, 1444.938028831528982, 186.7183914381823513 ) ) ;
#87411 = ORIENTED_EDGE ( 'NONE', *, *, #20788, .F. ) ;
#87412 = CARTESIAN_POINT ( 'NONE',  ( -15.57930627156463288, 1506.606278688346947, 193.4080148037165827 ) ) ;
#87413 = FACE_OUTER_BOUND ( 'NONE', #76349, .T. ) ;
#87414 = CARTESIAN_POINT ( 'NONE',  ( 10.98671988040000080, 1508.791612297629854, 234.6950353958980031 ) ) ;
#87415 = CARTESIAN_POINT ( 'NONE',  ( -9.185273275535660531, 1469.775230892159925, 215.0640531001920124 ) ) ;
#87416 = CARTESIAN_POINT ( 'NONE',  ( -5.851186079629999703, 1425.133448028729845, 186.4975221530980036 ) ) ;
#87417 = CARTESIAN_POINT ( 'NONE',  ( 3.081956807038389812, 1409.860509536320251, 270.0718037183509637 ) ) ;
#87418 = CARTESIAN_POINT ( 'NONE',  ( -11.60004869885203682, 1428.983126981193436, 137.0999999980979851 ) ) ;
#87419 = CARTESIAN_POINT ( 'NONE',  ( -5.693467891879999243, 1475.871200527190013, 200.4602000259690158 ) ) ;
#87420 = CARTESIAN_POINT ( 'NONE',  ( 10.21325682510000021, 1491.315150049489830, 213.3055097826090218 ) ) ;
#87421 = CARTESIAN_POINT ( 'NONE',  ( -18.83042350510000063, 1379.621298762690003, 208.9674219452180068 ) ) ;
#87422 = CARTESIAN_POINT ( 'NONE',  ( 9.651063919191019025, 1425.440657924460083, 195.4941620015079877 ) ) ;
#87424 = CYLINDRICAL_SURFACE ( 'NONE', #74406, 2.000000000000003553 ) ;
#87423 = CARTESIAN_POINT ( 'NONE',  ( -16.27918300179999989, 1504.249498869590070, 208.8571777317940246 ) ) ;
#87425 = CARTESIAN_POINT ( 'NONE',  ( 11.07149624271129973, 1422.788788392120068, 206.9676479960040183 ) ) ;
#87426 = CARTESIAN_POINT ( 'NONE',  ( -9.942063362116220659, 1439.630728003020067, 208.0683743633950087 ) ) ;
#87427 = CARTESIAN_POINT ( 'NONE',  ( -6.383820993025000057, 1512.069761553100079, 200.7506179303370288 ) ) ;
#87428 = ORIENTED_EDGE ( 'NONE', *, *, #13471, .F. ) ;
#87429 = CARTESIAN_POINT ( 'NONE',  ( 6.092217268310000655, 1412.362567999629846, 265.6112251771979800 ) ) ;
#87430 = VECTOR ( 'NONE', #19907, 1000.000000000000000 ) ;
#87431 = CARTESIAN_POINT ( 'NONE',  ( 13.76344037756659944, 1434.978125283600093, 148.5738572365669938 ) ) ;
#87432 = B_SPLINE_SURFACE_WITH_KNOTS ( 'NONE', 5, 5, ( 
 ( #58026, #92161, #15434, #25487, #15981, #42873 ),
 ( #24926, #26034, #110066, #77576, #7056, #85395 ),
 ( #75914, #51262, #8143, #41212, #42309, #884 ),
 ( #109521, #8692, #66438, #32797, #66981, #24391 ),
 ( #336, #7601, #58576, #34463, #92704, #76463 ),
 ( #60228, #17625, #59678, #50182, #41755, #102739 ),
 ( #33342, #67537, #101637, #59136, #93790, #45100 ),
 ( #70311, #52936, #1418, #62462, #88736, #69188 ),
 ( #27171, #37228, #52393, #86516, #88186, #63025 ),
 ( #11478, #78114, #60797, #79793, #104424, #87072 ),
 ( #26601, #2548, #10358, #78675, #80334, #20399 ),
 ( #94923, #18742, #70866, #79240, #12019, #3098 ),
 ( #18196, #71424, #9809, #105540, #54059, #53493 ),
 ( #35558, #45654, #19293, #69753, #97130, #28827 ),
 ( #54604, #103871, #46200, #27717, #35007, #103294 ),
 ( #36673, #43975, #61356, #95475, #44530, #104978 ),
 ( #1992, #96584, #61904, #36127, #96021, #87638 ),
 ( #10924, #28268, #19856, #65194, #98771, #97675 ),
 ( #57359, #99860, #37780, #99306, #91483, #12571 ),
 ( #106081, #22033, #14208, #21489, #72490, #82537 ),
 ( #13638, #47827, #74148, #65742, #5267, #29905 ),
 ( #3651, #38311, #106619, #90922, #63560, #64098 ),
 ( #48394, #98219, #56784, #5832, #14762, #23157 ),
 ( #71969, #22580, #73599, #4178, #55701, #46751 ),
 ( #39422, #29359, #108279, #31014, #107729, #31566 ),
 ( #39973, #48950, #20947, #55153, #89274, #80882 ),
 ( #89822, #13094, #47278, #81961, #81401, #4713 ) ),
 .UNSPECIFIED., .F., .F., .F.,
 ( 6, 3, 3, 3, 3, 3, 3, 3, 6 ),
 ( 6, 6 ),
 ( 0.000000000000000000, 1.995983313780000046, 2.887652819479999966, 3.183319327139999988, 3.726393308010000016, 4.077147875629999696, 4.748093181249999795, 5.511025199249999673, 7.372157449769999538 ),
 ( 0.000000000000000000, 2.000000000000000000 ),
 .UNSPECIFIED. ) ;
#87433 = CARTESIAN_POINT ( 'NONE',  ( 40.04386419106696593, 1448.778254206540169, 134.9801842265818550 ) ) ;
#87434 = B_SPLINE_CURVE_WITH_KNOTS ( 'NONE', 5,
 ( #21569, #98294, #30542, #39502, #72037, #73676, #106153, #29432, #28342 ),
 .UNSPECIFIED., .F., .F.,
 ( 6, 3, 6 ),
 ( 462.9758374870000353, 468.8934854820000169, 473.4384810120000111 ),
 .UNSPECIFIED. ) ;
#87435 = DIRECTION ( 'NONE',  ( -0.000000000000000000, -1.000000000000000000, -0.000000000000000000 ) ) ;
#87436 = CARTESIAN_POINT ( 'NONE',  ( 0.000000000000000000, 1518.913060387330006, 209.1218459616979999 ) ) ;
#87438 = ORIENTED_EDGE ( 'NONE', *, *, #6690, .F. ) ;
#87437 = CARTESIAN_POINT ( 'NONE',  ( -1.351910739713730214, 1515.082829241050149, 204.7928694849069871 ) ) ;
#87439 = CARTESIAN_POINT ( 'NONE',  ( -15.88445676962039599, 1415.959459656937725, 209.7365985937010180 ) ) ;
#87440 = CARTESIAN_POINT ( 'NONE',  ( -24.16388973340000135, 1443.918222318679909, 212.4831360045579913 ) ) ;
#87441 = CARTESIAN_POINT ( 'NONE',  ( -2.016955699854175776, 1450.205627335352347, 154.3312174505059033 ) ) ;
#87442 = CARTESIAN_POINT ( 'NONE',  ( -1.040347359575360064, 1429.922094406420001, 199.7824833409709981 ) ) ;
#87443 = FACE_OUTER_BOUND ( 'NONE', #10668, .T. ) ;
#87444 = CARTESIAN_POINT ( 'NONE',  ( 3.297000113654319886, 1370.245087421812514, 208.0695929694545043 ) ) ;
#87445 = CARTESIAN_POINT ( 'NONE',  ( 19.28837017967479994, 1509.586622668500013, 231.7115921283199782 ) ) ;
#87446 = B_SPLINE_CURVE_WITH_KNOTS ( 'NONE', 3,
 ( #3007, #69101, #20311, #27085, #95385, #52299, #87546, #70227, #54514, #78584, #786, #35471, #103784, #69661, #1331, #97048, #36037, #34916, #104332, #88651, #10836, #26508, #79150, #53969, #94827, #53397, #103203, #27625, #96487, #71329, #61270, #11389, #18649, #88102, #60703, #105442, #11928 ),
 .UNSPECIFIED., .F., .F.,
 ( 4, 3, 3, 3, 3, 3, 3, 3, 3, 3, 3, 3, 4 ),
 ( -12.92009077346300039, -12.71598438484270055, -12.02692291841409933, -11.29816837385320127, -10.53156648978099952, -9.713214318400439140, -8.755060695329159870, -7.805279224055939657, -7.050688516310069431, -6.129046816252760266, -5.323559768139629611, -4.615615438122199876, -3.948767879309999174 ),
 .UNSPECIFIED. ) ;
#87447 = DIRECTION ( 'NONE',  ( 0.000000000000000000, 0.000000000000000000, 1.000000000000000000 ) ) ;
#87448 = CARTESIAN_POINT ( 'NONE',  ( 11.99684948639972859, 1433.670360444001972, 149.8496142774944531 ) ) ;
#87449 = CARTESIAN_POINT ( 'NONE',  ( 13.18956788129999858, 1412.740670877530192, 228.5450254855980177 ) ) ;
#87450 = CARTESIAN_POINT ( 'NONE',  ( 9.934261248579540293, 1469.591094200070074, 210.6863934935470013 ) ) ;
#87451 = CARTESIAN_POINT ( 'NONE',  ( -15.74154664829999994, 1459.394320478729924, 230.7248325767979793 ) ) ;
#87453 = AXIS2_PLACEMENT_3D ( 'NONE', #87507, #46621, #10796 ) ;
#87452 = CARTESIAN_POINT ( 'NONE',  ( 3.445685077385000294, 1516.778761582560037, 206.6297153089269898 ) ) ;
#87454 = CARTESIAN_POINT ( 'NONE',  ( 41.47797487389999560, 1425.138039607129713, 268.3622462469979837 ) ) ;
#87455 = CARTESIAN_POINT ( 'NONE',  ( -33.17484411121681376, 1525.713797967456912, 217.3801513758764088 ) ) ;
#87456 = CARTESIAN_POINT ( 'NONE',  ( 13.80545266760000089, 1434.979654225609920, 148.5370281251980202 ) ) ;
#87457 = CIRCLE ( 'NONE', #39148, 1.000002395376709652 ) ;
#87459 = B_SPLINE_CURVE_WITH_KNOTS ( 'NONE', 5,
 ( #2237, #64334, #88417, #28509, #62710, #53751 ),
 .UNSPECIFIED., .F., .F.,
 ( 6, 6 ),
 ( 0.000000000000000000, 1.000000000000000000 ),
 .UNSPECIFIED. ) ;
#87458 = CARTESIAN_POINT ( 'NONE',  ( 20.44074684259999941, 1488.586588146029953, 191.1769514407980068 ) ) ;
#87460 = CARTESIAN_POINT ( 'NONE',  ( -21.80812349030000163, 1430.398269787930076, 219.2188554248980097 ) ) ;
#87461 = EDGE_CURVE ( 'NONE', #19417, #55990, #76987, .T. ) ;
#87462 = TOROIDAL_SURFACE ( 'NONE', #19412, 21.40691501530000096, 1.500287545629999997 ) ;
#87463 = CARTESIAN_POINT ( 'NONE',  ( 0.03697543579222300342, 1507.626287098129751, 237.3745122006210124 ) ) ;
#87464 = CARTESIAN_POINT ( 'NONE',  ( -16.30647051440000084, 1418.357332664029855, 226.9584847186979744 ) ) ;
#87465 = CARTESIAN_POINT ( 'NONE',  ( -15.46123378547330063, 1418.179543175669778, 203.0721989172009785 ) ) ;
#87466 = CARTESIAN_POINT ( 'NONE',  ( -41.44601667217140317, 1442.603978534169983, 136.4469555575219886 ) ) ;
#87467 = CARTESIAN_POINT ( 'NONE',  ( -13.04207679966010147, 1409.368499744919745, 225.9431846064669855 ) ) ;
#87468 = CARTESIAN_POINT ( 'NONE',  ( -15.89311463129999780, 1416.118927280270100, 209.3720684979659836 ) ) ;
#87469 = CARTESIAN_POINT ( 'NONE',  ( -12.73158637370000079, 1442.742385989480226, 186.8996798116980074 ) ) ;
#87470 = ADVANCED_FACE ( 'NONE', ( #110582 ), #88655, .F. ) ;
#87471 = CARTESIAN_POINT ( 'NONE',  ( -27.78496691744659941, 1508.044397529670050, 210.4698789973389808 ) ) ;
#87472 = CARTESIAN_POINT ( 'NONE',  ( -31.77787458389999387, 1435.606731000560103, 135.5694218124980068 ) ) ;
#87473 = DIRECTION ( 'NONE',  ( 0.000000000000000000, 1.000000000000000000, 0.000000000000000000 ) ) ;
#87474 = ORIENTED_EDGE ( 'NONE', *, *, #37831, .T. ) ;
#87475 = DIRECTION ( 'NONE',  ( 0.000000000000000000, 0.000000000000000000, -1.000000000000000000 ) ) ;
#87476 = CARTESIAN_POINT ( 'NONE',  ( -14.87542623989530099, 1409.432521718130147, 207.7979172480029888 ) ) ;
#87477 = CARTESIAN_POINT ( 'NONE',  ( -5.494437299350000359, 1439.687232799670255, 154.7535679683980163 ) ) ;
#87478 = CARTESIAN_POINT ( 'NONE',  ( -34.77865709046010778, 1512.187213306747481, 191.3609956664894014 ) ) ;
#87479 = B_SPLINE_CURVE_WITH_KNOTS ( 'NONE', 3,
 ( #52910, #35532, #8661, #26004, #69726, #17598, #104396, #70842 ),
 .UNSPECIFIED., .F., .F.,
 ( 4, 2, 2, 4 ),
 ( 2.428612866367529932E-17, 0.001073044933456048563, 0.001609567400184060701, 0.002146089866912072840 ),
 .UNSPECIFIED. ) ;
#87480 = CARTESIAN_POINT ( 'NONE',  ( -44.60802269250000052, 1451.081273266829839, 268.7932458390980059 ) ) ;
#87482 = VECTOR ( 'NONE', #27331, 1000.000000000000114 ) ;
#87481 = CARTESIAN_POINT ( 'NONE',  ( -30.00389853323245148, 1524.843416604514459, 195.9693362516085244 ) ) ;
#87483 = CARTESIAN_POINT ( 'NONE',  ( 0.1826205922680210203, 1420.410877725119917, 183.2589509447180092 ) ) ;
#87484 = CARTESIAN_POINT ( 'NONE',  ( -26.88785758550000082, 1509.181462003529987, 214.1987029181680100 ) ) ;
#87485 = CARTESIAN_POINT ( 'NONE',  ( -66.72900126439060386, 1384.672153193259874, 291.0917829019970213 ) ) ;
#87486 = CARTESIAN_POINT ( 'NONE',  ( -29.54457669783570140, 1384.967922959629959, 205.3221292075180031 ) ) ;
#87487 = CARTESIAN_POINT ( 'NONE',  ( 17.33264729495500234, 1424.042909391080002, 227.4554219137819757 ) ) ;
#87488 = CARTESIAN_POINT ( 'NONE',  ( 14.46594802229999921, 1415.931784856029935, 219.5940544748980301 ) ) ;
#87489 = CARTESIAN_POINT ( 'NONE',  ( 14.89315775630000083, 1485.046810827629997, 224.2543386747979923 ) ) ;
#87490 = CARTESIAN_POINT ( 'NONE',  ( -113.4000000000000057, 1308.913060387289988, 304.2218459572590064 ) ) ;
#87491 = CARTESIAN_POINT ( 'NONE',  ( -5.292751683389999684, 1386.092796132480089, 214.8417591471989851 ) ) ;
#87492 = CARTESIAN_POINT ( 'NONE',  ( -8.848268338060000460, 1384.931973698940055, 199.9247712804389892 ) ) ;
#87493 = CARTESIAN_POINT ( 'NONE',  ( 4.433889532992436600, 1421.449000901995305, 137.6338609017415422 ) ) ;
#87494 = CARTESIAN_POINT ( 'NONE',  ( 16.06428786779999740, 1414.913060387329779, 208.9262477901120008 ) ) ;
#87495 = CARTESIAN_POINT ( 'NONE',  ( 3.487592428934999766, 1509.038615934169911, 204.6345961781970004 ) ) ;
#87496 = CARTESIAN_POINT ( 'NONE',  ( 3.256084378020000170, 1422.858183810449873, 193.8949459527989916 ) ) ;
#87497 = CARTESIAN_POINT ( 'NONE',  ( 23.87472870330000063, 1411.107469451229917, 210.5066206584180009 ) ) ;
#87498 = CARTESIAN_POINT ( 'NONE',  ( -4.250000000000000000, 1516.051704408390151, 209.1218459616989946 ) ) ;
#87499 = CARTESIAN_POINT ( 'NONE',  ( -3.103172482810000243, 1450.690062953990036, 188.5470283436989973 ) ) ;
#87500 = CARTESIAN_POINT ( 'NONE',  ( -16.40900118989999967, 1421.678299158230175, 227.0581239876979964 ) ) ;
#87502 = CARTESIAN_POINT ( 'NONE',  ( -12.89895815099780130, 1379.435140844680063, 211.3213831571520132 ) ) ;
#87501 = DIRECTION ( 'NONE',  ( 0.000000000000000000, 0.000000000000000000, -1.000000000000000000 ) ) ;
#87503 = CARTESIAN_POINT ( 'NONE',  ( -5.277971523409999755, 1391.913060387289988, 203.7647467602490110 ) ) ;
#87504 = CARTESIAN_POINT ( 'NONE',  ( -102.9430107618170069, 1368.558218059089086, 309.9345253547082280 ) ) ;
#87505 = CARTESIAN_POINT ( 'NONE',  ( -14.87341339970349985, 1420.535920296580116, 212.2959427910559782 ) ) ;
#87506 = B_SPLINE_CURVE_WITH_KNOTS ( 'NONE', 3,
 ( #62318, #80743, #2961, #63423, #89137, #4052, #19146, #53353, #44958, #11886, #53923, #104839, #78538, #28688, #1852, #105394, #88604, #35987, #79106, #11343, #80191, #54466, #37078, #46058, #37633, #38178, #71838, #103733, #27032, #71281, #28126, #70175, #104286, #61221 ),
 .UNSPECIFIED., .F., .F.,
 ( 4, 3, 3, 3, 3, 3, 3, 3, 3, 3, 3, 4 ),
 ( 4.497076618296339975E-07, 0.8097585624606019605, 1.639511105808459934, 2.030720938957220056, 2.898872277768610228, 3.784635505398759925, 4.221522473682940202, 4.606556899451190290, 5.525126413775890200, 6.438844840059180008, 6.927804315340000407, 7.850516048179999373 ),
 .UNSPECIFIED. ) ;
#87507 = CARTESIAN_POINT ( 'NONE',  ( -32.28466283162143213, 1501.977400791986611, 219.1752493337717738 ) ) ;
#87508 = CARTESIAN_POINT ( 'NONE',  ( -3.787329988060110342, 1369.092969256073502, 210.6218459616991936 ) ) ;
#87509 = CARTESIAN_POINT ( 'NONE',  ( 0.7369041709050019318, 1517.080322339569875, 204.1102945640870132 ) ) ;
#87510 =( NAMED_UNIT ( * ) SI_UNIT ( $, .STERADIAN. ) SOLID_ANGLE_UNIT ( ) );
#87511 = CARTESIAN_POINT ( 'NONE',  ( -14.13260639439999977, 1484.576036422829930, 186.6695759715979932 ) ) ;
#87512 = FACE_OUTER_BOUND ( 'NONE', #89867, .T. ) ;
#87513 = AXIS2_PLACEMENT_3D ( 'NONE', #84563, #109773, #586 ) ;
#87514 = CARTESIAN_POINT ( 'NONE',  ( 41.48258358977700055, 1444.135548109920137, 136.5500177229649807 ) ) ;
#87516 = ORIENTED_EDGE ( 'NONE', *, *, #86530, .T. ) ;
#87515 = CARTESIAN_POINT ( 'NONE',  ( -62.61021140161710008, 1379.731611446759871, 270.6613306315579734 ) ) ;
#87517 = ORIENTED_EDGE ( 'NONE', *, *, #20118, .T. ) ;
#87518 = CARTESIAN_POINT ( 'NONE',  ( 11.74950119094600076, 1433.770027978590178, 150.9361992396719927 ) ) ;
#87519 = CARTESIAN_POINT ( 'NONE',  ( 0.07152473094740001425, 1397.597829882229917, 222.1216538301979995 ) ) ;
#87520 = VERTEX_POINT ( 'NONE', #104393 ) ;
#87521 = CARTESIAN_POINT ( 'NONE',  ( 18.97796697799407539, 1526.382868172864164, 185.2752177337489172 ) ) ;
#87522 = CARTESIAN_POINT ( 'NONE',  ( 11.01589229730000064, 1501.204512814589862, 206.0337867319090037 ) ) ;
#87524 = CARTESIAN_POINT ( 'NONE',  ( 0.1999013110879999944, 1508.573951179030018, 180.3597275294980022 ) ) ;
#87523 = CARTESIAN_POINT ( 'NONE',  ( -15.73574044604409927, 1409.462552572229924, 225.2910003602459881 ) ) ;
#87525 = CARTESIAN_POINT ( 'NONE',  ( -0.5392968480769999573, 1417.272289817929959, 235.8882545161980033 ) ) ;
#87526 = CIRCLE ( 'NONE', #82140, 0.9999999999999971134 ) ;
#87527 = CARTESIAN_POINT ( 'NONE',  ( 2.495004647950000098, 1488.172775063030031, 182.1516654459980202 ) ) ;
#87528 = CARTESIAN_POINT ( 'NONE',  ( 9.687429786604399240, 1439.765094063396873, 153.1584582019008849 ) ) ;
#87529 = CARTESIAN_POINT ( 'NONE',  ( 31.81407709660777527, 1512.187213306747481, 221.9534378623329758 ) ) ;
#87530 = FILL_AREA_STYLE_COLOUR ( '', #96873 ) ;
#87531 = PRODUCT_DEFINITION_SHAPE ( 'NONE', 'NONE',  #11756 ) ;
#87532 = CARTESIAN_POINT ( 'NONE',  ( 7.724423394095000894, 1517.122088787240045, 212.5760185856570104 ) ) ;
#87533 = CARTESIAN_POINT ( 'NONE',  ( 38.19279632128629487, 1437.094169275030026, 134.0999999969999692 ) ) ;
#87534 = DIRECTION ( 'NONE',  ( 0.8672669759446666182, -0.000000000000000000, 0.4978433412588672557 ) ) ;
#87535 = CARTESIAN_POINT ( 'NONE',  ( -15.82483088085467138, 1509.465675743439988, 234.0825299431272128 ) ) ;
#87536 = ORIENTED_EDGE ( 'NONE', *, *, #53583, .T. ) ;
#87537 = CARTESIAN_POINT ( 'NONE',  ( 14.45648542637160006, 1435.815601845680021, 149.7795650820339972 ) ) ;
#87538 = CARTESIAN_POINT ( 'NONE',  ( 0.3848239385950819602, 1432.484357106330208, 200.6930806709059993 ) ) ;
#87539 = VERTEX_POINT ( 'NONE', #29331 ) ;
#87540 = EDGE_LOOP ( 'NONE', ( #20718, #82995, #97157, #39100 ) ) ;
#87541 = ORIENTED_EDGE ( 'NONE', *, *, #10525, .F. ) ;
#87542 = CARTESIAN_POINT ( 'NONE',  ( 12.66043128553913810, 1445.026948396785428, 169.4635460886795784 ) ) ;
#87543 = CARTESIAN_POINT ( 'NONE',  ( 16.57651862990214653, 1513.029502680801215, 197.1488735994816750 ) ) ;
#87544 = FACE_OUTER_BOUND ( 'NONE', #82827, .T. ) ;
#87545 = CARTESIAN_POINT ( 'NONE',  ( -7.769368482660000019, 1384.919440823630111, 218.9178397582889772 ) ) ;
#87546 = CARTESIAN_POINT ( 'NONE',  ( -1.498494647347079933, 1465.094162369539845, 198.2212222711209790 ) ) ;
#87547 = VECTOR ( 'NONE', #20493, 1000.000000000000000 ) ;
#87548 = FACE_OUTER_BOUND ( 'NONE', #27428, .T. ) ;
#87549 = CARTESIAN_POINT ( 'NONE',  ( -57.39613275940437376, 1379.715796048977836, 255.4829930585067927 ) ) ;
#87550 = CARTESIAN_POINT ( 'NONE',  ( 4.231248707956949850, 1446.302976782659925, 164.6656280576010261 ) ) ;
#87551 = AXIS2_PLACEMENT_3D ( 'NONE', #42277, #110581, #108935 ) ;
#87552 = CARTESIAN_POINT ( 'NONE',  ( 8.583222999044879842, 1437.099971295089972, 208.1373760821520307 ) ) ;
#87553 = EDGE_LOOP ( 'NONE', ( #25798, #33091, #850, #58759, #42937 ) ) ;
#87554 = CARTESIAN_POINT ( 'NONE',  ( 1.118104729594999958, 1516.965971551240045, 206.8221779662269739 ) ) ;
#87555 = ORIENTED_EDGE ( 'NONE', *, *, #52259, .F. ) ;
#87556 = CARTESIAN_POINT ( 'NONE',  ( 33.36397945909019569, 1440.913060387330006, 258.2907522413270271 ) ) ;
#87557 = CARTESIAN_POINT ( 'NONE',  ( 11.60117971636739931, 1478.974074431269855, 207.2346898377800244 ) ) ;
#87558 = VERTEX_POINT ( 'NONE', #19824 ) ;
#87559 = CARTESIAN_POINT ( 'NONE',  ( -7.444964753889919074, 1508.731183030150078, 203.6086348057779958 ) ) ;
#87560 = CARTESIAN_POINT ( 'NONE',  ( -14.78674196459999912, 1410.361681208129994, 190.6508623267980056 ) ) ;
#87561 = CARTESIAN_POINT ( 'NONE',  ( -57.32900025239892727, 1379.717698082794413, 260.4930733565817604 ) ) ;
#87563 = CARTESIAN_POINT ( 'NONE',  ( 15.16811419108810099, 1512.319979277499897, 196.2625218158190137 ) ) ;
#87562 = FACE_OUTER_BOUND ( 'NONE', #53209, .T. ) ;
#87564 = CARTESIAN_POINT ( 'NONE',  ( 2.193121967036330222, 1423.464081223100038, 192.6388440160779965 ) ) ;
#87565 = CARTESIAN_POINT ( 'NONE',  ( 0.0002644827706587799215, 1396.374078736850834, 196.8444724510774222 ) ) ;
#87566 = CARTESIAN_POINT ( 'NONE',  ( -803.2235323108749299, 1451.575432553050177, 209.0911897361090155 ) ) ;
#87567 = CARTESIAN_POINT ( 'NONE',  ( -12.91292777029999961, 1434.774376582520063, 149.2723726445979935 ) ) ;
#87568 = CARTESIAN_POINT ( 'NONE',  ( -7.756964262599999493, 1508.430205954690109, 219.4938836478990254 ) ) ;
#87570 = DIRECTION ( 'NONE',  ( 0.9076061524720596685, 1.962993793439040551E-32, -0.4198226673190293412 ) ) ;
#87569 = CARTESIAN_POINT ( 'NONE',  ( 2.824784936839999983, 1465.895815560630126, 234.2053348773979735 ) ) ;
#87571 = AXIS2_PLACEMENT_3D ( 'NONE', #72773, #59157, #39141 ) ;
#87572 = B_SPLINE_SURFACE_WITH_KNOTS ( 'NONE', 5, 5, ( 
 ( #62672, #20063, #21140, #87851, #29034, #63219 ),
 ( #12212, #53713, #80540, #3855, #37982, #72164 ),
 ( #106281, #55347, #29567, #11139, #96039, #85412 ),
 ( #77593, #43443, #85983, #70884, #9826, #8711 ),
 ( #62482, #61371, #87655, #42889, #52954, #26620 ),
 ( #60816, #104441, #78129, #18211, #354, #10373 ) ),
 .UNSPECIFIED., .F., .F., .F.,
 ( 6, 6 ),
 ( 6, 6 ),
 ( 8.878996031149998913, 11.86168502449999984 ),
 ( 0.000000000000000000, 1.459712257500000110 ),
 .UNSPECIFIED. ) ;
#87573 = CARTESIAN_POINT ( 'NONE',  ( 2.295485501044999932, 1516.651306816259876, 214.1175719399469983 ) ) ;
#87574 = CARTESIAN_POINT ( 'NONE',  ( 11.43741207009999883, 1425.481177415629872, 144.1677667564979970 ) ) ;
#87575 = CARTESIAN_POINT ( 'NONE',  ( 6.003588533468550814, 1511.304111283970087, 216.7919996258230242 ) ) ;
#87576 = CARTESIAN_POINT ( 'NONE',  ( 30.98807061075474323, 1524.600389084707103, 221.8038906437711262 ) ) ;
#87577 = CARTESIAN_POINT ( 'NONE',  ( 6.950214933285000285, 1517.129577905929864, 211.9934263588270085 ) ) ;
#87578 = CARTESIAN_POINT ( 'NONE',  ( -21.31156959599999823, 1488.809466529130077, 209.0743529571010129 ) ) ;
#87579 = CARTESIAN_POINT ( 'NONE',  ( -17.25653015495222675, 1486.135578907454601, 187.8878648081120559 ) ) ;
#87581 = EDGE_LOOP ( 'NONE', ( #57409, #33332, #106662, #16425 ) ) ;
#87580 = CARTESIAN_POINT ( 'NONE',  ( -92.73157688390000430, 1386.757379292640053, 294.2674297909590564 ) ) ;
#87582 = CARTESIAN_POINT ( 'NONE',  ( -16.92737646175572763, 1525.317359687823455, 236.7941014278637226 ) ) ;
#87583 = AXIS2_PLACEMENT_3D ( 'NONE', #24794, #58999, #93127 ) ;
#87584 = CARTESIAN_POINT ( 'NONE',  ( 22.60664681420000122, 1452.395138154029837, 225.7920039562980037 ) ) ;
#87585 = CARTESIAN_POINT ( 'NONE',  ( 6.644648847156787497, 1485.119973938482872, 217.5961942112708982 ) ) ;
#87586 = CARTESIAN_POINT ( 'NONE',  ( -16.67046855446390197, 1516.551188146170034, 196.0483986024819956 ) ) ;
#87587 = CARTESIAN_POINT ( 'NONE',  ( -7.840274410260001048, 1507.896958070730079, 235.4362243845980061 ) ) ;
#87588 = CARTESIAN_POINT ( 'NONE',  ( -21.79827285660000058, 1452.321708545830006, 222.0267583476980064 ) ) ;
#87589 = B_SPLINE_CURVE_WITH_KNOTS ( 'NONE', 3,
 ( #6473, #7021, #101063, #15405, #22135, #82636, #57996, #100525, #24359, #31665, #39527, #14857, #82063, #48496, #7572, #23804, #33310, #73702, #32227, #23257, #67504, #40623, #49047, #57456, #58545, #84278, #107828, #65846, #41179, #5927, #14306, #5368, #40073, #66407, #56335, #74794, #108384, #50149, #108938, #92130, #74253, #32769, #56887, #31116, #99408, #13743, #49594, #90467, #91583, #83726, #99965, #83184, #75353, #92671, #15948, #22688, #91017, #41726, #75886, #110036, #47927, #69724, #76997, #87039, #26570, #110583, #101608, #51231, #60766, #69157, #103843 ),
 .UNSPECIFIED., .F., .F.,
 ( 4, 2, 2, 2, 1, 1, 1, 1, 1, 2, 2, 2, 2, 2, 1, 1, 1, 1, 1, 1, 1, 2, 2, 2, 2, 2, 2, 2, 1, 1, 1, 1, 2, 2, 2, 2, 2, 1, 1, 1, 1, 1, 2, 2, 2, 4 ),
 ( 0.000000000000000000, 0.1250000000075510986, 0.1875000000113273835, 0.2187500000132166778, 0.2343750000141613110, 0.2421875000146322121, 0.2460937500148676349, 0.2480468750149853463, 0.2490234375150427171, 0.2495117187650713608, 0.2500000000151000323, 0.3750000000222334373, 0.4375000000258001953, 0.4687500000275862111, 0.4843750000284820501, 0.4921875000289330226, 0.4960937500291585645, 0.4980468750292713631, 0.4990234375293277069, 0.4995117187793529090, 0.4997558594043624014, 0.4998779297168672309, 0.5000000000293720603, 0.5312500000262170285, 0.5625000000230618857, 0.5937500000199068539, 0.6093750000183260074, 0.6171875000175328640, 0.6210937500171362924, 0.6230468750169378955, 0.6240234375168386416, 0.6245117187667917902, 0.6247558593917682535, 0.6250000000167448277, 0.6875000000123349109, 0.7187500000101351150, 0.7343750000090352170, 0.7421875000084852125, 0.7460937500082102103, 0.7480468750080800922, 0.7490234375080077056, 0.7495117187579714013, 0.7497558593829608542, 0.7500000000079501961, 0.8750000000039751535, 1.000000000000000000 ),
 .UNSPECIFIED. ) ;
#87591 = CARTESIAN_POINT ( 'NONE',  ( 17.97731455220759855, 1410.660655195440086, 222.9643864582139940 ) ) ;
#87590 = CARTESIAN_POINT ( 'NONE',  ( 11.57799745920000056, 1432.441881432899891, 151.1964746161979747 ) ) ;
#87592 = CARTESIAN_POINT ( 'NONE',  ( -8.621728156553459144, 1448.683718559020008, 212.1725994164930000 ) ) ;
#87593 = CARTESIAN_POINT ( 'NONE',  ( -104.9983700835409905, 1380.418911759009916, 307.4638771597370237 ) ) ;
#87594 = EDGE_LOOP ( 'NONE', ( #95519, #7348, #91600, #47044 ) ) ;
#87595 = CARTESIAN_POINT ( 'NONE',  ( -6.946748557085000719, 1516.983995446890049, 204.1186252050270014 ) ) ;
#87596 = CARTESIAN_POINT ( 'NONE',  ( 1.764049411440000048, 1406.288942863529883, 269.2935851124980218 ) ) ;
#87597 = CARTESIAN_POINT ( 'NONE',  ( 28.44685754529808719, 1526.382868172863937, 198.3690656491830850 ) ) ;
#87598 = CARTESIAN_POINT ( 'NONE',  ( 44.70565502892719678, 1446.408339148580126, 269.9105772414620219 ) ) ;
#87599 = CARTESIAN_POINT ( 'NONE',  ( 2.478937890449999681, 1432.468588061860146, 157.5195758061979916 ) ) ;
#87600 = CARTESIAN_POINT ( 'NONE',  ( -27.28327444803209900, 1449.032218191109905, 136.7238657257040018 ) ) ;
#87601 = CARTESIAN_POINT ( 'NONE',  ( -42.09825630726439272, 1440.913060411040078, 262.0793472720840214 ) ) ;
#87602 = AXIS2_PLACEMENT_3D ( 'NONE', #90665, #13393, #73333 ) ;
#87603 = CARTESIAN_POINT ( 'NONE',  ( -27.74152905169999883, 1446.393006942010061, 137.1637342961979869 ) ) ;
#87604 = CARTESIAN_POINT ( 'NONE',  ( 2.017821789106273744, 1450.204743078944830, 154.3313547465386080 ) ) ;
#87605 = DIRECTION ( 'NONE',  ( -0.9076355166982633671, -0.02210890796429692759, -0.4191765320440813958 ) ) ;
#87606 = CARTESIAN_POINT ( 'NONE',  ( 1.958645842704549889, 1450.346086676289815, 154.2463840790279903 ) ) ;
#87607 = CARTESIAN_POINT ( 'NONE',  ( -1.204685347530000117, 1506.953552699789952, 221.9093730674989899 ) ) ;
#87608 = CARTESIAN_POINT ( 'NONE',  ( -1.546896723439913135, 1416.831923553206025, 228.0210884502933482 ) ) ;
#87609 = ORIENTED_EDGE ( 'NONE', *, *, #49688, .F. ) ;
#87610 = AXIS2_PLACEMENT_3D ( 'NONE', #16285, #50489, #42076 ) ;
#87611 = CARTESIAN_POINT ( 'NONE',  ( -3.946018174590000300E-15, 1427.166763959530044, 147.9649995502979891 ) ) ;
#87612 = CARTESIAN_POINT ( 'NONE',  ( 2.067823311539999764, 1486.525342903789806, 197.7722860763989843 ) ) ;
#87613 = CARTESIAN_POINT ( 'NONE',  ( 10.56485853567840039, 1469.565006426170157, 204.9063131257589987 ) ) ;
#87614 = CARTESIAN_POINT ( 'NONE',  ( -0.2161462641430000053, 1476.049917889630024, 268.4837592950979683 ) ) ;
#87615 = CARTESIAN_POINT ( 'NONE',  ( 10.73506988043325627, 1424.972993549859893, 139.1354236083641922 ) ) ;
#87616 = CARTESIAN_POINT ( 'NONE',  ( -32.99911596133329539, 1524.244163922423695, 196.1627191131780705 ) ) ;
#87617 = CARTESIAN_POINT ( 'NONE',  ( -3.825775683770979985, 1448.295119309961819, 185.0228311757895483 ) ) ;
#87618 = CARTESIAN_POINT ( 'NONE',  ( -10.97681301304650070, 1384.887672684300014, 218.8427800890989943 ) ) ;
#87619 = CIRCLE ( 'NONE', #51882, 2.000000000015774049 ) ;
#87620 = CARTESIAN_POINT ( 'NONE',  ( -18.88752285780000051, 1416.568813549730066, 207.5747269755180184 ) ) ;
#87621 = CARTESIAN_POINT ( 'NONE',  ( -9.968894432999999111, 1482.167632919289872, 205.0619827550790149 ) ) ;
#87622 = CARTESIAN_POINT ( 'NONE',  ( 26.38682956852759887, 1435.721715954939782, 136.2459471611129800 ) ) ;
#87623 = CARTESIAN_POINT ( 'NONE',  ( -6.669055308816830063, 1396.145948930530039, 200.3212403031140241 ) ) ;
#87624 = CARTESIAN_POINT ( 'NONE',  ( -15.51029599480000165, 1420.880494488829981, 227.0363825903980057 ) ) ;
#87625 = CARTESIAN_POINT ( 'NONE',  ( -17.38485670972179875, 1410.884453452420075, 225.7833130266830040 ) ) ;
#87626 = CARTESIAN_POINT ( 'NONE',  ( 22.09302970059145821, 1509.609508200493792, 226.9617867963430058 ) ) ;
#87627 = ORIENTED_EDGE ( 'NONE', *, *, #93360, .T. ) ;
#87628 = CARTESIAN_POINT ( 'NONE',  ( -11.33396083898640860, 1502.204733694695051, 207.2924597943140270 ) ) ;
#87629 = CARTESIAN_POINT ( 'NONE',  ( 2.370746254249999740, 1409.499373740729880, 231.5443631752980025 ) ) ;
#87630 = CARTESIAN_POINT ( 'NONE',  ( 3.827053565004849833, 1515.145425758850251, 209.1218459614979963 ) ) ;
#87632 = CARTESIAN_POINT ( 'NONE',  ( -9.952950791904509487, 1438.984619552230015, 209.5724956438699849 ) ) ;
#87631 = CARTESIAN_POINT ( 'NONE',  ( 11.20602548229999940, 1425.617270592030081, 128.4886806428979753 ) ) ;
#87633 = DIRECTION ( 'NONE',  ( 1.000000000000000000, 0.000000000000000000, 0.000000000000000000 ) ) ;
#87634 = CARTESIAN_POINT ( 'NONE',  ( 1.823067188510389982E-15, 1517.051704408389924, 209.1218459616989946 ) ) ;
#87635 = EDGE_CURVE ( 'NONE', #6139, #36366, #74219, .T. ) ;
#87636 = CIRCLE ( 'NONE', #110796, 0.4999999999999980016 ) ;
#87637 = FACE_OUTER_BOUND ( 'NONE', #61344, .T. ) ;
#87638 = CARTESIAN_POINT ( 'NONE',  ( 7.998636686930000295, 1425.977676336709919, 211.5360327896089814 ) ) ;
#87639 = CARTESIAN_POINT ( 'NONE',  ( -14.87168881317970026, 1430.147188212150240, 221.8136313441650032 ) ) ;
#87640 = CARTESIAN_POINT ( 'NONE',  ( 8.991748181960000252, 1509.227061564030009, 181.2342630857980055 ) ) ;
#87641 = CARTESIAN_POINT ( 'NONE',  ( 7.883416839195001025, 1512.215430505229961, 206.1881785102070239 ) ) ;
#87642 = CARTESIAN_POINT ( 'NONE',  ( 3.932775215530000423, 1448.980695957309990, 184.2693358957980081 ) ) ;
#87643 = CARTESIAN_POINT ( 'NONE',  ( 8.123801262052971595, 1364.937873541178078, 208.3718459617061285 ) ) ;
#87645 = ORIENTED_EDGE ( 'NONE', *, *, #74798, .F. ) ;
#87644 = CARTESIAN_POINT ( 'NONE',  ( 6.455724313810000226, 1455.041435863090101, 217.0620835976089893 ) ) ;
#87646 = ORIENTED_EDGE ( 'NONE', *, *, #38173, .F. ) ;
#87647 = CARTESIAN_POINT ( 'NONE',  ( -41.14739979139999804, 1443.970064379710038, 136.9302418245979709 ) ) ;
#87648 = CARTESIAN_POINT ( 'NONE',  ( 0.8306043666373410517, 1482.868851409599984, 236.2037489664579937 ) ) ;
#87649 = CARTESIAN_POINT ( 'NONE',  ( -20.19975713530000050, 1435.203085175508932, 142.9756137166980068 ) ) ;
#87650 = CARTESIAN_POINT ( 'NONE',  ( 2.317667528355622508, 1499.011937117496473, 198.0143009028709855 ) ) ;
#87651 = CARTESIAN_POINT ( 'NONE',  ( -1.356522590142140050, 1410.335674017130032, 185.6037846924129724 ) ) ;
#87652 = CIRCLE ( 'NONE', #52, 12.50000000000001066 ) ;
#87653 = CARTESIAN_POINT ( 'NONE',  ( -31.32941717379338797, 1525.856064936177972, 201.1886153483195301 ) ) ;
#87654 = PRESENTATION_STYLE_ASSIGNMENT (( #97147 ) ) ;
#87655 = CARTESIAN_POINT ( 'NONE',  ( 22.04779549230000057, 1409.847308075230103, 206.6119095045879988 ) ) ;
#87656 = CARTESIAN_POINT ( 'NONE',  ( -2.500000000000000000, 1448.261011210099923, 165.3792834674099765 ) ) ;
#87657 = CARTESIAN_POINT ( 'NONE',  ( 8.407436659505169274, 1396.206654546769869, 216.2971811410959901 ) ) ;
#87658 = CARTESIAN_POINT ( 'NONE',  ( 14.64909617470000214, 1409.247894962230021, 212.1421858282079711 ) ) ;
#87659 = CARTESIAN_POINT ( 'NONE',  ( -2.295142876860809977, 1406.025848543300071, 266.9592563235519833 ) ) ;
#87660 = CARTESIAN_POINT ( 'NONE',  ( 41.66043411209999903, 1443.874408430530139, 136.1362219313979836 ) ) ;
#87661 = ORIENTED_EDGE ( 'NONE', *, *, #106208, .F. ) ;
#87662 = CARTESIAN_POINT ( 'NONE',  ( 3.711571330249999967, 1441.008188660590122, 218.3178908880789777 ) ) ;
#87663 = CARTESIAN_POINT ( 'NONE',  ( 11.75889809420000098, 1441.171049811090143, 188.0932782936979777 ) ) ;
#87664 = ORIENTED_EDGE ( 'NONE', *, *, #12306, .T. ) ;
#87665 = EDGE_LOOP ( 'NONE', ( #107226, #3420, #65771, #45158 ) ) ;
#87666 = CARTESIAN_POINT ( 'NONE',  ( -4.222077225850000559, 1454.203573669889920, 200.3246332114389929 ) ) ;
#87667 = CARTESIAN_POINT ( 'NONE',  ( 8.796059898609998484, 1362.759824263850078, 207.6218459616989946 ) ) ;
#87668 = CARTESIAN_POINT ( 'NONE',  ( -2.868433836634999512, 1517.020727862619879, 214.1341630384669941 ) ) ;
#87669 = CARTESIAN_POINT ( 'NONE',  ( 4.805077557904999352, 1510.399296111369949, 216.6702268425969748 ) ) ;
#87670 = B_SPLINE_CURVE_WITH_KNOTS ( 'NONE', 5,
 ( #37023, #79057, #54413, #97486, #2361, #55499, #12914, #104787, #47094 ),
 .UNSPECIFIED., .F., .F.,
 ( 6, 3, 6 ),
 ( 0.000000000000000000, 0.6258773692719435955, 1.000000000000000000 ),
 .UNSPECIFIED. ) ;
#87671 = ORIENTED_EDGE ( 'NONE', *, *, #74750, .T. ) ;
#87672 = CARTESIAN_POINT ( 'NONE',  ( 8.309621275030000476, 1427.613389394789920, 212.3081093229889973 ) ) ;
#87673 = CARTESIAN_POINT ( 'NONE',  ( -88.74645359839999514, 1377.077971548199912, 297.4629295155589830 ) ) ;
#87674 = ADVANCED_FACE ( 'NONE', ( #78084 ), #61759, .T. ) ;
#87675 = EDGE_CURVE ( 'NONE', #26117, #99683, #67675, .T. ) ;
#87676 =( BOUNDED_CURVE ( )  B_SPLINE_CURVE ( 3, ( #316, #77011, #34442, #9788 ),
 .UNSPECIFIED., .F., .F. ) 
 B_SPLINE_CURVE_WITH_KNOTS ( ( 4, 4 ),
 ( 4.424456909600460008, 5.579818660903430150 ),
 .UNSPECIFIED. ) 
 CURVE ( )  GEOMETRIC_REPRESENTATION_ITEM ( )  RATIONAL_B_SPLINE_CURVE ( ( 1.000000000000000000, 0.8918208900286694885, 0.8918208900286694885, 1.000000000000000000 ) ) 
 REPRESENTATION_ITEM ( '' )  );
#87677 = EDGE_CURVE ( 'NONE', #41248, #3770, #105538, .T. ) ;
#87678 = CARTESIAN_POINT ( 'NONE',  ( 7.681065654920000263, 1415.931669658129977, 225.5629348723979888 ) ) ;
#87679 = CARTESIAN_POINT ( 'NONE',  ( 3.255967386345000047, 1516.989560013210166, 204.1101670940770134 ) ) ;
#87680 = AXIS2_PLACEMENT_3D ( 'NONE', #34480, #94940, #10942 ) ;
#87681 = CARTESIAN_POINT ( 'NONE',  ( -28.26971619810000291, 1508.651289824929790, 208.8373429800469978 ) ) ;
#87682 = EDGE_CURVE ( 'NONE', #79550, #3955, #41186, .T. ) ;
#87683 = B_SPLINE_SURFACE_WITH_KNOTS ( 'NONE', 3, 1, ( 
 ( #68916, #70572 ),
 ( #27985, #87915 ),
 ( #45367, #52100 ),
 ( #86230, #103017 ) ),
 .UNSPECIFIED., .F., .F., .F.,
 ( 4, 4 ),
 ( 2, 2 ),
 ( 0.000000000000000000, 1.000000000000000000 ),
 ( 0.000000000000000000, 1.000000000000000000 ),
 .UNSPECIFIED. ) ;
#87684 = CARTESIAN_POINT ( 'NONE',  ( -41.32341301190928107, 1435.252038220275381, 269.6346703354698775 ) ) ;
#87685 = CARTESIAN_POINT ( 'NONE',  ( 4.364199625590375220, 1509.032014613821502, 205.0059826343180873 ) ) ;
#87686 = CARTESIAN_POINT ( 'NONE',  ( -3.945491179890000311, 1409.050839975730014, 231.1832439529980263 ) ) ;
#87687 = CIRCLE ( 'NONE', #21460, 1.000000000000007772 ) ;
#87689 = ORIENTED_EDGE ( 'NONE', *, *, #82218, .F. ) ;
#87688 = CARTESIAN_POINT ( 'NONE',  ( -10.44960420120000144, 1446.424728451650026, 186.6666287116979959 ) ) ;
#87690 = CARTESIAN_POINT ( 'NONE',  ( 4.408349274510000804, 1512.051704408390151, 206.7128113371389873 ) ) ;
#87691 = CARTESIAN_POINT ( 'NONE',  ( -11.90084016216500196, 1512.572572334140204, 216.0729386259769740 ) ) ;
#87692 = CARTESIAN_POINT ( 'NONE',  ( 19.29371659517364890, 1526.349689584397083, 233.1523940083487219 ) ) ;
#87693 = CARTESIAN_POINT ( 'NONE',  ( 15.72751745975079984, 1517.151704408390060, 206.8816388537309763 ) ) ;
#87694 = CARTESIAN_POINT ( 'NONE',  ( -25.23898257620000152, 1435.663290897030038, 136.6833633521980005 ) ) ;
#87695 = B_SPLINE_CURVE_WITH_KNOTS ( 'NONE', 3,
 ( #26172, #110191, #50316, #68227, #93930, #86643, #51956, #51392, #42435, #77704, #60358, #77162, #68773, #110744, #8819, #69323, #43004, #18322, #103429, #24513, #94480, #464, #58702, #17753, #16111, #76593, #86098, #26737, #9939, #101215, #33464, #44111, #16650, #84444 ),
 .UNSPECIFIED., .F., .F.,
 ( 4, 2, 2, 2, 2, 2, 2, 2, 2, 1, 1, 2, 2, 2, 1, 1, 2, 2, 4 ),
 ( 0.000000000000000000, 0.001953124999952264747, 0.003906249999904529493, 0.007812499999882994636, 0.01562499999985087623, 0.03124999999978504694, 0.06249999999966276976, 0.1249999999995043132, 0.2499999999992956745, 0.3749999999990870081, 0.4374999999989006572, 0.4687499999988947730, 0.4999999999988888888, 0.6249999999992073008, 0.6874999999993666178, 0.7187499999994462208, 0.7343749999994860778, 0.7499999999995258237, 1.000000000000000000 ),
 .UNSPECIFIED. ) ;
#87697 = CARTESIAN_POINT ( 'NONE',  ( 5.012317068235000228, 1517.020727862619879, 211.9902797687369969 ) ) ;
#87696 = CONICAL_SURFACE ( 'NONE', #43011, 24.00000000000002132, 0.3430239404209998177 ) ;
#87698 = CARTESIAN_POINT ( 'NONE',  ( -66.40232362439998326, 1379.742130965479873, 275.2934539270590335 ) ) ;
#87699 = CARTESIAN_POINT ( 'NONE',  ( -109.9852647598198843, 1384.923065380487742, 311.4561663452018934 ) ) ;
#87700 = CARTESIAN_POINT ( 'NONE',  ( -30.38288201977564285, 1524.477587234266139, 221.8420718908230356 ) ) ;
#87701 = CARTESIAN_POINT ( 'NONE',  ( 13.52265959860729971, 1497.923474612530072, 227.8730153353740207 ) ) ;
#87702 = CARTESIAN_POINT ( 'NONE',  ( 6.949703334655000120, 1517.130100026000036, 209.8609679372960102 ) ) ;
#87703 = ORIENTED_EDGE ( 'NONE', *, *, #31211, .F. ) ;
#87704 = CARTESIAN_POINT ( 'NONE',  ( -1.803460047120530207, 1451.935679885149966, 184.2329819486090230 ) ) ;
#87706 = EDGE_CURVE ( 'NONE', #50191, #76524, #13609, .T. ) ;
#87705 = CARTESIAN_POINT ( 'NONE',  ( -1.699922289799999930, 1417.915507289630114, 233.2101064502979852 ) ) ;
#87707 = CARTESIAN_POINT ( 'NONE',  ( -54.13050464459999489, 1384.845572836569772, 270.3682627440589954 ) ) ;
#87708 = ORIENTED_EDGE ( 'NONE', *, *, #52789, .F. ) ;
#87710 = B_SPLINE_CURVE_WITH_KNOTS ( 'NONE', 3,
 ( #94008, #85051, #25688, #67734 ),
 .UNSPECIFIED., .F., .F.,
 ( 4, 4 ),
 ( -17.00590611422270015, -6.621488669319999687 ),
 .UNSPECIFIED. ) ;
#87709 = CARTESIAN_POINT ( 'NONE',  ( 25.25200551730000242, 1450.804230319249882, 137.6134878989979882 ) ) ;
#87711 = CARTESIAN_POINT ( 'NONE',  ( -17.68237282055029880, 1517.151704408390060, 205.6847408665509818 ) ) ;
#87712 = CARTESIAN_POINT ( 'NONE',  ( 2.779535121191639924, 1478.702761277170111, 234.6945779322839769 ) ) ;
#87713 = EDGE_CURVE ( 'NONE', #96354, #33795, #110277, .T. ) ;
#87714 = CARTESIAN_POINT ( 'NONE',  ( -24.04911046563629995, 1508.500148083520116, 222.3301988378860301 ) ) ;
#87715 = CARTESIAN_POINT ( 'NONE',  ( -1.984520192970000263, 1409.916377354330052, 186.2507124829979830 ) ) ;
#87716 = EDGE_CURVE ( 'NONE', #1004, #84814, #100396, .T. ) ;
#87717 = CARTESIAN_POINT ( 'NONE',  ( -0.5133565506310000526, 1410.311096912230141, 233.1717002627980264 ) ) ;
#87718 = CARTESIAN_POINT ( 'NONE',  ( -0.005886490086299069752, 1420.444031316269729, 182.6735942328060105 ) ) ;
#87719 = AXIS2_PLACEMENT_3D ( 'NONE', #11878, #45507, #104280 ) ;
#87721 = CARTESIAN_POINT ( 'NONE',  ( 6.825131319317435441, 1424.845011660433101, 213.4895702506433963 ) ) ;
#87720 = CARTESIAN_POINT ( 'NONE',  ( 0.01171160595180150039, 1516.939568781210028, 215.6786969668069958 ) ) ;
#87722 = LINE ( 'NONE', #36200, #38830 ) ;
#87723 = CARTESIAN_POINT ( 'NONE',  ( 11.31530712674089934, 1470.580251583589870, 207.8288594857730232 ) ) ;
#87724 = ORIENTED_EDGE ( 'NONE', *, *, #37865, .T. ) ;
#87725 = CARTESIAN_POINT ( 'NONE',  ( -12.60587301698909890, 1415.938742849230039, 196.3044052707020057 ) ) ;
#87726 = LINE ( 'NONE', #54135, #80271 ) ;
#87727 = ORIENTED_EDGE ( 'NONE', *, *, #77712, .F. ) ;
#87728 = EDGE_CURVE ( 'NONE', #89419, #66077, #23680, .T. ) ;
#87729 = CARTESIAN_POINT ( 'NONE',  ( -2.713960167710639967E-10, 1417.262443616730025, 235.9145977375980010 ) ) ;
#87730 = CARTESIAN_POINT ( 'NONE',  ( -21.84020450222076093, 1523.481610426287716, 183.2638850454220858 ) ) ;
#87731 = CARTESIAN_POINT ( 'NONE',  ( 8.209489800525210157, 1511.433089852210060, 203.5668989247379841 ) ) ;
#87732 = CARTESIAN_POINT ( 'NONE',  ( 2.936686034740000117, 1441.572633673089967, 218.1969960917990079 ) ) ;
#87733 = CARTESIAN_POINT ( 'NONE',  ( -32.92528853941070821, 1523.611961620354123, 201.0067946816169240 ) ) ;
#87734 = CARTESIAN_POINT ( 'NONE',  ( 0.000000000000000000, 1384.913060387289988, 209.1218459572589836 ) ) ;
#87735 = CARTESIAN_POINT ( 'NONE',  ( 17.97556616420000353, 1415.263254644529979, 210.1863902027079973 ) ) ;
#87736 = CARTESIAN_POINT ( 'NONE',  ( -18.37606861500000122, 1424.967732719430160, 227.5064700491979863 ) ) ;
#87737 = CARTESIAN_POINT ( 'NONE',  ( -22.92800964410000120, 1436.527409660840021, 141.8297638279979935 ) ) ;
#87738 = CARTESIAN_POINT ( 'NONE',  ( -11.88140585900000090, 1433.447543843229823, 147.6490162021979984 ) ) ;
#87739 = CARTESIAN_POINT ( 'NONE',  ( 15.76350792579999904, 1413.541987861329972, 191.4338706723980010 ) ) ;
#87741 = CARTESIAN_POINT ( 'NONE',  ( 4.329448781177520189, 1515.064792686469900, 207.2788827064790098 ) ) ;
#87740 = CARTESIAN_POINT ( 'NONE',  ( 4.414384251610000476, 1487.467097172089780, 197.9737507085990273 ) ) ;
#87742 = CARTESIAN_POINT ( 'NONE',  ( 27.69925877688100258, 1441.434395746940027, 137.3015763641899980 ) ) ;
#87743 = EDGE_LOOP ( 'NONE', ( #32031, #57679, #72201 ) ) ;
#87744 = CARTESIAN_POINT ( 'NONE',  ( 1.556549595879139991, 1415.034069327939960, 191.5954303787009962 ) ) ;
#87745 = CARTESIAN_POINT ( 'NONE',  ( 23.52041813219999966, 1430.461288272430238, 206.7123354197679816 ) ) ;
#87746 = CARTESIAN_POINT ( 'NONE',  ( -23.77394755739999965, 1436.009596247230093, 211.4729698866979959 ) ) ;
#87747 = LINE ( 'NONE', #29466, #56291 ) ;
#87748 = CARTESIAN_POINT ( 'NONE',  ( -18.57349606690000243, 1508.241272120329995, 229.7340498379979863 ) ) ;
#87749 = CARTESIAN_POINT ( 'NONE',  ( -2.976203730276889114, 1425.987994125993964, 185.4396839897474649 ) ) ;
#87750 = CARTESIAN_POINT ( 'NONE',  ( 11.76054352614784548, 1435.168637047273251, 151.3007564940777741 ) ) ;
#87751 = CARTESIAN_POINT ( 'NONE',  ( 29.30029655192931415, 1525.907212628473872, 221.3719603026171399 ) ) ;
#87752 = DIRECTION ( 'NONE',  ( 5.980589973904019347E-17, -1.000000000000000000, 1.736889445713099699E-16 ) ) ;
#87753 = CARTESIAN_POINT ( 'NONE',  ( -10.61843432092680040, 1489.244268642379893, 214.1625968120690118 ) ) ;
#87754 = CARTESIAN_POINT ( 'NONE',  ( 24.11200011979999758, 1496.633574749990203, 206.8275458132090137 ) ) ;
#87755 = CARTESIAN_POINT ( 'NONE',  ( -95.22212654925510833, 1383.767033602980064, 309.9034185838269764 ) ) ;
#87756 = CARTESIAN_POINT ( 'NONE',  ( -109.4402575644460001, 1383.302147128139950, 311.1271210982910134 ) ) ;
#87757 = CARTESIAN_POINT ( 'NONE',  ( -15.83141035718888645, 1506.691119452811790, 224.6832273421007642 ) ) ;
#87758 = CARTESIAN_POINT ( 'NONE',  ( -22.70290513515956832, 1409.705865905418023, 209.5810033907468721 ) ) ;
#87760 = ORIENTED_EDGE ( 'NONE', *, *, #35110, .T. ) ;
#87759 = CARTESIAN_POINT ( 'NONE',  ( 24.02863965889999776, 1507.902931924930044, 195.9323066764980013 ) ) ;
#87761 = CARTESIAN_POINT ( 'NONE',  ( -17.14943674877569890, 1460.897686246159992, 228.2718295297070199 ) ) ;
#87762 = AXIS2_PLACEMENT_3D ( 'NONE', #69542, #26961, #61151 ) ;
#87763 = CARTESIAN_POINT ( 'NONE',  ( -82.36118214929999226, 1380.660938380089874, 289.8805188183589507 ) ) ;
#87764 = DIRECTION ( 'NONE',  ( -1.836970198721029688E-16, -1.000000000000000000, 0.000000000000000000 ) ) ;
#87765 = VERTEX_POINT ( 'NONE', #32644 ) ;
#87766 = EDGE_LOOP ( 'NONE', ( #109587, #64780, #102654, #108783 ) ) ;
#87767 = CARTESIAN_POINT ( 'NONE',  ( 17.57493253053520021, 1415.090956648730071, 210.1540952727430067 ) ) ;
#87768 = CARTESIAN_POINT ( 'NONE',  ( -109.3492338110000048, 1384.921838666169833, 297.1385152072589904 ) ) ;
#87769 = CARTESIAN_POINT ( 'NONE',  ( 13.43245946205634667, 1443.480739768224339, 169.3649759703340294 ) ) ;
#87771 = CARTESIAN_POINT ( 'NONE',  ( -39.71667984470000334, 1443.385947343989756, 259.0958842110979958 ) ) ;
#87770 = CARTESIAN_POINT ( 'NONE',  ( 19.63212482909999679, 1452.819910076630094, 208.7504658628519962 ) ) ;
#87772 = FACE_OUTER_BOUND ( 'NONE', #64399, .T. ) ;
#87773 = CARTESIAN_POINT ( 'NONE',  ( -11.23615794200000018, 1433.983026149579928, 151.5834757130979824 ) ) ;
#87774 = EDGE_CURVE ( 'NONE', #37552, #109438, #90249, .T. ) ;
#87775 = CARTESIAN_POINT ( 'NONE',  ( -3.160255966859999877, 1481.778611285589932, 229.3886674967989734 ) ) ;
#87776 = CARTESIAN_POINT ( 'NONE',  ( -20.03090002299999739, 1485.143653381429885, 191.6176849518980134 ) ) ;
#87777 = CARTESIAN_POINT ( 'NONE',  ( 13.55936921520000027, 1409.552479627430102, 191.5919583953979952 ) ) ;
#87778 = EDGE_CURVE ( 'NONE', #83093, #777, #99553, .T. ) ;
#87779 = CARTESIAN_POINT ( 'NONE',  ( 4.891644445989999923, 1423.483205933229783, 184.7436577964980131 ) ) ;
#87780 = CARTESIAN_POINT ( 'NONE',  ( -11.36665844790000079, 1437.938651746620053, 152.0461524611979769 ) ) ;
#87781 = CARTESIAN_POINT ( 'NONE',  ( 11.26681265989999936, 1433.831805099620169, 151.5577295601979984 ) ) ;
#87782 = CARTESIAN_POINT ( 'NONE',  ( -16.06071031163280338, 1420.824417172319954, 203.3393085456370102 ) ) ;
#87783 = DIRECTION ( 'NONE',  ( 0.000000000000000000, -1.000000000000000000, 0.000000000000000000 ) ) ;
#87784 = DIRECTION ( 'NONE',  ( -1.755985294532469921E-16, 1.000000000000000000, -1.338183447452831989E-16 ) ) ;
#87785 = ORIENTED_EDGE ( 'NONE', *, *, #40371, .F. ) ;
#87786 = CARTESIAN_POINT ( 'NONE',  ( -2.382436964801009083, 1426.901689560119166, 137.0999999980979567 ) ) ;
#87787 = CARTESIAN_POINT ( 'NONE',  ( -5.440472735201729471, 1490.455374013109804, 185.8786135604090362 ) ) ;
#87788 = CARTESIAN_POINT ( 'NONE',  ( -38.10549725089999384, 1456.559844724929917, 270.3402585752979803 ) ) ;
#87789 = CARTESIAN_POINT ( 'NONE',  ( -113.4000000000000057, 1377.913060387289988, 304.2218459572590064 ) ) ;
#87790 = CARTESIAN_POINT ( 'NONE',  ( 17.22540035980000184, 1409.514584625130055, 222.3763175275979904 ) ) ;
#87791 = CARTESIAN_POINT ( 'NONE',  ( 49.24962907673571522, 1524.382868172863937, 407.9033880519289710 ) ) ;
#87792 = EDGE_CURVE ( 'NONE', #94490, #35126, #16903, .T. ) ;
#87793 = CARTESIAN_POINT ( 'NONE',  ( 8.407921469289998839, 1475.513060387329915, 189.8056153727980018 ) ) ;
#87794 = CARTESIAN_POINT ( 'NONE',  ( 2.858803364451159901, 1409.202624393130009, 230.9089643516309991 ) ) ;
#87795 = FACE_OUTER_BOUND ( 'NONE', #14458, .T. ) ;
#87796 = CARTESIAN_POINT ( 'NONE',  ( -11.46248030930000006, 1419.039353461930205, 229.2066792439979963 ) ) ;
#87797 = CIRCLE ( 'NONE', #82428, 1.999999999999999556 ) ;
#87798 = CARTESIAN_POINT ( 'NONE',  ( -10.76610287370000130, 1461.751116408590178, 211.3389343564790011 ) ) ;
#87799 = CARTESIAN_POINT ( 'NONE',  ( 8.379275254590000443, 1362.454991452509830, 207.6218459616989946 ) ) ;
#87800 = CARTESIAN_POINT ( 'NONE',  ( -44.72192564158709871, 1433.780113820020233, 266.2155848715870547 ) ) ;
#87801 = CARTESIAN_POINT ( 'NONE',  ( -2.500000000000000000, 1425.954745500930130, 184.7023283137979774 ) ) ;
#87802 = ORIENTED_EDGE ( 'NONE', *, *, #20343, .F. ) ;
#87803 = CARTESIAN_POINT ( 'NONE',  ( 23.71772659069999989, 1435.325744483010112, 137.0491500660980080 ) ) ;
#87804 = ORIENTED_EDGE ( 'NONE', *, *, #52202, .T. ) ;
#87805 = CARTESIAN_POINT ( 'NONE',  ( -6.938478822895000064, 1516.719999691880048, 209.8757167055200057 ) ) ;
#87806 = AXIS2_PLACEMENT_3D ( 'NONE', #12414, #38712, #65038 ) ;
#87807 = CARTESIAN_POINT ( 'NONE',  ( -9.472336532046449875, 1447.006353964749906, 212.1615584954940061 ) ) ;
#87808 = CARTESIAN_POINT ( 'NONE',  ( -21.33070998720000233, 1509.431296620130070, 190.3921826451980053 ) ) ;
#87809 = CARTESIAN_POINT ( 'NONE',  ( -2.610074113990000111, 1410.395240763830088, 186.5675311192979962 ) ) ;
#87810 = CARTESIAN_POINT ( 'NONE',  ( 2.188321237025089960, 1495.686656333250085, 221.2656737636790183 ) ) ;
#87811 = EDGE_LOOP ( 'NONE', ( #53738, #36813, #68133, #62358 ) ) ;
#87812 = CARTESIAN_POINT ( 'NONE',  ( 23.88021423819999711, 1436.089573992459918, 213.0827210816779882 ) ) ;
#87814 = CARTESIAN_POINT ( 'NONE',  ( 12.87559654649999885, 1416.820969729830040, 196.3104025333980189 ) ) ;
#87813 = CARTESIAN_POINT ( 'NONE',  ( 3.628818056492709943, 1505.602008419380127, 221.3635114792730292 ) ) ;
#87815 = EDGE_CURVE ( 'NONE', #41237, #15707, #28787, .T. ) ;
#87816 = CARTESIAN_POINT ( 'NONE',  ( 11.60004869885203505, 1425.456391939635751, 136.9368493822784671 ) ) ;
#87817 = VECTOR ( 'NONE', #34702, 1000.000000000000000 ) ;
#87818 = CARTESIAN_POINT ( 'NONE',  ( -18.37965383104189954, 1508.494210133719889, 211.1516869488499992 ) ) ;
#87819 = CARTESIAN_POINT ( 'NONE',  ( 6.246736226000000336, 1472.130509067990033, 217.1982816640689862 ) ) ;
#87820 = CARTESIAN_POINT ( 'NONE',  ( -8.792731325493480909, 1438.786328558429886, 208.0437710220710130 ) ) ;
#87821 = EDGE_LOOP ( 'NONE', ( #36864, #77355, #39320, #2758, #98130, #106275, #107829, #46870, #88488 ) ) ;
#87822 = CARTESIAN_POINT ( 'NONE',  ( -22.51472004476610067, 1414.327503631689979, 270.0970517051659385 ) ) ;
#87823 = CARTESIAN_POINT ( 'NONE',  ( 1.122033391945000069, 1516.972341476009888, 208.3659064338399673 ) ) ;
#87824 = CARTESIAN_POINT ( 'NONE',  ( 2.840174497108410634, 1416.937576063520055, 232.1670866114159821 ) ) ;
#87825 = CARTESIAN_POINT ( 'NONE',  ( 8.530885801226901322, 1436.944794269080148, 207.7948910702020271 ) ) ;
#87827 = ORIENTED_EDGE ( 'NONE', *, *, #97353, .F. ) ;
#87826 = CARTESIAN_POINT ( 'NONE',  ( -7.894907142693425861, 1366.239093409125644, 210.6218459617142003 ) ) ;
#87828 = ORIENTED_EDGE ( 'NONE', *, *, #59735, .F. ) ;
#87829 = CARTESIAN_POINT ( 'NONE',  ( 45.62288738355533724, 1441.767032437498983, 268.9751391232022684 ) ) ;
#87830 = EDGE_CURVE ( 'NONE', #19317, #16710, #84685, .T. ) ;
#87831 = CARTESIAN_POINT ( 'NONE',  ( 8.794242744369535458, 1511.655929346016364, 202.9804211893913362 ) ) ;
#87832 = CARTESIAN_POINT ( 'NONE',  ( -22.08622291482313926, 1523.382868172864164, 233.8253038720786776 ) ) ;
#87833 = CARTESIAN_POINT ( 'NONE',  ( -0.03032924301457349744, 1409.189327868429928, 185.6174390816690050 ) ) ;
#87834 = EDGE_CURVE ( 'NONE', #41116, #87329, #839, .T. ) ;
#87835 = DIRECTION ( 'NONE',  ( -0.02616798426500960631, 0.9993150019883682011, 0.02616798426500960631 ) ) ;
#87836 = CARTESIAN_POINT ( 'NONE',  ( -18.11774863200000141, 1420.839368349930055, 225.3824726533979970 ) ) ;
#87837 = CARTESIAN_POINT ( 'NONE',  ( -0.0001178445682933130075, 1475.048122365760037, 269.6502183532239769 ) ) ;
#87838 = CARTESIAN_POINT ( 'NONE',  ( -4.377444850077553795, 1466.548242231658151, 234.6382214351334028 ) ) ;
#87839 = CARTESIAN_POINT ( 'NONE',  ( 5.684860708799999607, 1446.208771210280020, 183.7854341813980170 ) ) ;
#87840 = CARTESIAN_POINT ( 'NONE',  ( 2.282915183265000092, 1516.876240617270014, 206.6278256496669883 ) ) ;
#87841 = VERTEX_POINT ( 'NONE', #10763 ) ;
#87842 = CARTESIAN_POINT ( 'NONE',  ( 21.54081683246133849, 1411.025740448911392, 217.0790126318913451 ) ) ;
#87843 = CARTESIAN_POINT ( 'NONE',  ( 1.516162725629030206, 1458.382341108720084, 183.2406470817350055 ) ) ;
#87844 = VERTEX_POINT ( 'NONE', #18028 ) ;
#87845 = DIRECTION ( 'NONE',  ( -0.8539859765994315399, 0.000000000000000000, 0.5202960232132425311 ) ) ;
#87846 = CARTESIAN_POINT ( 'NONE',  ( 25.36371696672659937, 1452.027352620659940, 135.3832310289139969 ) ) ;
#87847 = DIRECTION ( 'NONE',  ( 1.836970198721029688E-16, 1.000000000000000000, 0.000000000000000000 ) ) ;
#87848 = CARTESIAN_POINT ( 'NONE',  ( -27.75968971620000048, 1386.892151378640165, 225.4868526693589956 ) ) ;
#87849 = CARTESIAN_POINT ( 'NONE',  ( -13.29657497211445794, 1389.765381873174420, 214.2158378427034222 ) ) ;
#87850 = CARTESIAN_POINT ( 'NONE',  ( 18.26694772049999926, 1410.474778457329876, 193.9644247597979927 ) ) ;
#87851 = CARTESIAN_POINT ( 'NONE',  ( 22.98253439269999987, 1410.218983183530099, 207.4712557340779995 ) ) ;
#87852 = CARTESIAN_POINT ( 'NONE',  ( 16.19492570339999915, 1409.478599654730033, 224.8086529783979870 ) ) ;
#87853 = CARTESIAN_POINT ( 'NONE',  ( -19.34609354041575813, 1425.420091874406125, 223.6468805313006669 ) ) ;
#87854 = ADVANCED_FACE ( 'NONE', ( #28098 ), #31423, .T. ) ;
#87855 = CARTESIAN_POINT ( 'NONE',  ( 0.6086926234157500337, 1452.967218034779989, 183.3063368812749729 ) ) ;
#87856 = CARTESIAN_POINT ( 'NONE',  ( -8.982902946400001198, 1383.064277652569899, 218.2826811425790083 ) ) ;
#87857 = CARTESIAN_POINT ( 'NONE',  ( -2.868433836634999512, 1517.020727862619879, 214.1341630384669941 ) ) ;
#87858 = EDGE_CURVE ( 'NONE', #104164, #4923, #78751, .T. ) ;
#87859 = FACE_OUTER_BOUND ( 'NONE', #40946, .T. ) ;
#87860 = EDGE_LOOP ( 'NONE', ( #1050, #66968, #71378, #75281 ) ) ;
#87861 = CARTESIAN_POINT ( 'NONE',  ( -14.35518320136639936, 1509.483853104240097, 182.9676327163749932 ) ) ;
#87862 = DIRECTION ( 'NONE',  ( 0.3363363969979655810, -0.9417419115949056119, 0.000000000000000000 ) ) ;
#87863 = CARTESIAN_POINT ( 'NONE',  ( -9.751878866779549071, 1483.635755006349882, 202.2899340601439917 ) ) ;
#87864 = CARTESIAN_POINT ( 'NONE',  ( -9829.078716724869082, 2833.596074015789782, -1083.720023828399917 ) ) ;
#87865 = B_SPLINE_CURVE_WITH_KNOTS ( 'NONE', 3,
 ( #16951, #51709, #86398, #58454 ),
 .UNSPECIFIED., .F., .F.,
 ( 4, 4 ),
 ( 0.000000000000000000, 1.000000000000000000 ),
 .UNSPECIFIED. ) ;
#87866 = CARTESIAN_POINT ( 'NONE',  ( -36.44972635297019536, 1449.829476660199816, 136.2612135086269802 ) ) ;
#87867 = CARTESIAN_POINT ( 'NONE',  ( 0.1622545933607045798, 1506.474306115611853, 231.1380631582393903 ) ) ;
#87868 = CARTESIAN_POINT ( 'NONE',  ( 4.884981308350000102E-15, 1454.846680951630105, 214.3676144195279676 ) ) ;
#87869 = CARTESIAN_POINT ( 'NONE',  ( -2.391326140863789806, 1458.414063273499778, 184.3573557473769995 ) ) ;
#87870 = CARTESIAN_POINT ( 'NONE',  ( 11.14340129720000050, 1433.162048341109994, 151.6428083595979786 ) ) ;
#87871 = CARTESIAN_POINT ( 'NONE',  ( -4.227836598029999671, 1474.916636390029907, 269.6389068554980213 ) ) ;
#87872 = CARTESIAN_POINT ( 'NONE',  ( 25.99288283567859636, 1440.913060397479967, 221.8287371291170018 ) ) ;
#87873 = LINE ( 'NONE', #105771, #96582 ) ;
#87874 = CARTESIAN_POINT ( 'NONE',  ( 14.27741977803430196, 1427.979761714439974, 195.2518213606840050 ) ) ;
#87875 = ORIENTED_EDGE ( 'NONE', *, *, #100138, .T. ) ;
#87876 = CARTESIAN_POINT ( 'NONE',  ( 22.72903601766490311, 1507.336004462970095, 209.8256819690419945 ) ) ;
#87877 = CARTESIAN_POINT ( 'NONE',  ( 10.12814239611219946, 1462.553068569410243, 212.1302522725090114 ) ) ;
#87878 = CARTESIAN_POINT ( 'NONE',  ( -5.823492620599999725, 1486.046966802129873, 182.4545651139980009 ) ) ;
#87879 = AXIS2_PLACEMENT_3D ( 'NONE', #59658, #61884, #9248 ) ;
#87880 = CARTESIAN_POINT ( 'NONE',  ( -1.389373685231614308, 1526.382868172571079, 239.5386865367401299 ) ) ;
#87881 = CARTESIAN_POINT ( 'NONE',  ( 5.561733859871847763, 1387.291117539184825, 209.1218459616989946 ) ) ;
#87882 = CARTESIAN_POINT ( 'NONE',  ( 19.72588039849999930, 1469.237837315330125, 224.9730300090979824 ) ) ;
#87883 = CARTESIAN_POINT ( 'NONE',  ( -15.86366695747779332, 1420.273692602325809, 209.9455591108094836 ) ) ;
#87884 = CARTESIAN_POINT ( 'NONE',  ( 2.557733547691819709, 1428.430169347510173, 224.8392532217209805 ) ) ;
#87885 = CARTESIAN_POINT ( 'NONE',  ( -26.54368091973730159, 1383.846278271480060, 224.6430921072530111 ) ) ;
#87886 = CARTESIAN_POINT ( 'NONE',  ( -4.556906648196700438, 1508.729448895619953, 205.9844575237659967 ) ) ;
#87887 = CARTESIAN_POINT ( 'NONE',  ( 9.509570154840000455, 1407.604192000429975, 218.7432867935780223 ) ) ;
#87888 = CARTESIAN_POINT ( 'NONE',  ( -234.5897387251999930, 11221.53578756869865, 2175.945776423289772 ) ) ;
#87889 = CARTESIAN_POINT ( 'NONE',  ( 0.1659333737283860133, 1482.725682766760201, 181.9772994460549853 ) ) ;
#87891 = VERTEX_POINT ( 'NONE', #14591 ) ;
#87890 = CARTESIAN_POINT ( 'NONE',  ( 17.76546875260000036, 1430.865606781589804, 204.9340536459789917 ) ) ;
#87892 = CARTESIAN_POINT ( 'NONE',  ( -16.68463233076019492, 1445.052233488289630, 162.0935120523188857 ) ) ;
#87893 = CARTESIAN_POINT ( 'NONE',  ( -9.835690489261324387, 1389.390132783129729, 201.5977833131792920 ) ) ;
#87894 = CARTESIAN_POINT ( 'NONE',  ( 4.424121880270347695, 1432.332071595964408, 155.5695889658696274 ) ) ;
#87896 = ORIENTED_EDGE ( 'NONE', *, *, #39113, .T. ) ;
#87895 = CARTESIAN_POINT ( 'NONE',  ( -38.37377460175660104, 1450.184294006830214, 134.0999999983419855 ) ) ;
#87897 = CARTESIAN_POINT ( 'NONE',  ( -2.525895663881050357, 1508.551704408389924, 220.0390078997519936 ) ) ;
#87898 = ORIENTED_EDGE ( 'NONE', *, *, #64602, .T. ) ;
#87899 = VECTOR ( 'NONE', #37193, 1000.000000000000000 ) ;
#87900 = CARTESIAN_POINT ( 'NONE',  ( 1.514120561980000183E-16, 1515.551704408389924, 209.1218459616989946 ) ) ;
#87901 = CARTESIAN_POINT ( 'NONE',  ( 5.151097723079999469, 1490.744826430290004, 188.9005472705989916 ) ) ;
#87902 = DIRECTION ( 'NONE',  ( 0.000000000000000000, 0.000000000000000000, 1.000000000000000000 ) ) ;
#87903 = CARTESIAN_POINT ( 'NONE',  ( -2.905551374272877130, 1368.288386645854189, 207.9218722600712965 ) ) ;
#87904 = ADVANCED_FACE ( 'NONE', ( #71808 ), #47664, .T. ) ;
#87905 = CARTESIAN_POINT ( 'NONE',  ( 0.4974867301289990218, 1430.722264131989959, 217.6047022486590095 ) ) ;
#87906 = CARTESIAN_POINT ( 'NONE',  ( 1.842963673760084298, 1515.499673569527658, 213.2081603882464265 ) ) ;
#87907 = CARTESIAN_POINT ( 'NONE',  ( 12.40624418351419855, 1409.346295973229871, 217.4486123556800408 ) ) ;
#87908 = CARTESIAN_POINT ( 'NONE',  ( 4.617353517619999792, 1460.098150474590057, 228.0971968620989969 ) ) ;
#87909 = CARTESIAN_POINT ( 'NONE',  ( -100.7263133942470006, 1385.222699183060058, 296.4096551585109864 ) ) ;
#87910 = CARTESIAN_POINT ( 'NONE',  ( -17.71469135509999759, 1424.169313328530052, 191.8806465351980250 ) ) ;
#87911 = FACE_OUTER_BOUND ( 'NONE', #47583, .T. ) ;
#87912 = ORIENTED_EDGE ( 'NONE', *, *, #85128, .T. ) ;
#87913 = AXIS2_PLACEMENT_3D ( 'NONE', #52374, #76442, #67517 ) ;
#87914 = CARTESIAN_POINT ( 'NONE',  ( 11.13873845943729890, 1491.363418941899909, 209.7176399918620007 ) ) ;
#87916 = ORIENTED_EDGE ( 'NONE', *, *, #54949, .T. ) ;
#87915 = CARTESIAN_POINT ( 'NONE',  ( -1.581901184577762409, 1426.946688134061105, 134.0999999980979567 ) ) ;
#87917 = VERTEX_POINT ( 'NONE', #3478 ) ;
#87918 = CARTESIAN_POINT ( 'NONE',  ( 17.74362484289149933, 1457.960420730979877, 228.9108169342899828 ) ) ;
#87919 = CARTESIAN_POINT ( 'NONE',  ( -5.986709854334679726, 1361.264879806951967, 210.6218459616987957 ) ) ;
#87920 = CARTESIAN_POINT ( 'NONE',  ( 0.5070043562000440263, 1496.683860206890131, 196.7605787459179965 ) ) ;
#87921 = EDGE_CURVE ( 'NONE', #12979, #39452, #3413, .T. ) ;
#87922 = CARTESIAN_POINT ( 'NONE',  ( 29.52154479088818562, 1509.964009467801588, 211.6628974038054594 ) ) ;
#87923 = CARTESIAN_POINT ( 'NONE',  ( -30.79697748855893735, 1526.178928173327449, 221.8439766881946014 ) ) ;
#87924 = CARTESIAN_POINT ( 'NONE',  ( 2.495059952650000135, 1396.538088716130005, 221.4303740941980152 ) ) ;
#87925 = CARTESIAN_POINT ( 'NONE',  ( 32.05679137160524306, 1524.478200376950781, 201.5541812493231077 ) ) ;
#87926 = CARTESIAN_POINT ( 'NONE',  ( -6.069631065962992622, 1516.744148413207085, 213.5279290861298307 ) ) ;
#87927 = CARTESIAN_POINT ( 'NONE',  ( -0.8705189345459999339, 1455.061689295130009, 183.2811947162979891 ) ) ;
#87928 = CARTESIAN_POINT ( 'NONE',  ( -10.55984826015959221, 1366.521027767394116, 207.6218459616987673 ) ) ;
#87929 = CARTESIAN_POINT ( 'NONE',  ( -26.07931670434293281, 1436.684335497711118, 136.9216750084780756 ) ) ;
#87930 = CARTESIAN_POINT ( 'NONE',  ( -6.950833568235000648, 1517.156142772249950, 206.6378959915070084 ) ) ;
#87931 = CARTESIAN_POINT ( 'NONE',  ( -13.11326399589999880, 1435.169422440890003, 150.1511621572980175 ) ) ;
#87932 = CARTESIAN_POINT ( 'NONE',  ( 17.09517797430000030, 1409.510037156830094, 194.7435863138979926 ) ) ;
#87933 = CARTESIAN_POINT ( 'NONE',  ( 0.6649116665570009577, 1498.634995304990071, 197.7885086964990080 ) ) ;
#87934 = CARTESIAN_POINT ( 'NONE',  ( 13.96015159390320726, 1516.660421270692950, 226.2743875082219063 ) ) ;
#87935 = CARTESIAN_POINT ( 'NONE',  ( -109.0547027409999998, 1384.148091023459756, 297.1846209902590203 ) ) ;
#87936 = ORIENTED_EDGE ( 'NONE', *, *, #69028, .F. ) ;
#87937 = CARTESIAN_POINT ( 'NONE',  ( 13.62888593203049936, 1517.051704413129983, 191.9442378289920157 ) ) ;
#87938 = CARTESIAN_POINT ( 'NONE',  ( -22.23102603839999958, 1508.124938942629797, 193.6648602066980231 ) ) ;
#87940 = CARTESIAN_POINT ( 'NONE',  ( 5.451195050909999503E-14, 1410.389826760030019, 269.3346704430979912 ) ) ;
#87939 = CARTESIAN_POINT ( 'NONE',  ( -10.33698045908790064, 1425.426606213330160, 91.95338683678188829 ) ) ;
#87941 = CARTESIAN_POINT ( 'NONE',  ( -7.709032175815000443, 1516.534320418310244, 211.6070631641669877 ) ) ;
#87942 = PLANE ( 'NONE',  #22998 ) ;
#87943 = CARTESIAN_POINT ( 'NONE',  ( -33.33289073560000304, 1436.626756254900101, 248.0947902376980210 ) ) ;
#87944 = CARTESIAN_POINT ( 'NONE',  ( 19.95713565929469979, 1509.643969355689933, 231.1087739065170013 ) ) ;
#87945 = ADVANCED_FACE ( 'NONE', ( #28522 ), #3649, .T. ) ;
#87946 = CARTESIAN_POINT ( 'NONE',  ( -13.40958089250450058, 1414.996442620860080, 220.3303868550709694 ) ) ;
#87947 = CARTESIAN_POINT ( 'NONE',  ( -24.06079138099230263, 1410.858125179654508, 208.6187266795722621 ) ) ;
#87948 = EDGE_LOOP ( 'NONE', ( #87098, #35042 ) ) ;
#87949 = CARTESIAN_POINT ( 'NONE',  ( -2.500000000000000000, 1432.325347410999711, 157.4940207838979802 ) ) ;
#87950 = CARTESIAN_POINT ( 'NONE',  ( 14.72260980806426112, 1514.508970282057362, 225.4219501776639163 ) ) ;
#87951 = ADVANCED_FACE ( 'NONE', ( #87328 ), #73615, .F. ) ;
#87952 = CARTESIAN_POINT ( 'NONE',  ( 3.331783404088239919, 1517.151704408390060, 197.4348858789911674 ) ) ;
#87953 = VERTEX_POINT ( 'NONE', #97371 ) ;
#87954 = EDGE_LOOP ( 'NONE', ( #9777, #13724, #70764, #95719 ) ) ;
#87955 = CARTESIAN_POINT ( 'NONE',  ( -29.28608745770604216, 1509.936230668231474, 211.6463041379158199 ) ) ;
#87956 = CARTESIAN_POINT ( 'NONE',  ( 6.112774900040000681, 1424.453475662199935, 193.6149460215989961 ) ) ;
#87957 = ADVANCED_FACE ( 'NONE', ( #56487 ), #21182, .T. ) ;
#87958 = ORIENTED_EDGE ( 'NONE', *, *, #42808, .T. ) ;
#87959 = CIRCLE ( 'NONE', #61124, 23.69926344187880929 ) ;
#87960 = CARTESIAN_POINT ( 'NONE',  ( 0.08511096936709999783, 1424.315873630530177, 227.5527473093980007 ) ) ;
#87961 = CARTESIAN_POINT ( 'NONE',  ( -1.920602012799999869, 1420.567466289690174, 193.8392733480989989 ) ) ;
#87962 = DIRECTION ( 'NONE',  ( 0.9401064050714854625, -0.2476038110569656059, -0.2342910580744280991 ) ) ;
#87963 = EDGE_CURVE ( 'NONE', #5224, #54639, #31269, .T. ) ;
#87964 = CARTESIAN_POINT ( 'NONE',  ( -3.374329543420000022, 1470.482678873730038, 235.0946326950979994 ) ) ;
#87965 = CARTESIAN_POINT ( 'NONE',  ( 1.398466363930680023, 1420.912512660129778, 183.0157344917449791 ) ) ;
#87966 = CARTESIAN_POINT ( 'NONE',  ( 45.85445519596599695, 1441.844569312759859, 268.7564833741089956 ) ) ;
#87967 = CARTESIAN_POINT ( 'NONE',  ( -12.40508161610000037, 1391.584463596800106, 210.3939176184290147 ) ) ;
#87968 = CARTESIAN_POINT ( 'NONE',  ( 0.2192230774779999891, 1419.198292138529951, 184.6432371525980045 ) ) ;
#87969 = ORIENTED_EDGE ( 'NONE', *, *, #77466, .F. ) ;
#87970 = CARTESIAN_POINT ( 'NONE',  ( 2.287084270065000258, 1517.068517094990057, 204.1085709707169826 ) ) ;
#87971 = CARTESIAN_POINT ( 'NONE',  ( 2.494757998004999866, 1516.937508036699910, 210.8228737931069929 ) ) ;
#87972 = VERTEX_POINT ( 'NONE', #81655 ) ;
#87973 = CARTESIAN_POINT ( 'NONE',  ( 11.85573241129629984, 1431.613746796120040, 149.9352766684680205 ) ) ;
#87974 = AXIS2_PLACEMENT_3D ( 'NONE', #109343, #81909, #67349 ) ;
#87975 = CARTESIAN_POINT ( 'NONE',  ( 13.13407055734306006, 1444.772519759580291, 187.1788395466846850 ) ) ;
#87976 = VERTEX_POINT ( 'NONE', #90061 ) ;
#87977 = CARTESIAN_POINT ( 'NONE',  ( 0.7957076353827553516, 1507.773683909243118, 220.9213704339180993 ) ) ;
#87978 = CARTESIAN_POINT ( 'NONE',  ( -7.056546027978409796, 1508.551704406279896, 219.2861282186669882 ) ) ;
#87979 = CARTESIAN_POINT ( 'NONE',  ( 4.910254292329999437, 1507.788984001429981, 235.8016783594979700 ) ) ;
#87980 = CARTESIAN_POINT ( 'NONE',  ( -10.75669312256790100, 1470.034964047250014, 212.8110033683189783 ) ) ;
#87981 = CARTESIAN_POINT ( 'NONE',  ( 16.18847201900799959, 1452.347746487550012, 146.9707830506359869 ) ) ;
#87982 = CARTESIAN_POINT ( 'NONE',  ( 3.165485043389999920, 1408.317885794130007, 270.3910588707980196 ) ) ;
#87983 = CARTESIAN_POINT ( 'NONE',  ( -109.0712831559999927, 1385.610640481809924, 297.1783689030590381 ) ) ;
#87984 = CARTESIAN_POINT ( 'NONE',  ( -4.912635829359999207, 1474.545048648290049, 199.2507989359390024 ) ) ;
#87985 = CARTESIAN_POINT ( 'NONE',  ( -2.316872680442880306, 1421.992067379949958, 193.2449569725669960 ) ) ;
#87986 = CARTESIAN_POINT ( 'NONE',  ( -37.75146778639999923, 1379.660437608350094, 220.6592702495590004 ) ) ;
#87987 = CARTESIAN_POINT ( 'NONE',  ( 0.02828745832028754098, 1410.214488029192353, 233.2162056590676684 ) ) ;
#87989 = CARTESIAN_POINT ( 'NONE',  ( 15.02274787390000022, 1434.996842493880195, 196.2759273980980197 ) ) ;
#87988 = CARTESIAN_POINT ( 'NONE',  ( -15.05518181500000097, 1503.464336090389907, 209.0350305184400099 ) ) ;
#87990 = CARTESIAN_POINT ( 'NONE',  ( 11.12319339834159848, 1422.705095784430114, 206.9939503724160090 ) ) ;
#87991 = CARTESIAN_POINT ( 'NONE',  ( 17.77755434120550149, 1416.443526435939930, 224.9696923782719864 ) ) ;
#87992 = ADVANCED_FACE ( 'NONE', ( #88969 ), #20642, .F. ) ;
#87993 = CARTESIAN_POINT ( 'NONE',  ( -6.462730663574999923, 1512.074228084999959, 200.5954301961770057 ) ) ;
#87994 = ORIENTED_EDGE ( 'NONE', *, *, #8299, .F. ) ;
#87995 = CARTESIAN_POINT ( 'NONE',  ( 25.65427092280000210, 1434.769004650220268, 243.9198229472980017 ) ) ;
#87996 = AXIS2_PLACEMENT_3D ( 'NONE', #75860, #108908, #101583 ) ;
#87997 = CARTESIAN_POINT ( 'NONE',  ( 41.49255935287312269, 1443.690926113407841, 136.5669747823052376 ) ) ;
#87998 = CARTESIAN_POINT ( 'NONE',  ( -58.27342821996139577, 1385.074879826650204, 277.9421718526420477 ) ) ;
#87999 = CARTESIAN_POINT ( 'NONE',  ( 41.65675406397859604, 1443.992462633329978, 135.6790809494980010 ) ) ;
#88000 = CARTESIAN_POINT ( 'NONE',  ( 3.529344918850000123, 1506.116810151690061, 220.6266479957990043 ) ) ;
#88001 =( BOUNDED_SURFACE ( )  B_SPLINE_SURFACE ( 1, 2, ( 
 ( #85132, #76195, #42591, #33614, #59967, #52110, #24649, #60516, #93528 ),
 ( #94639, #86240, #16797, #102479, #25768, #109798, #85684, #1161, #35291 ) ),
 .UNSPECIFIED., .F., .T., .F. ) 
 B_SPLINE_SURFACE_WITH_KNOTS ( ( 2, 2 ),
 ( 3, 2, 2, 2, 3 ),
 ( -10000.00000000000000, 10000.00000000000000 ),
 ( 0.000000000000000000, 1.570796326794899889, 3.141592653589790007, 4.712388980384689674, 6.283185307179590673 ),
 .UNSPECIFIED. ) 
 GEOMETRIC_REPRESENTATION_ITEM ( )  RATIONAL_B_SPLINE_SURFACE ( (
 ( 1.000000000000000000, 0.7071067811865480168, 1.000000000000000000, 0.7071067811865480168, 1.000000000000000000, 0.7071067811865480168, 1.000000000000000000, 0.7071067811865480168, 1.000000000000000000),
 ( 1.000000000000000000, 0.7071067811865480168, 1.000000000000000000, 0.7071067811865480168, 1.000000000000000000, 0.7071067811865480168, 1.000000000000000000, 0.7071067811865480168, 1.000000000000000000) ) ) 
 REPRESENTATION_ITEM ( '' )  SURFACE ( )  );
#88002 = EDGE_CURVE ( 'NONE', #74404, #53058, #30155, .T. ) ;
#88003 = CARTESIAN_POINT ( 'NONE',  ( -15.46337283059999912, 1415.677402202029953, 209.5778880887239950 ) ) ;
#88004 = AXIS2_PLACEMENT_3D ( 'NONE', #17210, #110758, #67679 ) ;
#88006 = ORIENTED_EDGE ( 'NONE', *, *, #55075, .F. ) ;
#88005 = CARTESIAN_POINT ( 'NONE',  ( -1.771280571366619982, 1515.064792319160006, 204.7923971709010118 ) ) ;
#88007 = CARTESIAN_POINT ( 'NONE',  ( -15.92986207429999901, 1416.139014782290133, 209.7537124246929920 ) ) ;
#88008 = CARTESIAN_POINT ( 'NONE',  ( -24.09814796439999895, 1444.255765020069930, 212.5772278521379803 ) ) ;
#88009 = CARTESIAN_POINT ( 'NONE',  ( -1.426943104832486098, 1450.672165367667276, 154.2643989290685909 ) ) ;
#88010 = CARTESIAN_POINT ( 'NONE',  ( -1.484755140834890019, 1429.714486269279860, 199.8512846474560263 ) ) ;
#88011 = CARTESIAN_POINT ( 'NONE',  ( 15.33574361303499956, 1514.703592237370003, 224.8569613759669892 ) ) ;
#88012 = CARTESIAN_POINT ( 'NONE',  ( 28.00492654830749828, 1509.968806677990187, 194.4672643161270003 ) ) ;
#88013 = LINE ( 'NONE', #62265, #91402 ) ;
#88014 = CARTESIAN_POINT ( 'NONE',  ( -13.53916864874639892, 1429.119333790580185, 222.2883575635510169 ) ) ;
#88015 = CARTESIAN_POINT ( 'NONE',  ( 13.33339459179999942, 1417.421582639030021, 228.6994961110980000 ) ) ;
#88016 = CARTESIAN_POINT ( 'NONE',  ( -8.895549977471178593, 1462.225664532283872, 227.1186910807994934 ) ) ;
#88017 = CARTESIAN_POINT ( 'NONE',  ( -16.78296769010000133, 1460.265262334630279, 228.3353431369980058 ) ) ;
#88018 = CARTESIAN_POINT ( 'NONE',  ( -0.01323705180209850014, 1516.939658295650133, 206.6356258303270010 ) ) ;
#88019 = CARTESIAN_POINT ( 'NONE',  ( 43.71400391259999907, 1430.030208370729952, 266.2448334172979685 ) ) ;
#88020 = CARTESIAN_POINT ( 'NONE',  ( -17.58047195769999860, 1409.526983996129957, 222.6194513965980093 ) ) ;
#88021 = CARTESIAN_POINT ( 'NONE',  ( 16.98962153889999627, 1435.906362427300110, 148.1094881728979828 ) ) ;
#88022 = CARTESIAN_POINT ( 'NONE',  ( 22.63564133870000106, 1508.009850363030182, 193.1501364738980158 ) ) ;
#88023 = CARTESIAN_POINT ( 'NONE',  ( 29.43773002077689682, 1509.946928101494450, 206.9696982396478688 ) ) ;
#88024 = CARTESIAN_POINT ( 'NONE',  ( 1.925297170580940076, 1522.051704408389924, 230.6853930747409720 ) ) ;
#88025 = CARTESIAN_POINT ( 'NONE',  ( -1.000362776118160035E-16, 1517.151704408390060, 209.1218459616989946 ) ) ;
#88026 = CARTESIAN_POINT ( 'NONE',  ( -15.39825232982659919, 1418.148438324100198, 203.0909429379779851 ) ) ;
#88027 = CARTESIAN_POINT ( 'NONE',  ( -40.99906703070779912, 1440.733582855520126, 136.2526507852639952 ) ) ;
#88028 = CARTESIAN_POINT ( 'NONE',  ( -8.345511106849999194, 1409.144376880429945, 197.3321607578980093 ) ) ;
#88029 = CARTESIAN_POINT ( 'NONE',  ( -15.89396736049999959, 1416.225531559500041, 209.0250895600429999 ) ) ;
#88030 = CARTESIAN_POINT ( 'NONE',  ( -12.01638140429999879, 1440.881463611970048, 187.8051733414979765 ) ) ;
#88031 = CARTESIAN_POINT ( 'NONE',  ( -7.543275436179440518, 1384.798777593330215, 219.0854894083749969 ) ) ;
#88032 = CARTESIAN_POINT ( 'NONE',  ( -33.13365747560000329, 1435.654560788539811, 135.0902693358980287 ) ) ;
#88033 = CARTESIAN_POINT ( 'NONE',  ( -32.37018134260392088, 1512.187213306747481, 218.0712926453366833 ) ) ;
#88034 = ORIENTED_EDGE ( 'NONE', *, *, #23088, .F. ) ;
#88035 = CARTESIAN_POINT ( 'NONE',  ( 5.912224431970154015, 1510.631883404490736, 216.6440474061008388 ) ) ;
#88036 = CARTESIAN_POINT ( 'NONE',  ( -12.13069928485440130, 1409.336673740850074, 217.8481747060740190 ) ) ;
#88037 = CARTESIAN_POINT ( 'NONE',  ( -18.80299996640602700, 1468.065468973505176, 202.3792621952166257 ) ) ;
#88038 = CARTESIAN_POINT ( 'NONE',  ( -13.03265074581759997, 1508.448609993070022, 209.7186198884500072 ) ) ;
#88039 = CARTESIAN_POINT ( 'NONE',  ( -3.804428602223190126, 1420.825805556418345, 137.2934056698748861 ) ) ;
#88040 = CARTESIAN_POINT ( 'NONE',  ( -45.67177334430000712, 1440.913039353769818, 266.1885934045980093 ) ) ;
#88041 = CARTESIAN_POINT ( 'NONE',  ( -29.30029655192950244, 1525.907212628473644, 196.8717316207788315 ) ) ;
#88042 = CARTESIAN_POINT ( 'NONE',  ( 11.75869035456349998, 1521.951704408389787, 227.2994842691620079 ) ) ;
#88043 = CARTESIAN_POINT ( 'NONE',  ( 20.39893125377741612, 1526.069472839382115, 233.1323736274815701 ) ) ;
#88044 = CARTESIAN_POINT ( 'NONE',  ( -109.0035882723349943, 1384.583473043429876, 311.2498069574970714 ) ) ;
#88045 = CARTESIAN_POINT ( 'NONE',  ( -47.75334323544549875, 1385.011498351640057, 221.9354493742870034 ) ) ;
#88046 = DIRECTION ( 'NONE',  ( -1.755985294532469921E-16, 1.000000000000000000, -1.338183447452831989E-16 ) ) ;
#88047 = DIRECTION ( 'NONE',  ( 0.000000000000000000, 0.000000000000000000, -1.000000000000000000 ) ) ;
#88048 = CARTESIAN_POINT ( 'NONE',  ( 13.88551022039999872, 1452.408285299329918, 223.3855399223979816 ) ) ;
#88049 = CARTESIAN_POINT ( 'NONE',  ( 1.581901184577762853, 1426.946688134061105, 137.0999999980979851 ) ) ;
#88050 = CARTESIAN_POINT ( 'NONE',  ( 4.517196230222680242, 1517.151704408390060, 227.6318199458918343 ) ) ;
#88051 = CARTESIAN_POINT ( 'NONE',  ( -7.966031924080000159, 1384.919940016020064, 199.4892488166489670 ) ) ;
#88052 = CARTESIAN_POINT ( 'NONE',  ( -23.95637140939999910, 1411.110463997629950, 208.0703336090279834 ) ) ;
#88053 = CARTESIAN_POINT ( 'NONE',  ( 17.37509876899999739, 1416.823418193329871, 203.7862089741079785 ) ) ;
#88054 = CIRCLE ( 'NONE', #39752, 2.000000000000003553 ) ;
#88055 = CARTESIAN_POINT ( 'NONE',  ( -11.95789827870000011, 1415.263254644529979, 195.6584547795980029 ) ) ;
#88056 = LINE ( 'NONE', #72356, #28266 ) ;
#88057 = CARTESIAN_POINT ( 'NONE',  ( 23.48803479300000063, 1409.897858449729938, 209.7858158176040035 ) ) ;
#88058 = CARTESIAN_POINT ( 'NONE',  ( 11.43185072513739797, 1443.913060387330006, 147.9056598087979921 ) ) ;
#88059 = CARTESIAN_POINT ( 'NONE',  ( 0.8763902003015829889, 1462.562412067790092, 230.5019338175040104 ) ) ;
#88060 = CARTESIAN_POINT ( 'NONE',  ( -5.360200749763491146, 1422.242249887159915, 144.4955016248619870 ) ) ;
#88062 = CARTESIAN_POINT ( 'NONE',  ( -12.26635723510000098, 1379.122879128199884, 206.2237812648789941 ) ) ;
#88061 = CARTESIAN_POINT ( 'NONE',  ( -11.86563472409999953, 1432.300011745260008, 149.9825370587979876 ) ) ;
#88063 = CARTESIAN_POINT ( 'NONE',  ( -4.995284477430000258, 1391.732982068790079, 203.5424665078789985 ) ) ;
#88064 = CARTESIAN_POINT ( 'NONE',  ( -103.0889951380000014, 1378.528619065189559, 306.8546778052111108 ) ) ;
#88065 = CARTESIAN_POINT ( 'NONE',  ( -10.47439550540000042, 1490.889281562089991, 212.4388770995890070 ) ) ;
#88066 = CARTESIAN_POINT ( 'NONE',  ( -15.36549427709999982, 1420.352425059129928, 229.0210324418980008 ) ) ;
#88067 = CARTESIAN_POINT ( 'NONE',  ( 9.677596299730000240, 1463.237928047889909, 210.5383460088689844 ) ) ;
#88068 = CARTESIAN_POINT ( 'NONE',  ( 4.999456390405000228, 1516.830644417779922, 204.5005780481670001 ) ) ;
#88069 = FACE_OUTER_BOUND ( 'NONE', #42583, .T. ) ;
#88070 = CARTESIAN_POINT ( 'NONE',  ( -15.44463253599880126, 1485.324514085619967, 187.2482728325680057 ) ) ;
#88071 = AXIS2_PLACEMENT_3D ( 'NONE', #9339, #75986, #33976 ) ;
#88072 = CARTESIAN_POINT ( 'NONE',  ( 12.21456615412630065, 1501.625727090829969, 212.8586461374000010 ) ) ;
#88073 = CARTESIAN_POINT ( 'NONE',  ( -10.88610090654533913, 1422.259895732163159, 210.6369494421302875 ) ) ;
#88075 = ORIENTED_EDGE ( 'NONE', *, *, #15689, .F. ) ;
#88074 = CARTESIAN_POINT ( 'NONE',  ( -63.34523448999999573, 1379.747030511940238, 271.7626510974590133 ) ) ;
#88076 = ORIENTED_EDGE ( 'NONE', *, *, #88332, .F. ) ;
#88077 = CARTESIAN_POINT ( 'NONE',  ( 26.88905145119999673, 1508.006187447730099, 215.2211436898180068 ) ) ;
#88078 = ORIENTED_EDGE ( 'NONE', *, *, #58323, .T. ) ;
#88079 = CARTESIAN_POINT ( 'NONE',  ( 20.49599333844834348, 1525.960063244517187, 184.3798832129035077 ) ) ;
#88080 = CARTESIAN_POINT ( 'NONE',  ( 1.499137301480000017, 1414.988015881329829, 191.7262494052980060 ) ) ;
#88082 = CARTESIAN_POINT ( 'NONE',  ( 1.448681958479999921, 1507.129709326030024, 181.1126016739980003 ) ) ;
#88081 = CARTESIAN_POINT ( 'NONE',  ( -15.69204124918606169, 1410.669730017232723, 226.7211433092322466 ) ) ;
#88083 = CARTESIAN_POINT ( 'NONE',  ( -2.713960167710639967E-10, 1417.262443616730025, 235.9145977375980010 ) ) ;
#88084 = CARTESIAN_POINT ( 'NONE',  ( -24.06633326386470273, 1452.067469986559900, 136.8844249806119819 ) ) ;
#88085 = CARTESIAN_POINT ( 'NONE',  ( -1.921751667499999927, 1468.480854157690146, 219.3342396420989928 ) ) ;
#88086 = CARTESIAN_POINT ( 'NONE',  ( 12.86744022639999940, 1409.362401301430054, 227.0135731152979872 ) ) ;
#88087 = EDGE_CURVE ( 'NONE', #41783, #54360, #2242, .T. ) ;
#88088 = CARTESIAN_POINT ( 'NONE',  ( -4.028307778284999863, 1516.797038924770050, 212.3881954442970255 ) ) ;
#88089 = CARTESIAN_POINT ( 'NONE',  ( 39.02661178044039758, 1437.758897875479761, 134.0999999974839909 ) ) ;
#88090 = CARTESIAN_POINT ( 'NONE',  ( -9.997338218269998578, 1422.621669173350028, 210.6353445619989770 ) ) ;
#88091 = CARTESIAN_POINT ( 'NONE',  ( -8.991629940588330427, 1509.227055023859975, 237.0095830223739881 ) ) ;
#88092 = ORIENTED_EDGE ( 'NONE', *, *, #96519, .T. ) ;
#88093 = CARTESIAN_POINT ( 'NONE',  ( 14.43085696089999992, 1426.807557149800004, 195.4949581795989957 ) ) ;
#88094 = FACE_OUTER_BOUND ( 'NONE', #9096, .T. ) ;
#88095 = ORIENTED_EDGE ( 'NONE', *, *, #88529, .F. ) ;
#88096 = ORIENTED_EDGE ( 'NONE', *, *, #41297, .T. ) ;
#88097 = ORIENTED_EDGE ( 'NONE', *, *, #15882, .T. ) ;
#88098 = CARTESIAN_POINT ( 'NONE',  ( -8.502796056335000685, 1512.371933174390051, 215.9657241866970026 ) ) ;
#88099 = CARTESIAN_POINT ( 'NONE',  ( -0.3530891476770000037, 1467.116854362329832, 235.6078141479979990 ) ) ;
#88100 = DIRECTION ( 'NONE',  ( -0.6736849260863841948, 0.000000000000000000, 0.7390186874254148774 ) ) ;
#88101 = CARTESIAN_POINT ( 'NONE',  ( -2.903124885889999618, 1484.703481644929980, 183.2972796410979868 ) ) ;
#88102 = CARTESIAN_POINT ( 'NONE',  ( 2.902893324140370268, 1466.180773484049951, 198.4663733987970033 ) ) ;
#88103 = CARTESIAN_POINT ( 'NONE',  ( -18.86884385042500156, 1508.513763835350119, 210.1416286062879806 ) ) ;
#88104 = CARTESIAN_POINT ( 'NONE',  ( -56.30397432574992678, 1379.711908693320993, 253.0148838135297638 ) ) ;
#88105 = CARTESIAN_POINT ( 'NONE',  ( 4.222485211202849698, 1446.229405227499910, 167.6248456503689681 ) ) ;
#88106 = ADVANCED_FACE ( 'NONE', ( #80581 ), #107396, .F. ) ;
#88107 = CARTESIAN_POINT ( 'NONE',  ( 0.3138303437369999727, 1507.644171354529817, 237.4220927994979888 ) ) ;
#88108 = ORIENTED_EDGE ( 'NONE', *, *, #96646, .F. ) ;
#88109 = CARTESIAN_POINT ( 'NONE',  ( 2.863787855735000054, 1516.788317650260069, 207.4054531903269947 ) ) ;
#88110 = ORIENTED_EDGE ( 'NONE', *, *, #104508, .F. ) ;
#88111 = CARTESIAN_POINT ( 'NONE',  ( 27.15528332431300029, 1440.913060387330006, 245.4436605369820086 ) ) ;
#88112 = CARTESIAN_POINT ( 'NONE',  ( 11.35705511386439959, 1478.717693206790045, 206.1553733900099985 ) ) ;
#88113 = EDGE_LOOP ( 'NONE', ( #72291, #98989, #82295, #77114 ) ) ;
#88114 = CARTESIAN_POINT ( 'NONE',  ( -6.140086983543329602, 1508.880866264950100, 201.6144240918179946 ) ) ;
#88115 = EDGE_CURVE ( 'NONE', #50172, #70893, #4268, .T. ) ;
#88116 = CARTESIAN_POINT ( 'NONE',  ( -15.00325987230000102, 1410.369181960630158, 190.7724269911979889 ) ) ;
#88117 = CARTESIAN_POINT ( 'NONE',  ( -48.14807380225922628, 1379.685700880162813, 242.2423365738800101 ) ) ;
#88119 = CARTESIAN_POINT ( 'NONE',  ( -113.4000000000000057, 1379.013060387289897, 304.2218459572590064 ) ) ;
#88118 = CARTESIAN_POINT ( 'NONE',  ( -24.49730784189999966, 1441.139193927939914, 211.0002140101279906 ) ) ;
#88120 = CARTESIAN_POINT ( 'NONE',  ( 22.52079200403399994, 1410.876293387520036, 206.2022394633299882 ) ) ;
#88121 = CARTESIAN_POINT ( 'NONE',  ( -4.803664197750522748E-06, 1397.577875906359623, 196.1218455414115738 ) ) ;
#88122 = CARTESIAN_POINT ( 'NONE',  ( -12.69533288745581068, 1434.600403889475274, 147.1709292336272483 ) ) ;
#88123 = CARTESIAN_POINT ( 'NONE',  ( 7.848979634317430509, 1517.151704408390060, 215.9448598632019980 ) ) ;
#88124 = CARTESIAN_POINT ( 'NONE',  ( -5.690400742829999636, 1508.048825776489821, 220.5583476148989917 ) ) ;
#88126 = CARTESIAN_POINT ( 'NONE',  ( 18.30025784240000064, 1431.961054190390087, 210.0255047360110154 ) ) ;
#88125 = CARTESIAN_POINT ( 'NONE',  ( 9.935511340089998811, 1462.885007474029862, 233.7276471281980150 ) ) ;
#88127 = CARTESIAN_POINT ( 'NONE',  ( -7.328049318385000177, 1516.809497469189864, 215.6772390872569929 ) ) ;
#88128 = DIRECTION ( 'NONE',  ( 0.8832694794843597430, 0.3761007072180699295, -0.2799701495543689411 ) ) ;
#88129 = CARTESIAN_POINT ( 'NONE',  ( 6.150612979054229434, 1511.023286695659863, 216.6047038587689997 ) ) ;
#88130 = DIRECTION ( 'NONE',  ( -1.755985294532469921E-16, 1.000000000000000000, -1.338183447452831989E-16 ) ) ;
#88131 = CARTESIAN_POINT ( 'NONE',  ( -5.772403812434999892, 1516.676340709600026, 212.3853678745870184 ) ) ;
#88132 = CARTESIAN_POINT ( 'NONE',  ( -20.42904319129999635, 1470.816572149929925, 209.3526706922980054 ) ) ;
#88133 = EDGE_CURVE ( 'NONE', #74812, #40553, #68695, .T. ) ;
#88134 = CARTESIAN_POINT ( 'NONE',  ( 29.79244516856374858, 1525.556089352344770, 221.4002000438143511 ) ) ;
#88136 = VERTEX_POINT ( 'NONE', #33324 ) ;
#88135 = CARTESIAN_POINT ( 'NONE',  ( -98.84258614210000360, 1386.766722940489899, 296.3872529111589529 ) ) ;
#88137 = CARTESIAN_POINT ( 'NONE',  ( -16.86500412379770708, 1525.697946996610881, 236.3931742940298193 ) ) ;
#88138 = CARTESIAN_POINT ( 'NONE',  ( -1.296432797589999879E-09, 1463.596605969329858, 232.0486588194980015 ) ) ;
#88139 = CARTESIAN_POINT ( 'NONE',  ( -5.169271338600384347, 1487.151140008964830, 220.0115120792558798 ) ) ;
#88140 = CARTESIAN_POINT ( 'NONE',  ( -15.66247007830000015, 1415.943430100450087, 208.3724989932889855 ) ) ;
#88141 = CARTESIAN_POINT ( 'NONE',  ( 2.921722053920000395, 1414.540823234730169, 231.8164568075980014 ) ) ;
#88142 = CARTESIAN_POINT ( 'NONE',  ( -18.76806136029999905, 1457.583373696730177, 227.2045900892980228 ) ) ;
#88144 = CARTESIAN_POINT ( 'NONE',  ( 5.379505748067900051, 1430.582098177589842, 154.4820892377710209 ) ) ;
#88143 = CARTESIAN_POINT ( 'NONE',  ( 11.58007378539999976, 1432.582704238630186, 151.1961013072979938 ) ) ;
#88145 = CARTESIAN_POINT ( 'NONE',  ( -9.881594800496241504, 1448.777576682979770, 207.8817744914870218 ) ) ;
#88146 = CARTESIAN_POINT ( 'NONE',  ( -106.1744482317629945, 1381.515665816750015, 309.3820691888080319 ) ) ;
#88147 = ORIENTED_EDGE ( 'NONE', *, *, #94723, .F. ) ;
#88148 = CARTESIAN_POINT ( 'NONE',  ( 3.255340926295000159, 1516.962555622980062, 204.4977466407669908 ) ) ;
#88149 = CARTESIAN_POINT ( 'NONE',  ( 0.7720380218979999709, 1406.269671972929928, 269.2944987139979958 ) ) ;
#88150 = CARTESIAN_POINT ( 'NONE',  ( -1.093792492990000031, 1515.225200552689785, 213.4470939808389858 ) ) ;
#88151 = CARTESIAN_POINT ( 'NONE',  ( 12.75661095148570112, 1470.549711631520040, 269.3476708060779856 ) ) ;
#88152 = CARTESIAN_POINT ( 'NONE',  ( 2.478043214419999973, 1440.127217985849938, 157.7918389896980216 ) ) ;
#88153 = CARTESIAN_POINT ( 'NONE',  ( 10.33594274554624803, 1423.067651820833134, 137.1941078872085882 ) ) ;
#88154 = CARTESIAN_POINT ( 'NONE',  ( -38.15894704684880168, 1440.913060390959799, 256.5354463518759758 ) ) ;
#88155 = CARTESIAN_POINT ( 'NONE',  ( 37.12869866823530174, 1449.463881992789993, 136.3003431950029949 ) ) ;
#88156 = CARTESIAN_POINT ( 'NONE',  ( 1.425556924595323238, 1450.669415802774438, 154.2648944982862247 ) ) ;
#88157 = CARTESIAN_POINT ( 'NONE',  ( 0.0001408309371566590163, 1408.913070111550269, 186.4658721391990071 ) ) ;
#88158 = CARTESIAN_POINT ( 'NONE',  ( 0.8736373785452179463, 1450.882552294920060, 154.7893692902700025 ) ) ;
#88159 = B_SPLINE_CURVE_WITH_KNOTS ( 'NONE', 3,
 ( #29185, #95835, #79062, #36481 ),
 .UNSPECIFIED., .F., .F.,
 ( 4, 4 ),
 ( 0.000000000000000000, 1.000000000000000000 ),
 .UNSPECIFIED. ) ;
#88160 = CARTESIAN_POINT ( 'NONE',  ( 2.484221813290000025, 1505.974367507990110, 221.6747987149990138 ) ) ;
#88161 = CARTESIAN_POINT ( 'NONE',  ( 3.448830483803564828, 1512.187213306747481, 243.0842028158767789 ) ) ;
#88162 = ORIENTED_EDGE ( 'NONE', *, *, #55256, .F. ) ;
#88163 = CARTESIAN_POINT ( 'NONE',  ( -36.06124927020000115, 1436.776486029860052, 262.6648722463980334 ) ) ;
#88164 = CARTESIAN_POINT ( 'NONE',  ( 3.082592223099999806, 1485.754465970690035, 198.7996944297989899 ) ) ;
#88165 = CARTESIAN_POINT ( 'NONE',  ( 10.48885285482030127, 1469.765830575109931, 206.0548704900310213 ) ) ;
#88166 = CARTESIAN_POINT ( 'NONE',  ( -0.5589532248799999881, 1476.047851565629799, 268.4836504708979987 ) ) ;
#88167 = CARTESIAN_POINT ( 'NONE',  ( -4.291175242752039765, 1446.971469842819943, 154.7965863647420122 ) ) ;
#88168 = CARTESIAN_POINT ( 'NONE',  ( -33.93019615849274828, 1522.906561336852974, 197.6607374646097810 ) ) ;
#88169 = CARTESIAN_POINT ( 'NONE',  ( -2.973630401571459636, 1448.268562863430816, 184.4328599109281299 ) ) ;
#88170 = CARTESIAN_POINT ( 'NONE',  ( -23.36861497038490043, 1384.851536731240003, 222.6440924076069905 ) ) ;
#88171 = CARTESIAN_POINT ( 'NONE',  ( -2.500000000000000000, 1448.894380913990062, 169.3595559471979755 ) ) ;
#88172 = CARTESIAN_POINT ( 'NONE',  ( 26.45092774933420188, 1436.256316748539803, 136.6768279046889916 ) ) ;
#88173 = CARTESIAN_POINT ( 'NONE',  ( -4.353139012478820291, 1396.065075352050144, 219.2571886206609975 ) ) ;
#88174 = CARTESIAN_POINT ( 'NONE',  ( -15.34713811569999997, 1421.556258866430198, 227.2905572623980106 ) ) ;
#88175 = CARTESIAN_POINT ( 'NONE',  ( -16.65620699048979603, 1409.595037377370090, 225.3660632515070290 ) ) ;
#88176 = FACE_OUTER_BOUND ( 'NONE', #7179, .T. ) ;
#88177 = ORIENTED_EDGE ( 'NONE', *, *, #79257, .T. ) ;
#88178 = CARTESIAN_POINT ( 'NONE',  ( -20.86054011819999943, 1508.959477709930070, 190.3575368045979985 ) ) ;
#88179 = CARTESIAN_POINT ( 'NONE',  ( 1.498833634909999990, 1408.965400811229983, 230.5914988299979882 ) ) ;
#88180 = CARTESIAN_POINT ( 'NONE',  ( -12.71625625589999942, 1484.464918063330060, 185.9897890590980012 ) ) ;
#88182 = CARTESIAN_POINT ( 'NONE',  ( -14.37690903976499968, 1514.216506490359961, 192.5504339357670176 ) ) ;
#88181 = CARTESIAN_POINT ( 'NONE',  ( 11.38204197729999834, 1426.011755914629930, 126.2834675746979940 ) ) ;
#88183 = CARTESIAN_POINT ( 'NONE',  ( 11.60004869885203682, 1428.983126981193436, 134.0999999980966777 ) ) ;
#88184 = CARTESIAN_POINT ( 'NONE',  ( -13.51610093808350577, 1445.063428794548372, 151.4871142704430156 ) ) ;
#88185 = CARTESIAN_POINT ( 'NONE',  ( -109.9857364230449974, 1384.899971927750130, 311.4562996732899478 ) ) ;
#88186 = CARTESIAN_POINT ( 'NONE',  ( 7.751138421380000310, 1424.420707150859926, 212.0424422646189839 ) ) ;
#88187 = CARTESIAN_POINT ( 'NONE',  ( -7.320561577120000329, 1432.353341358199941, 149.5448088695980005 ) ) ;
#88188 = CARTESIAN_POINT ( 'NONE',  ( 2.588559417869999546, 1508.984568548630023, 179.8910387445980064 ) ) ;
#88189 = DIRECTION ( 'NONE',  ( -0.8926073982886787439, 0.000000000000000000, -0.4508348173337058951 ) ) ;
#88190 = CARTESIAN_POINT ( 'NONE',  ( -60.47573540665300129, 1377.428416197120214, 271.2551842102760133 ) ) ;
#88191 = CARTESIAN_POINT ( 'NONE',  ( 7.834673235704612715, 1365.208883084832678, 209.6218459617148824 ) ) ;
#88193 = ORIENTED_EDGE ( 'NONE', *, *, #12306, .F. ) ;
#88192 = CARTESIAN_POINT ( 'NONE',  ( -13.14000761400309969, 1461.232465202761659, 232.8227669047252846 ) ) ;
#88194 = ORIENTED_EDGE ( 'NONE', *, *, #98017, .F. ) ;
#88195 = CARTESIAN_POINT ( 'NONE',  ( 0.3722769099684289928, 1457.826255237599980, 228.9731060096619899 ) ) ;
#88196 = CARTESIAN_POINT ( 'NONE',  ( -13.51610093809999924, 1443.913060387330006, 169.3501091259980171 ) ) ;
#88197 = CARTESIAN_POINT ( 'NONE',  ( -22.37341732390000004, 1435.279001492648831, 139.8076879873978839 ) ) ;
#88198 = CARTESIAN_POINT ( 'NONE',  ( -8.324963459575000613, 1511.468585915670019, 214.5031579459970033 ) ) ;
#88200 = CARTESIAN_POINT ( 'NONE',  ( -1.318069841409999832, 1486.109660646130123, 181.8447665737980117 ) ) ;
#88199 = CARTESIAN_POINT ( 'NONE',  ( -105.5826496779999957, 1391.887501467710081, 304.2218457088590071 ) ) ;
#88201 = CARTESIAN_POINT ( 'NONE',  ( -31.88715249297895227, 1525.425686270224560, 201.2219484344741147 ) ) ;
#88202 = FACE_OUTER_BOUND ( 'NONE', #34401, .T. ) ;
#88203 = CARTESIAN_POINT ( 'NONE',  ( -41.65674201940959875, 1443.992456074669917, 135.6790666823760034 ) ) ;
#88204 =( NAMED_UNIT ( * ) SI_UNIT ( $, .STERADIAN. ) SOLID_ANGLE_UNIT ( ) );
#88205 = CARTESIAN_POINT ( 'NONE',  ( -2.500000000000000000, 1448.711455262680147, 157.7219972398099799 ) ) ;
#88206 = CARTESIAN_POINT ( 'NONE',  ( 3.934203666168589297, 1370.083327362674481, 207.6218459616987673 ) ) ;
#88207 = CARTESIAN_POINT ( 'NONE',  ( 2.285841285774699520E-15, 1391.426148861440197, 209.1218459572589836 ) ) ;
#88208 = CARTESIAN_POINT ( 'NONE',  ( 5.200164090505730256E-05, 1406.777850256470174, 269.6501335340969945 ) ) ;
#88209 = CARTESIAN_POINT ( 'NONE',  ( 40.71480606090000265, 1443.734517994560065, 137.1148378138979922 ) ) ;
#88210 = ORIENTED_EDGE ( 'NONE', *, *, #99506, .T. ) ;
#88211 = CARTESIAN_POINT ( 'NONE',  ( -11.57603212119999903, 1432.304338525750154, 151.1967213783980242 ) ) ;
#88212 = CARTESIAN_POINT ( 'NONE',  ( 12.25335341949999979, 1440.953202899389908, 188.4028591661979704 ) ) ;
#88213 = ORIENTED_EDGE ( 'NONE', *, *, #73718, .F. ) ;
#88214 = ORIENTED_EDGE ( 'NONE', *, *, #32949, .T. ) ;
#88215 = CARTESIAN_POINT ( 'NONE',  ( -3.497772968360000512, 1454.175141309589890, 199.2405839609089924 ) ) ;
#88216 = CARTESIAN_POINT ( 'NONE',  ( -9.692061980449999226, 1363.802329763670059, 207.6218459616989946 ) ) ;
#88217 = CARTESIAN_POINT ( 'NONE',  ( 5.781490544344999982, 1516.807958722750072, 215.6734893570070142 ) ) ;
#88218 = CARTESIAN_POINT ( 'NONE',  ( 2.385772184054999911, 1512.160709093490141, 216.7163506116569920 ) ) ;
#88219 = B_SPLINE_SURFACE_WITH_KNOTS ( 'NONE', 5, 5, ( 
 ( #101493, #82524, #50578, #109926, #108817, #100417 ),
 ( #23699, #57884, #83604, #6902, #39960, #41057 ),
 ( #15823, #109386, #32663, #100950, #50028, #7459 ),
 ( #41621, #102055, #33205, #59533, #67395, #24781 ),
 ( #84706, #8005, #76323, #110473, #51682, #16927 ),
 ( #9657, #18052, #1282, #69610, #43829, #8553 ),
 ( #9119, #85820, #76883, #733, #27031, #104837 ),
 ( #53351, #193, #94774, #35423, #86373, #104285 ),
 ( #60093, #68495, #70174, #103730, #61220, #95882 ) ),
 .UNSPECIFIED., .F., .F., .F.,
 ( 6, 3, 6 ),
 ( 6, 6 ),
 ( 3.046255633294209897, 5.238805263900000675, 7.431354894495790120 ),
 ( -0.0004283937457940030003, 2.000000000000000000 ),
 .UNSPECIFIED. ) ;
#88220 = B_SPLINE_CURVE_WITH_KNOTS ( 'NONE', 3,
 ( #109856, #16311, #84089, #51607 ),
 .UNSPECIFIED., .F., .F.,
 ( 4, 4 ),
 ( -96.65569485166331276, -19.64510849129999315 ),
 .UNSPECIFIED. ) ;
#88221 = ORIENTED_EDGE ( 'NONE', *, *, #74901, .T. ) ;
#88222 = CARTESIAN_POINT ( 'NONE',  ( -12.33252012447020185, 1378.517259983480017, 208.8147234695160250 ) ) ;
#88223 = CARTESIAN_POINT ( 'NONE',  ( -70.57508978779999609, 1378.817654444100071, 279.4267215249590208 ) ) ;
#88224 = ADVANCED_FACE ( 'NONE', ( #77014 ), #14425, .T. ) ;
#88225 = CARTESIAN_POINT ( 'NONE',  ( 12.22918761389999887, 1416.219761280829971, 223.5054628756979866 ) ) ;
#88226 = CARTESIAN_POINT ( 'NONE',  ( -0.01306004006829850073, 1516.939762005280045, 204.5032625402269844 ) ) ;
#88227 = CARTESIAN_POINT ( 'NONE',  ( 18.87853829029999986, 1458.344553362990155, 213.8102309971890236 ) ) ;
#88228 = EDGE_CURVE ( 'NONE', #64952, #81429, #66297, .T. ) ;
#88229 = CARTESIAN_POINT ( 'NONE',  ( -42.06231979437640689, 1440.913089571769888, 269.6487552725350270 ) ) ;
#88230 = CARTESIAN_POINT ( 'NONE',  ( 6.554778533645000849, 1516.929962200689943, 201.4024535497269994 ) ) ;
#88231 = CARTESIAN_POINT ( 'NONE',  ( -11.34430840129999929, 1409.809597392229989, 228.6274365818979959 ) ) ;
#88233 = ORIENTED_EDGE ( 'NONE', *, *, #32082, .T. ) ;
#88232 = CARTESIAN_POINT ( 'NONE',  ( -7.313096896839999417, 1447.188565721670102, 185.7316950759980045 ) ) ;
#88234 = CARTESIAN_POINT ( 'NONE',  ( 2.446787376320000096, 1432.353341358199941, 150.2884730787980061 ) ) ;
#88235 = CARTESIAN_POINT ( 'NONE',  ( -25.97046658602729963, 1440.913060480119839, 221.7145558740930085 ) ) ;
#88236 = CARTESIAN_POINT ( 'NONE',  ( 18.66420869458061205, 1526.382868172863937, 232.7837831374278039 ) ) ;
#88237 = CARTESIAN_POINT ( 'NONE',  ( 16.76344481147369336, 1422.586955737515609, 227.0118626232063832 ) ) ;
#88238 = CARTESIAN_POINT ( 'NONE',  ( 41.65086068609159753, 1427.189777683049897, 269.7492451942990215 ) ) ;
#88239 = CARTESIAN_POINT ( 'NONE',  ( 5.786527562335000319, 1517.025653221279981, 212.5728793591970032 ) ) ;
#88240 = CARTESIAN_POINT ( 'NONE',  ( -66.62763224750000290, 1379.742540601970177, 275.7011351548590028 ) ) ;
#88241 = CARTESIAN_POINT ( 'NONE',  ( -25.78156655170059608, 1509.813372604039841, 223.1298223243570078 ) ) ;
#88242 = CARTESIAN_POINT ( 'NONE',  ( -31.16645442585705084, 1524.201670966335314, 221.8713816554661094 ) ) ;
#88243 = CARTESIAN_POINT ( 'NONE',  ( 19.18685276606920453, 1410.944740066537406, 195.6341497936866176 ) ) ;
#88244 = CARTESIAN_POINT ( 'NONE',  ( -5.775625115495000017, 1516.745833913490060, 209.8771724060850090 ) ) ;
#88245 = ORIENTED_EDGE ( 'NONE', *, *, #100687, .T. ) ;
#88246 = DIRECTION ( 'NONE',  ( 0.000000000000000000, -1.836970198721029688E-16, -1.000000000000000000 ) ) ;
#88247 = CARTESIAN_POINT ( 'NONE',  ( -0.8146824607389999695, 1415.382299376130049, 233.3155241476979995 ) ) ;
#88248 = CARTESIAN_POINT ( 'NONE',  ( -76.10119759110000359, 1384.646775243249976, 301.2182732922589707 ) ) ;
#88249 = ORIENTED_EDGE ( 'NONE', *, *, #72103, .F. ) ;
#88250 = CARTESIAN_POINT ( 'NONE',  ( -35.41017701237090165, 1385.207010604219931, 234.7551950391080027 ) ) ;
#88251 = CARTESIAN_POINT ( 'NONE',  ( -3.304790277399999976, 1430.055923981690057, 201.4699411825889968 ) ) ;
#88252 = CARTESIAN_POINT ( 'NONE',  ( 18.49907080295740158, 1478.712406274740033, 228.6789878470059989 ) ) ;
#88253 = CARTESIAN_POINT ( 'NONE',  ( -24.68077630836099701, 1437.736159206269804, 210.5119845322900005 ) ) ;
#88254 = DIRECTION ( 'NONE',  ( -0.4198226673190288971, 7.712017286126290910E-17, -0.9076061524720597795 ) ) ;
#88255 = CARTESIAN_POINT ( 'NONE',  ( -0.3485419179389999678, 1410.306756102429972, 233.2101795455980096 ) ) ;
#88256 = CARTESIAN_POINT ( 'NONE',  ( 0.03428106877207290348, 1420.445078887740010, 182.6743165705210004 ) ) ;
#88257 = CIRCLE ( 'NONE', #107904, 4.000000000000003553 ) ;
#88258 = CARTESIAN_POINT ( 'NONE',  ( -7.326795561505000443, 1516.760434454289907, 214.9020780475669881 ) ) ;
#88259 = CARTESIAN_POINT ( 'NONE',  ( -3.338347951516314360, 1495.922107008597777, 197.9787877121366648 ) ) ;
#88260 = CARTESIAN_POINT ( 'NONE',  ( 10.86756440871599949, 1470.431609380819964, 207.9091087289500308 ) ) ;
#88261 = ORIENTED_EDGE ( 'NONE', *, *, #39236, .F. ) ;
#88262 = CARTESIAN_POINT ( 'NONE',  ( -11.46011354710740093, 1414.971717244360207, 196.6341504491270200 ) ) ;
#88263 = CARTESIAN_POINT ( 'NONE',  ( -11.54918848589999847, 1490.513422156330080, 183.1734117734980316 ) ) ;
#88264 = EDGE_LOOP ( 'NONE', ( #95391, #57550, #82656, #34640 ) ) ;
#88265 = CARTESIAN_POINT ( 'NONE',  ( 0.2353198783969999985, 1506.810797463830113, 231.1250055480980166 ) ) ;
#88266 = CARTESIAN_POINT ( 'NONE',  ( 10.58000746958911797, 1434.869963651638045, 152.0831908380279458 ) ) ;
#88267 = CARTESIAN_POINT ( 'NONE',  ( 8.640078715520209229, 1511.774605969369986, 202.9607466897689960 ) ) ;
#88268 = UNCERTAINTY_MEASURE_WITH_UNIT (LENGTH_MEASURE( 1.000000000000000082E-05 ), #2428, 'distance_accuracy_value', 'NONE');
#88269 = CARTESIAN_POINT ( 'NONE',  ( 3.365684841717370368, 1424.260763520689807, 191.4759580909079943 ) ) ;
#88270 = CARTESIAN_POINT ( 'NONE',  ( 16.92416502119278121, 1422.029238661900536, 226.8824423085827391 ) ) ;
#88271 = CARTESIAN_POINT ( 'NONE',  ( 22.37934203670000244, 1410.866856972729920, 205.0809305166880279 ) ) ;
#88272 = CARTESIAN_POINT ( 'NONE',  ( 17.33645360970000127, 1414.996444518330009, 210.3925742363780103 ) ) ;
#88273 = CARTESIAN_POINT ( 'NONE',  ( 34.18677586421181758, 1522.382868172863937, 198.4504086008745389 ) ) ;
#88274 = CARTESIAN_POINT ( 'NONE',  ( 17.30126322264720429, 1523.462669333491704, 180.8506073315129470 ) ) ;
#88275 = LINE ( 'NONE', #53592, #5647 ) ;
#88276 = CARTESIAN_POINT ( 'NONE',  ( 16.60587746830000100, 1428.779800883930193, 190.9634344794979768 ) ) ;
#88277 = CARTESIAN_POINT ( 'NONE',  ( -19.07391236770194354, 1440.581610101740807, 209.7732386265107039 ) ) ;
#88278 = CARTESIAN_POINT ( 'NONE',  ( -0.2282227750583530057, 1457.883215173980034, 229.2261862118490114 ) ) ;
#88279 = ORIENTED_EDGE ( 'NONE', *, *, #55126, .T. ) ;
#88280 = CARTESIAN_POINT ( 'NONE',  ( 1.045121606856920016, 1507.562507626550087, 186.2156307130109951 ) ) ;
#88281 = DIRECTION ( 'NONE',  ( 0.000000000000000000, 0.000000000000000000, 1.000000000000000000 ) ) ;
#88282 = CARTESIAN_POINT ( 'NONE',  ( -11.90000809277082183, 1434.914618699171342, 147.6452175350320317 ) ) ;
#88283 = DIRECTION ( 'NONE',  ( -1.755985294532469921E-16, 1.000000000000000000, -1.338183447452831989E-16 ) ) ;
#88284 = DIRECTION ( 'NONE',  ( 0.000000000000000000, 1.000000000000000000, 0.000000000000000000 ) ) ;
#88285 = CARTESIAN_POINT ( 'NONE',  ( -2.771042439397337631, 1425.976720272856255, 185.1763243323314043 ) ) ;
#88286 = CARTESIAN_POINT ( 'NONE',  ( 12.54268436849999979, 1408.913060387329779, 221.6645303301980050 ) ) ;
#88287 = CARTESIAN_POINT ( 'NONE',  ( 26.80766621430014496, 1435.433710258606880, 135.7240550330992903 ) ) ;
#88288 = CARTESIAN_POINT ( 'NONE',  ( -8.652776130911478347, 1511.435001053830092, 214.5073691320910143 ) ) ;
#88289 = CARTESIAN_POINT ( 'NONE',  ( -10.50807510266660039, 1489.705281234110089, 213.5102346389539889 ) ) ;
#88290 = CARTESIAN_POINT ( 'NONE',  ( -21.46486249247640288, 1504.440131453050071, 215.6677484931969957 ) ) ;
#88291 = CARTESIAN_POINT ( 'NONE',  ( -94.92604110475619450, 1383.767219722170239, 309.8421315003910195 ) ) ;
#88292 = EDGE_CURVE ( 'NONE', #76159, #68958, #103781, .T. ) ;
#88293 = CARTESIAN_POINT ( 'NONE',  ( -109.3255347603840022, 1384.025522620290076, 311.1851463503860487 ) ) ;
#88294 = CARTESIAN_POINT ( 'NONE',  ( -15.49546525088307192, 1506.491018773352152, 224.7822750072435838 ) ) ;
#88295 = CARTESIAN_POINT ( 'NONE',  ( -0.5361381215162029923, 1516.779489719179992, 201.4063938103320197 ) ) ;
#88297 = ORIENTED_EDGE ( 'NONE', *, *, #18796, .F. ) ;
#88296 = CARTESIAN_POINT ( 'NONE',  ( 20.76477904309999900, 1508.884216872730121, 189.8073430845979885 ) ) ;
#88298 = CARTESIAN_POINT ( 'NONE',  ( -93.71265355510000461, 1380.723683565119927, 297.1406752587590177 ) ) ;
#88299 = EDGE_CURVE ( 'NONE', #1788, #77903, #102345, .T. ) ;
#88300 = CARTESIAN_POINT ( 'NONE',  ( 9.196349486490200675, 1517.051704408389924, 214.4668224883511698 ) ) ;
#88301 = ORIENTED_EDGE ( 'NONE', *, *, #36336, .T. ) ;
#88302 = EDGE_LOOP ( 'NONE', ( #105528, #9056, #40320, #101537 ) ) ;
#88303 = EDGE_CURVE ( 'NONE', #48781, #34958, #21487, .T. ) ;
#88304 = CARTESIAN_POINT ( 'NONE',  ( 27.17824031941000129, 1496.227206563929940, 207.6753971228399962 ) ) ;
#88305 = CARTESIAN_POINT ( 'NONE',  ( 13.12077080189999911, 1508.676888898530024, 233.4678022570980147 ) ) ;
#88306 = CARTESIAN_POINT ( 'NONE',  ( 13.48138647031106352, 1443.612224725923852, 169.3589832081940756 ) ) ;
#88308 = CARTESIAN_POINT ( 'NONE',  ( -24.26836172750000031, 1463.758689926529996, 255.0044385419980131 ) ) ;
#88307 = CARTESIAN_POINT ( 'NONE',  ( 35.02402602625965500, 1424.077443822751775, 269.5318445452296032 ) ) ;
#88309 = DIRECTION ( 'NONE',  ( -0.8090169943749422332, 0.000000000000000000, 0.5877852522924802425 ) ) ;
#88310 = CARTESIAN_POINT ( 'NONE',  ( -109.1655177890000061, 1384.872414444939977, 297.1329087538589420 ) ) ;
#88311 = DIRECTION ( 'NONE',  ( 0.000000000000000000, 1.000000000000000000, 0.000000000000000000 ) ) ;
#88312 = CARTESIAN_POINT ( 'NONE',  ( 11.68583270360880100, 1426.729740719480105, 140.5078102237010000 ) ) ;
#88313 = CARTESIAN_POINT ( 'NONE',  ( 6.165765019510000222, 1409.128373646630052, 187.8915199111979746 ) ) ;
#88314 = FACE_OUTER_BOUND ( 'NONE', #101082, .T. ) ;
#88315 = CARTESIAN_POINT ( 'NONE',  ( -12.03552277399999859, 1436.199553089340043, 151.3007237992979981 ) ) ;
#88316 = DIRECTION ( 'NONE',  ( 4.973799150213359420E-14, 0.8730714504308808577, -0.4875922912049759361 ) ) ;
#88317 = CARTESIAN_POINT ( 'NONE',  ( -9.315871017458929870, 1479.165496450050114, 216.1736367611900107 ) ) ;
#88318 = CARTESIAN_POINT ( 'NONE',  ( 3.304926999371979868, 1524.538969332612623, 241.8712028721135994 ) ) ;
#88320 = ORIENTED_EDGE ( 'NONE', *, *, #105531, .F. ) ;
#88319 = CARTESIAN_POINT ( 'NONE',  ( -12.51045652733512981, 1414.677402202029953, 206.7437175916260230 ) ) ;
#88321 = VERTEX_POINT ( 'NONE', #37761 ) ;
#88322 = CARTESIAN_POINT ( 'NONE',  ( -11.61654445250000123, 1506.309187293489913, 207.9630299090890162 ) ) ;
#88323 = CARTESIAN_POINT ( 'NONE',  ( 9.941274985550709431, 1491.817956606359985, 188.4486685046520051 ) ) ;
#88325 = ADVANCED_FACE ( 'NONE', ( #29345 ), #19273, .T. ) ;
#88324 = CARTESIAN_POINT ( 'NONE',  ( -10.53025827939999992, 1470.866850696130086, 269.8740970541979323 ) ) ;
#88326 = CARTESIAN_POINT ( 'NONE',  ( 8.209570662930000040, 1421.454114719120298, 196.1494337501989946 ) ) ;
#88327 =( BOUNDED_CURVE ( )  B_SPLINE_CURVE ( 3, ( #81420, #45672, #20415, #3116 ),
 .UNSPECIFIED., .F., .T. ) 
 B_SPLINE_CURVE_WITH_KNOTS ( ( 4, 4 ),
 ( 1.530699404089715943, 1.539816210893797388 ),
 .UNSPECIFIED. ) 
 CURVE ( )  GEOMETRIC_REPRESENTATION_ITEM ( )  RATIONAL_B_SPLINE_CURVE ( ( 1.000000000000000000, 0.9999930736648015017, 0.9999930736648015017, 1.000000000000000000 ) ) 
 REPRESENTATION_ITEM ( '' )  );
#88328 = CARTESIAN_POINT ( 'NONE',  ( 16.69108863619999994, 1409.495926044930002, 223.4055895545979809 ) ) ;
#88329 = CARTESIAN_POINT ( 'NONE',  ( -15.28316321820000034, 1506.811133768429954, 224.9455926307979894 ) ) ;
#88330 = DIRECTION ( 'NONE',  ( -0.01484500364209119690, 0.5669078173028199163, 0.8236474686100957454 ) ) ;
#88331 = CARTESIAN_POINT ( 'NONE',  ( 18.22873622136830107, 1457.634151734390116, 229.9687917111629929 ) ) ;
#88332 = EDGE_CURVE ( 'NONE', #91721, #105303, #84101, .T. ) ;
#88333 = CARTESIAN_POINT ( 'NONE',  ( -17.66967187194796551, 1517.051704408389924, 195.1406325242839159 ) ) ;
#88334 = CARTESIAN_POINT ( 'NONE',  ( 9.258247136794901522, 1363.198586359130104, 210.6218459616991936 ) ) ;
#88335 = CARTESIAN_POINT ( 'NONE',  ( -45.32983761869079586, 1435.629079562749894, 268.7723279587979732 ) ) ;
#88336 = ORIENTED_EDGE ( 'NONE', *, *, #101405, .F. ) ;
#88337 = CARTESIAN_POINT ( 'NONE',  ( -8.090248624290001800, 1425.035463411989895, 209.7688195370299979 ) ) ;
#88338 = AXIS2_PLACEMENT_3D ( 'NONE', #71972, #79796, #88189 ) ;
#88339 = VERTEX_POINT ( 'NONE', #28250 ) ;
#88340 = CARTESIAN_POINT ( 'NONE',  ( -4.031168805994999715, 1516.805675336850072, 209.8787446699039947 ) ) ;
#88341 = DIRECTION ( 'NONE',  ( 0.7074300732568278294, 0.02470400251969403355, 0.7063514732138287400 ) ) ;
#88342 = CARTESIAN_POINT ( 'NONE',  ( -20.59685312390000078, 1507.762914164829908, 190.3821647269979849 ) ) ;
#88343 = LINE ( 'NONE', #104029, #48363 ) ;
#88344 = AXIS2_PLACEMENT_3D ( 'NONE', #63736, #82715, #40156 ) ;
#88345 = CARTESIAN_POINT ( 'NONE',  ( -3.141362685563839907, 1497.118792551569868, 221.1081249425609769 ) ) ;
#88346 = B_SPLINE_SURFACE_WITH_KNOTS ( 'NONE', 5, 5, ( 
 ( #31850, #48117, #81685, #40252, #73872, #22318, #90091, #15028, #32946 ),
 ( #92303, #83906, #40804, #55968, #67136, #82256, #109131, #57082, #74434 ),
 ( #107450, #4991, #30746, #5557, #7212, #65481, #21767, #108560, #13375 ),
 ( #56520, #90647, #39706, #108000, #31297, #99590, #22873, #91206, #14488 ),
 ( #50340, #35162, #84465, #76073, #93408, #9416, #44135, #78269, #8296 ),
 ( #18344, #68252, #60385, #7752, #110214, #68798, #94506, #26197, #60951 ),
 ( #101234, #34612, #17780, #16673, #86668, #33487, #92857, #110769, #1583 ),
 ( #41917, #85001, #67689, #17222, #50871, #103456, #101797, #25087, #43578 ),
 ( #59291, #77727, #42458, #16133, #69346, #25643, #76617, #34059, #102359 ),
 ( #59834, #93957, #35718, #9964, #51418, #24534, #1040, #58722, #95078 ),
 ( #85549, #8845, #43028, #26762, #77186, #489, #102899, #52535, #51981 ),
 ( #86122, #36826, #29520, #19456, #63711, #12168, #27316, #106234, #80492 ),
 ( #28427, #53655, #69907, #97821, #97277, #105703, #21099, #12726, #71016 ),
 ( #3254, #78840, #63173, #2151, #55301, #89434, #20550, #88335, #54754 ),
 ( #79938, #37381, #70459, #27875, #46907, #11627, #18896, #10519, #105137 ),
 ( #87800, #62626, #96744, #53091, #88884, #54210, #81030, #95627, #11084 ),
 ( #71581, #4339, #3808, #72119, #61497, #104021, #44693, #37939, #46358 ),
 ( #87230, #28985, #36269, #104580, #45251, #20015, #79387, #45805, #2701 ),
 ( #62056, #96181, #66465, #74851, #83234, #5977, #49099, #58048, #4867 ),
 ( #47986, #82123, #40677, #73755, #39583, #56392, #82687, #39010, #108995 ),
 ( #40122, #5425, #100022, #22742, #21649, #56946, #92184, #23856, #72647 ),
 ( #98377, #55857, #98924, #32281, #107878, #74307, #91075, #14358, #31718 ),
 ( #15455, #49647, #108437, #83783, #31166, #13800, #64254, #48550, #47440 ),
 ( #100574, #65904, #23314, #57507, #90524, #91632, #14908, #73187, #107332 ),
 ( #6525, #89976, #13250, #65356, #38470, #99464, #106772, #30063, #81564 ),
 ( #64816, #30628, #22194, #60821, #903, #68660, #58596, #33921, #50732 ),
 ( #41779, #8163, #77597, #69208, #42894, #102760, #42332, #75934, #67005 ),
 ( #8715, #17090, #93811, #94368, #59158, #110636, #33364, #51851, #26056 ),
 ( #59698, #85988, #51282, #85416, #77052, #67557, #32818, #25508, #93278 ),
 ( #75406, #358, #94946, #41234, #9286, #35029, #34485, #109545, #26625 ),
 ( #60251, #76484, #17650, #16541, #24411, #101115, #92727, #101660, #103317 ),
 ( #43448, #102229, #18215, #24947, #52411, #7078, #16003, #110089, #84865 ),
 ( #50206, #84331, #68116, #7621, #63046, #45120, #63582, #62487, #88759 ),
 ( #36149, #28851, #97152, #53516, #46224, #70333, #80358, #20421, #43999 ),
 ( #54626, #3674, #79262, #104445, #86536, #37802, #3122, #11502, #71990 ),
 ( #87659, #87093, #19876, #95494, #79816, #97699, #12042, #106104, #78134 ),
 ( #27192, #29381, #105565, #105002, #69775, #54083, #45678, #20971, #61927 ),
 ( #96044, #2572, #19315, #18762, #9830, #36694, #1437, #35583, #103893 ),
 ( #61375, #52959, #10378, #70888, #10948, #28291, #44551, #96607, #88208 ) ),
 .UNSPECIFIED., .F., .F., .F.,
 ( 6, 3, 3, 3, 3, 3, 3, 3, 3, 3, 3, 3, 6 ),
 ( 6, 3, 6 ),
 ( 24.04728406787560147, 26.41731193910000286, 28.47858422270000034, 30.53985650629999782, 34.66240107340000520, 42.94082674090000040, 51.21925240840000271, 84.61883450350001112, 101.2490010300000023, 117.8791675569999882, 130.6181505580000248, 136.9876420589999952, 143.3571909864640190 ),
 ( -7.608642969747240396E-05, 1.000000000000000000, 2.000086805724440087 ),
 .UNSPECIFIED. ) ;
#88347 = ORIENTED_EDGE ( 'NONE', *, *, #63153, .T. ) ;
#88348 = CARTESIAN_POINT ( 'NONE',  ( 173.8335085727406693, 1524.382868172863937, 317.3879012941853830 ) ) ;
#88349 = CARTESIAN_POINT ( 'NONE',  ( 4.034908559714999399, 1517.068717944079935, 201.7859449365070077 ) ) ;
#88350 = EDGE_CURVE ( 'NONE', #88970, #98935, #62442, .T. ) ;
#88351 = CARTESIAN_POINT ( 'NONE',  ( 10.38136293080000172, 1472.225397094090113, 214.0145097960790110 ) ) ;
#88352 = B_SPLINE_CURVE_WITH_KNOTS ( 'NONE', 5,
 ( #103098, #42118, #110414, #25283, #85759, #68997 ),
 .UNSPECIFIED., .F., .F.,
 ( 6, 6 ),
 ( 0.000000000000000000, 1.000000000000000000 ),
 .UNSPECIFIED. ) ;
#88353 = CARTESIAN_POINT ( 'NONE',  ( -8.371011905599029745, 1438.923880247289844, 206.6694023295629847 ) ) ;
#88354 = ORIENTED_EDGE ( 'NONE', *, *, #28772, .T. ) ;
#88355 = CARTESIAN_POINT ( 'NONE',  ( -8.402618400705980761, 1410.369408431269903, 270.0745577945219793 ) ) ;
#88356 = CARTESIAN_POINT ( 'NONE',  ( -4.625790014595000166, 1517.104192383289956, 208.0004623403669939 ) ) ;
#88357 = CARTESIAN_POINT ( 'NONE',  ( 3.515433849202130201, 1416.356576007590093, 231.8113076371539876 ) ) ;
#88358 = CARTESIAN_POINT ( 'NONE',  ( 0.000000000000000000, 1518.913060387330006, 209.1218459616979999 ) ) ;
#88360 = EDGE_LOOP ( 'NONE', ( #107420, #80784, #50467, #95007, #72002 ) ) ;
#88359 = CARTESIAN_POINT ( 'NONE',  ( -7.227598892266946962, 1366.688675025208795, 210.6218459617142003 ) ) ;
#88361 = ORIENTED_EDGE ( 'NONE', *, *, #39109, .T. ) ;
#88362 = CARTESIAN_POINT ( 'NONE',  ( 45.58870143954486309, 1442.488502812692332, 268.9760731915026213 ) ) ;
#88363 = CARTESIAN_POINT ( 'NONE',  ( 11.26621375010180159, 1471.492305945939961, 211.0164925480820273 ) ) ;
#88364 = CARTESIAN_POINT ( 'NONE',  ( 3.625818218658252157, 1424.595510787312151, 184.5955723309376992 ) ) ;
#88365 = CARTESIAN_POINT ( 'NONE',  ( -24.04208912931621711, 1411.123052270208063, 266.7327788561432271 ) ) ;
#88366 = VECTOR ( 'NONE', #4876, 1000.000000000000000 ) ;
#88367 = CARTESIAN_POINT ( 'NONE',  ( -18.69712754293130175, 1416.051481372519902, 207.5721598449429735 ) ) ;
#88368 = CARTESIAN_POINT ( 'NONE',  ( 2.500000047107329593, 1439.241554657300185, 157.7315143162209949 ) ) ;
#88369 = CARTESIAN_POINT ( 'NONE',  ( -0.0001195472470990460034, 1475.319258240860108, 269.4988494337139855 ) ) ;
#88370 = CARTESIAN_POINT ( 'NONE',  ( 12.71459596929999947, 1416.274718422629803, 222.8886675024980093 ) ) ;
#88371 = CARTESIAN_POINT ( 'NONE',  ( 7.138945119869999800, 1447.187254549259933, 185.3421223705979912 ) ) ;
#88372 = CARTESIAN_POINT ( 'NONE',  ( 5.771149074885000729, 1516.616791731099966, 206.6334853027970269 ) ) ;
#88373 = ORIENTED_EDGE ( 'NONE', *, *, #35846, .F. ) ;
#88374 = CARTESIAN_POINT ( 'NONE',  ( 21.31045967363568749, 1411.017795812226268, 217.5615436375129264 ) ) ;
#88375 = CARTESIAN_POINT ( 'NONE',  ( 1.480860223639280049, 1477.429525514950001, 182.4079029408990209 ) ) ;
#88376 = VERTEX_POINT ( 'NONE', #81947 ) ;
#88377 = CARTESIAN_POINT ( 'NONE',  ( 18.22873622136830107, 1457.634151734390116, 229.9687917111629929 ) ) ;
#88378 = CARTESIAN_POINT ( 'NONE',  ( 24.39998090177769896, 1451.998272387500037, 136.9252543644830098 ) ) ;
#88379 = FACE_OUTER_BOUND ( 'NONE', #49362, .T. ) ;
#88380 = CARTESIAN_POINT ( 'NONE',  ( -23.00221949109999997, 1384.956020836430071, 202.3857052141389943 ) ) ;
#88381 = CARTESIAN_POINT ( 'NONE',  ( -10.42770192888281144, 1387.487768598823777, 217.7251358788310256 ) ) ;
#88382 = CARTESIAN_POINT ( 'NONE',  ( 18.53966907490000082, 1409.560479898229914, 196.5394618705980179 ) ) ;
#88383 = CARTESIAN_POINT ( 'NONE',  ( 27.73483395940000307, 1444.994950788470987, 161.2078980334979690 ) ) ;
#88384 = CARTESIAN_POINT ( 'NONE',  ( 17.58997750089999812, 1410.451595763729983, 225.2085130754979900 ) ) ;
#88385 = CARTESIAN_POINT ( 'NONE',  ( -19.76302329002471936, 1426.035389032143939, 222.9111529220132866 ) ) ;
#88386 = CARTESIAN_POINT ( 'NONE',  ( 21.64192060530918482, 1453.490330227820550, 220.9236656602734001 ) ) ;
#88387 = ADVANCED_FACE ( 'NONE', ( #30998 ), #80124, .F. ) ;
#88388 = CARTESIAN_POINT ( 'NONE',  ( -10.37222135890000096, 1380.909514438620135, 216.5949044049989993 ) ) ;
#88389 = ADVANCED_FACE ( 'NONE', ( #107714 ), #49475, .T. ) ;
#88390 = CARTESIAN_POINT ( 'NONE',  ( 7.719392382375000139, 1516.929962200689943, 215.6766245038770080 ) ) ;
#88391 = CARTESIAN_POINT ( 'NONE',  ( 2.478666945488134932, 1524.659148609483054, 242.4727585245961450 ) ) ;
#88392 = ORIENTED_EDGE ( 'NONE', *, *, #103127, .T. ) ;
#88393 = CARTESIAN_POINT ( 'NONE',  ( -16.98382822079999954, 1417.304183444519822, 207.5927344675390032 ) ) ;
#88394 = CARTESIAN_POINT ( 'NONE',  ( -6.103113815119999508, 1482.731685980090106, 200.3426744219489990 ) ) ;
#88395 = CARTESIAN_POINT ( 'NONE',  ( -9.917060407088358787, 1483.572227753479865, 202.5254192721800166 ) ) ;
#88396 = CARTESIAN_POINT ( 'NONE',  ( 3.873571330434599780, 1517.051704409849890, 202.3168006365660005 ) ) ;
#88397 = CARTESIAN_POINT ( 'NONE',  ( -39.96604417509509943, 1445.822677059940133, 136.8290734187280009 ) ) ;
#88398 = CARTESIAN_POINT ( 'NONE',  ( -4.326992699989999913, 1515.158586642790169, 209.1218459619010162 ) ) ;
#88399 = CARTESIAN_POINT ( 'NONE',  ( 1.576516694969999887E-14, 1462.614442895030152, 248.0989693021979861 ) ) ;
#88400 = LINE ( 'NONE', #104646, #89629 ) ;
#88401 = CARTESIAN_POINT ( 'NONE',  ( -12.31697047491260122, 1378.344771059540108, 209.6432931632009797 ) ) ;
#88402 = CARTESIAN_POINT ( 'NONE',  ( -42.19478785709999613, 1454.283011521129993, 269.0694631118980169 ) ) ;
#88403 = CARTESIAN_POINT ( 'NONE',  ( -10.87726901145729919, 1461.906291937230208, 210.8265890786230159 ) ) ;
#88404 = CARTESIAN_POINT ( 'NONE',  ( -22.67178350569999878, 1508.009769414930133, 225.0292584458980230 ) ) ;
#88405 = CARTESIAN_POINT ( 'NONE',  ( 13.16561200850000013, 1429.090194843729932, 222.5186421963979910 ) ) ;
#88406 = ORIENTED_EDGE ( 'NONE', *, *, #48788, .F. ) ;
#88407 = DIRECTION ( 'NONE',  ( 0.000000000000000000, 1.000000000000000000, -6.123233995736769734E-17 ) ) ;
#88408 = CARTESIAN_POINT ( 'NONE',  ( -2.857351367441036238, 1525.661276915132476, 177.1476448543304514 ) ) ;
#88409 = CARTESIAN_POINT ( 'NONE',  ( 0.000000000000000000, 1526.382868172863937, 242.2588656733921653 ) ) ;
#88410 = CARTESIAN_POINT ( 'NONE',  ( -2.038646110889581031, 1525.960063244516959, 241.1857569150894562 ) ) ;
#88411 = CARTESIAN_POINT ( 'NONE',  ( 11.85959186116559927, 1501.678157499889949, 211.5145819234840019 ) ) ;
#88412 = ADVANCED_FACE ( 'NONE', ( #65176 ), #14, .F. ) ;
#88413 = CARTESIAN_POINT ( 'NONE',  ( 25.36027075109999984, 1449.801358167649823, 211.2972422996380146 ) ) ;
#88414 = VECTOR ( 'NONE', #105563, 1000.000000000000114 ) ;
#88415 = B_SPLINE_CURVE_WITH_KNOTS ( 'NONE', 3,
 ( #30913, #107076, #39873, #30362, #74041, #80785, #21934, #31462, #38217, #72399, #13000, #108171, #65642, #99204, #89725, #106530, #98116, #23048, #56127, #90262, #91382, #13545, #73493, #3553, #107629, #22483, #65092, #14101, #32017, #16833, #48849 ),
 .UNSPECIFIED., .F., .F.,
 ( 4, 2, 2, 1, 1, 1, 1, 2, 2, 2, 1, 1, 1, 1, 1, 2, 2, 2, 2, 4 ),
 ( 0.000000000000000000, 0.2500000000000182632, 0.3750000000000275335, 0.4375000000000320854, 0.4687500000000326406, 0.4843750000000336398, 0.4921875000000361933, 0.4960937500000365818, 0.5000000000000369704, 0.6250000000000401901, 0.6875000000000419664, 0.7187500000000440759, 0.7343750000000441869, 0.7421875000000438538, 0.7460937500000442979, 0.7480468750000439648, 0.7500000000000436318, 0.8125000000000325295, 0.8750000000000213163, 1.000000000000000000 ),
 .UNSPECIFIED. ) ;
#88416 = CARTESIAN_POINT ( 'NONE',  ( -16.85976061912537816, 1525.821544997590536, 236.1944305375348847 ) ) ;
#88417 = CARTESIAN_POINT ( 'NONE',  ( 7.671698190030000752, 1427.928538830389925, 213.1259091499790088 ) ) ;
#88418 = CARTESIAN_POINT ( 'NONE',  ( -30.94934575091909679, 1383.840876600240108, 228.8241727730240029 ) ) ;
#88419 = EDGE_CURVE ( 'NONE', #89436, #43690, #24777, .T. ) ;
#88420 = DIRECTION ( 'NONE',  ( 9.341989762165448955E-47, -1.000000000000000000, 1.836970198721029688E-16 ) ) ;
#88421 = CARTESIAN_POINT ( 'NONE',  ( 6.126746143464999683, 1514.923664147150021, 200.9956116846470309 ) ) ;
#88422 = CARTESIAN_POINT ( 'NONE',  ( -3.482404828285579956, 1485.996524617339901, 182.2044860649310181 ) ) ;
#88423 = CARTESIAN_POINT ( 'NONE',  ( 2.994687979099999620, 1464.609795697029995, 236.6065847252980063 ) ) ;
#88424 = EDGE_CURVE ( 'NONE', #30117, #8025, #16922, .T. ) ;
#88426 = EDGE_LOOP ( 'NONE', ( #44435, #71569 ) ) ;
#88425 = CARTESIAN_POINT ( 'NONE',  ( 5.151097723079999469, 1490.744826430290004, 188.9005472705989916 ) ) ;
#88427 = CARTESIAN_POINT ( 'NONE',  ( -1.535065677160000197, 1450.609239756710167, 182.1703775756980122 ) ) ;
#88428 = CARTESIAN_POINT ( 'NONE',  ( -9.420327913192419800, 1388.839158060524824, 201.0591600557601453 ) ) ;
#88429 = CARTESIAN_POINT ( 'NONE',  ( 11.90084012403499969, 1512.572572334140204, 202.1707532763570043 ) ) ;
#88431 = ORIENTED_EDGE ( 'NONE', *, *, #46991, .T. ) ;
#88430 = CARTESIAN_POINT ( 'NONE',  ( -17.13018491839999768, 1414.971993471370070, 208.1178512858780039 ) ) ;
#88432 = CARTESIAN_POINT ( 'NONE',  ( -2.861085386292339994, 1508.551704408389924, 220.0095495000269921 ) ) ;
#88433 = EDGE_LOOP ( 'NONE', ( #59844, #18920, #54117, #62130, #4826, #23355, #66226, #26659, #7969, #38480, #97171, #26158, #49103, #14635, #10882, #5948 ) ) ;
#88434 = PRODUCT_DEFINITION_SHAPE ( 'NONE', 'NONE',  #31601 ) ;
#88435 = CARTESIAN_POINT ( 'NONE',  ( -10.42777903026719954, 1387.487736158059988, 217.7251714971619947 ) ) ;
#88436 = LINE ( 'NONE', #2802, #51555 ) ;
#88437 = CARTESIAN_POINT ( 'NONE',  ( -2.760778634279479782, 1409.009468901610035, 188.0459411385839985 ) ) ;
#88439 = EDGE_CURVE ( 'NONE', #93856, #19743, #23264, .T. ) ;
#88438 = CARTESIAN_POINT ( 'NONE',  ( 3.879020388191510182, 1465.465499240460076, 203.2370418086409813 ) ) ;
#88440 = DIRECTION ( 'NONE',  ( 5.980589973904019347E-17, -1.000000000000000000, 1.736889445713099699E-16 ) ) ;
#88441 = CARTESIAN_POINT ( 'NONE',  ( -10.10631778097200062, 1472.663248310899917, 207.2585624568480114 ) ) ;
#88442 = CARTESIAN_POINT ( 'NONE',  ( 14.91350687018140064, 1409.433851523019939, 209.9051533666169860 ) ) ;
#88443 = CIRCLE ( 'NONE', #86839, 1.000000000000000888 ) ;
#88444 = LINE ( 'NONE', #36377, #47259 ) ;
#88445 = CARTESIAN_POINT ( 'NONE',  ( -103.8521778202700006, 1385.230324909849969, 296.8200838699809765 ) ) ;
#88446 = CARTESIAN_POINT ( 'NONE',  ( -17.63801041889999865, 1411.923586951229936, 192.9996560761979936 ) ) ;
#88447 = CARTESIAN_POINT ( 'NONE',  ( 10.28019753094960009, 1422.778998439059933, 209.5284952118790045 ) ) ;
#88448 = EDGE_CURVE ( 'NONE', #43187, #81049, #75230, .T. ) ;
#88449 = CARTESIAN_POINT ( 'NONE',  ( 10.93675118801170143, 1490.434561969760125, 209.9324825431089891 ) ) ;
#88450 = ORIENTED_EDGE ( 'NONE', *, *, #89984, .T. ) ;
#88451 = ORIENTED_EDGE ( 'NONE', *, *, #93991, .T. ) ;
#88452 = EDGE_CURVE ( 'NONE', #80101, #36031, #46271, .T. ) ;
#88454 = AXIS2_PLACEMENT_3D ( 'NONE', #54127, #88254, #3170 ) ;
#88453 = CARTESIAN_POINT ( 'NONE',  ( -11.94908641619550060, 1415.673583083980020, 194.9773138209209833 ) ) ;
#88455 = CARTESIAN_POINT ( 'NONE',  ( -0.5371945001445930234, 1496.425099764140214, 196.7755987515499783 ) ) ;
#88456 = CARTESIAN_POINT ( 'NONE',  ( 34.37943628549087549, 1458.453385912395106, 269.5229009448329407 ) ) ;
#88457 = CARTESIAN_POINT ( 'NONE',  ( -33.43367350703635310, 1524.397344074318198, 220.4773507679704494 ) ) ;
#88458 = CARTESIAN_POINT ( 'NONE',  ( 3.502832715609999870, 1396.096283016630196, 220.3210214699980156 ) ) ;
#88459 = CARTESIAN_POINT ( 'NONE',  ( 31.75407494088092264, 1525.055427061254250, 201.5867930770752423 ) ) ;
#88460 = EDGE_CURVE ( 'NONE', #41682, #98399, #94203, .T. ) ;
#88461 = CARTESIAN_POINT ( 'NONE',  ( -0.1433134854889999976, 1453.573377095430260, 183.1846218448980039 ) ) ;
#88462 = CARTESIAN_POINT ( 'NONE',  ( -11.42967626019537519, 1367.015145146939176, 209.6218459617033432 ) ) ;
#88463 = CARTESIAN_POINT ( 'NONE',  ( 3.628818059389999906, 1505.602008401590183, 221.3635115024989943 ) ) ;
#88464 = B_SPLINE_CURVE_WITH_KNOTS ( 'NONE', 3,
 ( #77330, #86820, #59439, #1183, #104174, #34210, #76769, #16821, #44284, #17377, #10112, #51576, #110364, #77875, #78428, #35878, #70062, #86264, #33642, #69500, #51022, #631, #68949, #104722, #62769, #46497, #105277, #20694, #87944, #47041, #54890, #36961, #28571, #54350, #71724, #70604, #105841 ),
 .UNSPECIFIED., .F., .F.,
 ( 4, 3, 3, 3, 3, 3, 3, 3, 3, 3, 3, 3, 4 ),
 ( 0.000000000000000000, 2.822161410921079749, 4.695069562297280008, 5.748948128523428736, 7.569543626606720643, 8.522194890855359972, 9.390139124690000116, 9.765848498500000474, 10.24736818868129973, 10.79639064002810045, 11.59603149051410043, 12.12355864179750142, 12.39567234100000093 ),
 .UNSPECIFIED. ) ;
#88465 = EDGE_CURVE ( 'NONE', #70633, #52400, #106319, .T. ) ;
#88466 = CARTESIAN_POINT ( 'NONE',  ( 4.608146781254999880, 1516.677239312369920, 206.8257210811669893 ) ) ;
#88467 = DIRECTION ( 'NONE',  ( 0.000000000000000000, 0.000000000000000000, 1.000000000000000000 ) ) ;
#88468 = B_SPLINE_SURFACE_WITH_KNOTS ( 'NONE', 5, 5, ( 
 ( #26425, #8517, #100915, #25861, #9085, #51649 ),
 ( #93079, #32637, #160, #77400, #17450, #94180 ),
 ( #66814, #16895, #60620, #67365, #34283, #7974 ),
 ( #85788, #34833, #60062, #69021, #24751, #94740 ),
 ( #58948, #42141, #76292, #110443, #33722, #67914 ),
 ( #102021, #25306, #59506, #93617, #87463, #98995 ) ),
 .UNSPECIFIED., .F., .F., .F.,
 ( 6, 6 ),
 ( 6, 6 ),
 ( 1.117146821299999981, 1.987971636789739982 ),
 ( 0.000000000000000000, 2.000000000000000000 ),
 .UNSPECIFIED. ) ;
#88469 = CARTESIAN_POINT ( 'NONE',  ( 17.64995062490000066, 1409.529410244630071, 195.7212478390979982 ) ) ;
#88470 = DIRECTION ( 'NONE',  ( -4.222254822704919979E-17, -1.000000000000000000, 7.728785610902649958E-17 ) ) ;
#88471 = CARTESIAN_POINT ( 'NONE',  ( -17.61758723057469922, 1488.711492928860025, 197.7573658785580051 ) ) ;
#88472 = EDGE_CURVE ( 'NONE', #69919, #5765, #32233, .T. ) ;
#88473 = DIRECTION ( 'NONE',  ( 0.9930361521007663450, 0.03467758656449191484, -0.1125906994869730476 ) ) ;
#88474 = VERTEX_POINT ( 'NONE', #34306 ) ;
#88475 = DIRECTION ( 'NONE',  ( 0.000000000000000000, 0.000000000000000000, 1.000000000000000000 ) ) ;
#88476 = CARTESIAN_POINT ( 'NONE',  ( -25.53333737259999836, 1449.803091291330020, 207.7075060623679974 ) ) ;
#88478 = DIRECTION ( 'NONE',  ( 0.000000000000000000, 1.000000000000000000, 0.000000000000000000 ) ) ;
#88477 = CARTESIAN_POINT ( 'NONE',  ( -3.549608295209999653, 1507.276800932030028, 180.9704960860979952 ) ) ;
#88479 = CARTESIAN_POINT ( 'NONE',  ( -5.513435596820279727, 1509.038615934079871, 216.6345961782780023 ) ) ;
#88480 = CARTESIAN_POINT ( 'NONE',  ( -31.18244400340000055, 1434.782053685539950, 244.2061907853979790 ) ) ;
#88481 = CARTESIAN_POINT ( 'NONE',  ( 2.480332738680000038, 1486.002627324889772, 219.7500672349989941 ) ) ;
#88482 = CARTESIAN_POINT ( 'NONE',  ( -5.100031674329999376, 1391.870658628590036, 214.4808810019090117 ) ) ;
#88483 = DIRECTION ( 'NONE',  ( -0.7067700949440681724, -0.03085664260706927689, -0.7067700478230329875 ) ) ;
#88484 = VERTEX_POINT ( 'NONE', #76318 ) ;
#88485 = CARTESIAN_POINT ( 'NONE',  ( -5.381406753977029389, 1431.114362971160062, 154.5700877874419916 ) ) ;
#88486 = CARTESIAN_POINT ( 'NONE',  ( 14.28812837704985661, 1514.188985847965341, 225.6571130645534424 ) ) ;
#88487 = CARTESIAN_POINT ( 'NONE',  ( -4.329448776275169664, 1515.064792882719985, 206.7917118343879963 ) ) ;
#88488 = ORIENTED_EDGE ( 'NONE', *, *, #71588, .F. ) ;
#88489 = ORIENTED_EDGE ( 'NONE', *, *, #103127, .F. ) ;
#88490 = VECTOR ( 'NONE', #42366, 999.9999999999998863 ) ;
#88491 = CARTESIAN_POINT ( 'NONE',  ( -16.33302336319999881, 1384.944327755149970, 200.5749513780490076 ) ) ;
#88492 = CARTESIAN_POINT ( 'NONE',  ( -24.06249508630390110, 1410.733114950599884, 208.7965224760120009 ) ) ;
#88493 = ORIENTED_EDGE ( 'NONE', *, *, #43968, .F. ) ;
#88494 = CARTESIAN_POINT ( 'NONE',  ( -0.04553580890769999556, 1421.815794421829878, 227.5038027964980074 ) ) ;
#88495 = DIRECTION ( 'NONE',  ( 0.9455185755993178454, 0.000000000000000000, -0.3255681544571537578 ) ) ;
#88496 = AXIS2_PLACEMENT_3D ( 'NONE', #147, #109881, #9611 ) ;
#88497 = FACE_OUTER_BOUND ( 'NONE', #21257, .T. ) ;
#88498 = VECTOR ( 'NONE', #62433, 1000.000000000000000 ) ;
#88499 = CARTESIAN_POINT ( 'NONE',  ( -16.41268168250000059, 1489.056318670530118, 229.5189257191980232 ) ) ;
#88500 = EDGE_CURVE ( 'NONE', #98761, #85274, #100164, .T. ) ;
#88501 = CARTESIAN_POINT ( 'NONE',  ( 1.925297170580940076, 1519.551704408389924, 230.6853930747409720 ) ) ;
#88502 = VERTEX_POINT ( 'NONE', #728 ) ;
#88503 = LINE ( 'NONE', #53827, #92812 ) ;
#88504 = CARTESIAN_POINT ( 'NONE',  ( -12.71641934408000019, 1415.429375168339902, 221.3762486804189962 ) ) ;
#88505 = ADVANCED_FACE ( 'NONE', ( #8547 ), #69792, .T. ) ;
#88506 = CARTESIAN_POINT ( 'NONE',  ( 14.18404988999999894, 1463.784527685830199, 224.5937116242980096 ) ) ;
#88507 = VERTEX_POINT ( 'NONE', #70717 ) ;
#88508 = CARTESIAN_POINT ( 'NONE',  ( -5.784008673325000238, 1516.911981270829983, 204.1205073037870079 ) ) ;
#88509 = ORIENTED_EDGE ( 'NONE', *, *, #20435, .T. ) ;
#88510 = CARTESIAN_POINT ( 'NONE',  ( 11.84405349179480105, 1430.816400222050106, 149.7709986801920081 ) ) ;
#88511 = B_SPLINE_CURVE_WITH_KNOTS ( 'NONE', 5,
 ( #21871, #91316, #73977, #48230, #39816, #108107, #81799, #39254, #14598 ),
 .UNSPECIFIED., .F., .F.,
 ( 6, 3, 6 ),
 ( 0.000000000000000000, 0.4996938382793605915, 1.000000000000000000 ),
 .UNSPECIFIED. ) ;
#88512 = CARTESIAN_POINT ( 'NONE',  ( 13.42720001465534629, 1444.358310982252533, 187.7973124303245811 ) ) ;
#88513 = ORIENTED_EDGE ( 'NONE', *, *, #91348, .F. ) ;
#88514 = EDGE_LOOP ( 'NONE', ( #57564, #92885, #46944, #1610 ) ) ;
#88515 = CARTESIAN_POINT ( 'NONE',  ( -1.455133652010000000, 1471.168344426330123, 183.0463840045979964 ) ) ;
#88516 = CARTESIAN_POINT ( 'NONE',  ( -4.886558140047800869, 1508.210669107129888, 220.4867294332269978 ) ) ;
#88517 = CARTESIAN_POINT ( 'NONE',  ( 3.314513664071169874, 1498.768387937489933, 198.2102665491759979 ) ) ;
#88518 = CARTESIAN_POINT ( 'NONE',  ( -4.092846354029450850, 1470.326128854550007, 218.4017925004950200 ) ) ;
#88519 = CARTESIAN_POINT ( 'NONE',  ( -30.31052258194604576, 1523.604703353109699, 195.7506062427372058 ) ) ;
#88520 = CARTESIAN_POINT ( 'NONE',  ( 0.4918853724044109921, 1407.650947704770033, 270.1377426703190281 ) ) ;
#88521 = CARTESIAN_POINT ( 'NONE',  ( 4.240938128610653557, 1509.032014137962506, 205.3774164840951357 ) ) ;
#88522 = CARTESIAN_POINT ( 'NONE',  ( -6.927514301909999617, 1474.889786700390005, 201.4444059491990231 ) ) ;
#88523 = CARTESIAN_POINT ( 'NONE',  ( 10.69530588519999981, 1492.057806767089915, 212.3894099842489993 ) ) ;
#88524 = CARTESIAN_POINT ( 'NONE',  ( -17.71193101166619854, 1521.951704408389787, 221.5709757775249784 ) ) ;
#88525 = CARTESIAN_POINT ( 'NONE',  ( 7.937011329750911059, 1423.927594114607018, 195.7595643984233220 ) ) ;
#88527 = CARTESIAN_POINT ( 'NONE',  ( 13.58268853709999924, 1416.851343898729965, 196.3340833726979895 ) ) ;
#88526 = CARTESIAN_POINT ( 'NONE',  ( -14.30100077960000071, 1503.190056882890076, 209.1269527976280074 ) ) ;
#88528 = CARTESIAN_POINT ( 'NONE',  ( -48.20259525661973043, 1379.738770687325086, 241.4393370634903988 ) ) ;
#88529 = EDGE_CURVE ( 'NONE', #46346, #16403, #25969, .T. ) ;
#88530 = CARTESIAN_POINT ( 'NONE',  ( 17.65466472533700326, 1412.463031515849934, 224.8541166168249958 ) ) ;
#88531 = CARTESIAN_POINT ( 'NONE',  ( -6.169347562924999195, 1511.326779185850000, 201.5833654368269947 ) ) ;
#88532 = EDGE_LOOP ( 'NONE', ( #327, #2612, #17325, #75564 ) ) ;
#88533 = CARTESIAN_POINT ( 'NONE',  ( 5.052203703969999182, 1416.825952163429974, 255.3819207742980097 ) ) ;
#88534 = CARTESIAN_POINT ( 'NONE',  ( 18.65749896656096496, 1509.387464492215713, 187.4422726699444866 ) ) ;
#88535 = CARTESIAN_POINT ( 'NONE',  ( -60.29112477526700076, 1385.064694404370130, 281.4546780721300365 ) ) ;
#88536 = CARTESIAN_POINT ( 'NONE',  ( 32.02808312589916540, 1512.187213306747481, 198.2787714533495489 ) ) ;
#88537 = AXIS2_PLACEMENT_3D ( 'NONE', #18922, #101821, #93986 ) ;
#88538 = CARTESIAN_POINT ( 'NONE',  ( 4.581657872230000095, 1506.594992437789870, 219.8628132245989946 ) ) ;
#88539 = CARTESIAN_POINT ( 'NONE',  ( -15.01049612569999958, 1415.677402202029953, 210.8311137397190009 ) ) ;
#88541 = ORIENTED_EDGE ( 'NONE', *, *, #42666, .T. ) ;
#88540 = CARTESIAN_POINT ( 'NONE',  ( -5.534100668969379910, 1464.371862158079921, 199.5915835189479992 ) ) ;
#88542 = CARTESIAN_POINT ( 'NONE',  ( 17.35267692490000258, 1414.988015876730060, 210.4487656595580063 ) ) ;
#88543 = ADVANCED_FACE ( 'NONE', ( #95328 ), #59107, .T. ) ;
#88544 = CARTESIAN_POINT ( 'NONE',  ( -2.434657972054051100, 1449.456394606908361, 154.4645640298018918 ) ) ;
#88545 = CARTESIAN_POINT ( 'NONE',  ( -12.54019733330000008, 1391.397793261360221, 209.7548870936209937 ) ) ;
#88546 = CARTESIAN_POINT ( 'NONE',  ( 11.59188835883499991, 1512.902436350919970, 225.5633015321670030 ) ) ;
#88547 = CARTESIAN_POINT ( 'NONE',  ( 3.861717407563222793, 1370.346415241654313, 208.3041812415887932 ) ) ;
#88548 = CIRCLE ( 'NONE', #59942, 2.000000000000001776 ) ;
#88549 = CARTESIAN_POINT ( 'NONE',  ( 17.06735424545500024, 1509.588153667619963, 233.8544743334759914 ) ) ;
#88550 = EDGE_CURVE ( 'NONE', #1585, #103193, #10778, .T. ) ;
#88551 = CARTESIAN_POINT ( 'NONE',  ( -40.27308906366239682, 1443.612067134240078, 137.1163379626329970 ) ) ;
#88552 = CARTESIAN_POINT ( 'NONE',  ( -11.73230603450000054, 1475.513060387329915, 226.3291547820980156 ) ) ;
#88553 = CARTESIAN_POINT ( 'NONE',  ( 15.64385495210000165, 1412.747091720930030, 227.2162067996979999 ) ) ;
#88554 = B_SPLINE_CURVE_WITH_KNOTS ( 'NONE', 5,
 ( #66642, #92909, #94011, #101284, #8343, #31902, #49829, #24579, #41422, #59341, #57689, #15082, #91804, #25138 ),
 .UNSPECIFIED., .F., .F.,
 ( 6, 2, 3, 3, 6 ),
 ( -60.28232112689999411, -50.75108181390000084, -43.93735686660000539, -43.22195389150000011, -41.21984250090000046 ),
 .UNSPECIFIED. ) ;
#88555 = CARTESIAN_POINT ( 'NONE',  ( -8.725374284720000873, 1478.773129111890057, 217.0898278110490196 ) ) ;
#88556 = CARTESIAN_POINT ( 'NONE',  ( -16.96620414819999922, 1460.582764900229904, 228.2621087521980030 ) ) ;
#88557 = CARTESIAN_POINT ( 'NONE',  ( 3.445201488374999954, 1516.743010792419909, 207.4064848398570291 ) ) ;
#88558 = CARTESIAN_POINT ( 'NONE',  ( 45.32382092809999818, 1434.935672970719907, 266.4295321061979962 ) ) ;
#88559 = CARTESIAN_POINT ( 'NONE',  ( -18.35086141989999931, 1409.718682756730004, 223.0331779077980059 ) ) ;
#88560 = CARTESIAN_POINT ( 'NONE',  ( 21.21222413589999789, 1436.051885491429857, 143.9410731133980050 ) ) ;
#88561 = CARTESIAN_POINT ( 'NONE',  ( 19.17287356779999996, 1469.162364348330129, 190.7723560717980149 ) ) ;
#88562 = CARTESIAN_POINT ( 'NONE',  ( 5.369163426388340099, 1427.167559700779975, 153.2169079524520043 ) ) ;
#88563 = FACE_OUTER_BOUND ( 'NONE', #64183, .T. ) ;
#88564 = CARTESIAN_POINT ( 'NONE',  ( -16.85082183769999986, 1423.343525757829866, 227.0118847376980113 ) ) ;
#88565 = DIRECTION ( 'NONE',  ( 0.9858563016923833633, 0.000000000000000000, 0.1675928173085483863 ) ) ;
#88566 = DIRECTION ( 'NONE',  ( 0.2054769195713317398, -1.225281874271768203E-16, 0.9786619618251628516 ) ) ;
#88567 = CARTESIAN_POINT ( 'NONE',  ( -13.82235482710600039, 1408.877038801369963, 210.6069041857849697 ) ) ;
#88568 = CARTESIAN_POINT ( 'NONE',  ( -15.44258166179999847, 1414.913060387329779, 203.7071583754979827 ) ) ;
#88569 = CARTESIAN_POINT ( 'NONE',  ( -12.65658667800000003, 1442.791283154439952, 186.1190103994979950 ) ) ;
#88570 = ADVANCED_FACE ( 'NONE', ( #63415 ), #37071, .F. ) ;
#88571 = CARTESIAN_POINT ( 'NONE',  ( -27.93079119180610093, 1508.830486288999964, 210.6192819018250191 ) ) ;
#88572 = CARTESIAN_POINT ( 'NONE',  ( 13.80595060949999997, 1434.979618316850065, 146.5972947611979862 ) ) ;
#88573 = CARTESIAN_POINT ( 'NONE',  ( -33.91369292130000446, 1435.681789575369976, 135.0664759990980315 ) ) ;
#88574 = CARTESIAN_POINT ( 'NONE',  ( -7.743156676465178911, 1456.414080484902570, 227.4372369063648591 ) ) ;
#88575 = EDGE_LOOP ( 'NONE', ( #54133, #3568, #6691, #95447 ) ) ;
#88576 = CARTESIAN_POINT ( 'NONE',  ( 5.898235284490000119, 1476.924971998690125, 199.0552711020989705 ) ) ;
#88577 = CARTESIAN_POINT ( 'NONE',  ( -1.565132884227080190, 1408.967716032030012, 224.0361922849110101 ) ) ;
#88578 = FACE_OUTER_BOUND ( 'NONE', #99737, .T. ) ;
#88579 = ORIENTED_EDGE ( 'NONE', *, *, #26729, .F. ) ;
#88581 = EDGE_CURVE ( 'NONE', #15971, #36895, #36709, .T. ) ;
#88580 = CARTESIAN_POINT ( 'NONE',  ( -13.34067739081810089, 1508.245746154080052, 209.5313100501030021 ) ) ;
#88582 = CARTESIAN_POINT ( 'NONE',  ( -17.22592475669953416, 1443.913060387330688, 162.9227486557969655 ) ) ;
#88583 = CARTESIAN_POINT ( 'NONE',  ( -44.66932832909999718, 1451.100843914730149, 266.4486768909980015 ) ) ;
#88584 = CARTESIAN_POINT ( 'NONE',  ( -11.79463582115499953, 1481.484189516729884, 210.3155264287200055 ) ) ;
#88585 = CARTESIAN_POINT ( 'NONE',  ( 0.4599152650301550072, 1418.782133919569787, 184.7029683564409765 ) ) ;
#88586 = CARTESIAN_POINT ( 'NONE',  ( -27.48211786359999920, 1509.872757090430014, 218.9219095898779983 ) ) ;
#88587 = CARTESIAN_POINT ( 'NONE',  ( -92.03485832854140369, 1384.615476698869998, 309.3200307111670213 ) ) ;
#88588 = CARTESIAN_POINT ( 'NONE',  ( -49.41110956018160749, 1385.017027258259986, 224.3527585868430094 ) ) ;
#88589 = FACE_OUTER_BOUND ( 'NONE', #23170, .T. ) ;
#88590 = DIRECTION ( 'NONE',  ( -0.000000000000000000, -1.000000000000000000, 0.000000000000000000 ) ) ;
#88591 = CARTESIAN_POINT ( 'NONE',  ( 2.553512956640000223E-15, 1433.447556881219953, 155.4376913957980264 ) ) ;
#88592 = EDGE_CURVE ( 'NONE', #288, #89851, #10832, .T. ) ;
#88593 = CARTESIAN_POINT ( 'NONE',  ( 1.191524307911311364, 1526.382868172864164, 179.0083900503168479 ) ) ;
#88595 = VERTEX_POINT ( 'NONE', #27568 ) ;
#88594 = CARTESIAN_POINT ( 'NONE',  ( 0.5076376709490001415, 1370.038171240497604, 206.9860627148225376 ) ) ;
#88596 = CARTESIAN_POINT ( 'NONE',  ( -5.682125987650000098, 1507.354943063129895, 181.2351845632980201 ) ) ;
#88598 = CARTESIAN_POINT ( 'NONE',  ( 5.371102036599521234, 1422.361277206714249, 138.9487451065114954 ) ) ;
#88597 = VECTOR ( 'NONE', #94474, 1000.000000000000114 ) ;
#88599 = CARTESIAN_POINT ( 'NONE',  ( -9.094607871690000067, 1498.018996692389919, 216.1637154482390031 ) ) ;
#88600 = CARTESIAN_POINT ( 'NONE',  ( -11.50684714910000039, 1415.041103189330215, 195.7533805636979878 ) ) ;
#88601 = CARTESIAN_POINT ( 'NONE',  ( 1.778378100730000133, 1422.883737999489995, 193.3551376869990008 ) ) ;
#88602 = CARTESIAN_POINT ( 'NONE',  ( 22.18009780759999927, 1409.687606470130049, 211.3518347607079875 ) ) ;
#88603 = B_SPLINE_SURFACE_WITH_KNOTS ( 'NONE', 5, 1, ( 
 ( #71127, #26313 ),
 ( #43689, #104486 ),
 ( #77093, #36187 ),
 ( #35619, #8200 ),
 ( #85454, #69251 ),
 ( #44594, #402 ) ),
 .UNSPECIFIED., .F., .F., .F.,
 ( 6, 6 ),
 ( 2, 2 ),
 ( 65.12638661990000344, 66.80157803080371082 ),
 ( 0.6126846217289999563, 3.463904735919999922 ),
 .UNSPECIFIED. ) ;
#88604 = CARTESIAN_POINT ( 'NONE',  ( -106.6417041771089913, 1391.913060387289988, 305.7294994898900313 ) ) ;
#88605 = CARTESIAN_POINT ( 'NONE',  ( -3.201099014209999982, 1451.080120310989969, 188.5408260424989919 ) ) ;
#88606 = CARTESIAN_POINT ( 'NONE',  ( -3.567499890613730074, 1508.690874479150125, 180.4371998924179934 ) ) ;
#88608 = CARTESIAN_POINT ( 'NONE',  ( -12.71390971709999995, 1379.576682373769927, 206.2215170013890031 ) ) ;
#88607 = CARTESIAN_POINT ( 'NONE',  ( -11.58215570839999842, 1432.723904499930086, 151.1956759123980021 ) ) ;
#88609 = CARTESIAN_POINT ( 'NONE',  ( -5.087358518910000349, 1391.865222393290196, 203.6716085637289950 ) ) ;
#88610 = CARTESIAN_POINT ( 'NONE',  ( -120.4155570069220431, 1376.302340817389222, 292.3950450905591083 ) ) ;
#88611 = CARTESIAN_POINT ( 'NONE',  ( -203.9558787908000284, -8382.262153571269664, 2179.147420460110425 ) ) ;
#88612 = EDGE_CURVE ( 'NONE', #7480, #108583, #39420, .T. ) ;
#88613 = DIRECTION ( 'NONE',  ( 0.1403901532130616969, 0.9900962604114879051, 0.000000000000000000 ) ) ;
#88614 = CARTESIAN_POINT ( 'NONE',  ( -9.657355732019999195, 1366.083296228050131, 210.6218459616991936 ) ) ;
#88615 = CARTESIAN_POINT ( 'NONE',  ( -5.784008673325000238, 1516.911981270829983, 204.1205073037870079 ) ) ;
#88616 = CARTESIAN_POINT ( 'NONE',  ( -20.74894096239999897, 1428.237764131229824, 223.0444765198980122 ) ) ;
#88617 = CARTESIAN_POINT ( 'NONE',  ( -16.67123089062359753, 1485.152086820359955, 188.0413787914010015 ) ) ;
#88618 = ADVANCED_FACE ( 'NONE', ( #79648 ), #46049, .T. ) ;
#88619 = DIRECTION ( 'NONE',  ( -0.02616798426500960631, -0.9993150019883682011, 0.02616798426500970345 ) ) ;
#88620 = CARTESIAN_POINT ( 'NONE',  ( -13.34182121425549994, 1421.262884902478618, 210.6379646114695277 ) ) ;
#88622 = ORIENTED_EDGE ( 'NONE', *, *, #6879, .T. ) ;
#88621 = CARTESIAN_POINT ( 'NONE',  ( -67.56980796919920351, 1379.745055568280122, 278.8799826345460815 ) ) ;
#88623 = ORIENTED_EDGE ( 'NONE', *, *, #27140, .T. ) ;
#88624 = CARTESIAN_POINT ( 'NONE',  ( 27.67579904629999987, 1509.157128445930084, 213.4451930261979840 ) ) ;
#88625 = VERTEX_POINT ( 'NONE', #52239 ) ;
#88626 = CARTESIAN_POINT ( 'NONE',  ( -105.7942891969999977, 1378.913060387289988, 304.0474106464590136 ) ) ;
#88627 = AXIS2_PLACEMENT_3D ( 'NONE', #41853, #110161, #93350 ) ;
#88628 = CARTESIAN_POINT ( 'NONE',  ( 1.555730441589999957, 1414.913528139930122, 192.0047335902979739 ) ) ;
#88630 = CARTESIAN_POINT ( 'NONE',  ( 23.03439503529999755, 1449.683642696550123, 219.5641606253980171 ) ) ;
#88629 = CARTESIAN_POINT ( 'NONE',  ( 0.7904366496569998901, 1426.935925255829943, 133.6118001900980232 ) ) ;
#88631 = CARTESIAN_POINT ( 'NONE',  ( 2.500000000000000000, 1417.575542695230070, 161.0097146487299824 ) ) ;
#88632 = CARTESIAN_POINT ( 'NONE',  ( -23.99188238352159885, 1452.075290040919981, 136.8468086068940295 ) ) ;
#88633 = CARTESIAN_POINT ( 'NONE',  ( -2.031695188920000117, 1468.162652163589883, 219.6587382871989860 ) ) ;
#88634 = CARTESIAN_POINT ( 'NONE',  ( 7.252569847259999314, 1409.670284998229818, 230.5441453657980162 ) ) ;
#88635 = CARTESIAN_POINT ( 'NONE',  ( 12.49721897139709981, 1501.189573146680004, 211.4713583651110014 ) ) ;
#88636 =( NAMED_UNIT ( * ) PLANE_ANGLE_UNIT ( ) SI_UNIT ( $, .RADIAN. ) );
#88637 = CARTESIAN_POINT ( 'NONE',  ( -3.446942109845000157, 1516.842852731759876, 212.3891375753969726 ) ) ;
#88639 = CIRCLE ( 'NONE', #97575, 7.500000000000000000 ) ;
#88638 = CARTESIAN_POINT ( 'NONE',  ( 40.76227011262719202, 1440.007145189029870, 134.0999999980880091 ) ) ;
#88640 = FACE_OUTER_BOUND ( 'NONE', #79140, .T. ) ;
#88641 = EDGE_LOOP ( 'NONE', ( #14552, #62500, #77099, #40606 ) ) ;
#88642 = FACE_OUTER_BOUND ( 'NONE', #22481, .T. ) ;
#88643 = CARTESIAN_POINT ( 'NONE',  ( -1.541238598094009972E-13, 1515.051704408389924, 212.9514660752490158 ) ) ;
#88644 = ORIENTED_EDGE ( 'NONE', *, *, #55661, .F. ) ;
#88645 = ORIENTED_EDGE ( 'NONE', *, *, #39541, .F. ) ;
#88646 = VERTEX_POINT ( 'NONE', #86367 ) ;
#88647 = CARTESIAN_POINT ( 'NONE',  ( -7.163002535094999956, 1512.132770473890105, 215.9896253418369838 ) ) ;
#88648 = CARTESIAN_POINT ( 'NONE',  ( 36.02435014169089555, 1445.276583512550133, 137.0631246346559919 ) ) ;
#88649 = CARTESIAN_POINT ( 'NONE',  ( 15.09916686074197578, 1451.148571410817340, 149.6580463515937822 ) ) ;
#88650 = CARTESIAN_POINT ( 'NONE',  ( -7.769002072320000174, 1384.928845199370016, 218.9178307580690159 ) ) ;
#88651 = CARTESIAN_POINT ( 'NONE',  ( 0.6565761022465029795, 1465.559853904359898, 198.1292258770540116 ) ) ;
#88652 = CARTESIAN_POINT ( 'NONE',  ( -16.73703974548556417, 1449.615440745906653, 220.0451451102140368 ) ) ;
#88653 = CARTESIAN_POINT ( 'NONE',  ( -68.48903935974368551, 1379.747406510886776, 279.4606711651055662 ) ) ;
#88654 = CARTESIAN_POINT ( 'NONE',  ( 4.262306684643539789, 1446.607359238689924, 159.1811806424360043 ) ) ;
#88655 =( BOUNDED_SURFACE ( )  B_SPLINE_SURFACE ( 3, 2, ( 
 ( #34429, #25451, #50148 ),
 ( #16490, #42278, #58544 ),
 ( #67503, #49593, #92670 ),
 ( #7571, #50680, #84812 ),
 ( #84275, #8111, #9237 ),
 ( #93755, #76429, #102169 ),
 ( #103260, #33867, #41725 ),
 ( #110033, #17032, #68058 ),
 ( #51230, #85363, #94316 ),
 ( #102705, #75885, #68602 ),
 ( #8658, #76996, #96551 ),
 ( #9775, #44499, #71392 ),
 ( #106054, #43941, #11447 ),
 ( #71941, #54031, #18710 ) ),
 .UNSPECIFIED., .F., .F., .F. ) 
 B_SPLINE_SURFACE_WITH_KNOTS ( ( 4, 2, 2, 2, 2, 2, 4 ),
 ( 3, 3 ),
 ( 3.068292148133977548E-17, 0.0009443072508235996528, 0.001416460876235384192, 0.001888614501647168731, 0.002360768127058953270, 0.002832921752470737593, 0.003777229003294306671 ),
 ( 0.000000000000000000, 1.000000000000000000 ),
 .UNSPECIFIED. ) 
 GEOMETRIC_REPRESENTATION_ITEM ( )  RATIONAL_B_SPLINE_SURFACE ( (
 ( 1.000000000000000000, 0.9376006582765952224, 1.000000000000000000),
 ( 1.000000000000000000, 0.9283977714737551290, 1.000000000000000000),
 ( 1.000000000000000000, 0.9189750060478811822, 1.000000000000000000),
 ( 1.000000000000000000, 0.9042792056128057254, 1.000000000000000000),
 ( 1.000000000000000000, 0.8992469033844706638, 1.000000000000000000),
 ( 1.000000000000000000, 0.8891280264680628820, 1.000000000000000000),
 ( 1.000000000000000000, 0.8840337471674211134, 1.000000000000000000),
 ( 1.000000000000000000, 0.8736395124164628712, 1.000000000000000000),
 ( 1.000000000000000000, 0.8683406746553720135, 1.000000000000000000),
 ( 1.000000000000000000, 0.8573361860706717463, 1.000000000000000000),
 ( 1.000000000000000000, 0.8516508399495776871, 1.000000000000000000),
 ( 1.000000000000000000, 0.8340914917066705181, 1.000000000000000000),
 ( 1.000000000000000000, 0.8215597275861525883, 1.000000000000000000),
 ( 1.000000000000000000, 0.8070209408750226299, 1.000000000000000000) ) ) 
 REPRESENTATION_ITEM ( '' )  SURFACE ( )  );
#88656 = CARTESIAN_POINT ( 'NONE',  ( 0.01130987586839999996, 1507.369121482229957, 237.3632175159979738 ) ) ;
#88657 = ORIENTED_EDGE ( 'NONE', *, *, #95210, .T. ) ;
#88658 = CARTESIAN_POINT ( 'NONE',  ( 5.770820141135000192, 1516.591755933730155, 207.4105347035570048 ) ) ;
#88659 = ORIENTED_EDGE ( 'NONE', *, *, #16624, .T. ) ;
#88660 = CARTESIAN_POINT ( 'NONE',  ( 27.83576393251260228, 1440.913060387330006, 247.1867187401149977 ) ) ;
#88661 = CARTESIAN_POINT ( 'NONE',  ( -2.348318232329873353E-05, 1452.887054547371918, 152.8599681479486776 ) ) ;
#88662 = VERTEX_POINT ( 'NONE', #31970 ) ;
#88663 = FACE_OUTER_BOUND ( 'NONE', #6157, .T. ) ;
#88664 = CARTESIAN_POINT ( 'NONE',  ( -15.10863497539999933, 1409.942448651430141, 191.0446830422980042 ) ) ;
#88665 = CARTESIAN_POINT ( 'NONE',  ( -18.74471293385864712, 1508.457619993740082, 210.6713976521029110 ) ) ;
#88667 = CARTESIAN_POINT ( 'NONE',  ( 14.86137034542100110, 1512.142158944850053, 196.7831344732769878 ) ) ;
#88666 = CARTESIAN_POINT ( 'NONE',  ( -24.90528981920000007, 1441.263847370060148, 210.4373564352579820 ) ) ;
#88668 = CARTESIAN_POINT ( 'NONE',  ( 22.31280560966569837, 1410.332809971110009, 206.2360209584310269 ) ) ;
#88669 = CARTESIAN_POINT ( 'NONE',  ( -6.048292043943890306, 1511.681069547209972, 200.4825432859090029 ) ) ;
#88670 = DIRECTION ( 'NONE',  ( -0.4999997527789440399, 0.7071067730516870098, 0.5000002587253580266 ) ) ;
#88671 = DIRECTION ( 'NONE',  ( -5.980589973904019347E-17, 1.000000000000000000, -1.736889445713099699E-16 ) ) ;
#88672 = CARTESIAN_POINT ( 'NONE',  ( -5.584613240470000406, 1508.184945842690013, 220.3909862082990117 ) ) ;
#88674 = CARTESIAN_POINT ( 'NONE',  ( -13.16517659032116860, 1517.051704408389924, 224.1947148507618408 ) ) ;
#88673 = CARTESIAN_POINT ( 'NONE',  ( 6.162479943850000197, 1464.100498801029971, 234.9357781952980133 ) ) ;
#88675 = CARTESIAN_POINT ( 'NONE',  ( 6.555393117025000826, 1516.809497469189864, 216.4498952504870033 ) ) ;
#88676 = CARTESIAN_POINT ( 'NONE',  ( -2.493590731671294414, 1524.152444737676660, 242.7218577030689062 ) ) ;
#88677 = CARTESIAN_POINT ( 'NONE',  ( 5.890586664718879817, 1511.182265711489890, 216.8011604359759872 ) ) ;
#88678 = CARTESIAN_POINT ( 'NONE',  ( 28.31864921020000025, 1509.156311056829963, 208.1546065555820064 ) ) ;
#88679 = CARTESIAN_POINT ( 'NONE',  ( -1.702406023195000007, 1516.999105586269934, 212.3918307515370145 ) ) ;
#88680 = AXIS2_PLACEMENT_3D ( 'NONE', #54548, #19798, #11422 ) ;
#88681 = CARTESIAN_POINT ( 'NONE',  ( -19.73776679940000278, 1452.815214894829978, 209.0753000189979787 ) ) ;
#88682 = DIRECTION ( 'NONE',  ( -1.000000000000000000, 0.000000000000000000, 0.000000000000000000 ) ) ;
#88684 = ORIENTED_EDGE ( 'NONE', *, *, #46053, .T. ) ;
#88683 = CARTESIAN_POINT ( 'NONE',  ( -113.4000000000000057, 1388.279812043220090, 298.3521000786590207 ) ) ;
#88685 = CARTESIAN_POINT ( 'NONE',  ( -16.49279160078807038, 1525.408337840050763, 236.9553505360240138 ) ) ;
#88686 = CARTESIAN_POINT ( 'NONE',  ( 30.53571888249999944, 1440.913060384770006, 240.1260121784980015 ) ) ;
#88687 = CARTESIAN_POINT ( 'NONE',  ( -10.97019733509999995, 1432.400418277960171, 151.7699536590980074 ) ) ;
#88688 = CARTESIAN_POINT ( 'NONE',  ( -15.56145363769999967, 1415.973220584759929, 207.8153022160889805 ) ) ;
#88689 = CARTESIAN_POINT ( 'NONE',  ( -1.423894748726279857, 1507.656498555010103, 237.2172253236890072 ) ) ;
#88690 = B_SPLINE_CURVE_WITH_KNOTS ( 'NONE', 5,
 ( #65436, #58129, #23399, #58678, #74936, #14436, #99545, #7162, #57035 ),
 .UNSPECIFIED., .F., .F.,
 ( 6, 3, 6 ),
 ( 0.000000000000000000, 0.5000000000000000000, 1.000000000000000000 ),
 .UNSPECIFIED. ) ;
#88691 = CARTESIAN_POINT ( 'NONE',  ( -22.89636893299999798, 1449.797811951130143, 219.2674029246980183 ) ) ;
#88693 = CARTESIAN_POINT ( 'NONE',  ( 19.46657980040000169, 1455.632578195829865, 226.1434856801980118 ) ) ;
#88692 = CARTESIAN_POINT ( 'NONE',  ( 11.87490714379999979, 1433.006767503300125, 150.3951466330979940 ) ) ;
#88694 = CARTESIAN_POINT ( 'NONE',  ( -0.2353198522280000038, 1506.810797420529980, 187.1186863663980091 ) ) ;
#88695 = CARTESIAN_POINT ( 'NONE',  ( -105.5885868690189966, 1378.666813780319899, 305.5093639108209800 ) ) ;
#88696 = EDGE_LOOP ( 'NONE', ( #85365, #87958, #59447, #84333, #41670, #64680, #73932, #12598, #108287, #22846, #106008, #9683, #3916, #97241, #50734, #43069, #59007, #92771, #22345, #59779, #63655 ) ) ;
#88697 = CARTESIAN_POINT ( 'NONE',  ( -5.784638357945000031, 1516.939574742129935, 204.5080835752170003 ) ) ;
#88698 = CARTESIAN_POINT ( 'NONE',  ( 1.323291931630000029, 1406.278073745629854, 269.2941001024979641 ) ) ;
#88699 = CARTESIAN_POINT ( 'NONE',  ( 1.471738374290000095, 1515.341568496189893, 213.3962787526390059 ) ) ;
#88700 = AXIS2_PLACEMENT_3D ( 'NONE', #83621, #84174, #6375 ) ;
#88701 = CARTESIAN_POINT ( 'NONE',  ( 31.66981299747059708, 1465.623440352080024, 270.1133457425380016 ) ) ;
#88702 = CARTESIAN_POINT ( 'NONE',  ( -26.56014455169999877, 1451.985525993130068, 134.9308153408980218 ) ) ;
#88703 = CARTESIAN_POINT ( 'NONE',  ( 22.08622291482350519, 1512.187213306747481, 233.8253038720783366 ) ) ;
#88704 = EDGE_CURVE ( 'NONE', #97242, #66900, #43464, .T. ) ;
#88705 = CARTESIAN_POINT ( 'NONE',  ( -20.39146254758225751, 1526.073434386618828, 233.1306592966913627 ) ) ;
#88706 = CARTESIAN_POINT ( 'NONE',  ( -30.31940284292399213, 1523.456872492435195, 222.4933038710547919 ) ) ;
#88707 = CARTESIAN_POINT ( 'NONE',  ( -0.6251419943069990159, 1430.668067383890047, 200.4025769807989832 ) ) ;
#88708 = EDGE_CURVE ( 'NONE', #101252, #30502, #34141, .T. ) ;
#88709 = CARTESIAN_POINT ( 'NONE',  ( -15.94269987122453536, 1416.079329809435649, 209.7066221775000656 ) ) ;
#88710 = CARTESIAN_POINT ( 'NONE',  ( -0.7502145772460020456, 1508.757402103690083, 220.8877261029990109 ) ) ;
#88711 = CARTESIAN_POINT ( 'NONE',  ( -18.74729292449999818, 1442.199705176290081, 209.1218459616989946 ) ) ;
#88712 = ORIENTED_EDGE ( 'NONE', *, *, #37893, .F. ) ;
#88713 = CARTESIAN_POINT ( 'NONE',  ( -6.850948847420000654, 1425.447270615729849, 224.8635561966979708 ) ) ;
#88714 = CARTESIAN_POINT ( 'NONE',  ( 9.577710299738889432, 1468.749342511669965, 205.5349571559659978 ) ) ;
#88715 = CARTESIAN_POINT ( 'NONE',  ( -0.3382973561789999750, 1475.836249162829972, 266.9611136385980217 ) ) ;
#88716 = CARTESIAN_POINT ( 'NONE',  ( -4.262501422047650479, 1446.609523482700070, 159.1513637479519900 ) ) ;
#88717 = CARTESIAN_POINT ( 'NONE',  ( -28.26084321609999961, 1508.649017708029987, 209.6368911950440008 ) ) ;
#88718 = CARTESIAN_POINT ( 'NONE',  ( -113.4000000000000057, 1377.913060387289988, 304.2218459572590064 ) ) ;
#88719 = CARTESIAN_POINT ( 'NONE',  ( -34.25392201084810040, 1384.812092138909975, 233.1617710834259753 ) ) ;
#88720 = EDGE_CURVE ( 'NONE', #64221, #102140, #37677, .T. ) ;
#88721 = CARTESIAN_POINT ( 'NONE',  ( -17.92792478850000037, 1415.296882282229944, 208.1699612212720183 ) ) ;
#88722 = CARTESIAN_POINT ( 'NONE',  ( -10.10336395149999866, 1482.676368233689800, 204.5951876114990000 ) ) ;
#88723 = CARTESIAN_POINT ( 'NONE',  ( 26.79415489093269898, 1435.433178437559945, 135.2874578969010031 ) ) ;
#88724 = CARTESIAN_POINT ( 'NONE',  ( -2.574213757757640053, 1396.002953912619887, 219.8362960026119879 ) ) ;
#88725 = CARTESIAN_POINT ( 'NONE',  ( -14.90609184490000061, 1421.333676412129989, 227.2836066624979878 ) ) ;
#88726 = CARTESIAN_POINT ( 'NONE',  ( 9.660544699540000835, 1432.353341358199941, 148.7316627034979888 ) ) ;
#88727 = ORIENTED_EDGE ( 'NONE', *, *, #105580, .T. ) ;
#88728 = CARTESIAN_POINT ( 'NONE',  ( -11.36969477628213276, 1501.477747086209320, 207.7773368182330671 ) ) ;
#88729 = DIRECTION ( 'NONE',  ( 0.6768489701308448847, 0.6839977328998089190, -0.2720708970484284062 ) ) ;
#88730 = CARTESIAN_POINT ( 'NONE',  ( -4.338670661869993062, 1484.259043665225363, 183.5078876442977389 ) ) ;
#88732 = CARTESIAN_POINT ( 'NONE',  ( -14.20095109106500075, 1513.466724478469814, 192.5929703138669993 ) ) ;
#88731 = CARTESIAN_POINT ( 'NONE',  ( 11.12283182329999853, 1426.473557707429791, 99.60385865669789496 ) ) ;
#88733 = CARTESIAN_POINT ( 'NONE',  ( -17.17241001986523941, 1511.187213306747708, 181.6185504016045797 ) ) ;
#88734 = CARTESIAN_POINT ( 'NONE',  ( -13.51610093808349866, 1443.913060387330006, 151.4871142704430156 ) ) ;
#88735 = CARTESIAN_POINT ( 'NONE',  ( -4.993214560040000194, 1391.653934889589891, 203.5347113830289913 ) ) ;
#88736 = CARTESIAN_POINT ( 'NONE',  ( 7.733699955179999641, 1424.219764885950099, 212.1813203967790002 ) ) ;
#88737 = CARTESIAN_POINT ( 'NONE',  ( -21.59687142900000012, 1507.523380033690046, 209.4572543540780032 ) ) ;
#88738 = CARTESIAN_POINT ( 'NONE',  ( 6.951567194469999933, 1508.626707931329747, 181.9880926591980312 ) ) ;
#88739 = CARTESIAN_POINT ( 'NONE',  ( -55.42473571849600233, 1377.502816453089963, 260.3293090052349612 ) ) ;
#88740 = ADVANCED_FACE ( 'NONE', ( #56636 ), #44768, .T. ) ;
#88741 = CARTESIAN_POINT ( 'NONE',  ( 9.231361398851440470, 1366.659448741856067, 210.6218459616987957 ) ) ;
#88743 = ORIENTED_EDGE ( 'NONE', *, *, #33017, .T. ) ;
#88742 = CARTESIAN_POINT ( 'NONE',  ( 8.498877730000000241, 1453.128683867390009, 213.4054510080989928 ) ) ;
#88744 = ORIENTED_EDGE ( 'NONE', *, *, #85080, .F. ) ;
#88745 = CARTESIAN_POINT ( 'NONE',  ( -14.66018946070000162, 1444.034773379980152, 188.9384452558980172 ) ) ;
#88746 = CARTESIAN_POINT ( 'NONE',  ( 1.420260137469999906, 1466.712984991329904, 235.0376562393980180 ) ) ;
#88747 = LINE ( 'NONE', #38324, #24303 ) ;
#88748 = CARTESIAN_POINT ( 'NONE',  ( 6.034821872916185548, 1499.876410579053299, 199.4702867286800938 ) ) ;
#88751 = EDGE_CURVE ( 'NONE', #44452, #41116, #107577, .T. ) ;
#88750 = CARTESIAN_POINT ( 'NONE',  ( -1.364645589921620106, 1416.551493819629968, 185.3405191386750062 ) ) ;
#88749 = CARTESIAN_POINT ( 'NONE',  ( -8.127570150269997740, 1383.933791805179908, 218.6735113165989901 ) ) ;
#88752 = CARTESIAN_POINT ( 'NONE',  ( 2.011589696679999761, 1429.772212105730205, 184.5964239730980125 ) ) ;
#88753 = LINE ( 'NONE', #54076, #90802 ) ;
#88754 = CARTESIAN_POINT ( 'NONE',  ( -41.38883695897280290, 1445.149448330730138, 136.3871248988700131 ) ) ;
#88755 =( NAMED_UNIT ( * ) PLANE_ANGLE_UNIT ( ) SI_UNIT ( $, .RADIAN. ) );
#88756 = CARTESIAN_POINT ( 'NONE',  ( -2.500000000000000000, 1448.435833742209979, 161.6007892298630111 ) ) ;
#88757 = CARTESIAN_POINT ( 'NONE',  ( -12.84239665067440050, 1435.935719077439899, 150.8114796122480072 ) ) ;
#88758 = CARTESIAN_POINT ( 'NONE',  ( -27.84617737330000153, 1442.188138044959942, 137.3853255075979973 ) ) ;
#88759 = CARTESIAN_POINT ( 'NONE',  ( -6.024456086116980025, 1407.067997541940031, 269.6384956777279740 ) ) ;
#88760 = CARTESIAN_POINT ( 'NONE',  ( 41.48601861270000057, 1444.048396303439858, 136.5661520294979709 ) ) ;
#88761 = ORIENTED_EDGE ( 'NONE', *, *, #51557, .T. ) ;
#88762 = CARTESIAN_POINT ( 'NONE',  ( 4.187049558480000044, 1423.917685550429951, 184.1424272131979762 ) ) ;
#88763 = CARTESIAN_POINT ( 'NONE',  ( 21.78062404853721290, 1524.843178112496162, 233.5929681532350912 ) ) ;
#88764 = ORIENTED_EDGE ( 'NONE', *, *, #27652, .F. ) ;
#88765 = ORIENTED_EDGE ( 'NONE', *, *, #8057, .T. ) ;
#88766 = CARTESIAN_POINT ( 'NONE',  ( -33.93019615848938741, 1522.382868172863937, 220.5829544587966211 ) ) ;
#88767 = CARTESIAN_POINT ( 'NONE',  ( -13.61466181890000016, 1460.855063855429762, 231.3360755285980019 ) ) ;
#88768 = CARTESIAN_POINT ( 'NONE',  ( 6.944231748164999551, 1516.882690742909972, 215.6753703478370028 ) ) ;
#88769 = CARTESIAN_POINT ( 'NONE',  ( 2.258825551794999775, 1511.942942747529969, 216.7106486523369995 ) ) ;
#88770 = CONICAL_SURFACE ( 'NONE', #103038, 0.9999999999999857891, 0.7853981633970000820 ) ;
#88771 = ORIENTED_EDGE ( 'NONE', *, *, #15487, .F. ) ;
#88772 = CARTESIAN_POINT ( 'NONE',  ( 0.05087345101610000336, 1508.993291644029796, 179.2717210570979773 ) ) ;
#88773 = CARTESIAN_POINT ( 'NONE',  ( -94.91986059570000123, 1378.602426990669983, 300.7314404810590531 ) ) ;
#88774 = AXIS2_PLACEMENT_3D ( 'NONE', #79494, #27414, #95730 ) ;
#88775 = CARTESIAN_POINT ( 'NONE',  ( 17.66282533229999885, 1415.426091369230107, 212.8695664232880063 ) ) ;
#88776 = CARTESIAN_POINT ( 'NONE',  ( -4.041472511874999896, 1516.858649670339901, 205.0922732913970208 ) ) ;
#88777 = CARTESIAN_POINT ( 'NONE',  ( -11.96800804735369894, 1489.717015978450036, 211.5846796328700066 ) ) ;
#88778 = CARTESIAN_POINT ( 'NONE',  ( -98.86863956199999848, 1385.102662047930153, 296.2487962393589669 ) ) ;
#88779 = AXIS2_PLACEMENT_3D ( 'NONE', #66750, #67298, #99755 ) ;
#88780 = CARTESIAN_POINT ( 'NONE',  ( -4.181137680949999158, 1409.562970863930104, 231.9380548681980088 ) ) ;
#88782 = ORIENTED_EDGE ( 'NONE', *, *, #17238, .F. ) ;
#88781 = DIRECTION ( 'NONE',  ( 0.7067701472209363400, 0.03085807451170261353, 0.7067699330296433047 ) ) ;
#88783 = CARTESIAN_POINT ( 'NONE',  ( -14.25058219265448045, 1435.219475802135548, 149.2644305274596945 ) ) ;
#88784 = CARTESIAN_POINT ( 'NONE',  ( 1.742626220133139947, 1466.605724716640225, 234.7106070719929960 ) ) ;
#88785 = CARTESIAN_POINT ( 'NONE',  ( -17.46864620450000061, 1384.529923560180123, 219.9544858071590170 ) ) ;
#88786 = CARTESIAN_POINT ( 'NONE',  ( 8.968032268709999144, 1477.614756788489785, 227.8520689727990032 ) ) ;
#88787 = CARTESIAN_POINT ( 'NONE',  ( 28.70938062880000174, 1416.088826313630079, 270.3384725155980277 ) ) ;
#88788 = CARTESIAN_POINT ( 'NONE',  ( -2.284199401535000007, 1516.940296199220029, 212.3910308785969789 ) ) ;
#88789 = CARTESIAN_POINT ( 'NONE',  ( -66.34652574609999931, 1379.749084393009980, 275.3210452576589660 ) ) ;
#88790 = CARTESIAN_POINT ( 'NONE',  ( -1.543833121739990100, 1424.175334750540060, 228.3471663839470125 ) ) ;
#88791 = CARTESIAN_POINT ( 'NONE',  ( -1.906499758064230099E-08, 1515.051704408389924, 209.1218459511669892 ) ) ;
#88792 = CARTESIAN_POINT ( 'NONE',  ( 22.53878404599999641, 1411.058442739730026, 206.1986151668880041 ) ) ;
#88793 = CARTESIAN_POINT ( 'NONE',  ( -2.486220139904999904, 1516.939658295650133, 209.1350829839039989 ) ) ;
#88794 = ORIENTED_EDGE ( 'NONE', *, *, #87774, .T. ) ;
#88795 = CARTESIAN_POINT ( 'NONE',  ( 4.343520079308760273, 1421.964317546590109, 183.8964818372369905 ) ) ;
#88796 = DIRECTION ( 'NONE',  ( 0.9993908270190849930, -0.03489949670280780014, 8.033055426964939564E-16 ) ) ;
#88797 = CARTESIAN_POINT ( 'NONE',  ( 8.141878239905574688, 1423.434623704914429, 137.0999999979602535 ) ) ;
#88798 = ORIENTED_EDGE ( 'NONE', *, *, #83267, .F. ) ;
#88799 = CARTESIAN_POINT ( 'NONE',  ( -37.94803686207870186, 1385.193463608850152, 238.6440774005280048 ) ) ;
#88800 = CARTESIAN_POINT ( 'NONE',  ( -2.670663765640000520, 1430.456430591890012, 201.2104194720490113 ) ) ;
#88801 = LINE ( 'NONE', #3719, #63006 ) ;
#88802 = LINE ( 'NONE', #72563, #47538 ) ;
#88803 = CARTESIAN_POINT ( 'NONE',  ( -0.08328763183689999461, 1408.915968883630057, 232.2275454037979898 ) ) ;
#88804 = CARTESIAN_POINT ( 'NONE',  ( 0.1681674884180490159, 1420.473121907760060, 182.7464979049940155 ) ) ;
#88806 = CARTESIAN_POINT ( 'NONE',  ( 21.83863729848984292, 1523.580204110584418, 183.2673815993468054 ) ) ;
#88805 = CARTESIAN_POINT ( 'NONE',  ( 7.718763505904999711, 1516.905946377369901, 216.0642002436470079 ) ) ;
#88807 = CARTESIAN_POINT ( 'NONE',  ( -3.393904228248314947, 1496.579901245492465, 198.4093902612280260 ) ) ;
#88808 = CARTESIAN_POINT ( 'NONE',  ( 10.54397772302610115, 1470.567053305489935, 209.2853404595599898 ) ) ;
#88809 = ORIENTED_EDGE ( 'NONE', *, *, #38387, .F. ) ;
#88810 = CARTESIAN_POINT ( 'NONE',  ( -5.779603138255000161, 1516.738222552470233, 201.4074744291170020 ) ) ;
#88811 = CARTESIAN_POINT ( 'NONE',  ( -16.20447082416500351, 1512.376261820769969, 220.4782031007670184 ) ) ;
#88812 = EDGE_LOOP ( 'NONE', ( #100577, #11650, #64295, #36700, #80063 ) ) ;
#88813 = CARTESIAN_POINT ( 'NONE',  ( 11.60004869884835621, 1426.567385858177886, 135.1569352595896589 ) ) ;
#88814 = CIRCLE ( 'NONE', #51312, 0.9999999999999975575 ) ;
#88815 = CARTESIAN_POINT ( 'NONE',  ( 17.69622264849999738, 1430.679833671289771, 213.5595385020990022 ) ) ;
#88816 = CARTESIAN_POINT ( 'NONE',  ( -19.63722818134010240, 1517.051704408389924, 200.0074286634620364 ) ) ;
#88817 = CARTESIAN_POINT ( 'NONE',  ( 0.02750565378459880056, 1442.646891867090062, 219.1054768861489777 ) ) ;
#88818 = CARTESIAN_POINT ( 'NONE',  ( 15.70386933114422590, 1421.083856898652130, 227.5869605700097509 ) ) ;
#88819 = CARTESIAN_POINT ( 'NONE',  ( 5.950109296629999989, 1421.372702594429938, 186.2244564570979719 ) ) ;
#88820 = CARTESIAN_POINT ( 'NONE',  ( -18.07122677940000344, 1424.826032087529939, 227.1937097634979921 ) ) ;
#88821 = CARTESIAN_POINT ( 'NONE',  ( -15.42782019790000092, 1435.461599119239963, 148.9396145078979998 ) ) ;
#88822 = FACE_OUTER_BOUND ( 'NONE', #108980, .T. ) ;
#88823 = CARTESIAN_POINT ( 'NONE',  ( 17.16923421059999910, 1410.829425249829910, 192.1173138142980008 ) ) ;
#88825 = CARTESIAN_POINT ( 'NONE',  ( -17.29437801252285922, 1433.661299895118873, 216.7949840967941100 ) ) ;
#88824 = CARTESIAN_POINT ( 'NONE',  ( -34.18677586421173942, 1524.726013923371283, 219.7932833225216882 ) ) ;
#88826 = CARTESIAN_POINT ( 'NONE',  ( 2.038847259689227531, 1522.382868172863937, 244.9330574173806667 ) ) ;
#88828 = ORIENTED_EDGE ( 'NONE', *, *, #23589, .T. ) ;
#88827 = B_SPLINE_CURVE_WITH_KNOTS ( 'NONE', 3,
 ( #105365, #28656, #20236, #88031, #53896, #10762, #96972, #105926, #104259, #11315, #89104, #54438, #61732, #10193, #95855, #20779, #80155, #79079, #1824, #71806, #3476, #29205, #44368, #4021, #27550, #54979, #46578, #71243, #35959, #2385, #11854 ),
 .UNSPECIFIED., .F., .F.,
 ( 4, 3, 3, 3, 3, 3, 3, 3, 3, 3, 4 ),
 ( -27.07213034079750003, -26.91076046188110027, -26.52795488250579936, -26.13083096461109989, -25.74235510102220204, -25.70743013386550047, -25.40268465535810094, -25.05323574494259731, -24.71773051742599847, -24.43806349879320194, -24.41308947361219950 ),
 .UNSPECIFIED. ) ;
#88829 = CARTESIAN_POINT ( 'NONE',  ( -105.5765755770000141, 1378.244848860319962, 304.0471334908590393 ) ) ;
#88830 = CARTESIAN_POINT ( 'NONE',  ( -9.519511910620000350, 1508.480989645490126, 218.8877205799990122 ) ) ;
#88831 = CYLINDRICAL_SURFACE ( 'NONE', #56816, 2.000000000000002220 ) ;
#88832 = CARTESIAN_POINT ( 'NONE',  ( -19.39503999260000100, 1507.708763760590045, 209.4440057405769835 ) ) ;
#88833 = DIRECTION ( 'NONE',  ( -0.000000000000000000, -1.000000000000000000, -0.000000000000000000 ) ) ;
#88834 = CARTESIAN_POINT ( 'NONE',  ( -16.66194338029631439, 1417.248714584018671, 206.9614914337466587 ) ) ;
#88835 = CARTESIAN_POINT ( 'NONE',  ( -2.971820252585304800, 1425.987760232464780, 185.4345033297641692 ) ) ;
#88836 = CARTESIAN_POINT ( 'NONE',  ( 11.40030748711895825, 1434.654611036206006, 151.4913564614089125 ) ) ;
#88837 = CARTESIAN_POINT ( 'NONE',  ( -3.829620113550000315, 1515.051704408389924, 209.0973262533439936 ) ) ;
#88838 = CARTESIAN_POINT ( 'NONE',  ( -2.551544005433064477, 1507.143443351390488, 236.9472590348812275 ) ) ;
#88839 = CARTESIAN_POINT ( 'NONE',  ( -11.10192713642759976, 1489.530782677959905, 213.0257327280270090 ) ) ;
#88840 = B_SPLINE_CURVE_WITH_KNOTS ( 'NONE', 3,
 ( #93934, #91332, #100286, #82927, #17200, #51396, #85529, #107031, #21886, #23005, #57208 ),
 .UNSPECIFIED., .F., .F.,
 ( 4, 2, 1, 1, 1, 2, 4 ),
 ( 0.000000000000000000, 0.03125000000040171338, 0.06250000000080342677, 0.1250000000016067148, 0.2500000000020394242, 0.5000000000017441604, 1.000000000000000000 ),
 .UNSPECIFIED. ) ;
#88841 = CARTESIAN_POINT ( 'NONE',  ( -17.55007709685750328, 1487.029497697219995, 194.9701149225189738 ) ) ;
#88843 = ADVANCED_FACE ( 'NONE', ( #81262 ), #4577, .F. ) ;
#88842 = CARTESIAN_POINT ( 'NONE',  ( -89.68991106499699129, 1383.770515819449884, 308.4149094695740132 ) ) ;
#88844 = CARTESIAN_POINT ( 'NONE',  ( -109.2165961150899989, 1384.279859431989962, 311.2110007195050230 ) ) ;
#88845 = CARTESIAN_POINT ( 'NONE',  ( 0.2440728571770119926, 1517.002586324550066, 201.4005528731310051 ) ) ;
#88847 = VERTEX_POINT ( 'NONE', #29765 ) ;
#88846 = CARTESIAN_POINT ( 'NONE',  ( 21.42336641369999839, 1508.384612396429930, 191.1046303810979907 ) ) ;
#88848 = FACE_OUTER_BOUND ( 'NONE', #56141, .T. ) ;
#88849 = CARTESIAN_POINT ( 'NONE',  ( 12.62550843869419914, 1512.222316757839963, 224.1785689195619966 ) ) ;
#88850 = EDGE_CURVE ( 'NONE', #24399, #12743, #51371, .T. ) ;
#88851 = ORIENTED_EDGE ( 'NONE', *, *, #79772, .F. ) ;
#88852 = VERTEX_POINT ( 'NONE', #84025 ) ;
#88853 = CARTESIAN_POINT ( 'NONE',  ( -7.799113859560000250, 1493.006535639589856, 207.9966435741489761 ) ) ;
#88854 = CARTESIAN_POINT ( 'NONE',  ( -110.0636336660000012, 1384.926148863469962, 296.9511392543589636 ) ) ;
#88855 = CARTESIAN_POINT ( 'NONE',  ( 13.35954871928184318, 1443.329911868641602, 169.3723227893304113 ) ) ;
#88857 = CARTESIAN_POINT ( 'NONE',  ( -9.545816650640000844, 1464.920850551829744, 240.4008508568979892 ) ) ;
#88856 = CARTESIAN_POINT ( 'NONE',  ( 30.16113214930838993, 1419.695379429048671, 269.4725258538827006 ) ) ;
#88858 = CARTESIAN_POINT ( 'NONE',  ( -19.82279908859999651, 1484.712476145529990, 190.4276546656979860 ) ) ;
#88859 = CARTESIAN_POINT ( 'NONE',  ( -11.92780736370000128, 1433.439050768640072, 150.0136606030979749 ) ) ;
#88860 = CARTESIAN_POINT ( 'NONE',  ( -2.174738361970000255, 1481.606857451690075, 229.5102325974989981 ) ) ;
#88861 = CARTESIAN_POINT ( 'NONE',  ( -19.42119839770000311, 1486.154863920830167, 189.7844104138979731 ) ) ;
#88862 = VECTOR ( 'NONE', #58643, 1000.000000000000114 ) ;
#88863 = LINE ( 'NONE', #45228, #20452 ) ;
#88864 = CARTESIAN_POINT ( 'NONE',  ( 4.992020700599999472, 1423.657950984729951, 185.2360043649980241 ) ) ;
#88865 = CARTESIAN_POINT ( 'NONE',  ( 1.771280571301239837, 1515.064792319160006, 213.4512947524970059 ) ) ;
#88866 = CARTESIAN_POINT ( 'NONE',  ( 8.251909802380000158, 1439.861449115349842, 153.7181668371979981 ) ) ;
#88867 = LINE ( 'NONE', #37364, #25130 ) ;
#88868 = CARTESIAN_POINT ( 'NONE',  ( -9.470856273389999913, 1451.339473522230037, 152.7638238112979820 ) ) ;
#88870 = ORIENTED_EDGE ( 'NONE', *, *, #29653, .T. ) ;
#88869 = CARTESIAN_POINT ( 'NONE',  ( -15.62861634609999761, 1418.244678181539939, 203.0179525210089935 ) ) ;
#88871 = ORIENTED_EDGE ( 'NONE', *, *, #102131, .T. ) ;
#88872 = CARTESIAN_POINT ( 'NONE',  ( -12.30879063490000114, 1505.268327336890025, 208.7613493058290146 ) ) ;
#88874 = CARTESIAN_POINT ( 'NONE',  ( -11.88584868791679838, 1482.380097381399992, 228.1376906553660149 ) ) ;
#88873 = B_SPLINE_CURVE_WITH_KNOTS ( 'NONE', 3,
 ( #43491, #1487, #93858, #33965 ),
 .UNSPECIFIED., .F., .F.,
 ( 4, 4 ),
 ( 0.000000000000000000, 0.0002960034161023854899 ),
 .UNSPECIFIED. ) ;
#88875 = CARTESIAN_POINT ( 'NONE',  ( -10.97762738589999998, 1473.214251705830065, 270.1116084939980055 ) ) ;
#88876 = DIRECTION ( 'NONE',  ( -5.980589973904019347E-17, 1.000000000000000000, -1.736889445713099699E-16 ) ) ;
#88877 = CARTESIAN_POINT ( 'NONE',  ( -113.4000000000000057, 1375.179104070690073, 316.4799049169590148 ) ) ;
#88878 = CARTESIAN_POINT ( 'NONE',  ( -15.39218706910000023, 1506.810797462329901, 224.8468255945980161 ) ) ;
#88879 = CARTESIAN_POINT ( 'NONE',  ( 0.3240298866389390020, 1450.984562072739891, 181.8401462983730141 ) ) ;
#88880 = CARTESIAN_POINT ( 'NONE',  ( -13.51720310719999851, 1421.523852283830138, 229.8336178099980032 ) ) ;
#88881 = VECTOR ( 'NONE', #74232, 999.9999999999998863 ) ;
#88882 = CARTESIAN_POINT ( 'NONE',  ( -8.494894331139999366, 1459.365948010190095, 213.8040489441289935 ) ) ;
#88883 = CARTESIAN_POINT ( 'NONE',  ( 10.69580974240662563, 1363.139536609160814, 210.6218459617030021 ) ) ;
#88884 = CARTESIAN_POINT ( 'NONE',  ( -45.29232520150449659, 1433.625543105270026, 267.6243001420129985 ) ) ;
#88885 = ORIENTED_EDGE ( 'NONE', *, *, #102328, .F. ) ;
#88886 = CARTESIAN_POINT ( 'NONE',  ( 0.000000000000000000, 1522.382868172863937, 240.9330574173806951 ) ) ;
#88887 = VERTEX_POINT ( 'NONE', #7867 ) ;
#88888 = CARTESIAN_POINT ( 'NONE',  ( -3.445201526505000000, 1516.743010792419909, 210.8372070624770060 ) ) ;
#88889 = DIRECTION ( 'NONE',  ( 0.3090169943749654369, -2.144236138472418401E-15, 0.9510565162951478690 ) ) ;
#88890 = CARTESIAN_POINT ( 'NONE',  ( -22.52609270419999987, 1509.699688878229836, 190.3921826525979952 ) ) ;
#88891 = CARTESIAN_POINT ( 'NONE',  ( -15.23280641220000220, 1410.405619594230075, 190.9016463256980103 ) ) ;
#88892 = CIRCLE ( 'NONE', #54940, 29.84605316883209625 ) ;
#88893 = CARTESIAN_POINT ( 'NONE',  ( 2.034091252963869945, 1495.719183412219991, 221.2929912278799804 ) ) ;
#88894 = VERTEX_POINT ( 'NONE', #15149 ) ;
#88895 = FACE_OUTER_BOUND ( 'NONE', #86964, .T. ) ;
#88896 = CARTESIAN_POINT ( 'NONE',  ( -7.717505791104999346, 1516.857914730730045, 201.4043401791270185 ) ) ;
#88897 = CARTESIAN_POINT ( 'NONE',  ( -3.206876023490000005, 1419.434649146130141, 184.2270935463979811 ) ) ;
#88898 = DIRECTION ( 'NONE',  ( -0.9125304618754029873, 0.000000000000000000, -0.4090087482554177756 ) ) ;
#88899 = ORIENTED_EDGE ( 'NONE', *, *, #8893, .T. ) ;
#88900 = CARTESIAN_POINT ( 'NONE',  ( -26.02511763151360213, 1416.147910639220072, 270.1077897879640091 ) ) ;
#88901 = CARTESIAN_POINT ( 'NONE',  ( -1.608351468689999786, 1426.598937817530214, 144.1938086916980239 ) ) ;
#88902 = LINE ( 'NONE', #106256, #85831 ) ;
#88904 = ORIENTED_EDGE ( 'NONE', *, *, #77703, .T. ) ;
#88903 = CARTESIAN_POINT ( 'NONE',  ( -8.646226660069116221, 1365.433969532401761, 210.6218459617142003 ) ) ;
#88905 = ORIENTED_EDGE ( 'NONE', *, *, #97268, .T. ) ;
#88906 = CARTESIAN_POINT ( 'NONE',  ( 45.42636855331534917, 1444.198313664763418, 268.9805725394130604 ) ) ;
#88907 = CARTESIAN_POINT ( 'NONE',  ( 8.748307446421703659, 1511.491070485854152, 203.4049457530220195 ) ) ;
#88908 = CARTESIAN_POINT ( 'NONE',  ( 19.04497961809999751, 1456.669328884790048, 205.4206990132790054 ) ) ;
#88909 = CARTESIAN_POINT ( 'NONE',  ( 2.407253779970412566, 1523.313115944345554, 175.0653106450178882 ) ) ;
#88910 = AXIS2_PLACEMENT_3D ( 'NONE', #53565, #36739, #96655 ) ;
#88911 = CARTESIAN_POINT ( 'NONE',  ( -17.40764085468179800, 1414.996442620800053, 207.5654756526599840 ) ) ;
#88912 = CARTESIAN_POINT ( 'NONE',  ( 2.689507531282340214, 1439.963205020849955, 157.5730311057610038 ) ) ;
#88913 = CARTESIAN_POINT ( 'NONE',  ( 10.54362614759770089, 1474.753171831259806, 269.4739217683639936 ) ) ;
#88914 = CARTESIAN_POINT ( 'NONE',  ( 11.46423597849999965, 1415.041103191730144, 222.5613496819979957 ) ) ;
#88915 = CARTESIAN_POINT ( 'NONE',  ( -17.36636230016033267, 1422.631182428599232, 226.5763293091231390 ) ) ;
#88916 = CARTESIAN_POINT ( 'NONE',  ( -2.880592967115000125, 1516.859514182039902, 206.2568738160869941 ) ) ;
#88917 = EDGE_LOOP ( 'NONE', ( #66893, #24803, #47928, #109985 ) ) ;
#88918 = FACE_OUTER_BOUND ( 'NONE', #94410, .T. ) ;
#88919 = CARTESIAN_POINT ( 'NONE',  ( -23.61303499308581166, 1447.799747876519405, 215.1558229191804514 ) ) ;
#88920 = VERTEX_POINT ( 'NONE', #50992 ) ;
#88921 = CARTESIAN_POINT ( 'NONE',  ( 10.59300109150884239, 1455.143630007434922, 226.2791905348894090 ) ) ;
#88922 = CARTESIAN_POINT ( 'NONE',  ( -28.17856943518795276, 1509.667335740066619, 211.1330165289786294 ) ) ;
#88923 = CARTESIAN_POINT ( 'NONE',  ( 1.925297170580940076, 1522.051704408389924, 230.6853930747409720 ) ) ;
#88924 = CARTESIAN_POINT ( 'NONE',  ( -9.117370426725258881, 1384.541028373849940, 199.9667117751619685 ) ) ;
#88925 = CARTESIAN_POINT ( 'NONE',  ( 19.74363812609999869, 1410.524512607730230, 196.8232449923980028 ) ) ;
#88926 = CARTESIAN_POINT ( 'NONE',  ( 28.46619500829999794, 1445.052233488290085, 168.7181723459979992 ) ) ;
#88927 = CARTESIAN_POINT ( 'NONE',  ( 16.64312535719999886, 1409.659826693630066, 225.8601930648979987 ) ) ;
#88928 = CARTESIAN_POINT ( 'NONE',  ( -14.07701606803241923, 1379.612174084935305, 211.7004875632037226 ) ) ;
#88929 = CARTESIAN_POINT ( 'NONE',  ( 20.85017764587675515, 1454.877224260557341, 222.3149521191053850 ) ) ;
#88930 = CIRCLE ( 'NONE', #90679, 1.999999999999999556 ) ;
#88931 = CARTESIAN_POINT ( 'NONE',  ( -1.906509838889290056E-08, 1508.551704408389924, 204.1347675157070114 ) ) ;
#88932 = CARTESIAN_POINT ( 'NONE',  ( 6.945490048805000427, 1516.932669162149978, 214.9002185338470099 ) ) ;
#88933 = DIRECTION ( 'NONE',  ( 0.000000000000000000, 6.123233995736769734E-17, 1.000000000000000000 ) ) ;
#88934 = VERTEX_POINT ( 'NONE', #597 ) ;
#88935 = CARTESIAN_POINT ( 'NONE',  ( -7.027952441359999192, 1482.449581481789892, 201.0380530320790058 ) ) ;
#88936 = FACE_OUTER_BOUND ( 'NONE', #37469, .T. ) ;
#88937 = CARTESIAN_POINT ( 'NONE',  ( 4.075310198389409777, 1517.051704406860154, 202.0559764476869873 ) ) ;
#88938 = CARTESIAN_POINT ( 'NONE',  ( -37.45632682353310372, 1449.248250845319944, 136.3260026918899825 ) ) ;
#88939 = CARTESIAN_POINT ( 'NONE',  ( 11.01785724859542626, 1425.018945203718204, 138.3717623160356709 ) ) ;
#88940 = CARTESIAN_POINT ( 'NONE',  ( 2.182839453575158295, 1417.483061668222035, 233.3517557601115300 ) ) ;
#88941 = CARTESIAN_POINT ( 'NONE',  ( 17.90144918474177160, 1423.842768551787003, 225.8231199409207477 ) ) ;
#88942 = CARTESIAN_POINT ( 'NONE',  ( 11.68841187039999951, 1433.169245300249941, 150.9165344040980017 ) ) ;
#88943 = CARTESIAN_POINT ( 'NONE',  ( -4.168267939633230057, 1474.036593221349904, 270.1339685919859903 ) ) ;
#88944 = CARTESIAN_POINT ( 'NONE',  ( -10.47157504770849989, 1461.831102136270147, 210.4833357475050093 ) ) ;
#88945 = CARTESIAN_POINT ( 'NONE',  ( -109.3532201929999985, 1385.076312201809969, 297.1413702938589836 ) ) ;
#88946 = CARTESIAN_POINT ( 'NONE',  ( 1.420259601960000229, 1466.712985171129958, 235.0376566307980113 ) ) ;
#88947 = ORIENTED_EDGE ( 'NONE', *, *, #48415, .T. ) ;
#88948 = DIRECTION ( 'NONE',  ( 0.000000000000000000, -1.000000000000000000, 0.000000000000000000 ) ) ;
#88949 = CARTESIAN_POINT ( 'NONE',  ( 10.51777314836719945, 1480.734379257120054, 208.3815665556330146 ) ) ;
#88950 = CIRCLE ( 'NONE', #33461, 9.341369339569999042 ) ;
#88951 = CARTESIAN_POINT ( 'NONE',  ( -19.41856793929088099, 1485.592250299008128, 189.9265828168643395 ) ) ;
#88952 = CARTESIAN_POINT ( 'NONE',  ( -1.399663831989999885, 1443.805352974990228, 199.9250768807590077 ) ) ;
#88953 = CARTESIAN_POINT ( 'NONE',  ( -11.74015320060000001, 1428.979986575930070, 144.1938086916980239 ) ) ;
#88954 = AXIS2_PLACEMENT_3D ( 'NONE', #93675, #34347, #42203 ) ;
#88955 = CARTESIAN_POINT ( 'NONE',  ( -16.81049281787982252, 1526.143142182167367, 235.5964692618745175 ) ) ;
#88956 = CARTESIAN_POINT ( 'NONE',  ( -10.95472753179999970, 1509.295607902330175, 236.2198715736980148 ) ) ;
#88957 = CARTESIAN_POINT ( 'NONE',  ( -23.95151507931580070, 1383.849269534789983, 222.8015749634270151 ) ) ;
#88958 = CARTESIAN_POINT ( 'NONE',  ( -21.59687146514269784, 1507.523380887320172, 209.4572544992919916 ) ) ;
#88959 = CARTESIAN_POINT ( 'NONE',  ( 2.499944437997340341, 1419.584213655310123, 133.9247507763970191 ) ) ;
#88961 =( BOUNDED_CURVE ( )  B_SPLINE_CURVE ( 3, ( #9612, #86879, #85772, #25293 ),
 .UNSPECIFIED., .F., .F. ) 
 B_SPLINE_CURVE_WITH_KNOTS ( ( 4, 4 ),
 ( 1.478867175770939957, 1.985375841758659998 ),
 .UNSPECIFIED. ) 
 CURVE ( )  GEOMETRIC_REPRESENTATION_ITEM ( )  RATIONAL_B_SPLINE_CURVE ( ( 1.000000000000000000, 0.9787347716977619072, 0.9787347716977619072, 1.000000000000000000 ) ) 
 REPRESENTATION_ITEM ( '' )  );
#88960 = CARTESIAN_POINT ( 'NONE',  ( -1966.823930461590180, 11221.53578756869865, -25.46789276350280318 ) ) ;
#88962 = CARTESIAN_POINT ( 'NONE',  ( 1.458694644860000000, 1465.700659552730031, 235.2691402379979877 ) ) ;
#88964 = ORIENTED_EDGE ( 'NONE', *, *, #48851, .T. ) ;
#88963 = CARTESIAN_POINT ( 'NONE',  ( 31.10385014139599136, 1525.795403383247276, 216.3488197230036860 ) ) ;
#88965 = CARTESIAN_POINT ( 'NONE',  ( -1.129710524660000104, 1450.979185682630032, 182.6858286092979995 ) ) ;
#88966 = CARTESIAN_POINT ( 'NONE',  ( -6.053292825790000720, 1379.821371071459907, 214.0283920821290167 ) ) ;
#88967 = CARTESIAN_POINT ( 'NONE',  ( -5.062212445509999270, 1474.342205042089972, 198.8731682765990172 ) ) ;
#88968 = ADVANCED_FACE ( 'NONE', ( #42034 ), #105586, .T. ) ;
#88970 = VERTEX_POINT ( 'NONE', #34726 ) ;
#88969 = FACE_OUTER_BOUND ( 'NONE', #5144, .T. ) ;
#88971 = CARTESIAN_POINT ( 'NONE',  ( -8.229004279106218789, 1439.448159900319979, 228.6152177230760003 ) ) ;
#88972 = ORIENTED_EDGE ( 'NONE', *, *, #72108, .T. ) ;
#88973 = CARTESIAN_POINT ( 'NONE',  ( -11.11381666019869918, 1389.577331926439911, 215.4847763224689743 ) ) ;
#88974 = DIRECTION ( 'NONE',  ( 0.9993902469226793039, -0.03489947646363077138, -0.001077449947926189004 ) ) ;
#88975 = CARTESIAN_POINT ( 'NONE',  ( 11.60004869885204570, 1426.273943615695998, 138.2686089212693332 ) ) ;
#88976 = CARTESIAN_POINT ( 'NONE',  ( 6.315236557301221687, 1506.394552972206839, 218.9623958905396819 ) ) ;
#88977 = CARTESIAN_POINT ( 'NONE',  ( -2.097032581780000182, 1432.708420430490150, 218.4264516295189935 ) ) ;
#88978 = CARTESIAN_POINT ( 'NONE',  ( 7.700010710769999989, 1490.081763956990017, 208.3600023555910070 ) ) ;
#88979 = CIRCLE ( 'NONE', #83620, 1.999999999999999556 ) ;
#88980 = CARTESIAN_POINT ( 'NONE',  ( 14.77784225791719841, 1409.429114010250032, 211.2770915593420114 ) ) ;
#88981 = CARTESIAN_POINT ( 'NONE',  ( -3.487592469735000478, 1508.551704408389924, 214.1089243866569802 ) ) ;
#88982 = CARTESIAN_POINT ( 'NONE',  ( -88.76030199668080911, 1385.188808422029979, 291.7738006920690168 ) ) ;
#88983 = CARTESIAN_POINT ( 'NONE',  ( -17.96086529829999989, 1440.788139876609876, 191.1125201911979730 ) ) ;
#88984 = CARTESIAN_POINT ( 'NONE',  ( -68.57300709150000273, 1379.748249346600005, 279.7358748726589965 ) ) ;
#88985 = CARTESIAN_POINT ( 'NONE',  ( 11.23938785293669795, 1490.970187199380234, 207.0635000114160107 ) ) ;
#88986 = ORIENTED_EDGE ( 'NONE', *, *, #43319, .F. ) ;
#88987 = ORIENTED_EDGE ( 'NONE', *, *, #7765, .T. ) ;
#88988 = CARTESIAN_POINT ( 'NONE',  ( -109.1645132478509908, 1384.901512804259937, 297.1326343494729940 ) ) ;
#88989 = CARTESIAN_POINT ( 'NONE',  ( 18.24033452539389799, 1459.341357182790034, 227.8698260022179909 ) ) ;
#88990 = CARTESIAN_POINT ( 'NONE',  ( -2.251423912408169858, 1495.949164212019923, 196.9898274163030010 ) ) ;
#88991 = CARTESIAN_POINT ( 'NONE',  ( 29.98468393967828050, 1462.259853740634071, 269.4706430128066472 ) ) ;
#88992 = CARTESIAN_POINT ( 'NONE',  ( -20.59032573514600273, 1507.551486734899981, 190.3983201303999806 ) ) ;
#88993 = CARTESIAN_POINT ( 'NONE',  ( 4.365782049980000856, 1396.065516855929900, 219.3093729220980208 ) ) ;
#88994 = FACE_OUTER_BOUND ( 'NONE', #1127, .T. ) ;
#88995 = DIRECTION ( 'NONE',  ( 0.9455185755993178454, 0.000000000000000000, -0.3255681544571539243 ) ) ;
#88996 = CARTESIAN_POINT ( 'NONE',  ( -9.934709065784959492, 1365.494406819940195, 210.6218459616991936 ) ) ;
#88997 = CARTESIAN_POINT ( 'NONE',  ( -26.59801442624275580, 1436.739763347805138, 136.7954695389641699 ) ) ;
#88998 = CARTESIAN_POINT ( 'NONE',  ( -19.16007793760780231, 1428.477562982570134, 208.5540069974889832 ) ) ;
#88999 = EDGE_CURVE ( 'NONE', #15749, #87844, #107429, .T. ) ;
#89000 = CARTESIAN_POINT ( 'NONE',  ( 5.770820141135000192, 1516.591755933730155, 207.4105347035570048 ) ) ;
#89001 = AXIS2_PLACEMENT_3D ( 'NONE', #51516, #578, #50431 ) ;
#89002 = CARTESIAN_POINT ( 'NONE',  ( 0.000000000000000000, 1518.913060387330006, 179.0139814193315999 ) ) ;
#89003 = CARTESIAN_POINT ( 'NONE',  ( 30.79916350760221277, 1526.104292489146474, 201.1259370313290731 ) ) ;
#89004 = CARTESIAN_POINT ( 'NONE',  ( 16.19087789078229989, 1409.478458302130093, 193.2334102746530107 ) ) ;
#89005 = DIRECTION ( 'NONE',  ( 0.000000000000000000, 1.000000000000000000, 0.000000000000000000 ) ) ;
#89006 = CARTESIAN_POINT ( 'NONE',  ( -10.48474110849999974, 1480.275079708390194, 208.2232256045050178 ) ) ;
#89007 = CARTESIAN_POINT ( 'NONE',  ( 41.58338113919019463, 1444.065857391419968, 136.1223126983269935 ) ) ;
#89008 = ORIENTED_EDGE ( 'NONE', *, *, #95837, .T. ) ;
#89009 = CARTESIAN_POINT ( 'NONE',  ( 33.60183515439999979, 1440.913060392849957, 248.0844435622979915 ) ) ;
#89010 = CARTESIAN_POINT ( 'NONE',  ( -25.81147510950000168, 1488.682669034729997, 202.5064507356880199 ) ) ;
#89012 = CARTESIAN_POINT ( 'NONE',  ( 13.35004134540000109, 1415.296882282229944, 197.1179729259980036 ) ) ;
#89011 = CARTESIAN_POINT ( 'NONE',  ( -11.08316036037830088, 1426.485585298449905, 96.72966585604500267 ) ) ;
#89013 = CARTESIAN_POINT ( 'NONE',  ( -17.14220118670536763, 1410.074716354810107, 270.0732288711442948 ) ) ;
#89014 = CARTESIAN_POINT ( 'NONE',  ( -6.248994202630000494, 1409.477339443830033, 259.9484415741980001 ) ) ;
#89015 = DIRECTION ( 'NONE',  ( -0.6736849260863841948, 0.000000000000000000, 0.7390186874254148774 ) ) ;
#89016 = CARTESIAN_POINT ( 'NONE',  ( 2.500574528909250027, 1448.942056006560051, 154.5733147652059927 ) ) ;
#89017 = CARTESIAN_POINT ( 'NONE',  ( -23.71385545433166797, 1410.153949831662885, 208.7056953457179418 ) ) ;
#89018 = ORIENTED_EDGE ( 'NONE', *, *, #96960, .F. ) ;
#89019 = CARTESIAN_POINT ( 'NONE',  ( 3.657048081452280108, 1396.576469495309993, 196.6488135896609890 ) ) ;
#89020 = CARTESIAN_POINT ( 'NONE',  ( 14.81823676263572587, 1514.585431681391583, 225.3567438282504440 ) ) ;
#89021 = B_SPLINE_CURVE_WITH_KNOTS ( 'NONE', 3,
 ( #87615, #106060, #29338, #70846 ),
 .UNSPECIFIED., .F., .F.,
 ( 4, 4 ),
 ( 0.000000000000000000, 0.3624990114314036171 ),
 .UNSPECIFIED. ) ;
#89022 = LINE ( 'NONE', #87952, #18552 ) ;
#89023 = ORIENTED_EDGE ( 'NONE', *, *, #64701, .F. ) ;
#89024 = ORIENTED_EDGE ( 'NONE', *, *, #42040, .T. ) ;
#89025 = CIRCLE ( 'NONE', #24584, 0.5001123349366123350 ) ;
#89026 = CARTESIAN_POINT ( 'NONE',  ( 9.707007897230489846, 1452.234270665119993, 209.8038064800559823 ) ) ;
#89027 = CARTESIAN_POINT ( 'NONE',  ( 5.485856304330000377, 1423.003856355439893, 194.7031335851989695 ) ) ;
#89028 = ORIENTED_EDGE ( 'NONE', *, *, #63312, .T. ) ;
#89029 = CARTESIAN_POINT ( 'NONE',  ( -1.077779315100000135, 1415.654178936130165, 185.0928310270980148 ) ) ;
#89030 = CARTESIAN_POINT ( 'NONE',  ( -5.824210366952714324, 1419.534194419528376, 194.8654209611248120 ) ) ;
#89031 = CIRCLE ( 'NONE', #81836, 1.999999999999999556 ) ;
#89032 = CARTESIAN_POINT ( 'NONE',  ( -0.3620056675250000189, 1489.066376473530227, 236.5422289001979834 ) ) ;
#89033 = CARTESIAN_POINT ( 'NONE',  ( 17.12202622828785792, 1526.104292489130330, 235.9427193670906320 ) ) ;
#89034 = ORIENTED_EDGE ( 'NONE', *, *, #56189, .F. ) ;
#89035 = EDGE_CURVE ( 'NONE', #92712, #43923, #109212, .T. ) ;
#89036 = ADVANCED_FACE ( 'NONE', ( #50450, #91876 ), #8970, .F. ) ;
#89037 = CARTESIAN_POINT ( 'NONE',  ( -12.13987205284939996, 1415.426207913209964, 221.7061766877399975 ) ) ;
#89038 = CARTESIAN_POINT ( 'NONE',  ( 14.57546012949999970, 1474.756325762929919, 224.5278850946980072 ) ) ;
#89039 = ORIENTED_EDGE ( 'NONE', *, *, #27652, .T. ) ;
#89040 = CARTESIAN_POINT ( 'NONE',  ( 2.286446325635000054, 1517.042661899400173, 204.4961520670869959 ) ) ;
#89041 = ORIENTED_EDGE ( 'NONE', *, *, #67878, .T. ) ;
#89043 = EDGE_CURVE ( 'NONE', #104774, #76367, #30545, .T. ) ;
#89042 = CARTESIAN_POINT ( 'NONE',  ( 11.85702737606739987, 1431.703556386109994, 149.9456834834640233 ) ) ;
#89044 = CARTESIAN_POINT ( 'NONE',  ( 12.70925652983267895, 1445.012977275617231, 186.3879696001495176 ) ) ;
#89045 = VERTEX_POINT ( 'NONE', #17342 ) ;
#89046 = ORIENTED_EDGE ( 'NONE', *, *, #99829, .T. ) ;
#89047 = FACE_OUTER_BOUND ( 'NONE', #22882, .T. ) ;
#89048 = EDGE_CURVE ( 'NONE', #29269, #39549, #12647, .T. ) ;
#89049 = CARTESIAN_POINT ( 'NONE',  ( -2.146051933368469999, 1508.551704408360138, 220.2827628139220053 ) ) ;
#89050 = CARTESIAN_POINT ( 'NONE',  ( 3.424621566958379937, 1498.316785755180035, 198.1282711917500023 ) ) ;
#89051 = EDGE_CURVE ( 'NONE', #82365, #100321, #626, .T. ) ;
#89052 = CARTESIAN_POINT ( 'NONE',  ( -7.941319541319999509, 1469.154588994090091, 217.1846401660390029 ) ) ;
#89053 = CARTESIAN_POINT ( 'NONE',  ( 26.27891900751420096, 1507.831017877699878, 209.0944339814940065 ) ) ;
#89054 = CARTESIAN_POINT ( 'NONE',  ( 11.16376535829999916, 1420.610325767149789, 198.7943618068990190 ) ) ;
#89055 = CARTESIAN_POINT ( 'NONE',  ( -13.72624666517843472, 1521.951704408389787, 195.8110037935180969 ) ) ;
#89056 = CARTESIAN_POINT ( 'NONE',  ( -5.445054425793269814, 1494.866999379700246, 198.0707246423999948 ) ) ;
#89057 = FACE_OUTER_BOUND ( 'NONE', #33112, .T. ) ;
#89058 = CARTESIAN_POINT ( 'NONE',  ( 0.03679684590394945165, 1409.773880882323510, 233.0990921512198213 ) ) ;
#89059 = EDGE_CURVE ( 'NONE', #107071, #70320, #68150, .T. ) ;
#89061 = CARTESIAN_POINT ( 'NONE',  ( 6.531167973260559201, 1517.151704408390060, 201.5366623270788295 ) ) ;
#89060 = CARTESIAN_POINT ( 'NONE',  ( -19.24236553089999902, 1505.018157644889925, 209.0733177765920345 ) ) ;
#89062 = CARTESIAN_POINT ( 'NONE',  ( -68.31098214250890521, 1379.747686652805669, 279.8373429272113526 ) ) ;
#89063 = CIRCLE ( 'NONE', #40786, 1.999999999999999556 ) ;
#89064 = CARTESIAN_POINT ( 'NONE',  ( -9.851036438101349546, 1439.921995732989899, 207.3463547441290302 ) ) ;
#89065 = CARTESIAN_POINT ( 'NONE',  ( -6.277682590474999991, 1511.927085655870087, 201.2403123398769935 ) ) ;
#89066 = EDGE_LOOP ( 'NONE', ( #89764, #58743 ) ) ;
#89067 = CARTESIAN_POINT ( 'NONE',  ( 39.48812356990000438, 1431.587789823920048, 268.3665355202980436 ) ) ;
#89068 = DIRECTION ( 'NONE',  ( 0.000000000000000000, 1.000000000000000000, 0.000000000000000000 ) ) ;
#89069 = CARTESIAN_POINT ( 'NONE',  ( -87.61701047141821164, 1384.975105123960020, 307.8438091251570086 ) ) ;
#89070 = CARTESIAN_POINT ( 'NONE',  ( 35.95604727100876374, 1451.436200009825143, 134.6958367465652202 ) ) ;
#89071 = CARTESIAN_POINT ( 'NONE',  ( 5.237925579300000578, 1505.876516098390084, 219.6658948394990034 ) ) ;
#89072 = CARTESIAN_POINT ( 'NONE',  ( 45.63713829939310074, 1440.913067348179993, 268.9747433721050243 ) ) ;
#89073 = EDGE_CURVE ( 'NONE', #58638, #35907, #33067, .T. ) ;
#89075 = ORIENTED_EDGE ( 'NONE', *, *, #97262, .F. ) ;
#89074 = CARTESIAN_POINT ( 'NONE',  ( -8.107801870790000365, 1463.844143246390104, 201.5100198155989801 ) ) ;
#89076 = CARTESIAN_POINT ( 'NONE',  ( 8.598096571001718758, 1427.995879741943554, 137.0999999980979567 ) ) ;
#89077 = CARTESIAN_POINT ( 'NONE',  ( -2.511980889886960000, 1439.367824232180055, 157.7248736099130042 ) ) ;
#89078 = DIRECTION ( 'NONE',  ( -0.9125304618753961039, 0.000000000000000000, 0.4090087482554332632 ) ) ;
#89079 = CARTESIAN_POINT ( 'NONE',  ( -1.337785777300729784, 1429.784825555620046, 199.8250566260579717 ) ) ;
#89080 = CARTESIAN_POINT ( 'NONE',  ( 12.28497684303499859, 1512.406775501100128, 225.6610851038670091 ) ) ;
#89081 = CYLINDRICAL_SURFACE ( 'NONE', #49183, 0.4999999999999449329 ) ;
#89082 = EDGE_CURVE ( 'NONE', #26024, #3898, #16630, .T. ) ;
#89083 = CARTESIAN_POINT ( 'NONE',  ( 27.67618890949159649, 1509.957365838989972, 222.7461888534850232 ) ) ;
#89084 = CARTESIAN_POINT ( 'NONE',  ( 8.289359074433349406, 1461.164466581640227, 203.9471711042499749 ) ) ;
#89085 = CARTESIAN_POINT ( 'NONE',  ( -8.805428988939999257, 1497.713060387329961, 229.3821491682979854 ) ) ;
#89086 = EDGE_CURVE ( 'NONE', #96069, #101117, #73496, .T. ) ;
#89087 = CARTESIAN_POINT ( 'NONE',  ( 12.07722019555130544, 1511.957228877181251, 223.9708055708832148 ) ) ;
#89088 = CARTESIAN_POINT ( 'NONE',  ( 10.01013843233299916, 1469.369181467840008, 209.9819040969830155 ) ) ;
#89089 = CARTESIAN_POINT ( 'NONE',  ( -20.38673671613199545, 1525.878013734321939, 236.1208636900185525 ) ) ;
#89090 = CARTESIAN_POINT ( 'NONE',  ( -5.788436372295000076, 1517.116049120239950, 206.8334885244969712 ) ) ;
#89091 = CARTESIAN_POINT ( 'NONE',  ( 43.82551825799999534, 1429.987201715729952, 268.8187383044979697 ) ) ;
#89092 = CARTESIAN_POINT ( 'NONE',  ( -18.29824102079999903, 1410.475830671229915, 224.2242554351979891 ) ) ;
#89093 = CARTESIAN_POINT ( 'NONE',  ( 19.22696748599999950, 1435.168248072100141, 144.6563286545979850 ) ) ;
#89094 = EDGE_CURVE ( 'NONE', #31217, #108726, #84171, .T. ) ;
#89095 = CARTESIAN_POINT ( 'NONE',  ( 20.12413710170000414, 1488.587669296430022, 190.7085797787979971 ) ) ;
#89096 = CARTESIAN_POINT ( 'NONE',  ( 5.359753019955250330, 1422.468040155149993, 146.8791528727659852 ) ) ;
#89097 = CARTESIAN_POINT ( 'NONE',  ( -4.970712357689999195, 1475.638404632529955, 266.9514863814980004 ) ) ;
#89098 = CARTESIAN_POINT ( 'NONE',  ( -14.24733479436660133, 1416.667683397399969, 203.2028330777899896 ) ) ;
#89099 = CARTESIAN_POINT ( 'NONE',  ( -36.85982855397319469, 1436.428218451429984, 135.9089977690080104 ) ) ;
#89100 = CARTESIAN_POINT ( 'NONE',  ( 0.2124338303341239964, 1455.982566712989865, 183.1254455901450058 ) ) ;
#89101 = CARTESIAN_POINT ( 'NONE',  ( -11.97297630299070015, 1408.007688502349993, 215.8652761565809897 ) ) ;
#89102 = CARTESIAN_POINT ( 'NONE',  ( 0.7950258152958181723, 1426.814114633998997, 137.0999999982234385 ) ) ;
#89103 = CARTESIAN_POINT ( 'NONE',  ( -4.138993620949999119, 1515.551749212189861, 208.7474755485019955 ) ) ;
#89104 = CARTESIAN_POINT ( 'NONE',  ( -7.573230445929720389, 1384.232072112190053, 219.0440869779680213 ) ) ;
#89105 = CARTESIAN_POINT ( 'NONE',  ( 11.87582791709999874, 1433.006487889580058, 146.9202945366980089 ) ) ;
#89106 = CARTESIAN_POINT ( 'NONE',  ( -36.51516363092789419, 1436.208852636029860, 134.0999999969979797 ) ) ;
#89107 = CARTESIAN_POINT ( 'NONE',  ( 10.29822466560000116, 1441.809080340180117, 186.9379677964980146 ) ) ;
#89108 = ORIENTED_EDGE ( 'NONE', *, *, #48120, .T. ) ;
#89109 = CARTESIAN_POINT ( 'NONE',  ( -7.114141310732409629, 1427.484008838899626, 137.0999999980979567 ) ) ;
#89110 = CARTESIAN_POINT ( 'NONE',  ( -7.000838161960609263, 1409.157535043050075, 222.3551060745959944 ) ) ;
#89111 = CARTESIAN_POINT ( 'NONE',  ( -11.00301364519999936, 1492.094801868890045, 210.0154387525699917 ) ) ;
#89112 = CARTESIAN_POINT ( 'NONE',  ( -2.478156609180000025, 1439.614611698830231, 157.7689743226979999 ) ) ;
#89113 = CARTESIAN_POINT ( 'NONE',  ( 14.65718418945929891, 1509.165728398129886, 233.2531174127820179 ) ) ;
#89114 = CARTESIAN_POINT ( 'NONE',  ( -31.73415138219999676, 1466.561829745230170, 267.4236068477979984 ) ) ;
#89115 = CARTESIAN_POINT ( 'NONE',  ( -29.95988583836330221, 1525.317349363550193, 196.6841769033301546 ) ) ;
#89116 = CIRCLE ( 'NONE', #21145, 1.000000000000004441 ) ;
#89117 = CARTESIAN_POINT ( 'NONE',  ( -16.66936639838851875, 1523.456924617339610, 237.7608804993614910 ) ) ;
#89118 = CARTESIAN_POINT ( 'NONE',  ( -25.59999408250000030, 1509.583809833630085, 220.6387430072979896 ) ) ;
#89119 = CARTESIAN_POINT ( 'NONE',  ( -89.61547716558578713, 1384.619918949700150, 308.5733451897559689 ) ) ;
#89120 = CARTESIAN_POINT ( 'NONE',  ( -43.09652149413830102, 1384.997786203090072, 216.0876167203250020 ) ) ;
#89121 = CARTESIAN_POINT ( 'NONE',  ( -12.18503172777290011, 1490.802926859980062, 207.7326696222349938 ) ) ;
#89122 = CARTESIAN_POINT ( 'NONE',  ( -3.548015302541859928, 1508.551704408389924, 204.3702150974099823 ) ) ;
#89123 = AXIS2_PLACEMENT_3D ( 'NONE', #73152, #107296, #67524 ) ;
#89124 = CARTESIAN_POINT ( 'NONE',  ( -29.61157949331689920, 1509.955833110559979, 208.5825572949630100 ) ) ;
#89125 = EDGE_CURVE ( 'NONE', #76827, #91492, #62730, .T. ) ;
#89126 = CARTESIAN_POINT ( 'NONE',  ( 2.273033093151324735, 1525.821544997590536, 177.3097463090895189 ) ) ;
#89128 = ORIENTED_EDGE ( 'NONE', *, *, #26874, .T. ) ;
#89127 = DIRECTION ( 'NONE',  ( 0.000000000000000000, 1.000000000000000000, 0.000000000000000000 ) ) ;
#89129 = DIRECTION ( 'NONE',  ( -1.000000000000000000, 0.000000000000000000, 0.000000000000000000 ) ) ;
#89130 = AXIS2_PLACEMENT_3D ( 'NONE', #24726, #25836, #60036 ) ;
#89131 = CARTESIAN_POINT ( 'NONE',  ( 1.455000209906389896, 1507.073729425429974, 236.7651043255590082 ) ) ;
#89132 = EDGE_CURVE ( 'NONE', #94873, #11858, #80737, .T. ) ;
#89133 = CARTESIAN_POINT ( 'NONE',  ( -4.584247552609999943, 1495.956452401090019, 219.3622640912990107 ) ) ;
#89134 = CARTESIAN_POINT ( 'NONE',  ( 3.487592430751666583, 1508.603735221695615, 204.3914617688909345 ) ) ;
#89135 = FACE_OUTER_BOUND ( 'NONE', #36547, .T. ) ;
#89136 = CARTESIAN_POINT ( 'NONE',  ( 22.63852601520000007, 1409.703615135929795, 209.5818420717589845 ) ) ;
#89137 = CARTESIAN_POINT ( 'NONE',  ( -107.0758886263459999, 1391.913060387289988, 306.8605669363920470 ) ) ;
#89138 = CARTESIAN_POINT ( 'NONE',  ( -16.49825404190000100, 1466.404193669789947, 220.8530316403990241 ) ) ;
#89139 = CARTESIAN_POINT ( 'NONE',  ( -5.362414201681900749, 1424.198757875690035, 150.5191954795400022 ) ) ;
#89141 = CARTESIAN_POINT ( 'NONE',  ( -12.98386958510000078, 1379.322232870260223, 207.9132534626290010 ) ) ;
#89140 = CARTESIAN_POINT ( 'NONE',  ( -11.77874533540000002, 1433.007533761370041, 150.8097953740980017 ) ) ;
#89142 = CARTESIAN_POINT ( 'NONE',  ( 25.68368308515399789, 1449.916366644430127, 208.3382958551559909 ) ) ;
#89143 = CARTESIAN_POINT ( 'NONE',  ( -101.1419410402999972, 1375.179104070690073, 304.2218459572590064 ) ) ;
#89144 = CARTESIAN_POINT ( 'NONE',  ( -11.79257197010000091, 1490.424928053189888, 209.6468059298940148 ) ) ;
#89145 = CARTESIAN_POINT ( 'NONE',  ( 17.00810803830026074, 1492.794519359084234, 195.6196894796988488 ) ) ;
#89146 = CARTESIAN_POINT ( 'NONE',  ( 8.988338641399998608, 1366.896325247149889, 210.6218459616991936 ) ) ;
#89147 = EDGE_CURVE ( 'NONE', #64955, #37540, #10901, .T. ) ;
#89148 = CARTESIAN_POINT ( 'NONE',  ( 6.937338745574999521, 1516.706638732659940, 204.5037262658370025 ) ) ;
#89149 = CARTESIAN_POINT ( 'NONE',  ( 13.37450925738970042, 1507.663501308599962, 233.0614823370259785 ) ) ;
#89150 = CARTESIAN_POINT ( 'NONE',  ( -18.71617348083620058, 1485.537080198780131, 189.3638635336550067 ) ) ;
#89151 = CARTESIAN_POINT ( 'NONE',  ( -9.200421138165051360, 1422.937291722789951, 210.7384568321920142 ) ) ;
#89152 = CARTESIAN_POINT ( 'NONE',  ( -10.64684140641754517, 1422.356867849525770, 210.6398257839229871 ) ) ;
#89154 = ORIENTED_EDGE ( 'NONE', *, *, #49368, .T. ) ;
#89153 = CARTESIAN_POINT ( 'NONE',  ( -67.36707325840760063, 1379.746113040620003, 278.5175139230419745 ) ) ;
#89155 = ORIENTED_EDGE ( 'NONE', *, *, #69154, .T. ) ;
#89156 = CARTESIAN_POINT ( 'NONE',  ( 29.17336346449999951, 1509.870405656429966, 210.3367036282079994 ) ) ;
#89157 = ORIENTED_EDGE ( 'NONE', *, *, #32405, .F. ) ;
#89158 = CARTESIAN_POINT ( 'NONE',  ( -105.1701064949999989, 1379.114530330549997, 304.0350749897590390 ) ) ;
#89159 = CARTESIAN_POINT ( 'NONE',  ( -109.9851113750000025, 1384.920600747060007, 311.4561369192589950 ) ) ;
#89161 = CARTESIAN_POINT ( 'NONE',  ( 1.716050170100000161, 1509.007692890629869, 179.5167852785979790 ) ) ;
#89160 = CARTESIAN_POINT ( 'NONE',  ( 1.496858517070000172, 1428.056401037730211, 101.8807690336980016 ) ) ;
#89162 = CARTESIAN_POINT ( 'NONE',  ( -0.1798688738929999642, 1417.261861208530263, 235.9169760632979944 ) ) ;
#89163 = ADVANCED_FACE ( 'NONE', ( #2270 ), #52649, .T. ) ;
#89164 = CARTESIAN_POINT ( 'NONE',  ( -24.10240618318239925, 1452.071386932320138, 136.4706332069859798 ) ) ;
#89165 = CARTESIAN_POINT ( 'NONE',  ( -0.06658362883100119034, 1468.466425048889960, 219.2800796028990078 ) ) ;
#89166 = CARTESIAN_POINT ( 'NONE',  ( 8.774939133739998454, 1409.219488014130093, 228.7704650873980086 ) ) ;
#89167 = CARTESIAN_POINT ( 'NONE',  ( 8.099523513883839954, 1483.863015130160193, 216.2634084175389830 ) ) ;
#89168 = FILL_AREA_STYLE_COLOUR ( '', #91520 ) ;
#89169 = CARTESIAN_POINT ( 'NONE',  ( 41.50828902763819173, 1442.131284356850074, 134.0999999980909934 ) ) ;
#89170 = CARTESIAN_POINT ( 'NONE',  ( 14.98723526979999932, 1429.231381954089784, 197.7821723486989924 ) ) ;
#89171 = ORIENTED_EDGE ( 'NONE', *, *, #32476, .T. ) ;
#89172 = CARTESIAN_POINT ( 'NONE',  ( 0.5708672984259970384, 1460.784242392889837, 230.4191149236990270 ) ) ;
#89173 = EDGE_CURVE ( 'NONE', #83952, #106220, #66309, .T. ) ;
#89174 = CARTESIAN_POINT ( 'NONE',  ( 5.312679136500000787, 1493.059131431590231, 218.8466398904690209 ) ) ;
#89175 = VERTEX_POINT ( 'NONE', #78393 ) ;
#89176 = ORIENTED_EDGE ( 'NONE', *, *, #63832, .T. ) ;
#89177 = ORIENTED_EDGE ( 'NONE', *, *, #10464, .T. ) ;
#89178 = CARTESIAN_POINT ( 'NONE',  ( -6.166911790614999944, 1513.656171171930055, 216.7076464020170192 ) ) ;
#89179 = CARTESIAN_POINT ( 'NONE',  ( 16.01537988097770437, 1514.821748395666646, 194.0245274743359118 ) ) ;
#89180 = CARTESIAN_POINT ( 'NONE',  ( 8.173996330113771691, 1451.383476035822923, 152.8928977840655818 ) ) ;
#89181 = CARTESIAN_POINT ( 'NONE',  ( -8.581307173289999923, 1384.896522470129867, 218.6696871042690020 ) ) ;
#89182 = CARTESIAN_POINT ( 'NONE',  ( -17.48410805928437384, 1448.286856264058997, 218.1600271269404629 ) ) ;
#89183 = CARTESIAN_POINT ( 'NONE',  ( -67.60155324206988325, 1379.745550781364045, 277.6215540139086784 ) ) ;
#89184 = FACE_OUTER_BOUND ( 'NONE', #89264, .T. ) ;
#89185 = EDGE_CURVE ( 'NONE', #16564, #52504, #16210, .T. ) ;
#89186 = CARTESIAN_POINT ( 'NONE',  ( -4.427981762014999489, 1510.423579818969984, 201.5728291684769999 ) ) ;
#89187 = CARTESIAN_POINT ( 'NONE',  ( 6.036596006619999955, 1415.425582719929707, 192.3914609787979941 ) ) ;
#89188 = CARTESIAN_POINT ( 'NONE',  ( -57.84584034184130275, 1384.660072621870086, 239.4800334103370005 ) ) ;
#89189 = ORIENTED_EDGE ( 'NONE', *, *, #93360, .F. ) ;
#89190 = CARTESIAN_POINT ( 'NONE',  ( -2.882326017515000061, 1516.969638403840008, 207.4201161117570109 ) ) ;
#89191 = ORIENTED_EDGE ( 'NONE', *, *, #64561, .F. ) ;
#89192 = CARTESIAN_POINT ( 'NONE',  ( 25.26674768904949886, 1440.913060387330006, 239.9653784531180065 ) ) ;
#89193 = CARTESIAN_POINT ( 'NONE',  ( 3.448830483803564828, 1511.187213306747708, 243.0842028158767789 ) ) ;
#89194 = ADVANCED_FACE ( 'NONE', ( #36384 ), #87683, .T. ) ;
#89195 = EDGE_LOOP ( 'NONE', ( #48080, #35257, #10297, #11129 ) ) ;
#89196 = CARTESIAN_POINT ( 'NONE',  ( -0.3328315121010000377, 1452.976685501030261, 183.2631392977980056 ) ) ;
#89197 = CARTESIAN_POINT ( 'NONE',  ( -16.48988658240000049, 1410.421086167129943, 191.6528615609980193 ) ) ;
#89198 = CARTESIAN_POINT ( 'NONE',  ( -6.954065720117950100, 1517.551704408389924, 183.5505540514350002 ) ) ;
#89200 = CARTESIAN_POINT ( 'NONE',  ( 20.12203338850000023, 1473.683243806589871, 208.1564127194919820 ) ) ;
#89199 = CARTESIAN_POINT ( 'NONE',  ( -24.90364451589999817, 1441.171407319239961, 210.4346984424180107 ) ) ;
#89201 = CARTESIAN_POINT ( 'NONE',  ( -5.652324135034829666, 1434.623555776060130, 216.9489395581130111 ) ) ;
#89202 = CARTESIAN_POINT ( 'NONE',  ( -5.567226385628840646, 1511.487400615810202, 200.5687758574929944 ) ) ;
#89203 = CARTESIAN_POINT ( 'NONE',  ( 0.8854628104720000392, 1405.995467260429905, 266.9608410729979937 ) ) ;
#89204 = DIRECTION ( 'NONE',  ( 0.000000000000000000, 0.000000000000000000, 1.000000000000000000 ) ) ;
#89206 = CARTESIAN_POINT ( 'NONE',  ( -11.60004869885203860, 1425.163648261535172, 137.9639116715027853 ) ) ;
#89205 = CARTESIAN_POINT ( 'NONE',  ( 15.69844654775839921, 1410.486775117663228, 191.5641288874454631 ) ) ;
#89207 = CIRCLE ( 'NONE', #48040, 20.98341875040010507 ) ;
#89208 = CARTESIAN_POINT ( 'NONE',  ( 4.617490466775000080, 1516.685667699390024, 216.4467608883869900 ) ) ;
#89209 = AXIS2_PLACEMENT_3D ( 'NONE', #99888, #82567, #23186 ) ;
#89210 = ADVANCED_FACE ( 'NONE', ( #2811 ), #88603, .F. ) ;
#89211 = CARTESIAN_POINT ( 'NONE',  ( 7.105427357599999217E-15, 1425.413060387329779, 188.2701767054980166 ) ) ;
#89212 = CARTESIAN_POINT ( 'NONE',  ( 5.972112752736340013, 1511.562335007999991, 217.9146188711339960 ) ) ;
#89213 = VECTOR ( 'NONE', #58237, 1000.000000000000000 ) ;
#89214 = CARTESIAN_POINT ( 'NONE',  ( 2.448631922079805179, 1516.534705479064542, 216.8308881910905370 ) ) ;
#89215 = CARTESIAN_POINT ( 'NONE',  ( -3.446329813785000251, 1516.812046502680005, 212.0014881234369852 ) ) ;
#89216 = CARTESIAN_POINT ( 'NONE',  ( -22.09833645820000214, 1506.806593688730118, 209.0739427216549871 ) ) ;
#89217 = DIRECTION ( 'NONE',  ( 0.07283688039883663701, -0.01177923247455932992, 0.9972743045602228129 ) ) ;
#89219 = ORIENTED_EDGE ( 'NONE', *, *, #32389, .F. ) ;
#89218 = CARTESIAN_POINT ( 'NONE',  ( -5.010230764180000129, 1425.855359435129913, 208.5321074068529867 ) ) ;
#89220 = CARTESIAN_POINT ( 'NONE',  ( -0.5679639878839999323, 1416.568813547830132, 227.7576290933980090 ) ) ;
#89221 = CARTESIAN_POINT ( 'NONE',  ( 29.87497052560000199, 1440.913060386509869, 238.0574391280980251 ) ) ;
#89222 = CARTESIAN_POINT ( 'NONE',  ( 29.71163624023450467, 1526.333389947941441, 217.1029916164621909 ) ) ;
#89223 = CARTESIAN_POINT ( 'NONE',  ( -14.94752639080000023, 1415.823955448430070, 205.5818586423190197 ) ) ;
#89224 = CARTESIAN_POINT ( 'NONE',  ( 1.980002924110000118, 1414.522533370030033, 232.1992291241980126 ) ) ;
#89225 = CARTESIAN_POINT ( 'NONE',  ( 16.75454338844407687, 1526.382868173645875, 183.6974516591938880 ) ) ;
#89227 = CARTESIAN_POINT ( 'NONE',  ( -6.144376325710156905, 1512.187213306747481, 247.6867189913431844 ) ) ;
#89226 = CARTESIAN_POINT ( 'NONE',  ( -24.11883138550000183, 1457.436797524329904, 215.1402808420379813 ) ) ;
#89228 = CARTESIAN_POINT ( 'NONE',  ( -2.845522529430000169, 1486.018762278030181, 182.0897997094980099 ) ) ;
#89229 = CARTESIAN_POINT ( 'NONE',  ( -106.2303729149999896, 1379.004472240850191, 307.4679664830589445 ) ) ;
#89230 = CIRCLE ( 'NONE', #98173, 30.00000000000000000 ) ;
#89231 = ORIENTED_EDGE ( 'NONE', *, *, #36766, .T. ) ;
#89232 = CARTESIAN_POINT ( 'NONE',  ( -0.7564342523539989704, 1516.783665406140017, 204.5091745923169810 ) ) ;
#89233 = CARTESIAN_POINT ( 'NONE',  ( 2.112228378390000216, 1405.752148843630039, 267.8521524492979893 ) ) ;
#89234 = EDGE_CURVE ( 'NONE', #55990, #59685, #17684, .T. ) ;
#89235 = CARTESIAN_POINT ( 'NONE',  ( 1.082449427709999856, 1515.225850744089939, 213.4470767797189978 ) ) ;
#89236 = CARTESIAN_POINT ( 'NONE',  ( 30.92651641011650199, 1464.557726000649836, 270.3478336023849806 ) ) ;
#89237 = B_SPLINE_CURVE_WITH_KNOTS ( 'NONE', 3,
 ( #88196, #55714, #5845, #6387, #39437, #75264, #73612, #64666, #74711, #92044, #98232, #90372, #32139, #64111, #73048, #23171, #13650, #15316, #66324, #47840, #99872, #49509, #40535, #107741, #81973, #98783, #83634, #5281, #22046, #108842, #23725, #13107, #100442, #31025, #109413, #6930, #21501, #56243, #65207, #65755, #99320, #57371, #108292, #57910, #82551, #41087, #22594, #48963, #89835, #56797, #47290, #74161, #83094, #90934, #14221, #107189, #48407, #39985, #91498, #81413, #14777 ),
 .UNSPECIFIED., .F., .F.,
 ( 4, 2, 2, 2, 2, 2, 1, 2, 2, 2, 1, 2, 2, 2, 2, 1, 1, 1, 2, 2, 2, 2, 2, 1, 2, 2, 2, 1, 2, 2, 2, 2, 2, 4 ),
 ( 0.000000000000000000, 0.06249999999394668937, 0.09374999999092048508, 0.1093749999892469627, 0.1249999999875734263, 0.1874999999799758787, 0.2187499999763425629, 0.2343749999743528212, 0.2499999999723631072, 0.3124999999644023640, 0.3437499999604230472, 0.3593749999585725274, 0.3749999999567220632, 0.4374999999493155989, 0.4687499999456131716, 0.4843749999436541276, 0.4921874999427758302, 0.4960937499424362129, 0.4980468749422645725, 0.4999999999420928765, 0.5624999999485508217, 0.5937499999517797944, 0.6093749999533922823, 0.6171874999542571461, 0.6210937499547435348, 0.6249999999552299235, 0.6874999999624902269, 0.7187499999661217664, 0.7343749999679390905, 0.7499999999697564146, 0.8124999999772816173, 0.8437499999811264306, 0.8749999999849713550, 1.000000000000000000 ),
 .UNSPECIFIED. ) ;
#89238 = CARTESIAN_POINT ( 'NONE',  ( -4.623067421070000016, 1470.601194648889987, 189.6761541078989808 ) ) ;
#89239 = CARTESIAN_POINT ( 'NONE',  ( -0.04641543425164652847, 1517.051704408389924, 230.3502074417858978 ) ) ;
#89240 = CARTESIAN_POINT ( 'NONE',  ( -6.725822268156810502, 1439.879530295837412, 203.5093415176590383 ) ) ;
#89241 = CARTESIAN_POINT ( 'NONE',  ( -3.703897191089999819, 1458.190786016390120, 219.1639864912989992 ) ) ;
#89242 = CARTESIAN_POINT ( 'NONE',  ( 9.923338817417189262, 1442.404032688280040, 184.8562081593751429 ) ) ;
#89243 = CARTESIAN_POINT ( 'NONE',  ( 1.962873812034300114, 1450.341737227420026, 154.5188752846379714 ) ) ;
#89244 = CARTESIAN_POINT ( 'NONE',  ( -13.81908124539619998, 1415.258594623649969, 220.7407950635269742 ) ) ;
#89245 = CARTESIAN_POINT ( 'NONE',  ( 18.35614473481600584, 1445.354571529838722, 191.3429017698720145 ) ) ;
#89246 = EDGE_LOOP ( 'NONE', ( #10639, #91377, #94057, #25261, #101626, #45895, #109157, #73212, #48225, #44979, #68381, #46817, #104060, #95374 ) ) ;
#89247 = CARTESIAN_POINT ( 'NONE',  ( -37.18025140759999658, 1432.092748029830091, 265.6112249940979950 ) ) ;
#89249 = CARTESIAN_POINT ( 'NONE',  ( 8.483440609833868606, 1468.250586555449900, 202.2169064785170178 ) ) ;
#89248 =( REPRESENTATION_RELATIONSHIP ('NONE','NONE', #14372, #60858 ) REPRESENTATION_RELATIONSHIP_WITH_TRANSFORMATION ( #101950 )SHAPE_REPRESENTATION_RELATIONSHIP( ) );
#89250 = CARTESIAN_POINT ( 'NONE',  ( -0.8899015605279998464, 1476.102961708030080, 267.8536994237979911 ) ) ;
#89251 = CARTESIAN_POINT ( 'NONE',  ( -12.98226713004480004, 1414.913060387349788, 219.9156686614909972 ) ) ;
#89252 = CARTESIAN_POINT ( 'NONE',  ( -17.18726318579999912, 1440.321463842890125, 217.4344804300990290 ) ) ;
#89253 = CARTESIAN_POINT ( 'NONE',  ( 16.19492570339999915, 1409.478599654730033, 224.8086529783979870 ) ) ;
#89254 = CARTESIAN_POINT ( 'NONE',  ( -35.02326960185389737, 1384.808974036340032, 234.2283971188210216 ) ) ;
#89255 = AXIS2_PLACEMENT_3D ( 'NONE', #67786, #25190, #76170 ) ;
#89256 = B_SPLINE_SURFACE_WITH_KNOTS ( 'NONE', 5, 5, ( 
 ( #102145, #83699, #67481, #32202, #7549, #68580 ),
 ( #33289, #60179, #50124, #50660, #76974, #34407 ),
 ( #92105, #9216, #85912, #41153, #110560, #59621 ),
 ( #281, #43375, #8090, #102684, #110013, #15382 ),
 ( #77523, #25426, #93732, #17011, #66384, #100503 ),
 ( #49571, #75328, #109470, #58519, #88691, #60745 ),
 ( #35510, #10305, #54011, #79193, #53443, #19233 ),
 ( #45600, #18143, #52340, #87588, #46153, #43918 ),
 ( #103822, #71371, #3050, #86461, #61853, #37175 ),
 ( #10877, #27667, #79742, #61307, #94867, #78625 ),
 ( #1367, #78065, #11970, #36077, #823, #95426 ),
 ( #62974, #104930, #19806, #70818, #105484, #34953 ),
 ( #28774, #45048, #69703, #104371, #9752, #2499 ),
 ( #95972, #88142, #36618, #97087, #44479, #28215 ),
 ( #27121, #18687, #62404, #96532, #11430, #52885 ) ),
 .UNSPECIFIED., .F., .F., .F.,
 ( 6, 3, 3, 3, 6 ),
 ( 6, 6 ),
 ( 44.15568540390000152, 56.49823163619999633, 69.80263562410000588, 81.33849626609999461, 85.77622357600000669 ),
 ( 0.000000000000000000, 2.000000000000000000 ),
 .UNSPECIFIED. ) ;
#89257 = CARTESIAN_POINT ( 'NONE',  ( 12.03449227190490056, 1491.353386486839781, 206.6667661091970274 ) ) ;
#89258 = CARTESIAN_POINT ( 'NONE',  ( -10.67819692480000171, 1482.848997777490240, 204.9256918032390047 ) ) ;
#89259 = CARTESIAN_POINT ( 'NONE',  ( 7.951441301218317825, 1511.804171812503228, 205.9133947108762186 ) ) ;
#89260 = CARTESIAN_POINT ( 'NONE',  ( -11.07268104156529986, 1396.299726929629969, 209.2078313262790061 ) ) ;
#89261 = CARTESIAN_POINT ( 'NONE',  ( -15.67023493909999665, 1420.566432160730074, 227.0266865602980033 ) ) ;
#89262 = VECTOR ( 'NONE', #69579, 1000.000000000000341 ) ;
#89263 = CARTESIAN_POINT ( 'NONE',  ( 19.56650236141162935, 1455.497407615608608, 225.8439199820629142 ) ) ;
#89264 = EDGE_LOOP ( 'NONE', ( #33231, #55325, #12868, #100131, #53577 ) ) ;
#89265 = CARTESIAN_POINT ( 'NONE',  ( -2.991447891192810182, 1436.484000074640107, 227.3801637149809949 ) ) ;
#89266 = CARTESIAN_POINT ( 'NONE',  ( 1.137831829869999867, 1408.952794351630018, 231.4765879240979984 ) ) ;
#89267 = CARTESIAN_POINT ( 'NONE',  ( -6.358358198699995967, 1484.270642863229568, 183.8946942232976483 ) ) ;
#89269 = CARTESIAN_POINT ( 'NONE',  ( -12.30406198576499932, 1511.972232048389969, 194.0466686572669914 ) ) ;
#89268 = CARTESIAN_POINT ( 'NONE',  ( 11.01694515279999997, 1425.660268107129923, 115.7225178154979943 ) ) ;
#89270 = CARTESIAN_POINT ( 'NONE',  ( 5399.190776299724348, 2837.541834147233658, -8134.792049093189235 ) ) ;
#89271 = CARTESIAN_POINT ( 'NONE',  ( -13.51610093808349866, 1443.913060387330006, 205.0760988357349959 ) ) ;
#89272 = EDGE_CURVE ( 'NONE', #42124, #49270, #88873, .T. ) ;
#89273 = CARTESIAN_POINT ( 'NONE',  ( -7.717505791104999346, 1516.857914730730045, 201.4043401791270185 ) ) ;
#89274 = CARTESIAN_POINT ( 'NONE',  ( 8.060566621569998702, 1428.063481974589877, 213.0156338157989921 ) ) ;
#89275 = CARTESIAN_POINT ( 'NONE',  ( -2.439001525050000119, 1430.488531030629929, 150.2249694046979869 ) ) ;
#89276 = CARTESIAN_POINT ( 'NONE',  ( 4.287256129599999355, 1508.836301919430298, 180.7363543702979882 ) ) ;
#89277 = CARTESIAN_POINT ( 'NONE',  ( 7.594504641424999924, 1512.160709093490141, 206.7360737480470050 ) ) ;
#89278 = CARTESIAN_POINT ( 'NONE',  ( -86.98686869178300185, 1379.577998201610171, 300.8196123566030451 ) ) ;
#89279 = AXIS2_PLACEMENT_3D ( 'NONE', #105870, #57129, #13981 ) ;
#89280 = CARTESIAN_POINT ( 'NONE',  ( 8.988338641399998608, 1366.896325247149889, 207.6218459616989946 ) ) ;
#89282 = ORIENTED_EDGE ( 'NONE', *, *, #17992, .F. ) ;
#89281 = CARTESIAN_POINT ( 'NONE',  ( -14.02644022332259865, 1379.579259008480221, 211.8354623865689916 ) ) ;
#89283 = VERTEX_POINT ( 'NONE', #27779 ) ;
#89284 = CARTESIAN_POINT ( 'NONE',  ( 7.848979634317430509, 1522.051704408389924, 215.9448598632019980 ) ) ;
#89285 = CONICAL_SURFACE ( 'NONE', #41003, 0.9999999999999930056, 0.7853981633970000820 ) ;
#89286 = CARTESIAN_POINT ( 'NONE',  ( 0.4654153100249480146, 1490.951906556200129, 236.6680651313590147 ) ) ;
#89287 = CARTESIAN_POINT ( 'NONE',  ( 15.28420222189999933, 1497.713060387329961, 225.7900586086979899 ) ) ;
#89288 = CARTESIAN_POINT ( 'NONE',  ( -7.618992712005001167, 1511.297452611760036, 212.2897357890169872 ) ) ;
#89289 =( BOUNDED_CURVE ( )  B_SPLINE_CURVE ( 3, ( #50500, #75153, #33662, #101967 ),
 .UNSPECIFIED., .F., .F. ) 
 B_SPLINE_CURVE_WITH_KNOTS ( ( 4, 4 ),
 ( 4.834686371853470277, 5.479655915121550258 ),
 .UNSPECIFIED. ) 
 CURVE ( )  GEOMETRIC_REPRESENTATION_ITEM ( )  RATIONAL_B_SPLINE_CURVE ( ( 1.000000000000000000, 0.9656339083259537492, 0.9656339083259537492, 1.000000000000000000 ) ) 
 REPRESENTATION_ITEM ( '' )  );
#89291 = CARTESIAN_POINT ( 'NONE',  ( -1.360610103134009874, 1413.432550495719852, 185.4726596582680145 ) ) ;
#89290 = CARTESIAN_POINT ( 'NONE',  ( -7.544733521269999521, 1384.899971913130003, 219.0877090843589770 ) ) ;
#89292 = ADVANCED_FACE ( 'NONE', ( #9871 ), #71650, .F. ) ;
#89293 = CARTESIAN_POINT ( 'NONE',  ( 2.982689009480000486, 1410.303126873030124, 185.7169846868979732 ) ) ;
#89294 = CARTESIAN_POINT ( 'NONE',  ( -1.935216760905889899, 1464.825770518590161, 198.7112181189110061 ) ) ;
#89295 = CARTESIAN_POINT ( 'NONE',  ( 8.272555700608019129E-16, 1374.413060387289988, 209.1218459616989946 ) ) ;
#89296 = SURFACE_STYLE_FILL_AREA ( #46220 ) ;
#89297 = CARTESIAN_POINT ( 'NONE',  ( 40.45017409928269814, 1439.698990137739884, 136.1552142357990078 ) ) ;
#89298 = CARTESIAN_POINT ( 'NONE',  ( 7.675121520048339363, 1396.181081537549971, 217.0737066862720042 ) ) ;
#89299 = CARTESIAN_POINT ( 'NONE',  ( -19.25375188179999952, 1464.258769156330118, 194.1747703853979772 ) ) ;
#89300 = CARTESIAN_POINT ( 'NONE',  ( 11.74760992340000065, 1430.665155385330081, 150.5937701333980101 ) ) ;
#89301 = CARTESIAN_POINT ( 'NONE',  ( 41.66194051640000140, 1443.744879019749987, 136.1277437682980178 ) ) ;
#89302 = ORIENTED_EDGE ( 'NONE', *, *, #23308, .T. ) ;
#89303 = CARTESIAN_POINT ( 'NONE',  ( 3.957454374529999708, 1424.240901629729933, 184.6710418408979990 ) ) ;
#89304 = CARTESIAN_POINT ( 'NONE',  ( 12.16634552240000033, 1441.485087603719876, 188.2667282966980338 ) ) ;
#89305 = B_SPLINE_CURVE_WITH_KNOTS ( 'NONE', 3,
 ( #79435, #27921, #79978, #35770, #69953, #3297, #36312 ),
 .UNSPECIFIED., .F., .F.,
 ( 4, 3, 4 ),
 ( -157.7844419369999969, -101.5360198676929997, -30.93609007920730392 ),
 .UNSPECIFIED. ) ;
#89306 = VERTEX_POINT ( 'NONE', #47343 ) ;
#89307 = ORIENTED_EDGE ( 'NONE', *, *, #97268, .F. ) ;
#89308 = CARTESIAN_POINT ( 'NONE',  ( -17.65750842319999947, 1478.114914029529928, 228.8033778946980021 ) ) ;
#89309 = CARTESIAN_POINT ( 'NONE',  ( 9.671060821790000261, 1366.060403940050037, 207.6218459616989946 ) ) ;
#89310 = CIRCLE ( 'NONE', #92887, 2.000000000000001776 ) ;
#89311 = CARTESIAN_POINT ( 'NONE',  ( -6.937965698444999774, 1516.732530461250008, 214.1275461716370216 ) ) ;
#89312 = DIRECTION ( 'NONE',  ( -0.9786619618251657382, 0.000000000000000000, 0.2054769195713179730 ) ) ;
#89313 = EDGE_LOOP ( 'NONE', ( #14806, #74590, #47083, #32978, #67439 ) ) ;
#89314 = DIRECTION ( 'NONE',  ( 0.9455185755993178454, 0.000000000000000000, -0.3255681544571539243 ) ) ;
#89315 = CARTESIAN_POINT ( 'NONE',  ( -42.70366651140000158, 1379.809904802510118, 226.7036006354589972 ) ) ;
#89316 = CARTESIAN_POINT ( 'NONE',  ( 5.281924519060000378, 1415.931391677329884, 226.2877012803980108 ) ) ;
#89317 = CARTESIAN_POINT ( 'NONE',  ( 1.704794803334999997, 1517.096587378560116, 204.4952540647470016 ) ) ;
#89318 = AXIS2_PLACEMENT_3D ( 'NONE', #67962, #6917, #15840 ) ;
#89319 = CARTESIAN_POINT ( 'NONE',  ( -37.61786880320000392, 1440.913060387330006, 264.6588860065979816 ) ) ;
#89320 = EDGE_CURVE ( 'NONE', #12979, #40553, #80944, .T. ) ;
#89321 = CARTESIAN_POINT ( 'NONE',  ( 11.86794117217350397, 1433.007090821210568, 150.2053110587648632 ) ) ;
#89322 = CARTESIAN_POINT ( 'NONE',  ( -10.07203899970000016, 1409.765688315129864, 229.3746300812979939 ) ) ;
#89323 = EDGE_CURVE ( 'NONE', #73846, #32838, #46272, .T. ) ;
#89325 = ORIENTED_EDGE ( 'NONE', *, *, #92098, .F. ) ;
#89324 = CARTESIAN_POINT ( 'NONE',  ( -12.54268436849999979, 1408.913060387329779, 195.2008187059980173 ) ) ;
#89326 = DIRECTION ( 'NONE',  ( -9.341989762165448955E-47, 1.000000000000000000, -1.836970198721029688E-16 ) ) ;
#89327 = CARTESIAN_POINT ( 'NONE',  ( -25.24317812581459819, 1440.913060497079869, 217.5666783990430133 ) ) ;
#89328 = CARTESIAN_POINT ( 'NONE',  ( 20.64229337434479561, 1507.778434579259965, 226.7718724856480037 ) ) ;
#89329 = CARTESIAN_POINT ( 'NONE',  ( 12.96503937710000010, 1476.856299447390029, 225.6431713718990011 ) ) ;
#89330 = ADVANCED_FACE ( 'NONE', ( #74220 ), #89500, .T. ) ;
#89331 = CARTESIAN_POINT ( 'NONE',  ( 44.43452778323990060, 1436.360229837989891, 270.0922544047889460 ) ) ;
#89332 = CARTESIAN_POINT ( 'NONE',  ( -0.7356989727169980231, 1517.020847257979995, 212.5827121409169820 ) ) ;
#89333 = CARTESIAN_POINT ( 'NONE',  ( -67.90588950680000835, 1379.745915699690158, 278.2978613680589888 ) ) ;
#89334 = EDGE_CURVE ( 'NONE', #77692, #76715, #95415, .T. ) ;
#89335 = CARTESIAN_POINT ( 'NONE',  ( 23.33118560439999811, 1410.121805423329988, 208.1130523111279729 ) ) ;
#89336 = CARTESIAN_POINT ( 'NONE',  ( 0.009105150452084580931, 1508.374673153829917, 237.8724040003439768 ) ) ;
#89337 = CARTESIAN_POINT ( 'NONE',  ( 15.62837127357619771, 1427.648990501440039, 199.9598782853679779 ) ) ;
#89338 = CARTESIAN_POINT ( 'NONE',  ( -7.711493580499960032, 1516.628317670949855, 210.2679642827060036 ) ) ;
#89339 = CARTESIAN_POINT ( 'NONE',  ( -0.7468175536419978666, 1517.006509894990131, 209.1289748073840258 ) ) ;
#89340 = CARTESIAN_POINT ( 'NONE',  ( 4.172120233436539927, 1421.397866124950042, 185.0689737346249899 ) ) ;
#89341 = CARTESIAN_POINT ( 'NONE',  ( -1.884384940320000146, 1417.914943765129919, 233.1634843046979881 ) ) ;
#89342 = CARTESIAN_POINT ( 'NONE',  ( -109.9987472809999929, 1384.808520183549945, 311.2744866012590137 ) ) ;
#89343 = VERTEX_POINT ( 'NONE', #65264 ) ;
#89344 = CARTESIAN_POINT ( 'NONE',  ( -22.65830243868510152, 1385.265625594450057, 222.2095871976100057 ) ) ;
#89345 = AXIS2_PLACEMENT_3D ( 'NONE', #69457, #88440, #104130 ) ;
#89346 = CARTESIAN_POINT ( 'NONE',  ( -2.847681058950000121, 1430.845634743689970, 201.2564363298089916 ) ) ;
#89347 = PRODUCT_DEFINITION_SHAPE ( 'NONE', 'NONE',  #110833 ) ;
#89348 = CARTESIAN_POINT ( 'NONE',  ( 19.59880151960000205, 1507.802454151830034, 188.8055342685979952 ) ) ;
#89349 = AXIS2_PLACEMENT_3D ( 'NONE', #95747, #71699, #44257 ) ;
#89350 = CARTESIAN_POINT ( 'NONE',  ( -24.90171366722389834, 1441.078953672730222, 210.4323502101370025 ) ) ;
#89351 = CARTESIAN_POINT ( 'NONE',  ( 12.26530152830000020, 1421.362759829509969, 204.2608483305789946 ) ) ;
#89352 = CARTESIAN_POINT ( 'NONE',  ( 0.4110931836658809901, 1452.974865402240084, 183.2795641384469718 ) ) ;
#89354 = CARTESIAN_POINT ( 'NONE',  ( -16.70830179842720042, 1417.149226859160080, 207.3570905742490140 ) ) ;
#89353 = CARTESIAN_POINT ( 'NONE',  ( -7.716252091104999877, 1516.810037859429940, 216.0641906620670056 ) ) ;
#89355 = CARTESIAN_POINT ( 'NONE',  ( 18.64442764509999861, 1507.939506224430033, 188.5219863284980022 ) ) ;
#89356 = CARTESIAN_POINT ( 'NONE',  ( -11.44665353847253186, 1425.798163151176823, 139.1345268192609126 ) ) ;
#89357 = VERTEX_POINT ( 'NONE', #56852 ) ;
#89358 = CARTESIAN_POINT ( 'NONE',  ( -6.555393155154999540, 1516.809497469189864, 201.7937966518470034 ) ) ;
#89359 = EDGE_CURVE ( 'NONE', #54701, #40948, #83497, .T. ) ;
#89360 = CARTESIAN_POINT ( 'NONE',  ( 10.28987036248729936, 1480.775536434839751, 206.8081037193859970 ) ) ;
#89361 = ORIENTED_EDGE ( 'NONE', *, *, #69020, .F. ) ;
#89362 = AXIS2_PLACEMENT_3D ( 'NONE', #85922, #104380, #79201 ) ;
#89363 = CARTESIAN_POINT ( 'NONE',  ( 11.60004869885203327, 1426.765776710964019, 134.3812685280135497 ) ) ;
#89364 = CARTESIAN_POINT ( 'NONE',  ( 9.940067125116463842, 1435.763642648871837, 152.5323839883900803 ) ) ;
#89365 = ADVANCED_FACE ( 'NONE', ( #82601 ), #50112, .T. ) ;
#89366 = CARTESIAN_POINT ( 'NONE',  ( 7.948444925817987006, 1423.758263538081110, 195.8503688939058804 ) ) ;
#89367 = UNCERTAINTY_MEASURE_WITH_UNIT (LENGTH_MEASURE( 1.000000000000000082E-05 ), #19752, 'distance_accuracy_value', 'NONE');
#89368 = CARTESIAN_POINT ( 'NONE',  ( 1.329590663860000133, 1443.548274132990173, 217.9512969677389833 ) ) ;
#89369 = CARTESIAN_POINT ( 'NONE',  ( -26.95412021097830291, 1509.373492805739943, 201.3014358241730122 ) ) ;
#89370 = FACE_OUTER_BOUND ( 'NONE', #108045, .T. ) ;
#89371 = CARTESIAN_POINT ( 'NONE',  ( -19.24890086970000169, 1426.049025734429961, 226.0195547209980305 ) ) ;
#89372 = CARTESIAN_POINT ( 'NONE',  ( -21.13920444840000101, 1435.664861300689836, 143.7512800368980095 ) ) ;
#89373 = CARTESIAN_POINT ( 'NONE',  ( -2.834860085976320221, 1464.859481028689970, 198.4842492681709984 ) ) ;
#89374 = CARTESIAN_POINT ( 'NONE',  ( 16.27871131059999854, 1509.481525512630014, 185.4630867003979802 ) ) ;
#89376 = CARTESIAN_POINT ( 'NONE',  ( -18.71783619763316509, 1437.581472098226641, 211.6929844148049824 ) ) ;
#89375 = CARTESIAN_POINT ( 'NONE',  ( 3.535327672168380175, 1487.160996015089950, 197.6951163816430039 ) ) ;
#89377 = CARTESIAN_POINT ( 'NONE',  ( -0.2682795917991919743, 1457.891717849350016, 229.2666142623699841 ) ) ;
#89378 = EDGE_LOOP ( 'NONE', ( #78776, #82620, #50491, #2026, #87391, #83660 ) ) ;
#89379 = CARTESIAN_POINT ( 'NONE',  ( -4.487249792034999629, 1509.038615934239942, 209.1727295022979831 ) ) ;
#89380 = CARTESIAN_POINT ( 'NONE',  ( -0.3621993323151809774, 1416.825784014559986, 191.0664209890499876 ) ) ;
#89381 = CARTESIAN_POINT ( 'NONE',  ( -8.301987938657498844, 1522.051704408389924, 185.0111222839169898 ) ) ;
#89382 = CARTESIAN_POINT ( 'NONE',  ( -17.22845748920260434, 1525.848198008145346, 236.4819726785932517 ) ) ;
#89383 = CARTESIAN_POINT ( 'NONE',  ( -2.170628039509999940, 1485.611815934889819, 197.4219877966989998 ) ) ;
#89384 = CONICAL_SURFACE ( 'NONE', #67907, 8.000000000000003553, 0.02617993877989872875 ) ;
#89385 = CARTESIAN_POINT ( 'NONE',  ( -18.56428495200000128, 1507.623776005530090, 229.7144034790980243 ) ) ;
#89386 = CARTESIAN_POINT ( 'NONE',  ( -2.664527636416262890, 1524.964230758899930, 241.7075690384371569 ) ) ;
#89387 = CARTESIAN_POINT ( 'NONE',  ( 21.20437582439999957, 1519.913060387329779, 218.3247824702980040 ) ) ;
#89388 = B_SPLINE_SURFACE_WITH_KNOTS ( 'NONE', 5, 1, ( 
 ( #47205, #46125 ),
 ( #37147, #105457 ),
 ( #81332, #72960 ),
 ( #80255, #107097 ),
 ( #71899, #30386 ),
 ( #57280, #84091 ) ),
 .UNSPECIFIED., .F., .F., .F.,
 ( 6, 6 ),
 ( 2, 2 ),
 ( 0.000000000000000000, 4.001056960039999666 ),
 ( 0.000000000000000000, 14.00000000000000000 ),
 .UNSPECIFIED. ) ;
#89389 = CARTESIAN_POINT ( 'NONE',  ( -16.81223226430000039, 1414.913060387329779, 207.5743821216680089 ) ) ;
#89390 = CARTESIAN_POINT ( 'NONE',  ( -3.487592469735000478, 1508.551704408389924, 214.1089243866569802 ) ) ;
#89391 = ADVANCED_BREP_SHAPE_REPRESENTATION ( '', ( #46279, #21632 ), #46788 ) ;
#89392 = CARTESIAN_POINT ( 'NONE',  ( -9.838233766173130945, 1462.268829427310038, 227.9668122194469788 ) ) ;
#89393 = CARTESIAN_POINT ( 'NONE',  ( -14.94996665966239924, 1415.677402202029953, 207.1999397929429847 ) ) ;
#89394 = CARTESIAN_POINT ( 'NONE',  ( -109.2564495476770077, 1383.425552342079982, 311.0677364371869658 ) ) ;
#89395 = CARTESIAN_POINT ( 'NONE',  ( 4.506137960680000276, 1429.623679839590068, 216.5655692257590204 ) ) ;
#89397 = ORIENTED_EDGE ( 'NONE', *, *, #60037, .F. ) ;
#89396 = CARTESIAN_POINT ( 'NONE',  ( 20.99191170940000362, 1509.583341178129785, 188.7493971674979889 ) ) ;
#89398 = AXIS2_PLACEMENT_3D ( 'NONE', #27444, #28556, #88467 ) ;
#89399 = FACE_OUTER_BOUND ( 'NONE', #90958, .T. ) ;
#89400 = CARTESIAN_POINT ( 'NONE',  ( 13.13649027217820020, 1512.464953430860078, 224.3787356123430072 ) ) ;
#89401 = ORIENTED_EDGE ( 'NONE', *, *, #526, .F. ) ;
#89402 = ORIENTED_EDGE ( 'NONE', *, *, #79152, .T. ) ;
#89403 = CARTESIAN_POINT ( 'NONE',  ( 12.25335341949999979, 1440.953202899389908, 188.4028591661979704 ) ) ;
#89404 = CARTESIAN_POINT ( 'NONE',  ( 14.12038737319999804, 1509.406339941330089, 234.8413163218980060 ) ) ;
#89405 = CARTESIAN_POINT ( 'NONE',  ( 12.88090278901364094, 1442.881791335779553, 169.4390353358178345 ) ) ;
#89407 = CARTESIAN_POINT ( 'NONE',  ( -34.21460436289999762, 1445.299194188719866, 250.0133502388980276 ) ) ;
#89406 = CARTESIAN_POINT ( 'NONE',  ( 29.35424698433324053, 1419.108688181071784, 269.4640726278769307 ) ) ;
#89408 = CARTESIAN_POINT ( 'NONE',  ( -19.79895059749999930, 1487.981277986430086, 190.0341339962980101 ) ) ;
#89409 = CARTESIAN_POINT ( 'NONE',  ( -11.77426720859999953, 1433.514918800020041, 150.7945381811979928 ) ) ;
#89410 = CARTESIAN_POINT ( 'NONE',  ( 28.08606285309999961, 1509.893847314130198, 201.5170686698379825 ) ) ;
#89411 = CARTESIAN_POINT ( 'NONE',  ( -19.13600947890000015, 1486.262565671930133, 189.4467765145979854 ) ) ;
#89412 = DIRECTION ( 'NONE',  ( -1.836970198721024757E-16, -1.000000000000000000, -1.001483571081361959E-32 ) ) ;
#89413 = CARTESIAN_POINT ( 'NONE',  ( -26.64345414829999825, 1440.570068888169999, 137.3587798196979861 ) ) ;
#89414 = CARTESIAN_POINT ( 'NONE',  ( -0.1187972037638400091, 1515.157712620099801, 213.4488615487820198 ) ) ;
#89415 = FACE_OUTER_BOUND ( 'NONE', #73285, .T. ) ;
#89416 = CARTESIAN_POINT ( 'NONE',  ( -10.41014360099929981, 1479.888900791299875, 214.5375557550950134 ) ) ;
#89417 = CARTESIAN_POINT ( 'NONE',  ( 31.97190655716449115, 1524.330813522192102, 201.5540712235606975 ) ) ;
#89419 = VERTEX_POINT ( 'NONE', #82029 ) ;
#89418 = CARTESIAN_POINT ( 'NONE',  ( 3.622743996232769967E-09, 1410.219912027380133, 258.0694156936299919 ) ) ;
#89420 = ORIENTED_EDGE ( 'NONE', *, *, #57002, .F. ) ;
#89421 = DIRECTION ( 'NONE',  ( -0.000000000000000000, -1.000000000000000000, -0.000000000000000000 ) ) ;
#89422 = CARTESIAN_POINT ( 'NONE',  ( -21.55607067240000063, 1488.682141303889921, 202.2062732307990132 ) ) ;
#89423 = CARTESIAN_POINT ( 'NONE',  ( -20.84494148259999946, 1470.316654825529895, 270.2130226670980164 ) ) ;
#89424 = CARTESIAN_POINT ( 'NONE',  ( 7.634170062339999063, 1421.957731401030060, 195.7691812542990135 ) ) ;
#89425 = CARTESIAN_POINT ( 'NONE',  ( -105.7573910491803844, 1371.894749952187794, 317.1057287443589985 ) ) ;
#89426 = FACE_OUTER_BOUND ( 'NONE', #83672, .T. ) ;
#89427 = AXIS2_PLACEMENT_3D ( 'NONE', #75273, #109420, #66876 ) ;
#89428 = CARTESIAN_POINT ( 'NONE',  ( 0.2060742663968820054, 1452.528028601769847, 183.2209051729230112 ) ) ;
#89429 = CARTESIAN_POINT ( 'NONE',  ( -14.09400383010000013, 1421.906236174930200, 228.7093513157980169 ) ) ;
#89430 = CARTESIAN_POINT ( 'NONE',  ( 10.73506988043325627, 1424.972993549859893, 139.1354236083641922 ) ) ;
#89431 =( BOUNDED_CURVE ( )  B_SPLINE_CURVE ( 3, ( #14915, #105833, #20684, #11757 ),
 .UNSPECIFIED., .F., .T. ) 
 B_SPLINE_CURVE_WITH_KNOTS ( ( 4, 4 ),
 ( 0.000000000000000000, 0.7048113239778114325 ),
 .UNSPECIFIED. ) 
 CURVE ( )  GEOMETRIC_REPRESENTATION_ITEM ( )  RATIONAL_B_SPLINE_CURVE ( ( 1.000000000000000000, 0.9590300661663084814, 0.9590300661663084814, 1.000000000000000000 ) ) 
 REPRESENTATION_ITEM ( '' )  );
#89432 = CARTESIAN_POINT ( 'NONE',  ( -3.586339042944182598, 1515.071394417498368, 205.0391425136844248 ) ) ;
#89433 = CARTESIAN_POINT ( 'NONE',  ( 10.14339872067701975, 1362.384246550940361, 210.6218459617030021 ) ) ;
#89434 = CARTESIAN_POINT ( 'NONE',  ( -45.62535461455620123, 1435.567858674460012, 268.2222749696159667 ) ) ;
#89435 = TOROIDAL_SURFACE ( 'NONE', #96631, 5.868098490439999537, 1.000000000000000000 ) ;
#89436 = VERTEX_POINT ( 'NONE', #41694 ) ;
#89437 = CARTESIAN_POINT ( 'NONE',  ( -3.531632230717580256, 1490.204869628420056, 181.6974446958380156 ) ) ;
#89438 = VERTEX_POINT ( 'NONE', #31080 ) ;
#89439 = EDGE_LOOP ( 'NONE', ( #83151, #15495, #56490 ) ) ;
#89440 = CARTESIAN_POINT ( 'NONE',  ( 7.726331925474999807, 1517.194972660189933, 211.4133602680070112 ) ) ;
#89441 = CARTESIAN_POINT ( 'NONE',  ( -10.93363683719999813, 1471.692480041690033, 205.6467075678189929 ) ) ;
#89442 = FACE_OUTER_BOUND ( 'NONE', #54898, .T. ) ;
#89443 = CARTESIAN_POINT ( 'NONE',  ( -15.84954036500000107, 1425.421969000529998, 190.5298818713980040 ) ) ;
#89444 = VECTOR ( 'NONE', #46457, 1000.000000000000114 ) ;
#89445 = CARTESIAN_POINT ( 'NONE',  ( 4.406802116531240543, 1421.289453786690501, 144.1378412804505160 ) ) ;
#89446 = ORIENTED_EDGE ( 'NONE', *, *, #100468, .F. ) ;
#89447 = CARTESIAN_POINT ( 'NONE',  ( -2.873329398885000163, 1516.572193931679976, 201.7997408644770019 ) ) ;
#89448 = ADVANCED_FACE ( 'NONE', ( #47893 ), #54647, .T. ) ;
#89449 = CARTESIAN_POINT ( 'NONE',  ( 7.800297031879999565, 1471.072109769290137, 215.6814025974289848 ) ) ;
#89450 = CARTESIAN_POINT ( 'NONE',  ( 0.8087773895360982346, 1508.989140809515220, 238.8276268623044132 ) ) ;
#89451 = VERTEX_POINT ( 'NONE', #103813 ) ;
#89452 = CARTESIAN_POINT ( 'NONE',  ( -13.46173026269689998, 1409.689012232490086, 270.3660067276319978 ) ) ;
#89453 = CARTESIAN_POINT ( 'NONE',  ( -33.13365747560000329, 1435.654560788539811, 135.0902693358980287 ) ) ;
#89454 = CARTESIAN_POINT ( 'NONE',  ( 2.903721707529999602E-11, 1395.913060387330006, 198.1220674040980043 ) ) ;
#89456 = ORIENTED_EDGE ( 'NONE', *, *, #77742, .T. ) ;
#89455 = CARTESIAN_POINT ( 'NONE',  ( -9.936738324562218949, 1364.340818343083811, 210.6218459616987957 ) ) ;
#89457 = ORIENTED_EDGE ( 'NONE', *, *, #39389, .T. ) ;
#89458 = CARTESIAN_POINT ( 'NONE',  ( 43.59041716596218663, 1451.056131081360263, 269.0321477434157487 ) ) ;
#89459 = CARTESIAN_POINT ( 'NONE',  ( 1.836900179243859954, 1466.949332984869898, 220.0337271301659996 ) ) ;
#89460 = CARTESIAN_POINT ( 'NONE',  ( 19.33955305990000184, 1457.046069667190068, 207.2605506525090107 ) ) ;
#89461 = VECTOR ( 'NONE', #39526, 1000.000000000000000 ) ;
#89462 = CARTESIAN_POINT ( 'NONE',  ( -0.9471777936590000113, 1485.704136142530160, 181.8966647610979805 ) ) ;
#89463 = CARTESIAN_POINT ( 'NONE',  ( -18.38499229356419917, 1415.595619977600109, 207.5688028031409829 ) ) ;
#89464 = CARTESIAN_POINT ( 'NONE',  ( 10.13545575494789830, 1453.511789163979984, 212.2748783515349942 ) ) ;
#89465 = EDGE_CURVE ( 'NONE', #90041, #13675, #14386, .T. ) ;
#89466 = CARTESIAN_POINT ( 'NONE',  ( -0.0001241292207142050271, 1476.050175603799744, 268.4837846581640406 ) ) ;
#89467 = CARTESIAN_POINT ( 'NONE',  ( 12.45642902069999991, 1416.822690122629865, 223.4763059356979795 ) ) ;
#89468 = CARTESIAN_POINT ( 'NONE',  ( 7.669726159795000164, 1510.984078637139874, 204.3009007237270112 ) ) ;
#89469 = CARTESIAN_POINT ( 'NONE',  ( 2.864326087304999824, 1516.826109302209943, 206.6287721023469999 ) ) ;
#89470 = ORIENTED_EDGE ( 'NONE', *, *, #106519, .F. ) ;
#89471 = CARTESIAN_POINT ( 'NONE',  ( -40.71747595459120106, 1438.773003512900004, 135.6928028942980120 ) ) ;
#89472 = CARTESIAN_POINT ( 'NONE',  ( -23.89217091865537768, 1446.185953660134601, 213.4188154793815784 ) ) ;
#89473 = VERTEX_POINT ( 'NONE', #69128 ) ;
#89475 = CIRCLE ( 'NONE', #62745, 33.13701971169416538 ) ;
#89474 = CARTESIAN_POINT ( 'NONE',  ( 1.577711128016545006, 1457.769755330347834, 228.8717772423867700 ) ) ;
#89477 = EDGE_CURVE ( 'NONE', #58839, #38904, #103530, .T. ) ;
#89476 = CARTESIAN_POINT ( 'NONE',  ( 25.37853710749670100, 1450.982216501690118, 137.2656895386909923 ) ) ;
#89478 = CARTESIAN_POINT ( 'NONE',  ( 14.08840122829999864, 1415.996778985530000, 196.6785942718979925 ) ) ;
#89479 = CARTESIAN_POINT ( 'NONE',  ( -3.709420239419999987, 1414.325356040540100, 206.4743715362490093 ) ) ;
#89480 = CARTESIAN_POINT ( 'NONE',  ( 21.45434793639999782, 1410.156528989129811, 201.8904129172080104 ) ) ;
#89481 = CARTESIAN_POINT ( 'NONE',  ( 28.84486411959998975, 1445.052233488288948, 176.6843673542979332 ) ) ;
#89482 = CARTESIAN_POINT ( 'NONE',  ( 16.98922847780000112, 1409.671041244329899, 225.3825873552979999 ) ) ;
#89483 = CARTESIAN_POINT ( 'NONE',  ( -19.66678637224480397, 1517.151704408390060, 215.8936635741279986 ) ) ;
#89484 = CARTESIAN_POINT ( 'NONE',  ( 21.03221526084817583, 1454.576107912622774, 222.0093531227894061 ) ) ;
#89485 = CARTESIAN_POINT ( 'NONE',  ( 2.500000000000000000, 1439.390253026290111, 161.6061712116469948 ) ) ;
#89486 = CARTESIAN_POINT ( 'NONE',  ( -6.551643424905000401, 1516.807958722750072, 214.9033365145770063 ) ) ;
#89487 = ORIENTED_EDGE ( 'NONE', *, *, #61139, .F. ) ;
#89488 = CARTESIAN_POINT ( 'NONE',  ( 7.708967986252149629, 1516.531870573939841, 207.1906748737330020 ) ) ;
#89489 = CARTESIAN_POINT ( 'NONE',  ( -2.621457251404222255, 1522.051704408389924, 228.0616540033011574 ) ) ;
#89490 = CARTESIAN_POINT ( 'NONE',  ( -3.609044149889999886, 1448.294815638699902, 185.0160860582980149 ) ) ;
#89491 = CARTESIAN_POINT ( 'NONE',  ( 1.154619285495940073E-14, 1421.542801637179991, 144.1895650386140062 ) ) ;
#89492 = CARTESIAN_POINT ( 'NONE',  ( -40.26102048347320306, 1444.237160703029986, 137.0925857260259875 ) ) ;
#89493 = EDGE_CURVE ( 'NONE', #105791, #55354, #25165, .T. ) ;
#89494 = CARTESIAN_POINT ( 'NONE',  ( 10.98404765546614215, 1424.970519178970562, 138.3342105157259425 ) ) ;
#89495 = CARTESIAN_POINT ( 'NONE',  ( 1.854797713449190644, 1416.891245252034878, 232.8243438672992909 ) ) ;
#89496 = CIRCLE ( 'NONE', #55552, 1.000000000000002442 ) ;
#89497 = CARTESIAN_POINT ( 'NONE',  ( -2.634342770595469840, 1484.261925542240078, 183.2842859132129831 ) ) ;
#89498 = CARTESIAN_POINT ( 'NONE',  ( 11.87548778179999864, 1433.045415409350198, 150.0930343713980051 ) ) ;
#89499 = CARTESIAN_POINT ( 'NONE',  ( -27.00409795999999929, 1468.895988936930280, 269.4154629628980047 ) ) ;
#89500 = B_SPLINE_SURFACE_WITH_KNOTS ( 'NONE', 4, 5, ( 
 ( #101028, #99374, #40589, #90984, #23222, #14272 ),
 ( #22648, #31630, #110003, #39493, #6985, #65810 ),
 ( #109460, #75317, #57422, #6443, #83148, #56298 ),
 ( #41138, #49561, #91548, #14825, #74760, #32189 ),
 ( #108898, #73664, #66373, #90428, #33280, #49012 ) ),
 .UNSPECIFIED., .F., .F., .F.,
 ( 5, 5 ),
 ( 6, 6 ),
 ( 5.896863119889999894, 6.006609908439999757 ),
 ( 0.000000000000000000, 2.000000000000000000 ),
 .UNSPECIFIED. ) ;
#89501 = CARTESIAN_POINT ( 'NONE',  ( 28.90001227645370108, 1440.913060387309997, 234.6055553947669807 ) ) ;
#89502 = CARTESIAN_POINT ( 'NONE',  ( -109.8888322889999927, 1385.262561173820131, 297.0413350713590148 ) ) ;
#89503 = CARTESIAN_POINT ( 'NONE',  ( 9.817766946204249834, 1499.485800321180022, 202.4310653781669771 ) ) ;
#89504 = EDGE_LOOP ( 'NONE', ( #75856, #101721, #76413, #81567, #68823 ) ) ;
#89505 = CARTESIAN_POINT ( 'NONE',  ( -17.83486663330526767, 1523.678648413191695, 180.3677388339002334 ) ) ;
#89506 = DIRECTION ( 'NONE',  ( -0.000000000000000000, -1.000000000000000000, -0.000000000000000000 ) ) ;
#89507 = CARTESIAN_POINT ( 'NONE',  ( -2.746473951679999637, 1441.879883984389835, 200.6855579648789956 ) ) ;
#89508 = TOROIDAL_SURFACE ( 'NONE', #69888, 30.13701971169416538, 3.000000000000000000 ) ;
#89509 = CARTESIAN_POINT ( 'NONE',  ( -10.87194929170000002, 1491.777874968590140, 211.0477909272190118 ) ) ;
#89510 = CARTESIAN_POINT ( 'NONE',  ( -8.326400914709999768, 1507.918721568629962, 235.2420587249980031 ) ) ;
#89511 = CARTESIAN_POINT ( 'NONE',  ( -30.76149245344669936, 1383.841116178839911, 228.6174415704900014 ) ) ;
#89512 = CARTESIAN_POINT ( 'NONE',  ( -3.176055666263430055, 1508.610720281340036, 204.4420550583219836 ) ) ;
#89513 = CARTESIAN_POINT ( 'NONE',  ( 5.703571544217409972, 1423.268783014629889, 97.22701424869330822 ) ) ;
#89514 = CARTESIAN_POINT ( 'NONE',  ( -11.50607850114139907, 1501.456740653870156, 208.7151705893799942 ) ) ;
#89515 = CARTESIAN_POINT ( 'NONE',  ( 1.486914849300000174, 1466.335769990830158, 234.9545319649979831 ) ) ;
#89517 = ORIENTED_EDGE ( 'NONE', *, *, #66450, .F. ) ;
#89516 = CARTESIAN_POINT ( 'NONE',  ( 3.909710721586129534, 1517.151704408390060, 220.4764703678949900 ) ) ;
#89518 = CARTESIAN_POINT ( 'NONE',  ( -0.4497180320269999476, 1451.473261245730100, 182.7775570608980047 ) ) ;
#89519 = CARTESIAN_POINT ( 'NONE',  ( -28.66947223450000237, 1379.875917421989925, 220.8353055514589869 ) ) ;
#89520 = CARTESIAN_POINT ( 'NONE',  ( -3.428118280760000136, 1475.747349183789993, 199.2424158423789891 ) ) ;
#89522 = ORIENTED_EDGE ( 'NONE', *, *, #72271, .T. ) ;
#89521 = DIRECTION ( 'NONE',  ( -0.4978433412588676998, 0.000000000000000000, 0.8672669759446663962 ) ) ;
#89523 = CARTESIAN_POINT ( 'NONE',  ( -4.705763804352860014, 1479.984617471649926, 230.9466402758990000 ) ) ;
#89524 = EDGE_LOOP ( 'NONE', ( #46628, #21703, #90673, #90674 ) ) ;
#89525 = B_SPLINE_CURVE_WITH_KNOTS ( 'NONE', 5,
 ( #81083, #49158, #97875, #4399, #38527, #90581, #48045, #21705, #106829 ),
 .UNSPECIFIED., .F., .F.,
 ( 6, 3, 6 ),
 ( -24.01273564469999755, -22.33923004749999919, -20.66572445029999727 ),
 .UNSPECIFIED. ) ;
#89526 = CIRCLE ( 'NONE', #41256, 33.13701971169416538 ) ;
#89527 = CARTESIAN_POINT ( 'NONE',  ( -10.82440957829840045, 1387.838188296759881, 217.4113806752309870 ) ) ;
#89528 = CARTESIAN_POINT ( 'NONE',  ( -8.456465142934460388, 1517.051704408389924, 195.1434824822571841 ) ) ;
#89529 = CARTESIAN_POINT ( 'NONE',  ( 3.156166260290000025, 1466.544008048530031, 236.1241471695980181 ) ) ;
#89530 = CARTESIAN_POINT ( 'NONE',  ( -11.60004869885203860, 1426.730434967580550, 134.4361580478455949 ) ) ;
#89531 = DIRECTION ( 'NONE',  ( 0.9510565162951564178, 0.000000000000000000, 0.3090169943749387915 ) ) ;
#89532 = AXIS2_PLACEMENT_3D ( 'NONE', #92414, #110333, #58290 ) ;
#89533 = CARTESIAN_POINT ( 'NONE',  ( 19.53037967897675387, 1509.610924284994326, 186.9102273450286305 ) ) ;
#89534 = CARTESIAN_POINT ( 'NONE',  ( 2.629053311723080100, 1409.004868951980143, 194.3627930264940176 ) ) ;
#89535 = CARTESIAN_POINT ( 'NONE',  ( 3.354719857970000163, 1453.857986919590076, 214.8728744567289937 ) ) ;
#89536 = CARTESIAN_POINT ( 'NONE',  ( -101.1010672691480181, 1385.223634408800081, 296.4705977010279980 ) ) ;
#89537 = CARTESIAN_POINT ( 'NONE',  ( -18.35381443609999863, 1463.216262999530045, 190.2560332892980171 ) ) ;
#89538 = CARTESIAN_POINT ( 'NONE',  ( -68.27348358399999029, 1379.748432006229905, 279.1146441202590722 ) ) ;
#89539 = CARTESIAN_POINT ( 'NONE',  ( -3.259594021489010007, 1449.992738614869950, 184.7284798427360215 ) ) ;
#89540 = ORIENTED_EDGE ( 'NONE', *, *, #13079, .T. ) ;
#89541 = ORIENTED_EDGE ( 'NONE', *, *, #73025, .T. ) ;
#89542 = CARTESIAN_POINT ( 'NONE',  ( 17.89234610336740516, 1523.611961620354123, 237.9279674222333369 ) ) ;
#89543 = CARTESIAN_POINT ( 'NONE',  ( -11.66418951239869983, 1415.301705643500100, 195.2579644112690289 ) ) ;
#89544 = CARTESIAN_POINT ( 'NONE',  ( -11.96285889400000002, 1434.857482882780005, 151.1275188542980175 ) ) ;
#89545 = AXIS2_PLACEMENT_3D ( 'NONE', #26986, #9073, #34821 ) ;
#89546 = B_SPLINE_CURVE_WITH_KNOTS ( 'NONE', 3,
 ( #38451, #46888, #107860, #105684, #64236, #63157, #20533, #47422, #39563, #3788, #37921, #31149, #13782, #89958, #22175, #72101, #65337, #55837, #98905, #73170, #107314, #64796, #29499, #30044, #54190, #106217, #88317, #13233, #11611, #45788, #97804, #21631, #21082, #89416, #81545, #12704, #81014, #4320, #106755, #4846, #30608, #56374, #90504, #32262, #65883, #100004 ),
 .UNSPECIFIED., .F., .F.,
 ( 4, 3, 3, 3, 3, 3, 3, 3, 3, 3, 3, 3, 3, 3, 3, 4 ),
 ( -34.67967148219459972, -33.25777146041880172, -31.83587143864300018, -30.43034291442640082, -29.01390005850370102, -27.61223930463379972, -26.21389002340420049, -24.81975935856400284, -23.82611339485449875, -22.43810463356840046, -21.04786899275110201, -19.65824082723219846, -18.27352136797000171, -16.89443640706300087, -15.52263656855669893, -14.15949905700000144 ),
 .UNSPECIFIED. ) ;
#89547 = CARTESIAN_POINT ( 'NONE',  ( -7.765407202818009861E-10, 1467.540443453480066, 246.7923564290519778 ) ) ;
#89548 = CARTESIAN_POINT ( 'NONE',  ( -20.54913697329470068, 1506.217349134330107, 190.4370943769829978 ) ) ;
#89549 = CARTESIAN_POINT ( 'NONE',  ( 10.07328664426130516, 1509.264827308277518, 236.8976276071642246 ) ) ;
#89550 = CARTESIAN_POINT ( 'NONE',  ( -109.1248564459999955, 1385.804671263960017, 311.1746157432589825 ) ) ;
#89551 = CARTESIAN_POINT ( 'NONE',  ( 0.2192852207989999802, 1452.168323573130010, 183.2890642940980115 ) ) ;
#89552 = CARTESIAN_POINT ( 'NONE',  ( -11.87249271966457620, 1363.781469426163085, 209.6218459617033432 ) ) ;
#89553 = CARTESIAN_POINT ( 'NONE',  ( -26.43279506992269390, 1436.721711417935239, 136.8206605300602234 ) ) ;
#89554 = CARTESIAN_POINT ( 'NONE',  ( 1.514120561980000183E-16, 1515.551704408389924, 209.1218459616989946 ) ) ;
#89555 = CARTESIAN_POINT ( 'NONE',  ( 0.7374508827770021036, 1516.978425811520083, 207.9881927911069965 ) ) ;
#89556 = CARTESIAN_POINT ( 'NONE',  ( 11.14607745555529839, 1434.019391663140141, 151.6534738377419842 ) ) ;
#89557 = CARTESIAN_POINT ( 'NONE',  ( -13.52799278891819945, 1434.953562907949845, 148.7718104166640103 ) ) ;
#89558 = CARTESIAN_POINT ( 'NONE',  ( -8.024497890290000157, 1385.179405298659958, 218.7778930676890070 ) ) ;
#89559 = FACE_OUTER_BOUND ( 'NONE', #48401, .T. ) ;
#89560 = CARTESIAN_POINT ( 'NONE',  ( 19.03110457515579768, 1457.047041246000163, 226.1578386336209974 ) ) ;
#89561 = FACE_OUTER_BOUND ( 'NONE', #40529, .T. ) ;
#89562 = ORIENTED_EDGE ( 'NONE', *, *, #103560, .F. ) ;
#89563 = CARTESIAN_POINT ( 'NONE',  ( 34.48978216879999792, 1440.913060389390012, 250.0021841763980319 ) ) ;
#89564 = DIRECTION ( 'NONE',  ( 1.755985294532469921E-16, -1.000000000000000000, 1.338183447452831989E-16 ) ) ;
#89566 = DIRECTION ( 'NONE',  ( 0.000000000000000000, 1.000000000000000000, 0.000000000000000000 ) ) ;
#89565 = CARTESIAN_POINT ( 'NONE',  ( -9.984537528192330313, 1425.226300119460120, 93.54765018715950475 ) ) ;
#89567 = CARTESIAN_POINT ( 'NONE',  ( -5.513435592011666664, 1508.603735221805437, 216.3914617690659554 ) ) ;
#89568 = CARTESIAN_POINT ( 'NONE',  ( -25.05703569219999949, 1435.888271332780050, 220.8261789359980014 ) ) ;
#89569 = CARTESIAN_POINT ( 'NONE',  ( -0.2696770069730009545, 1486.167527700089977, 220.6462483113989776 ) ) ;
#89570 = CARTESIAN_POINT ( 'NONE',  ( -13.12775437379390020, 1414.913060581094669, 220.0542260670848123 ) ) ;
#89571 = CARTESIAN_POINT ( 'NONE',  ( 29.24087205800000078, 1450.603665907289951, 136.3826361771980089 ) ) ;
#89572 = ORIENTED_EDGE ( 'NONE', *, *, #82087, .T. ) ;
#89573 = CARTESIAN_POINT ( 'NONE',  ( 11.24566101859999812, 1493.273975466890079, 214.3640310562390141 ) ) ;
#89574 = CARTESIAN_POINT ( 'NONE',  ( -32.02808312589930040, 1512.187213306747481, 197.2787714533499752 ) ) ;
#89575 = CARTESIAN_POINT ( 'NONE',  ( 11.51728378950000042, 1509.315252799729933, 236.2324387071979857 ) ) ;
#89576 = VERTEX_POINT ( 'NONE', #29305 ) ;
#89577 = ORIENTED_EDGE ( 'NONE', *, *, #93787, .F. ) ;
#89578 = CARTESIAN_POINT ( 'NONE',  ( 9.394927480355990568, 1451.851897013709959, 209.9054632338170165 ) ) ;
#89579 = CARTESIAN_POINT ( 'NONE',  ( -24.04783088717389816, 1410.733285934720243, 208.7113026174390029 ) ) ;
#89580 = ORIENTED_EDGE ( 'NONE', *, *, #62089, .T. ) ;
#89581 = CARTESIAN_POINT ( 'NONE',  ( -3.847666503130200422, 1440.496978037559984, 204.4642126257899974 ) ) ;
#89582 = DIRECTION ( 'NONE',  ( 0.000000000000000000, -1.836970198721029688E-16, -1.000000000000000000 ) ) ;
#89583 = VECTOR ( 'NONE', #75930, 1000.000000000000000 ) ;
#89584 = B_SPLINE_CURVE_WITH_KNOTS ( 'NONE', 3,
 ( #51053, #658, #51602, #25816, #8471, #60014, #43750, #77901, #1208, #41549, #33673, #67865, #34236, #92477, #42644, #109852, #15747, #34789, #49948, #75705, #16305, #68422, #7384, #84086, #25262, #42098, #85735, #76797, #110393, #101413, #94135, #24705, #9034, #94693, #43206, #50509, #66772, #68976, #103077, #26378, #60573, #17966, #52161, #100871, #24162, #58352, #19065, #86846, #37547, #35342, #28594, #63333, #52711, #88510, #97453, #44310, #11794, #78454, #61137, #80098, #54916, #45961, #87973, #89042, #28039, #62229, #18514, #20180, #19633, #20721, #95251, #53270, #53834, #45424, #96355, #12330, #36437, #70088, #10702, #1767, #3418, #46520, #71182, #10139, #62796, #80655, #27486, #44874, #36988, #79566, #11262, #71749, #87409, #2867, #61675, #105866, #54378, #29145, #105304, #69530, #96910, #103650, #79025, #26948, #35905, #104201, #95798, #2327, #70634 ),
 .UNSPECIFIED., .F., .F.,
 ( 4, 3, 3, 3, 3, 3, 3, 3, 3, 3, 3, 3, 3, 3, 3, 3, 3, 3, 3, 3, 3, 3, 3, 3, 3, 3, 3, 3, 3, 3, 3, 3, 3, 3, 3, 3, 4 ),
 ( 3.497608506310000198, 4.529268212650570113, 4.673809866680000091, 5.552633724228540402, 5.850011227059999541, 6.748642867657440370, 7.649943429611059997, 8.202413947820000217, 9.104080493403879260, 10.00194339904189889, 10.89091721172289873, 11.77326960059560079, 12.64490599439209895, 12.90721938930000157, 13.77712401890710048, 14.64888018335460096, 15.52348301336279945, 16.34806929659060160, 17.19513031426199845, 18.01644611260000062, 18.06848103991510257, 18.56473004397999915, 18.75451818430730100, 18.85043071655640290, 18.86798389980000223, 18.98461694718449877, 19.11219043176969734, 19.21468060761500141, 19.30785973235489905, 19.39334657279270147, 19.44079725900000000, 19.48296743266269715, 19.52937033080259965, 19.59042956274780067, 19.64886608588970063, 19.69360426244629991, 19.71952168709999853 ),
 .UNSPECIFIED. ) ;
#89585 = CARTESIAN_POINT ( 'NONE',  ( -1.618414601050000012, 1489.063570503329856, 236.3146473097979765 ) ) ;
#89586 = CARTESIAN_POINT ( 'NONE',  ( 16.89460221416486618, 1526.348417187218047, 234.9076154478274248 ) ) ;
#89587 = ORIENTED_EDGE ( 'NONE', *, *, #42783, .T. ) ;
#89588 = CARTESIAN_POINT ( 'NONE',  ( 45.63691321389429589, 1440.912969052420067, 268.9749694736630090 ) ) ;
#89589 = CARTESIAN_POINT ( 'NONE',  ( -12.56955872635460025, 1415.089118586279938, 220.8661684437149972 ) ) ;
#89590 = CARTESIAN_POINT ( 'NONE',  ( -107.6348030694729943, 1384.897191107869958, 297.0734579783350000 ) ) ;
#89591 = CARTESIAN_POINT ( 'NONE',  ( 5.775236792744999903, 1516.804776704140068, 204.1142572851869943 ) ) ;
#89592 = ORIENTED_EDGE ( 'NONE', *, *, #91338, .F. ) ;
#89593 = CARTESIAN_POINT ( 'NONE',  ( 6.919958127207899601, 1483.315291266040049, 218.7186626761050263 ) ) ;
#89594 = CARTESIAN_POINT ( 'NONE',  ( 13.08711526621821442, 1443.014180111750193, 187.3495770229439188 ) ) ;
#89595 = ORIENTED_EDGE ( 'NONE', *, *, #98660, .F. ) ;
#89596 = ORIENTED_EDGE ( 'NONE', *, *, #107944, .F. ) ;
#89597 = CARTESIAN_POINT ( 'NONE',  ( 2.425477467416652377, 1523.390106123591067, 175.1521078860171770 ) ) ;
#89598 = CARTESIAN_POINT ( 'NONE',  ( 0.000000000000000000, 1384.913060387289988, 209.1218459572589836 ) ) ;
#89599 = CARTESIAN_POINT ( 'NONE',  ( 12.72577279029999886, 1508.073447237130040, 233.4251884259979875 ) ) ;
#89600 = CARTESIAN_POINT ( 'NONE',  ( -4.438955121070089938, 1469.007804208310063, 218.6173878029609909 ) ) ;
#89601 = CARTESIAN_POINT ( 'NONE',  ( 22.98351633743509836, 1452.110458311199864, 138.7999742373860101 ) ) ;
#89602 = CARTESIAN_POINT ( 'NONE',  ( 10.46957727719999909, 1420.496586446350193, 197.8100847527989856 ) ) ;
#89603 = CARTESIAN_POINT ( 'NONE',  ( -0.6258287210304879222, 1475.511722453250059, 220.5356275081750255 ) ) ;
#89604 = CARTESIAN_POINT ( 'NONE',  ( 10.99924977368306145, 1433.357864536487796, 151.7593666591178021 ) ) ;
#89605 = CARTESIAN_POINT ( 'NONE',  ( -21.21787123920067586, 1509.703102098133513, 230.0033421491306740 ) ) ;
#89606 = CARTESIAN_POINT ( 'NONE',  ( 0.02456836867461557536, 1409.062161665360918, 232.4158905231754488 ) ) ;
#89608 = CARTESIAN_POINT ( 'NONE',  ( -3.482404828285579956, 1485.996524617339901, 182.2044860649310181 ) ) ;
#89607 = CARTESIAN_POINT ( 'NONE',  ( -18.39585571575249645, 1464.527486176419870, 190.2183615832909993 ) ) ;
#89609 = CARTESIAN_POINT ( 'NONE',  ( 11.35837942423910008, 1422.392381634520007, 207.1029687616070021 ) ) ;
#89610 = VECTOR ( 'NONE', #84560, 1000.000000000000114 ) ;
#89611 = CARTESIAN_POINT ( 'NONE',  ( -9.552138306242289545, 1440.406794419209973, 206.0807338902480126 ) ) ;
#89612 = CARTESIAN_POINT ( 'NONE',  ( -7.643022785574999034, 1513.886778333989923, 202.1073616889970026 ) ) ;
#89613 = EDGE_LOOP ( 'NONE', ( #57401, #12998, #48308, #64817, #81724 ) ) ;
#89614 = CARTESIAN_POINT ( 'NONE',  ( 4.687651746879999415, 1478.378160227390254, 228.9010599218989910 ) ) ;
#89615 = CARTESIAN_POINT ( 'NONE',  ( -16.94401720158110081, 1417.331033520996471, 206.9668984956705629 ) ) ;
#89616 = CARTESIAN_POINT ( 'NONE',  ( -95.18267266084710343, 1384.957561219689978, 310.0846393943140242 ) ) ;
#89617 = CARTESIAN_POINT ( 'NONE',  ( -8.291911044340000814, 1385.641098659349836, 199.7466504416589999 ) ) ;
#89618 = CARTESIAN_POINT ( 'NONE',  ( -15.28223244349999987, 1416.009837697190051, 211.6183304183890073 ) ) ;
#89619 =( BOUNDED_CURVE ( )  B_SPLINE_CURVE ( 3, ( #97754, #5910, #21580, #14291 ),
 .UNSPECIFIED., .F., .F. ) 
 B_SPLINE_CURVE_WITH_KNOTS ( ( 4, 4 ),
 ( 1.569654617349090175, 1.584186644469695038 ),
 .UNSPECIFIED. ) 
 CURVE ( )  GEOMETRIC_REPRESENTATION_ITEM ( )  RATIONAL_B_SPLINE_CURVE ( ( 1.000000000000000000, 0.9999824017597387371, 0.9999824017597387371, 1.000000000000000000 ) ) 
 REPRESENTATION_ITEM ( '' )  );
#89621 = VERTEX_POINT ( 'NONE', #70808 ) ;
#89620 = CARTESIAN_POINT ( 'NONE',  ( -10.61999372029469946, 1462.990852176999852, 206.0510140530389833 ) ) ;
#89622 = CARTESIAN_POINT ( 'NONE',  ( 16.81223226430000039, 1414.913060387329779, 210.6693098017280192 ) ) ;
#89623 = AXIS2_PLACEMENT_3D ( 'NONE', #67478, #14831, #49020 ) ;
#89624 = CARTESIAN_POINT ( 'NONE',  ( 16.48487881372698638, 1525.795403621570358, 236.4701071512044166 ) ) ;
#89625 = CARTESIAN_POINT ( 'NONE',  ( -7.005911337589346921, 1476.499442542723500, 216.7627521230403431 ) ) ;
#89626 = CARTESIAN_POINT ( 'NONE',  ( -1.968833673825499897, 1429.476492495610046, 199.9497084242159985 ) ) ;
#89627 = CARTESIAN_POINT ( 'NONE',  ( 15.36700631263500050, 1514.600163677630007, 224.7419540494670116 ) ) ;
#89628 = CARTESIAN_POINT ( 'NONE',  ( 12.86384817108610079, 1415.089948427380023, 197.4268898898679936 ) ) ;
#89629 = VECTOR ( 'NONE', #10034, 1000.000000000000000 ) ;
#89630 = CARTESIAN_POINT ( 'NONE',  ( 2.981764581055819985, 1456.749145475010209, 198.8578628538780322 ) ) ;
#89631 = CARTESIAN_POINT ( 'NONE',  ( 3.552713678799999608E-15, 1384.913060387289988, 209.1218459572589836 ) ) ;
#89632 = CARTESIAN_POINT ( 'NONE',  ( 13.73047359140000090, 1422.103018753830156, 228.7261909963979747 ) ) ;
#89633 = EDGE_CURVE ( 'NONE', #2864, #42578, #45816, .T. ) ;
#89634 = CARTESIAN_POINT ( 'NONE',  ( -22.01290455779406940, 1522.906363951597314, 235.3651141902285815 ) ) ;
#89635 = CARTESIAN_POINT ( 'NONE',  ( 2.282301578035000222, 1516.836638729160086, 207.4044134838369757 ) ) ;
#89636 = CARTESIAN_POINT ( 'NONE',  ( 41.46315275289999391, 1425.141660529629917, 266.8282284094979673 ) ) ;
#89637 = CARTESIAN_POINT ( 'NONE',  ( -18.88903524680000245, 1410.934759576429997, 223.1880985098980261 ) ) ;
#89638 = CARTESIAN_POINT ( 'NONE',  ( 16.06624336259999808, 1435.502499720209926, 148.4819144917980225 ) ) ;
#89639 = AXIS2_PLACEMENT_3D ( 'NONE', #20367, #54573, #78082 ) ;
#89640 = CARTESIAN_POINT ( 'NONE',  ( 19.93032256160000415, 1508.017639892230136, 189.0239162005979949 ) ) ;
#89641 = CARTESIAN_POINT ( 'NONE',  ( 22.91663120903140083, 1507.606285602550088, 210.6365840681099826 ) ) ;
#89642 = CARTESIAN_POINT ( 'NONE',  ( 12.78755496029999961, 1416.844618638430120, 222.9177554082980066 ) ) ;
#89643 = CARTESIAN_POINT ( 'NONE',  ( 12.45662817246929954, 1427.088122696140090, 206.6493147128259977 ) ) ;
#89644 = DIRECTION ( 'NONE',  ( 1.224227143275519934E-16, 0.02617694830788819954, -0.9996573249755569268 ) ) ;
#89645 = CARTESIAN_POINT ( 'NONE',  ( 0.2148841057284759937, 1454.612562414240074, 183.1842180022130151 ) ) ;
#89646 = CARTESIAN_POINT ( 'NONE',  ( -11.92254695265209996, 1407.392238798829794, 215.8238487423210188 ) ) ;
#89647 = CARTESIAN_POINT ( 'NONE',  ( 0.3152240322409999851, 1418.590776207229965, 184.6848380081979997 ) ) ;
#89648 = CARTESIAN_POINT ( 'NONE',  ( -4.328507300020000059, 1515.100746401290053, 208.0463350318690061 ) ) ;
#89649 = CARTESIAN_POINT ( 'NONE',  ( 0.4812364869308506932, 1484.453808314565094, 198.4264615785256467 ) ) ;
#89650 = CARTESIAN_POINT ( 'NONE',  ( 11.94155113780000121, 1433.614991520300009, 147.2728962421979872 ) ) ;
#89651 = CARTESIAN_POINT ( 'NONE',  ( -28.14953226589999957, 1435.638849176820031, 136.1223312599980204 ) ) ;
#89652 = CARTESIAN_POINT ( 'NONE',  ( 5.501991724969999886, 1440.536034637450030, 185.1205903260980108 ) ) ;
#89653 = ORIENTED_EDGE ( 'NONE', *, *, #58907, .F. ) ;
#89654 = CARTESIAN_POINT ( 'NONE',  ( 2.224758152370000186, 1476.466451172889947, 198.2506516725989911 ) ) ;
#89655 = CARTESIAN_POINT ( 'NONE',  ( -1.235199885961179911, 1408.956194517850008, 224.0686660204410146 ) ) ;
#89656 = CARTESIAN_POINT ( 'NONE',  ( -11.00740228139999921, 1492.792315462490023, 207.9066467806190133 ) ) ;
#89657 = CARTESIAN_POINT ( 'NONE',  ( 0.1903840683780030074, 1469.229546031989912, 189.1368665698990128 ) ) ;
#89658 = PLANE ( 'NONE',  #74212 ) ;
#89659 = CARTESIAN_POINT ( 'NONE',  ( 40.56704996976148436, 1425.248325938897096, 269.1138862120274666 ) ) ;
#89660 = CARTESIAN_POINT ( 'NONE',  ( -11.84289190199999986, 1435.906080920110071, 147.6777950973980182 ) ) ;
#89661 = CARTESIAN_POINT ( 'NONE',  ( 19.70612301839999958, 1434.996842493730128, 210.6610967273779806 ) ) ;
#89662 = CARTESIAN_POINT ( 'NONE',  ( -28.77730028790000105, 1509.917985857229951, 212.2396942694179813 ) ) ;
#89663 = CARTESIAN_POINT ( 'NONE',  ( -99.83863661568889825, 1384.601139973999807, 310.8064402255530467 ) ) ;
#89664 = CARTESIAN_POINT ( 'NONE',  ( -41.61181380557460585, 1384.993891243530015, 214.4858607009509797 ) ) ;
#89665 = CARTESIAN_POINT ( 'NONE',  ( -12.24498567495730050, 1490.542231505709879, 208.5855889815660191 ) ) ;
#89666 = CARTESIAN_POINT ( 'NONE',  ( -4.943465364638519155, 1508.551704408389924, 206.1607460916300170 ) ) ;
#89667 = CARTESIAN_POINT ( 'NONE',  ( -27.53433169550000059, 1451.090186181929994, 136.3574917508980207 ) ) ;
#89668 = CARTESIAN_POINT ( 'NONE',  ( -30.79106905599208588, 1526.107880201381477, 201.1252782592679864 ) ) ;
#89670 = ORIENTED_EDGE ( 'NONE', *, *, #76306, .T. ) ;
#89669 = CARTESIAN_POINT ( 'NONE',  ( 0.9157618521929991040, 1508.480794317990103, 218.1010525276389842 ) ) ;
#89671 = CARTESIAN_POINT ( 'NONE',  ( -109.3079486820000028, 1384.885661341739933, 311.2646263232589376 ) ) ;
#89672 = ADVANCED_FACE ( 'NONE', ( #20342 ), #70726, .F. ) ;
#89673 = CARTESIAN_POINT ( 'NONE',  ( -23.13309514930000077, 1409.720885870030088, 208.8451414652710127 ) ) ;
#89674 = ADVANCED_FACE ( 'NONE', ( #62395 ), #37632, .F. ) ;
#89675 = AXIS2_PLACEMENT_3D ( 'NONE', #652, #36982, #1762 ) ;
#89676 = CARTESIAN_POINT ( 'NONE',  ( -25.25200574389469921, 1450.804213008409988, 137.6134964715130025 ) ) ;
#89677 = CARTESIAN_POINT ( 'NONE',  ( -11.75715125319999999, 1415.140114695929924, 195.7397137993980039 ) ) ;
#89678 = CARTESIAN_POINT ( 'NONE',  ( 0.003765252625069999848, 1466.769817372230136, 235.6257278897980143 ) ) ;
#89679 = ADVANCED_FACE ( 'NONE', ( #56722 ), #38537, .F. ) ;
#89680 = CARTESIAN_POINT ( 'NONE',  ( 18.88559166019999935, 1410.934781852329934, 221.7939351717979832 ) ) ;
#89681 = CARTESIAN_POINT ( 'NONE',  ( -2.421689921559070147, 1414.941989913409998, 186.2944651685450026 ) ) ;
#89682 = CARTESIAN_POINT ( 'NONE',  ( -9.838236027148290930, 1462.268809849160107, 227.9668099468159710 ) ) ;
#89683 = CARTESIAN_POINT ( 'NONE',  ( -5.376483239217891175, 1429.660786141449762, 154.2333551657499982 ) ) ;
#89685 = CARTESIAN_POINT ( 'NONE',  ( -11.78917987459999850, 1378.809900039579816, 205.3323986359689854 ) ) ;
#89684 = CARTESIAN_POINT ( 'NONE',  ( -11.86750609110000099, 1432.440555272449956, 149.9822222932980083 ) ) ;
#89686 = CARTESIAN_POINT ( 'NONE',  ( 25.82124364776869641, 1449.911324753369854, 209.1312396996160032 ) ) ;
#89687 = CARTESIAN_POINT ( 'NONE',  ( -121.0426089508195560, 1371.894749952188249, 291.3379631701592416 ) ) ;
#89688 = DIRECTION ( 'NONE',  ( -0.2054769195713296581, 0.000000000000000000, -0.9786619618251632957 ) ) ;
#89689 = CARTESIAN_POINT ( 'NONE',  ( -1.883560539969999947, 1415.581158730429934, 233.0664532878980140 ) ) ;
#89690 = CARTESIAN_POINT ( 'NONE',  ( 9.925983360900000108, 1364.303202023259928, 210.6218459616991936 ) ) ;
#89691 = AXIS2_PLACEMENT_3D ( 'NONE', #38571, #72748, #106877 ) ;
#89692 = CARTESIAN_POINT ( 'NONE',  ( -7.723480117524999855, 1517.086065052259983, 205.0863097070169943 ) ) ;
#89693 = CARTESIAN_POINT ( 'NONE',  ( -3.379827007410890261, 1485.523830331509998, 182.9521946713460068 ) ) ;
#89694 = ORIENTED_EDGE ( 'NONE', *, *, #25752, .F. ) ;
#89695 = CARTESIAN_POINT ( 'NONE',  ( -8843.778997819570577, -2339.246371527898646, 3013.944470869236739 ) ) ;
#89696 = CARTESIAN_POINT ( 'NONE',  ( 17.86855543449999928, 1415.163755998629995, 210.6784302842380043 ) ) ;
#89698 = ORIENTED_EDGE ( 'NONE', *, *, #33624, .F. ) ;
#89697 = CARTESIAN_POINT ( 'NONE',  ( -68.32464321669628760, 1379.746866834220100, 279.9001328348240349 ) ) ;
#89699 = ORIENTED_EDGE ( 'NONE', *, *, #82941, .F. ) ;
#89700 = CARTESIAN_POINT ( 'NONE',  ( 27.93707802169999965, 1509.154714909829863, 212.3148866501879866 ) ) ;
#89701 = ORIENTED_EDGE ( 'NONE', *, *, #68742, .T. ) ;
#89702 = LINE ( 'NONE', #65071, #20567 ) ;
#89703 = CARTESIAN_POINT ( 'NONE',  ( -15.09047375999177021, 1517.151704408390060, 202.6311677367078232 ) ) ;
#89705 = CARTESIAN_POINT ( 'NONE',  ( -19.63722818156799832, 1519.551704408389924, 200.0074286628000095 ) ) ;
#89704 = CARTESIAN_POINT ( 'NONE',  ( -1.610281973209999908E-15, 1427.674934138829940, 112.4493539157979995 ) ) ;
#89706 = CARTESIAN_POINT ( 'NONE',  ( -2.282301616165000269, 1516.836638729160086, 210.8392784184970026 ) ) ;
#89707 = EDGE_CURVE ( 'NONE', #50703, #77021, #58137, .T. ) ;
#89708 = B_SPLINE_CURVE_WITH_KNOTS ( 'NONE', 3,
 ( #56354, #71541, #97784, #80995, #89936, #2663, #20510, #37344, #98886, #45768, #105097, #4301, #28387 ),
 .UNSPECIFIED., .F., .F.,
 ( 4, 3, 3, 3, 4 ),
 ( 0.000000000000000000, 0.9326141499816539282, 1.865530147010150186, 2.798283637250339684, 3.468500186270000007 ),
 .UNSPECIFIED. ) ;
#89709 = CIRCLE ( 'NONE', #30713, 0.9999999999999975575 ) ;
#89710 = CARTESIAN_POINT ( 'NONE',  ( -24.55869259776619984, 1452.050375068560015, 136.1074992667110166 ) ) ;
#89711 = CARTESIAN_POINT ( 'NONE',  ( -11.15480544429999910, 1425.160630053029990, 144.1619436909979868 ) ) ;
#89712 = CARTESIAN_POINT ( 'NONE',  ( 14.12491358549999987, 1409.406313238730036, 226.3524348291979891 ) ) ;
#89713 = CARTESIAN_POINT ( 'NONE',  ( 10.77494494982569861, 1480.716361118370060, 211.2102488021930071 ) ) ;
#89714 = DIRECTION ( 'NONE',  ( 0.000000000000000000, 0.000000000000000000, 1.000000000000000000 ) ) ;
#89715 = EDGE_CURVE ( 'NONE', #35721, #43348, #26974, .T. ) ;
#89716 = CARTESIAN_POINT ( 'NONE',  ( 41.65030538173530061, 1443.228731902989921, 134.0999999981379744 ) ) ;
#89717 = CARTESIAN_POINT ( 'NONE',  ( 8.897749601629998395, 1427.579448381289922, 192.9038597873990284 ) ) ;
#89718 = CARTESIAN_POINT ( 'NONE',  ( 10.75631864630000045, 1451.138109685189875, 190.3409053448989994 ) ) ;
#89719 = CARTESIAN_POINT ( 'NONE',  ( -16.94109862351797346, 1410.873590852185316, 226.2869239458361790 ) ) ;
#89720 = ORIENTED_EDGE ( 'NONE', *, *, #110571, .T. ) ;
#89721 = ORIENTED_EDGE ( 'NONE', *, *, #68157, .T. ) ;
#89722 = ADVANCED_FACE ( 'NONE', ( #59486 ), #65425, .T. ) ;
#89723 = ORIENTED_EDGE ( 'NONE', *, *, #110291, .F. ) ;
#89724 = B_SPLINE_CURVE_WITH_KNOTS ( 'NONE', 3,
 ( #51040, #6271, #40419, #57803, #74596, #32023 ),
 .UNSPECIFIED., .F., .F.,
 ( 4, 2, 4 ),
 ( 0.000000000000000000, 0.5000000000000000000, 1.000000000000000000 ),
 .UNSPECIFIED. ) ;
#89725 = CARTESIAN_POINT ( 'NONE',  ( 11.23374711189292618, 1410.679338792965154, 229.3371837158982203 ) ) ;
#89726 = CARTESIAN_POINT ( 'NONE',  ( 32.52439779765787620, 1524.599984580802129, 217.0762361364453454 ) ) ;
#89727 = CARTESIAN_POINT ( 'NONE',  ( -15.20279581456499862, 1516.814170398969964, 193.2119433744669834 ) ) ;
#89728 = CARTESIAN_POINT ( 'NONE',  ( -3.140448395399999537, 1485.996777215629891, 182.1629481133980164 ) ) ;
#89729 = VECTOR ( 'NONE', #49163, 1000.000000000000000 ) ;
#89730 = CARTESIAN_POINT ( 'NONE',  ( -18.52166933778729785, 1508.551400274589923, 210.3449052712999787 ) ) ;
#89731 = CARTESIAN_POINT ( 'NONE',  ( -67.31567742948190869, 1379.744923755474019, 277.0446396347198856 ) ) ;
#89732 = CARTESIAN_POINT ( 'NONE',  ( -3.180365954794715400, 1370.226539215816501, 210.2066197577219100 ) ) ;
#89733 = CARTESIAN_POINT ( 'NONE',  ( -0.9145582870020000366, 1497.690648267530150, 231.5795319701980191 ) ) ;
#89734 = CARTESIAN_POINT ( 'NONE',  ( 9.612666450629999915, 1414.913060387329779, 195.8647609382979908 ) ) ;
#89735 = CARTESIAN_POINT ( 'NONE',  ( -60.86138114716440128, 1384.678333052500193, 245.8750988077819954 ) ) ;
#89736 = ORIENTED_EDGE ( 'NONE', *, *, #103476, .T. ) ;
#89737 = AXIS2_PLACEMENT_3D ( 'NONE', #102087, #67425, #101524 ) ;
#89738 = CARTESIAN_POINT ( 'NONE',  ( 4.995623452895000760, 1516.636036526019780, 207.4092012159470073 ) ) ;
#89739 = ORIENTED_EDGE ( 'NONE', *, *, #82984, .F. ) ;
#89740 = CARTESIAN_POINT ( 'NONE',  ( 38.06114384108260396, 1440.913060387330006, 265.0356504283799950 ) ) ;
#89741 = CARTESIAN_POINT ( 'NONE',  ( -31.41104781486826880, 1511.187213306747708, 202.3296363711539527 ) ) ;
#89742 = ORIENTED_EDGE ( 'NONE', *, *, #76298, .F. ) ;
#89743 = CARTESIAN_POINT ( 'NONE',  ( -0.4429558866438589870, 1450.897592026909933, 181.2687265345639958 ) ) ;
#89744 = CARTESIAN_POINT ( 'NONE',  ( -14.38276615811366810, 1518.913060387330006, 182.7943691050095367 ) ) ;
#89745 = CARTESIAN_POINT ( 'NONE',  ( -8.881784196999999612E-15, 1452.913060387330006, 126.8032249175980155 ) ) ;
#89746 = B_SPLINE_CURVE_WITH_KNOTS ( 'NONE', 3,
 ( #72814, #98543, #31895, #23490, #57682, #107497, #91796, #30789, #46522, #106405 ),
 .UNSPECIFIED., .F., .F.,
 ( 4, 2, 2, 2, 4 ),
 ( 0.000000000000000000, 0.2500000000000000000, 0.5000000000000000000, 0.7500000000000000000, 1.000000000000000000 ),
 .UNSPECIFIED. ) ;
#89747 = DIRECTION ( 'NONE',  ( 0.4978433412588755269, 0.000000000000000000, 0.8672669759446619553 ) ) ;
#89748 = CARTESIAN_POINT ( 'NONE',  ( -7.332452461205139826, 1435.726086304749970, 215.5220642470920325 ) ) ;
#89749 = CARTESIAN_POINT ( 'NONE',  ( -5.745732830054069318, 1511.535603804869879, 200.5210532146669777 ) ) ;
#89750 = CARTESIAN_POINT ( 'NONE',  ( 18.29857331400000220, 1408.824872542730191, 266.8292035143980456 ) ) ;
#89751 = CARTESIAN_POINT ( 'NONE',  ( -11.87984373480000144, 1433.310963811260081, 146.4341628266979853 ) ) ;
#89752 = CARTESIAN_POINT ( 'NONE',  ( 11.73605004184446976, 1425.975720587435035, 144.1605505835322560 ) ) ;
#89754 = CARTESIAN_POINT ( 'NONE',  ( 0.05885997228641060702, 1457.844234150280045, 229.0443196536700157 ) ) ;
#89753 = CARTESIAN_POINT ( 'NONE',  ( 2.937605202049999864, 1464.526028384730125, 236.2516354109980057 ) ) ;
#89755 = B_SPLINE_CURVE_WITH_KNOTS ( 'NONE', 5,
 ( #29356, #64648, #36670, #63557, #47823, #98767, #70863, #31010, #6369, #75783, #16389, #6911 ),
 .UNSPECIFIED., .F., .F.,
 ( 6, 3, 3, 6 ),
 ( 0.000000000000000000, 0.2378339703147543949, 0.7135077814956326536, 1.000000000000000000 ),
 .UNSPECIFIED. ) ;
#89756 = CARTESIAN_POINT ( 'NONE',  ( 3.455377977254999955, 1516.627618683580067, 216.0573038954169931 ) ) ;
#89757 = CARTESIAN_POINT ( 'NONE',  ( -0.9205759412220010374, 1469.929133761889943, 216.3346150991189916 ) ) ;
#89758 = CARTESIAN_POINT ( 'NONE',  ( -0.1538198133092779918, 1507.373913156659910, 180.8743467545279771 ) ) ;
#89759 = CARTESIAN_POINT ( 'NONE',  ( 19.12527834899882606, 1443.894831870294183, 213.6836570825134629 ) ) ;
#89760 = CARTESIAN_POINT ( 'NONE',  ( 5.010422963235000360, 1516.929569650079884, 213.1529883219070030 ) ) ;
#89761 = CARTESIAN_POINT ( 'NONE',  ( -21.21614429629999776, 1488.813684182929819, 209.3550077978840136 ) ) ;
#89762 = CARTESIAN_POINT ( 'NONE',  ( 29.67375891017061917, 1525.697947650418428, 221.2718125036566335 ) ) ;
#89764 = ORIENTED_EDGE ( 'NONE', *, *, #17302, .T. ) ;
#89763 = CARTESIAN_POINT ( 'NONE',  ( -3.264420175239999722, 1430.087089178589849, 204.4765990926489962 ) ) ;
#89765 = CARTESIAN_POINT ( 'NONE',  ( -8.371550284740001402, 1384.904409945399948, 199.7750102909289751 ) ) ;
#89766 = CARTESIAN_POINT ( 'NONE',  ( 2.339444114659999990E-09, 1462.218800619629974, 225.7558667929980061 ) ) ;
#89767 = CARTESIAN_POINT ( 'NONE',  ( -11.76643225729999997, 1432.100642793779798, 150.8086033765980289 ) ) ;
#89768 = CARTESIAN_POINT ( 'NONE',  ( -2.170627987649289992, 1485.611815795640041, 197.4219879416550327 ) ) ;
#89769 = CARTESIAN_POINT ( 'NONE',  ( -31.34137657934026677, 1523.481610426287716, 196.3411265156551906 ) ) ;
#89770 = CARTESIAN_POINT ( 'NONE',  ( -14.72897262537098584, 1415.677402202029953, 211.7043269262228762 ) ) ;
#89771 = CARTESIAN_POINT ( 'NONE',  ( -13.35314405190779929, 1481.629087625479769, 225.5920811498180001 ) ) ;
#89772 = EDGE_CURVE ( 'NONE', #10960, #92224, #103848, .T. ) ;
#89773 = AXIS2_PLACEMENT_3D ( 'NONE', #83350, #83904, #109129 ) ;
#89775 = CARTESIAN_POINT ( 'NONE',  ( 5.386383302847690402, 1432.333871934329864, 154.6074109928329960 ) ) ;
#89774 = CARTESIAN_POINT ( 'NONE',  ( -19.70972463880000092, 1444.803624437849976, 224.6978511680979977 ) ) ;
#89776 = CARTESIAN_POINT ( 'NONE',  ( -1.465804341989999982, 1484.360936341829984, 182.4810536920979871 ) ) ;
#89777 = ORIENTED_EDGE ( 'NONE', *, *, #46047, .F. ) ;
#89778 = CARTESIAN_POINT ( 'NONE',  ( -5.785582951674999919, 1516.981965530290154, 205.0894480302270040 ) ) ;
#89779 = CARTESIAN_POINT ( 'NONE',  ( 3.435598742629999869, 1405.939636272029929, 267.2300248611979896 ) ) ;
#89780 = EDGE_CURVE ( 'NONE', #66077, #40683, #78847, .T. ) ;
#89781 = CARTESIAN_POINT ( 'NONE',  ( -16.42420382550000113, 1507.212883782629888, 224.6993357452979865 ) ) ;
#89782 = CARTESIAN_POINT ( 'NONE',  ( 23.52024624973322986, 1433.790221880693707, 214.9612971668913133 ) ) ;
#89783 = CARTESIAN_POINT ( 'NONE',  ( -32.28466283162143213, 1512.187213306747481, 219.1752493337717738 ) ) ;
#89784 = CARTESIAN_POINT ( 'NONE',  ( -1.906499846882070084E-08, 1517.051704408389924, 209.1218459511669892 ) ) ;
#89785 = CIRCLE ( 'NONE', #36091, 1.000000000000000888 ) ;
#89786 = CARTESIAN_POINT ( 'NONE',  ( -10.13093604337480080, 1447.191456030310064, 211.1552813046679944 ) ) ;
#89787 = ADVANCED_FACE ( 'NONE', ( #97478 ), #36714, .F. ) ;
#89788 = CARTESIAN_POINT ( 'NONE',  ( -0.5699886577095060192, 1450.893155944799901, 155.0620570460170029 ) ) ;
#89789 = CARTESIAN_POINT ( 'NONE',  ( -1.609652689937413061, 1451.521214583105120, 183.9748645127235420 ) ) ;
#89790 = CARTESIAN_POINT ( 'NONE',  ( 1.981093176729999739, 1450.324655956839933, 155.6080914326980178 ) ) ;
#89791 = CARTESIAN_POINT ( 'NONE',  ( -13.90692152972509987, 1415.348334734779883, 220.8295855263409919 ) ) ;
#89792 = FACE_OUTER_BOUND ( 'NONE', #38815, .T. ) ;
#89793 = CARTESIAN_POINT ( 'NONE',  ( -25.52872275889999898, 1431.191366577369990, 248.0989693098979956 ) ) ;
#89794 = CARTESIAN_POINT ( 'NONE',  ( 11.18156373363127720, 1425.045528541028943, 138.1873464159537832 ) ) ;
#89795 = CARTESIAN_POINT ( 'NONE',  ( 3.702277819670000358, 1440.893270118220016, 155.9286631201980242 ) ) ;
#89796 = CARTESIAN_POINT ( 'NONE',  ( -0.8855859651640000108, 1475.830651730830141, 266.9608409856979847 ) ) ;
#89797 = CARTESIAN_POINT ( 'NONE',  ( -4.251778211643499894, 1446.495381983220113, 160.8243770259319945 ) ) ;
#89798 = CARTESIAN_POINT ( 'NONE',  ( -19.02991910360000105, 1457.008642855029848, 192.0880663617980133 ) ) ;
#89799 = ADVANCED_FACE ( 'NONE', ( #109732 ), #11464, .T. ) ;
#89800 = DIRECTION ( 'NONE',  ( 0.8775825618903746461, -8.693568535565067726E-32, 0.4794255386041995082 ) ) ;
#89801 = CARTESIAN_POINT ( 'NONE',  ( -33.01652097059809421, 1384.817001746299866, 231.5368980879269998 ) ) ;
#89802 = AXIS2_PLACEMENT_3D ( 'NONE', #80955, #21571, #14835 ) ;
#89803 = CARTESIAN_POINT ( 'NONE',  ( 16.56954271164469716, 1507.336004463039899, 193.5476776774169707 ) ) ;
#89804 = CARTESIAN_POINT ( 'NONE',  ( -106.2219607800000176, 1378.969459979150088, 301.4482640438590693 ) ) ;
#89805 = CARTESIAN_POINT ( 'NONE',  ( 32.79520279072050215, 1523.954914175595377, 217.1622232076301771 ) ) ;
#89806 = CARTESIAN_POINT ( 'NONE',  ( 7.902600983353781139, 1511.989325512384539, 206.0920258474665161 ) ) ;
#89807 = ADVANCED_FACE ( 'NONE', ( #45862 ), #87296, .F. ) ;
#89808 = CARTESIAN_POINT ( 'NONE',  ( -7.863301563632830948, 1396.187652929399974, 216.8893108632619828 ) ) ;
#89809 = EDGE_CURVE ( 'NONE', #47286, #96482, #102070, .T. ) ;
#89810 = CARTESIAN_POINT ( 'NONE',  ( -2.656558671120380133, 1508.551704408389924, 204.1390352724760078 ) ) ;
#89811 = CARTESIAN_POINT ( 'NONE',  ( -44.88917860750000699, 1439.584993159529859, 269.6920180689979247 ) ) ;
#89812 = VERTEX_POINT ( 'NONE', #105762 ) ;
#89813 = CARTESIAN_POINT ( 'NONE',  ( -2.451711519242490311, 1410.376778189126981, 232.6822308553063294 ) ) ;
#89814 = CARTESIAN_POINT ( 'NONE',  ( 2.825023614729999633, 1409.011712385729879, 230.6344011842979853 ) ) ;
#89815 = CARTESIAN_POINT ( 'NONE',  ( -20.49599333844833993, 1525.960063244516959, 233.8638087104925489 ) ) ;
#89817 = CARTESIAN_POINT ( 'NONE',  ( -11.40944913866499988, 1511.843510977570077, 193.5978051729669858 ) ) ;
#89816 = CARTESIAN_POINT ( 'NONE',  ( 10.56488187690000125, 1425.074640677629986, 128.4926088604979952 ) ) ;
#89818 = CARTESIAN_POINT ( 'NONE',  ( -0.2981780139620000547, 1491.118694209130126, 236.6398961300979806 ) ) ;
#89819 = CARTESIAN_POINT ( 'NONE',  ( -7.160726076929999628, 1452.136940029189873, 201.9019911547090089 ) ) ;
#89820 = EDGE_CURVE ( 'NONE', #36699, #108962, #35310, .T. ) ;
#89821 = CARTESIAN_POINT ( 'NONE',  ( 2.871580388595000422, 1517.129577905929864, 202.1716309988170224 ) ) ;
#89822 = CARTESIAN_POINT ( 'NONE',  ( 7.069913304450000879, 1426.666554455719961, 213.2414280093890113 ) ) ;
#89823 = CARTESIAN_POINT ( 'NONE',  ( 16.66442743440000029, 1492.498864364090196, 193.3249227319990098 ) ) ;
#89824 = CARTESIAN_POINT ( 'NONE',  ( 3.510779589379999788, 1509.015428989629982, 180.0383898831980218 ) ) ;
#89825 = DIRECTION ( 'NONE',  ( 1.734723475976805517E-14, 0.000000000000000000, 1.000000000000000000 ) ) ;
#89826 = CARTESIAN_POINT ( 'NONE',  ( -86.31866470790001244, 1376.287402133280011, 302.0943157429590542 ) ) ;
#89827 = CARTESIAN_POINT ( 'NONE',  ( 5.215187551932488397, 1368.779556716660181, 210.6218459616987957 ) ) ;
#89828 = EDGE_CURVE ( 'NONE', #60200, #41219, #44649, .T. ) ;
#89830 = EDGE_LOOP ( 'NONE', ( #90080, #40721, #5867, #77476 ) ) ;
#89829 = CARTESIAN_POINT ( 'NONE',  ( 8.723132970039999989, 1451.781319090490115, 212.2855359169589917 ) ) ;
#89831 = EDGE_LOOP ( 'NONE', ( #86598, #48167, #35659, #44563 ) ) ;
#89832 = CARTESIAN_POINT ( 'NONE',  ( 8.359890770754999423, 1517.051704408389924, 212.3516885548369828 ) ) ;
#89833 = DIRECTION ( 'NONE',  ( 1.836970198721029688E-16, 1.000000000000000000, -1.262177448353620010E-31 ) ) ;
#89834 = CARTESIAN_POINT ( 'NONE',  ( -1.477202341559999965, 1415.048591094029916, 226.7491272332979975 ) ) ;
#89835 = CARTESIAN_POINT ( 'NONE',  ( -12.82920166685754815, 1444.968562662791328, 169.4458598129212419 ) ) ;
#89836 = PLANE ( 'NONE',  #90401 ) ;
#89838 = CARTESIAN_POINT ( 'NONE',  ( -21.50507852072029991, 1505.473545802760100, 209.5822816567780080 ) ) ;
#89837 = CARTESIAN_POINT ( 'NONE',  ( -8.021758511559999860, 1384.613687009050182, 218.7789206626590044 ) ) ;
#89839 = CARTESIAN_POINT ( 'NONE',  ( 11.68659302070000194, 1410.292622361829899, 189.6048334739980135 ) ) ;
#89840 = SURFACE_SIDE_STYLE ('',( #63041 ) ) ;
#89841 = CARTESIAN_POINT ( 'NONE',  ( -40.57136080872869854, 1447.824542289230067, 135.5531601139149984 ) ) ;
#89842 =( NAMED_UNIT ( * ) SI_UNIT ( $, .STERADIAN. ) SOLID_ANGLE_UNIT ( ) );
#89843 = CARTESIAN_POINT ( 'NONE',  ( 11.05891918951989972, 1396.299246355200239, 209.6785178209389926 ) ) ;
#89844 = DIRECTION ( 'NONE',  ( 3.828568698926946970E-16, 0.000000000000000000, -1.000000000000000000 ) ) ;
#89845 = CARTESIAN_POINT ( 'NONE',  ( 11.84502656599999959, 1430.880975159330092, 149.7917605896980149 ) ) ;
#89846 = DIRECTION ( 'NONE',  ( 0.000000000000000000, 1.000000000000000000, 0.000000000000000000 ) ) ;
#89847 = ORIENTED_EDGE ( 'NONE', *, *, #8293, .T. ) ;
#89848 = CARTESIAN_POINT ( 'NONE',  ( 4.282619229829998986, 1425.872306577030031, 185.4231226939979820 ) ) ;
#89849 = CARTESIAN_POINT ( 'NONE',  ( 12.16249367390000025, 1441.737599154800137, 188.1412300377979818 ) ) ;
#89850 = B_SPLINE_CURVE_WITH_KNOTS ( 'NONE', 5,
 ( #31846, #108556, #13370, #81143, #23440, #100692 ),
 .UNSPECIFIED., .F., .F.,
 ( 6, 6 ),
 ( 0.000000000000000000, 1.000000000000000000 ),
 .UNSPECIFIED. ) ;
#89851 = VERTEX_POINT ( 'NONE', #1653 ) ;
#89852 = ADVANCED_FACE ( 'NONE', ( #11685 ), #69914, .T. ) ;
#89853 = ORIENTED_EDGE ( 'NONE', *, *, #97902, .F. ) ;
#89854 = CARTESIAN_POINT ( 'NONE',  ( 12.32716646574370145, 1492.190914138330072, 209.5898718627249764 ) ) ;
#89855 = CYLINDRICAL_SURFACE ( 'NONE', #29532, 2.000000000000003553 ) ;
#89856 = CARTESIAN_POINT ( 'NONE',  ( 24.55901760849999960, 1440.913060394469994, 213.0859796112679874 ) ) ;
#89858 = EDGE_CURVE ( 'NONE', #1545, #68662, #100247, .T. ) ;
#89857 = CARTESIAN_POINT ( 'NONE',  ( 13.29676293300000012, 1434.820761659849950, 195.7037073619979992 ) ) ;
#89859 = CARTESIAN_POINT ( 'NONE',  ( 3.457266605394999637, 1516.691414181030041, 214.8945738789770132 ) ) ;
#89860 = CARTESIAN_POINT ( 'NONE',  ( -13.69973612571159904, 1380.327653692039803, 209.8720025058139811 ) ) ;
#89861 = ORIENTED_EDGE ( 'NONE', *, *, #14706, .F. ) ;
#89862 = CARTESIAN_POINT ( 'NONE',  ( -17.97364528888469692, 1508.456286852059975, 211.9534032401529942 ) ) ;
#89863 = CARTESIAN_POINT ( 'NONE',  ( -14.37487418797869942, 1509.495309192210016, 182.9308568162230131 ) ) ;
#89864 = CARTESIAN_POINT ( 'NONE',  ( -57.14396138109999868, 1375.865580479029859, 252.3469708248590280 ) ) ;
#89865 = CARTESIAN_POINT ( 'NONE',  ( 4.836108313140000448, 1414.913060387329779, 224.5514542965979956 ) ) ;
#89866 = CARTESIAN_POINT ( 'NONE',  ( 4.030514512585000375, 1516.901952101700090, 204.4990030879170320 ) ) ;
#89867 = EDGE_LOOP ( 'NONE', ( #14873, #6780, #31682, #12467, #89694, #11288, #96202, #27229, #70339 ) ) ;
#89868 = CARTESIAN_POINT ( 'NONE',  ( -28.45308972560000171, 1509.159845678530019, 208.7911871173449754 ) ) ;
#89869 = CARTESIAN_POINT ( 'NONE',  ( -38.90379940696828243, 1429.368923031839358, 269.5913158308796369 ) ) ;
#89870 = CARTESIAN_POINT ( 'NONE',  ( -0.8669575069650000687, 1409.449195270830160, 232.8795264863980208 ) ) ;
#89872 = ORIENTED_EDGE ( 'NONE', *, *, #61336, .F. ) ;
#89871 = CARTESIAN_POINT ( 'NONE',  ( -4.063550476549999679, 1497.713060387329961, 187.6673214695979937 ) ) ;
#89873 = DIRECTION ( 'NONE',  ( 1.000000000000000000, 0.000000000000000000, 0.000000000000000000 ) ) ;
#89874 = CARTESIAN_POINT ( 'NONE',  ( -35.16444583816929992, 1440.913060388340000, 251.2596977943379954 ) ) ;
#89875 = CARTESIAN_POINT ( 'NONE',  ( -86.93521348900000589, 1384.624802884190103, 307.7215772890590415 ) ) ;
#89876 = CARTESIAN_POINT ( 'NONE',  ( -0.4289664345794019784, 1465.008324844339995, 237.3601925583080003 ) ) ;
#89877 = CARTESIAN_POINT ( 'NONE',  ( 28.03275775867099995, 1417.152506600500146, 270.1137522001889693 ) ) ;
#89878 = CARTESIAN_POINT ( 'NONE',  ( -3.253141175365000137, 1516.858171774179937, 212.3894494859370070 ) ) ;
#89879 = CARTESIAN_POINT ( 'NONE',  ( -65.06949576879998176, 1379.738499687689909, 272.5769493850589811 ) ) ;
#89880 = CARTESIAN_POINT ( 'NONE',  ( 23.48437040230000150, 1410.391238764530044, 207.9633649421280097 ) ) ;
#89881 = CARTESIAN_POINT ( 'NONE',  ( 0.02088113289338846754, 1507.124156042135382, 237.3527289089472845 ) ) ;
#89882 = CARTESIAN_POINT ( 'NONE',  ( -30.41976661596593345, 1524.374142163904025, 221.8533802443857894 ) ) ;
#89883 = CARTESIAN_POINT ( 'NONE',  ( -7.709221527022020126, 1516.541553964140121, 211.7112638145030132 ) ) ;
#89884 = CARTESIAN_POINT ( 'NONE',  ( -1.700259714084999763, 1516.898441858519845, 210.8400494336869997 ) ) ;
#89885 = CARTESIAN_POINT ( 'NONE',  ( 4.247639483515419201, 1421.862531007339840, 184.3113611789599986 ) ) ;
#89886 = CARTESIAN_POINT ( 'NONE',  ( -3.082646531299999992, 1415.375634542629996, 232.7232394780980087 ) ) ;
#89887 = CARTESIAN_POINT ( 'NONE',  ( -73.55227667629998223, 1384.892239458130007, 298.9565473808590355 ) ) ;
#89888 = VERTEX_POINT ( 'NONE', #53156 ) ;
#89889 = CARTESIAN_POINT ( 'NONE',  ( -30.24061963389690177, 1385.232462148140030, 228.2819463136630134 ) ) ;
#89890 = CARTESIAN_POINT ( 'NONE',  ( 18.96325319869999859, 1416.831305841230005, 210.2431144155779918 ) ) ;
#89891 = CARTESIAN_POINT ( 'NONE',  ( -113.4000000000000057, 1305.913060387289988, 304.2218459572590064 ) ) ;
#89892 = CARTESIAN_POINT ( 'NONE',  ( 20.15452300067990166, 1507.845791525220193, 189.3412703910400126 ) ) ;
#89893 = CARTESIAN_POINT ( 'NONE',  ( -24.89775034519999863, 1442.835538705840008, 210.5176537872779932 ) ) ;
#89894 = CARTESIAN_POINT ( 'NONE',  ( 10.78022355800000120, 1423.856158455210107, 204.2982030289390138 ) ) ;
#89895 = CARTESIAN_POINT ( 'NONE',  ( -21.62164173326539895, 1517.051704408389924, 210.2163513712909833 ) ) ;
#89896 = ADVANCED_FACE ( 'NONE', ( #20608 ), #71642, .F. ) ;
#89898 = CARTESIAN_POINT ( 'NONE',  ( 18.34590456075850184, 1416.851343895820037, 209.3831232368769975 ) ) ;
#89897 = CARTESIAN_POINT ( 'NONE',  ( 2.485845998894999909, 1516.545806094630279, 216.4433018439569878 ) ) ;
#89899 = DIRECTION ( 'NONE',  ( 1.000000000000000000, 0.000000000000000000, 0.000000000000000000 ) ) ;
#89900 = CARTESIAN_POINT ( 'NONE',  ( 10.38868706420140064, 1469.976612653159918, 207.5338502487639971 ) ) ;
#89901 = EDGE_LOOP ( 'NONE', ( #71917, #18451, #8187, #61510 ) ) ;
#89902 = CARTESIAN_POINT ( 'NONE',  ( 2.290886266485000267, 1517.184383877180153, 201.7830921018669983 ) ) ;
#89903 = CARTESIAN_POINT ( 'NONE',  ( -15.25940260716499886, 1512.044075975079977, 221.6912987172670171 ) ) ;
#89904 = ORIENTED_EDGE ( 'NONE', *, *, #2988, .F. ) ;
#89905 = CARTESIAN_POINT ( 'NONE',  ( 11.60004869885205459, 1426.591397983647767, 134.9942396637077024 ) ) ;
#89906 = CARTESIAN_POINT ( 'NONE',  ( 10.59993614363193970, 1434.841029502628317, 152.0686027719855531 ) ) ;
#89907 = CARTESIAN_POINT ( 'NONE',  ( 7.554100936931009258, 1510.639750819960000, 203.5987926776629706 ) ) ;
#89908 = CARTESIAN_POINT ( 'NONE',  ( 2.729745825120000191, 1442.383552003789873, 217.6907392106589896 ) ) ;
#89909 = CARTESIAN_POINT ( 'NONE',  ( -27.88505092258619911, 1509.867173926660143, 200.9431876222099902 ) ) ;
#89910 = ADVANCED_FACE ( 'NONE', ( #106295 ), #56451, .F. ) ;
#89911 = CARTESIAN_POINT ( 'NONE',  ( -4.260142627790000525, 1446.575473928930023, 159.4573725592980225 ) ) ;
#89912 = CARTESIAN_POINT ( 'NONE',  ( -18.95264117809999860, 1425.362752766330232, 224.3521994502980021 ) ) ;
#89913 = CARTESIAN_POINT ( 'NONE',  ( -30.31940284292427634, 1512.187213306747481, 195.7503880523418616 ) ) ;
#89914 = CARTESIAN_POINT ( 'NONE',  ( -104.4841888330000046, 1390.137343023919811, 303.0785894239589879 ) ) ;
#89915 = CARTESIAN_POINT ( 'NONE',  ( 2.719262146893400038E-32, 1524.051704408389924, 209.1218459616989946 ) ) ;
#89917 = CARTESIAN_POINT ( 'NONE',  ( 28.29412261439999909, 1508.657108462829910, 209.2602327817579919 ) ) ;
#89916 = CARTESIAN_POINT ( 'NONE',  ( -105.4624709189999834, 1391.255327103129957, 304.2078109453590287 ) ) ;
#89918 = CARTESIAN_POINT ( 'NONE',  ( 0.4992773797353766141, 1524.841055067849993, 244.1317247718872068 ) ) ;
#89919 = ORIENTED_EDGE ( 'NONE', *, *, #48082, .F. ) ;
#89921 = EDGE_CURVE ( 'NONE', #80100, #57683, #23534, .T. ) ;
#89920 = CARTESIAN_POINT ( 'NONE',  ( -2.923521517025829741, 1410.394928878200062, 186.6127595807840009 ) ) ;
#89922 = CARTESIAN_POINT ( 'NONE',  ( -8.869906122459999764, 1508.539665163490099, 218.9157064153390024 ) ) ;
#89923 = CARTESIAN_POINT ( 'NONE',  ( 1.106990746626510029E-15, 1390.939237335599955, 209.1218459572589836 ) ) ;
#89924 = CARTESIAN_POINT ( 'NONE',  ( 11.34715271451710095, 1470.684505017819902, 208.1686757782699999 ) ) ;
#89925 = CARTESIAN_POINT ( 'NONE',  ( -14.59882275830000076, 1475.513060387329915, 223.7206687204979971 ) ) ;
#89926 = CARTESIAN_POINT ( 'NONE',  ( -18.55728995089999955, 1509.324399913130037, 230.4821994879980025 ) ) ;
#89927 = CARTESIAN_POINT ( 'NONE',  ( -3.317918599975760330, 1524.412928176729338, 241.9115272520634790 ) ) ;
#89928 = CARTESIAN_POINT ( 'NONE',  ( -13.05831431138886956, 1442.991492262945712, 186.6128402540535092 ) ) ;
#89929 = CARTESIAN_POINT ( 'NONE',  ( 26.79414481833639883, 1435.433178084320161, 135.2874577367330176 ) ) ;
#89930 = CARTESIAN_POINT ( 'NONE',  ( -19.66678637224480397, 1519.551704408389924, 215.8936635741279986 ) ) ;
#89931 = CARTESIAN_POINT ( 'NONE',  ( -17.84103545810000213, 1489.004099770289940, 195.1797354288989936 ) ) ;
#89932 = CARTESIAN_POINT ( 'NONE',  ( -30.31052258194577931, 1523.604703353109699, 222.4930856806594193 ) ) ;
#89933 = CARTESIAN_POINT ( 'NONE',  ( -9.658033403218869495, 1460.449140326730003, 209.2581822647210004 ) ) ;
#89934 =( BOUNDED_CURVE ( )  B_SPLINE_CURVE ( 3, ( #52799, #8010, #85260, #102598 ),
 .UNSPECIFIED., .F., .F. ) 
 B_SPLINE_CURVE_WITH_KNOTS ( ( 4, 4 ),
 ( 6.131270930140640729, 6.235467248071880242 ),
 .UNSPECIFIED. ) 
 CURVE ( )  GEOMETRIC_REPRESENTATION_ITEM ( )  RATIONAL_B_SPLINE_CURVE ( ( 1.000000000000000000, 0.9990954652306247574, 0.9990954652306247574, 1.000000000000000000 ) ) 
 REPRESENTATION_ITEM ( '' )  );
#89935 = CARTESIAN_POINT ( 'NONE',  ( -0.7166913390183430321, 1516.729697371089969, 201.4076976688539844 ) ) ;
#89937 = EDGE_LOOP ( 'NONE', ( #108369, #96730, #108874, #98990 ) ) ;
#89936 = CARTESIAN_POINT ( 'NONE',  ( -18.59348773727160165, 1443.611734087849982, 211.9870899472090002 ) ) ;
#89938 = CARTESIAN_POINT ( 'NONE',  ( -109.9987472829999859, 1382.340119938149883, 310.6123152972590447 ) ) ;
#89939 = EDGE_CURVE ( 'NONE', #100597, #21777, #60957, .T. ) ;
#89940 = CARTESIAN_POINT ( 'NONE',  ( -16.69366550187188381, 1526.382868172863937, 234.5416713104940811 ) ) ;
#89941 = VERTEX_POINT ( 'NONE', #83293 ) ;
#89942 = VERTEX_POINT ( 'NONE', #48049 ) ;
#89943 = FACE_OUTER_BOUND ( 'NONE', #6415, .T. ) ;
#89944 = CARTESIAN_POINT ( 'NONE',  ( 13.04304233460000084, 1507.484018513129968, 233.1962564005980028 ) ) ;
#89945 = CARTESIAN_POINT ( 'NONE',  ( -8.039615859688613142, 1383.830106102227774, 199.5870606692544982 ) ) ;
#89947 = CARTESIAN_POINT ( 'NONE',  ( 4.840407647989999825E-09, 1466.838857907629972, 244.5742075736980041 ) ) ;
#89946 = CARTESIAN_POINT ( 'NONE',  ( 38.63445848827170437, 1428.905190833854476, 269.5867826533756215 ) ) ;
#89948 = EDGE_CURVE ( 'NONE', #52143, #8084, #35923, .T. ) ;
#89949 = CARTESIAN_POINT ( 'NONE',  ( 9.682472890002770782, 1436.279939607890128, 210.8543570392099866 ) ) ;
#89950 = CARTESIAN_POINT ( 'NONE',  ( -11.92436129959999924, 1433.423661116180028, 149.9160561082979939 ) ) ;
#89951 = ADVANCED_FACE ( 'NONE', ( #4402 ), #11696, .T. ) ;
#89952 = DIRECTION ( 'NONE',  ( 0.9236442117861071166, -0.3798549797792020732, 0.05090740978445951193 ) ) ;
#89953 = CARTESIAN_POINT ( 'NONE',  ( 11.60536311244090513, 1426.783531571186131, 134.7591166632975899 ) ) ;
#89954 = CARTESIAN_POINT ( 'NONE',  ( 9.371512452695059281, 1464.461258777040030, 212.0981161559300290 ) ) ;
#89955 = CARTESIAN_POINT ( 'NONE',  ( -25.79175640970000316, 1440.622088907729903, 138.3748975615980044 ) ) ;
#89956 = CARTESIAN_POINT ( 'NONE',  ( -24.41186851410000003, 1440.913063283769816, 212.0284779319380277 ) ) ;
#89957 = DIRECTION ( 'NONE',  ( 0.000000000000000000, 0.7071067811865475727, 0.7071067811865475727 ) ) ;
#89958 = CARTESIAN_POINT ( 'NONE',  ( -6.828376997004060200, 1477.897708468349947, 218.4866115316829962 ) ) ;
#89959 = CARTESIAN_POINT ( 'NONE',  ( 5.604365146386656171, 1361.139420828382072, 210.6218459616987957 ) ) ;
#89960 = EDGE_CURVE ( 'NONE', #101100, #67656, #24566, .T. ) ;
#89961 = CARTESIAN_POINT ( 'NONE',  ( -20.32885181593275448, 1509.740925697234843, 231.1842896567873140 ) ) ;
#89963 = VERTEX_POINT ( 'NONE', #44487 ) ;
#89962 = CARTESIAN_POINT ( 'NONE',  ( 1.124394224133599967E-08, 1406.771932233190000, 265.4689318986550006 ) ) ;
#89964 = EDGE_LOOP ( 'NONE', ( #109952, #60149, #69270, #60114, #95536, #48043, #77883, #14858 ) ) ;
#89965 = CARTESIAN_POINT ( 'NONE',  ( -12.86821319049999879, 1505.199346322990095, 208.9590989587390197 ) ) ;
#89966 = CARTESIAN_POINT ( 'NONE',  ( -11.99264260133359983, 1481.591995386910185, 228.0251739801319957 ) ) ;
#89967 = CARTESIAN_POINT ( 'NONE',  ( -28.70951102109999908, 1465.737235724629954, 270.3384643691979932 ) ) ;
#89968 = DIRECTION ( 'NONE',  ( -5.980589973904019347E-17, 1.000000000000000000, -1.736889445713099699E-16 ) ) ;
#89969 = DIRECTION ( 'NONE',  ( -0.000000000000000000, -1.000000000000000000, -0.000000000000000000 ) ) ;
#89970 = CARTESIAN_POINT ( 'NONE',  ( -5.013264356492538099, 1375.413060387289761, 214.7179447576738482 ) ) ;
#89971 = CARTESIAN_POINT ( 'NONE',  ( 0.2292726218886919909, 1451.597858639469905, 182.7735418884959699 ) ) ;
#89972 = CARTESIAN_POINT ( 'NONE',  ( -14.16989755279999841, 1420.440733325929841, 227.4201777901979824 ) ) ;
#89973 = CARTESIAN_POINT ( 'NONE',  ( -16.17568153084674520, 1459.146937367386045, 230.7169172031621542 ) ) ;
#89974 = CARTESIAN_POINT ( 'NONE',  ( -4.963305069829999638, 1458.663087589289944, 218.6479516874489946 ) ) ;
#89975 = CARTESIAN_POINT ( 'NONE',  ( 8.468955835539853538, 1361.070818662583406, 210.6218459617030021 ) ) ;
#89976 = CARTESIAN_POINT ( 'NONE',  ( -27.41102939123420157, 1412.722695273399950, 266.9253032451249510 ) ) ;
#89977 = ORIENTED_EDGE ( 'NONE', *, *, #18142, .F. ) ;
#89978 = CARTESIAN_POINT ( 'NONE',  ( -3.528579519175909951, 1487.425795918970152, 181.8155835057870036 ) ) ;
#89979 = ADVANCED_FACE ( 'NONE', ( #61860 ), #28687, .T. ) ;
#89980 = VERTEX_POINT ( 'NONE', #32496 ) ;
#89981 = VERTEX_POINT ( 'NONE', #91292 ) ;
#89982 = CARTESIAN_POINT ( 'NONE',  ( 6.564578685215000320, 1517.199196846569976, 210.8299485595169926 ) ) ;
#89983 = CARTESIAN_POINT ( 'NONE',  ( -8.610796597750850268, 1448.268247762119927, 212.2416356316149972 ) ) ;
#89984 = EDGE_CURVE ( 'NONE', #43805, #45625, #2028, .T. ) ;
#89986 = CARTESIAN_POINT ( 'NONE',  ( -2.499999999999998668, 1439.922964613317845, 170.5265280277067461 ) ) ;
#89985 = CARTESIAN_POINT ( 'NONE',  ( -6.933879441005000643, 1516.560253536979872, 211.6083207129769903 ) ) ;
#89987 = CARTESIAN_POINT ( 'NONE',  ( -16.29048445220000119, 1440.437958515699847, 190.0548704972979976 ) ) ;
#89988 = DIRECTION ( 'NONE',  ( 0.000000000000000000, 0.000000000000000000, 1.000000000000000000 ) ) ;
#89989 = ORIENTED_EDGE ( 'NONE', *, *, #16880, .T. ) ;
#89990 = LINE ( 'NONE', #13265, #43942 ) ;
#89991 = EDGE_CURVE ( 'NONE', #12156, #57816, #30828, .T. ) ;
#89992 = CARTESIAN_POINT ( 'NONE',  ( -7.718134667564999774, 1516.881930554049859, 201.7919159189069944 ) ) ;
#89993 = CARTESIAN_POINT ( 'NONE',  ( 9.563615785819999715, 1471.196293976290008, 212.9450669879490192 ) ) ;
#89994 = CARTESIAN_POINT ( 'NONE',  ( -24.13074931272349843, 1384.542629409289930, 202.9617085307660034 ) ) ;
#89995 = CARTESIAN_POINT ( 'NONE',  ( -38.39577626298080304, 1426.808633107450078, 269.8162326586069639 ) ) ;
#89996 = CARTESIAN_POINT ( 'NONE',  ( -31.76432722529999708, 1435.606706419230022, 135.1329931210979964 ) ) ;
#89997 = CARTESIAN_POINT ( 'NONE',  ( -3.320612525290000061, 1396.029018731929909, 198.5240420177980241 ) ) ;
#89999 = VERTEX_POINT ( 'NONE', #73953 ) ;
#89998 = CARTESIAN_POINT ( 'NONE',  ( -8.820192260065399026, 1365.532793008303315, 207.6218459616988241 ) ) ;
#90000 = ORIENTED_EDGE ( 'NONE', *, *, #29727, .T. ) ;
#90001 = CARTESIAN_POINT ( 'NONE',  ( 34.55717928115133475, 1463.247045597946226, 269.2604522464154684 ) ) ;
#90002 = CARTESIAN_POINT ( 'NONE',  ( 1.144541242519509838, 1467.157765914260153, 220.1362019054899974 ) ) ;
#90003 = CARTESIAN_POINT ( 'NONE',  ( -3.347801439296141268, 1518.913060387330006, 176.1543725841967500 ) ) ;
#90004 = CARTESIAN_POINT ( 'NONE',  ( -0.03316221134518849978, 1410.241317949180257, 185.0241807165079990 ) ) ;
#90005 = CARTESIAN_POINT ( 'NONE',  ( -1.700259714084999763, 1516.898441858519845, 210.8400494336869997 ) ) ;
#90006 = CARTESIAN_POINT ( 'NONE',  ( -19.78000735379999853, 1435.771566308190131, 223.7853677692980057 ) ) ;
#90007 = CARTESIAN_POINT ( 'NONE',  ( 10.66803740613750051, 1475.468785709809936, 268.4528686381480043 ) ) ;
#90008 = CARTESIAN_POINT ( 'NONE',  ( -1.587029028349338455, 1467.007754443978001, 235.3619703211468561 ) ) ;
#90009 = CARTESIAN_POINT ( 'NONE',  ( 8.652776102125001145, 1511.435001052829875, 203.7363227704070141 ) ) ;
#90010 = CARTESIAN_POINT ( 'NONE',  ( -5.012317106364999830, 1517.020727862619879, 206.2534121335969814 ) ) ;
#90011 = ORIENTED_EDGE ( 'NONE', *, *, #30425, .T. ) ;
#90012 = CARTESIAN_POINT ( 'NONE',  ( -33.91369107994319876, 1451.728768198530133, 135.3761648363289964 ) ) ;
#90013 = CARTESIAN_POINT ( 'NONE',  ( -22.96340384543530178, 1450.270798277949325, 217.9471854896650882 ) ) ;
#90014 = EDGE_LOOP ( 'NONE', ( #24894, #68953, #25919, #33983, #61242, #33260 ) ) ;
#90015 = CARTESIAN_POINT ( 'NONE',  ( -5.292247061280000331, 1391.913060387289988, 214.4361776263990009 ) ) ;
#90016 = CARTESIAN_POINT ( 'NONE',  ( 24.63819526104030189, 1451.813975265550198, 137.3334418279220017 ) ) ;
#90017 = CARTESIAN_POINT ( 'NONE',  ( 13.45946769660000086, 1415.628674266529742, 196.7502466371980177 ) ) ;
#90018 = CARTESIAN_POINT ( 'NONE',  ( -9.123213394318430147, 1384.511223218079977, 199.9709075427289804 ) ) ;
#90019 = CARTESIAN_POINT ( 'NONE',  ( 21.64785686290000299, 1411.027693062930211, 201.8270548794779984 ) ) ;
#90020 = DIRECTION ( 'NONE',  ( -1.000000000000000000, 0.000000000000000000, 0.000000000000000000 ) ) ;
#90021 = CARTESIAN_POINT ( 'NONE',  ( 10.58556907870000074, 1489.200871216989981, 206.2039989270789988 ) ) ;
#90022 = DIRECTION ( 'NONE',  ( 0.9942586961433742543, 0.000000000000000000, -0.1070030146457445069 ) ) ;
#90023 = CARTESIAN_POINT ( 'NONE',  ( 24.53302258951347525, 1443.964919931875556, 213.3614358596423983 ) ) ;
#90024 = CARTESIAN_POINT ( 'NONE',  ( 2.500000000000000000, 1439.621629183889809, 170.0481663565560098 ) ) ;
#90025 = CARTESIAN_POINT ( 'NONE',  ( 6.557909882634999299, 1516.908489800550115, 214.8995913655070069 ) ) ;
#90026 = EDGE_LOOP ( 'NONE', ( #70899, #69591, #47836, #47744 ) ) ;
#90027 = CARTESIAN_POINT ( 'NONE',  ( 7.709003288537009446, 1516.533218713809902, 207.2190329785249787 ) ) ;
#90028 = CARTESIAN_POINT ( 'NONE',  ( -3.196891731540000059, 1474.092834640029878, 270.1354749226979379 ) ) ;
#90029 = CARTESIAN_POINT ( 'NONE',  ( 5.257080573758899256, 1517.151704408390060, 218.9984329930441618 ) ) ;
#90030 = CARTESIAN_POINT ( 'NONE',  ( -6.160533402158700156, 1422.363863605520010, 133.5162229238370060 ) ) ;
#90031 = CARTESIAN_POINT ( 'NONE',  ( -37.03079991490060507, 1449.523054757250065, 136.2935849128809878 ) ) ;
#90032 = CARTESIAN_POINT ( 'NONE',  ( 11.60004869885203682, 1426.073251783285741, 137.8255840559769183 ) ) ;
#90033 = B_SPLINE_CURVE_WITH_KNOTS ( 'NONE', 3,
 ( #96190, #79944, #46365, #96752 ),
 .UNSPECIFIED., .F., .F.,
 ( 4, 4 ),
 ( -23.51228018140000131, -6.734755223260002310 ),
 .UNSPECIFIED. ) ;
#90034 = CARTESIAN_POINT ( 'NONE',  ( 1.833592485732214783, 1416.810683918116865, 232.7762320029798389 ) ) ;
#90035 = CARTESIAN_POINT ( 'NONE',  ( -2.500000000000000000, 1419.382839383030159, 144.1073686758980159 ) ) ;
#90036 = CARTESIAN_POINT ( 'NONE',  ( -0.2705593682478190098, 1455.625011699110019, 198.5897262588950127 ) ) ;
#90037 = CARTESIAN_POINT ( 'NONE',  ( 1.191993025707729934E-05, 1406.952180159080172, 222.1219960650689984 ) ) ;
#90038 = CARTESIAN_POINT ( 'NONE',  ( 34.25124623592680706, 1440.913060384829805, 249.3947555928999975 ) ) ;
#90039 = CARTESIAN_POINT ( 'NONE',  ( 10.83571774430070001, 1499.415958313539932, 203.3525490312119928 ) ) ;
#90040 = ORIENTED_EDGE ( 'NONE', *, *, #20547, .F. ) ;
#90041 = VERTEX_POINT ( 'NONE', #108644 ) ;
#90042 = B_SPLINE_CURVE_WITH_KNOTS ( 'NONE', 5,
 ( #33440, #40208, #24490, #109624, #40759, #84418 ),
 .UNSPECIFIED., .F., .F.,
 ( 6, 6 ),
 ( 0.000000000000000000, 1.000000000000000000 ),
 .UNSPECIFIED. ) ;
#90043 = CARTESIAN_POINT ( 'NONE',  ( 12.37499353609999986, 1442.762691980110048, 150.7815459944920065 ) ) ;
#90044 = FACE_BOUND ( 'NONE', #98471, .T. ) ;
#90045 = CARTESIAN_POINT ( 'NONE',  ( -1.330041464690565611, 1409.969616266280809, 185.6431087925785164 ) ) ;
#90046 = CARTESIAN_POINT ( 'NONE',  ( 1.705087066220000169, 1507.082462650630077, 236.5153987699980007 ) ) ;
#90047 = DIRECTION ( 'NONE',  ( 1.755985294532469921E-16, -1.000000000000000000, 1.338183447452831989E-16 ) ) ;
#90048 = CARTESIAN_POINT ( 'NONE',  ( -5.496544701782279496, 1440.579441524449976, 154.7743156926269705 ) ) ;
#90049 = CARTESIAN_POINT ( 'NONE',  ( -39.22814701120859127, 1383.829334103110114, 240.4562005770879978 ) ) ;
#90050 = CARTESIAN_POINT ( 'NONE',  ( -4.495269895834999474, 1510.967342883699985, 201.4658172643670184 ) ) ;
#90051 = CARTESIAN_POINT ( 'NONE',  ( 23.21626404799999932, 1452.102330582029936, 139.5326100675980001 ) ) ;
#90052 = CARTESIAN_POINT ( 'NONE',  ( -9.094910673856409389, 1384.931050598509955, 199.9427862989620053 ) ) ;
#90053 = CARTESIAN_POINT ( 'NONE',  ( 1.420260064800000110, 1466.712984990630048, 235.0376563120979938 ) ) ;
#90055 = EDGE_LOOP ( 'NONE', ( #56011, #41058, #71129, #59897 ) ) ;
#90054 = CARTESIAN_POINT ( 'NONE',  ( 31.63976464710268388, 1525.343727714918259, 216.1854883492157740 ) ) ;
#90056 = CARTESIAN_POINT ( 'NONE',  ( -0.6686366138079999910, 1452.253038997929934, 183.3051521255979992 ) ) ;
#90057 = EDGE_CURVE ( 'NONE', #68807, #65505, #5617, .T. ) ;
#90058 = CARTESIAN_POINT ( 'NONE',  ( -25.83964422380000059, 1382.988494219330050, 203.6397759949089732 ) ) ;
#90059 = ADVANCED_FACE ( 'NONE', ( #15115 ), #66669, .T. ) ;
#90060 = CARTESIAN_POINT ( 'NONE',  ( 4.206093649894939723, 1508.551704408389924, 204.8199791756389914 ) ) ;
#90062 = ORIENTED_EDGE ( 'NONE', *, *, #89477, .F. ) ;
#90061 = CARTESIAN_POINT ( 'NONE',  ( 0.000000000000000000, 1522.051704408389924, 179.0139814193315999 ) ) ;
#90063 = CARTESIAN_POINT ( 'NONE',  ( -16.61338081808710143, 1463.629459303540216, 220.4654957482720192 ) ) ;
#90064 = ORIENTED_EDGE ( 'NONE', *, *, #72721, .T. ) ;
#90065 = CARTESIAN_POINT ( 'NONE',  ( -9.447981863928919921, 1387.027753276099929, 218.0739194378299999 ) ) ;
#90066 = CARTESIAN_POINT ( 'NONE',  ( 35.97546153048689632, 1437.423085270620049, 136.5373550775509841 ) ) ;
#90067 = CARTESIAN_POINT ( 'NONE',  ( -18.07041998555320106, 1523.313115944345327, 180.1545818505813941 ) ) ;
#90068 = VECTOR ( 'NONE', #93978, 1000.000000000000000 ) ;
#90069 = DIRECTION ( 'NONE',  ( -0.9455185755993178454, 0.000000000000000000, 0.3255681544571539243 ) ) ;
#90070 = DIRECTION ( 'NONE',  ( -0.6906235816661248084, 0.2466512791670449067, 0.6798545542481227999 ) ) ;
#90071 = CARTESIAN_POINT ( 'NONE',  ( 21.39771952614790251, 1509.704955107219803, 188.4542851670070149 ) ) ;
#90072 = CYLINDRICAL_SURFACE ( 'NONE', #86097, 1.638701816490922836 ) ;
#90073 = CARTESIAN_POINT ( 'NONE',  ( 18.29046601820000006, 1425.439462508929864, 225.0338555594980221 ) ) ;
#90074 = CARTESIAN_POINT ( 'NONE',  ( 18.30701642943642327, 1458.756281124563429, 215.8796111928478467 ) ) ;
#90075 = CARTESIAN_POINT ( 'NONE',  ( -19.45301492749999994, 1470.713061780830230, 191.6830327524980078 ) ) ;
#90076 = CARTESIAN_POINT ( 'NONE',  ( -68.78243321479477856, 1379.747970891648492, 280.2954871354117472 ) ) ;
#90077 = AXIS2_PLACEMENT_3D ( 'NONE', #30017, #105654, #64207 ) ;
#90078 = CARTESIAN_POINT ( 'NONE',  ( -2.928230722141350384, 1449.385141265240009, 184.4057003796210097 ) ) ;
#90079 = ORIENTED_EDGE ( 'NONE', *, *, #52242, .T. ) ;
#90080 = ORIENTED_EDGE ( 'NONE', *, *, #93484, .F. ) ;
#90081 = CARTESIAN_POINT ( 'NONE',  ( 19.67623451925527434, 1525.581535527370761, 237.1855307018971928 ) ) ;
#90082 = CARTESIAN_POINT ( 'NONE',  ( -18.61360911655499706, 1441.740792946530064, 211.1815796315490275 ) ) ;
#90083 = CARTESIAN_POINT ( 'NONE',  ( -5.649719788644999241, 1514.216922324319739, 217.7705376956769783 ) ) ;
#90084 = B_SPLINE_CURVE_WITH_KNOTS ( 'NONE', 3,
 ( #87274, #102942, #1631, #8889, #94005, #43070, #35767, #35208, #79433, #43623 ),
 .UNSPECIFIED., .F., .F.,
 ( 4, 2, 2, 2, 4 ),
 ( -0.1037542911854470035, -0.07904524408052189532, -0.05440765139039069331, -0.02871539828174819731, -5.298799732322834188E-10 ),
 .UNSPECIFIED. ) ;
#90085 = CARTESIAN_POINT ( 'NONE',  ( -3.261635522710140146E-10, 1469.285592605210240, 252.0667581022420052 ) ) ;
#90086 = CARTESIAN_POINT ( 'NONE',  ( -20.05210432756090100, 1490.118056226199997, 190.9036615977489930 ) ) ;
#90087 = CARTESIAN_POINT ( 'NONE',  ( -14.90843596520000069, 1420.513868878929998, 212.4962506662589874 ) ) ;
#90088 = CARTESIAN_POINT ( 'NONE',  ( -109.4227531280000107, 1386.586214323900094, 311.1300201212590082 ) ) ;
#90089 = CARTESIAN_POINT ( 'NONE',  ( -1.467496020479999830, 1486.532142015430054, 182.3879484836979827 ) ) ;
#90090 = CARTESIAN_POINT ( 'NONE',  ( -11.67265150915122085, 1366.570619958580210, 209.6218459617033432 ) ) ;
#90091 = CARTESIAN_POINT ( 'NONE',  ( -46.02995229330920068, 1440.913068804449949, 268.4959856126969839 ) ) ;
#90092 = VECTOR ( 'NONE', #105158, 1000.000000000000000 ) ;
#90093 = CARTESIAN_POINT ( 'NONE',  ( 14.13195592840999915, 1452.421092199690065, 222.7290593210850034 ) ) ;
#90094 = CARTESIAN_POINT ( 'NONE',  ( 2.282301578035000222, 1516.836638729160086, 207.4044134838369757 ) ) ;
#90095 = CARTESIAN_POINT ( 'NONE',  ( -9.436093020126769204, 1447.921129549329862, 210.5458514588860055 ) ) ;
#90096 = CARTESIAN_POINT ( 'NONE',  ( 3.985678545446159848, 1408.516722457220112, 222.1641616639979873 ) ) ;
#90097 = CARTESIAN_POINT ( 'NONE',  ( -13.34678598724409859, 1434.913712705049875, 149.0316152958799876 ) ) ;
#90098 = CARTESIAN_POINT ( 'NONE',  ( -8.310258910639999996, 1385.293885163340065, 218.6824948903590098 ) ) ;
#90099 = EDGE_CURVE ( 'NONE', #86013, #25072, #107540, .T. ) ;
#90100 = CARTESIAN_POINT ( 'NONE',  ( 3.134082760970000159, 1421.411057458130017, 144.1516174827979739 ) ) ;
#90101 = CARTESIAN_POINT ( 'NONE',  ( 20.20959865099491992, 1522.382868172863937, 236.2316688286738611 ) ) ;
#90102 = EDGE_LOOP ( 'NONE', ( #102216, #84433, #107220, #82124, #42231 ) ) ;
#90103 = CARTESIAN_POINT ( 'NONE',  ( 5.442004251710000240, 1413.088571896030089, 250.5651368636980294 ) ) ;
#90104 = DIRECTION ( 'NONE',  ( 0.000000000000000000, -1.000000000000000000, 0.000000000000000000 ) ) ;
#90106 = CARTESIAN_POINT ( 'NONE',  ( -17.54329334670000051, 1410.021607005030091, 194.9097843735980007 ) ) ;
#90105 = CARTESIAN_POINT ( 'NONE',  ( 1.530048329109999994, 1452.704402376130020, 183.4894930016980084 ) ) ;
#90107 = EDGE_CURVE ( 'NONE', #104584, #105548, #62816, .T. ) ;
#90108 = CARTESIAN_POINT ( 'NONE',  ( -28.62989887450860138, 1415.197388761415141, 269.9536704965778426 ) ) ;
#90109 = CARTESIAN_POINT ( 'NONE',  ( -16.58223822780000134, 1424.948544771930074, 220.7841459318979958 ) ) ;
#90110 = CARTESIAN_POINT ( 'NONE',  ( -13.15516954878490097, 1379.513185257769919, 208.2695793304900178 ) ) ;
#90111 = CARTESIAN_POINT ( 'NONE',  ( -6.452039925207460946, 1452.687750188360042, 151.7627216464220226 ) ) ;
#90112 = CARTESIAN_POINT ( 'NONE',  ( 28.25319066630000009, 1451.926638454029899, 134.8820817050979883 ) ) ;
#90113 = VERTEX_POINT ( 'NONE', #64469 ) ;
#90114 = CARTESIAN_POINT ( 'NONE',  ( -0.04898430503675949704, 1396.985968514940168, 196.3070536892440145 ) ) ;
#90115 = CARTESIAN_POINT ( 'NONE',  ( 13.59249326269330638, 1513.749562428420177, 225.8724118782147627 ) ) ;
#90116 = CARTESIAN_POINT ( 'NONE',  ( -0.04569930594200000140, 1508.911464532430273, 238.4016181626980142 ) ) ;
#90117 = VERTEX_POINT ( 'NONE', #6179 ) ;
#90118 = ORIENTED_EDGE ( 'NONE', *, *, #2155, .T. ) ;
#90119 = CARTESIAN_POINT ( 'NONE',  ( -16.33178904099999684, 1384.664735002020052, 200.5821943269089900 ) ) ;
#90120 = CARTESIAN_POINT ( 'NONE',  ( -24.02848715508979893, 1410.733037965189851, 208.6273024917730083 ) ) ;
#90121 = B_SPLINE_CURVE_WITH_KNOTS ( 'NONE', 3,
 ( #91577, #92123, #7565, #85358, #50143, #102165 ),
 .UNSPECIFIED., .F., .F.,
 ( 4, 2, 4 ),
 ( 0.000000000000000000, 0.01392848930680899884, 0.02784760531277210086 ),
 .UNSPECIFIED. ) ;
#90122 = EDGE_LOOP ( 'NONE', ( #21024, #45942, #108676, #108662, #108352 ) ) ;
#90123 = CARTESIAN_POINT ( 'NONE',  ( 4.832613787568170061, 1508.551704408610021, 205.6342609684550098 ) ) ;
#90124 = CARTESIAN_POINT ( 'NONE',  ( 3.394586472146719824, 1484.752177823880174, 220.4731790846979891 ) ) ;
#90125 = CARTESIAN_POINT ( 'NONE',  ( -7.332328763730000531, 1479.766960287329994, 234.2465134582980113 ) ) ;
#90126 = DIRECTION ( 'NONE',  ( -1.962483594669999970E-13, -8.350994019880001345E-15, 1.000000000000000000 ) ) ;
#90127 = ORIENTED_EDGE ( 'NONE', *, *, #97559, .F. ) ;
#90128 = CARTESIAN_POINT ( 'NONE',  ( 10.81518740880000173, 1424.921099675630103, 144.1705347732979874 ) ) ;
#90129 = CARTESIAN_POINT ( 'NONE',  ( -12.57270521884790071, 1416.218865267220053, 221.9821426913590017 ) ) ;
#90130 = DIRECTION ( 'NONE',  ( 0.9455185755993178454, 0.000000000000000000, -0.3255681544571537578 ) ) ;
#90131 = CARTESIAN_POINT ( 'NONE',  ( -2.295485539174999978, 1516.651306816259876, 204.1261199623870368 ) ) ;
#90132 = ORIENTED_EDGE ( 'NONE', *, *, #219, .T. ) ;
#90133 = CARTESIAN_POINT ( 'NONE',  ( 9.365354866811589574, 1482.088108353989810, 216.3257182807389825 ) ) ;
#90134 = CARTESIAN_POINT ( 'NONE',  ( 13.25261745213164843, 1443.177766318758358, 187.6357070691568936 ) ) ;
#90135 = ORIENTED_EDGE ( 'NONE', *, *, #80244, .T. ) ;
#90136 = ORIENTED_EDGE ( 'NONE', *, *, #17077, .T. ) ;
#90137 = CARTESIAN_POINT ( 'NONE',  ( 1.909107468229654714, 1507.666028270077504, 220.7249166300547358 ) ) ;
#90138 = CARTESIAN_POINT ( 'NONE',  ( 17.19739463999647100, 1525.960063244516959, 236.2603809477409982 ) ) ;
#90139 = CARTESIAN_POINT ( 'NONE',  ( 5.663308409567039625, 1499.770466072930049, 199.1301411769080119 ) ) ;
#90140 = CARTESIAN_POINT ( 'NONE',  ( -4.271147774425892329, 1424.301298031622082, 185.4449705293434931 ) ) ;
#90141 = CARTESIAN_POINT ( 'NONE',  ( -4.550427519660000364, 1425.535076783930208, 186.2088322612979994 ) ) ;
#90142 = CARTESIAN_POINT ( 'NONE',  ( -1.709436532471480112E-05, 1408.236684775530193, 270.3925729408980487 ) ) ;
#90143 = CARTESIAN_POINT ( 'NONE',  ( -1.848955060214049873, 1475.902979036260149, 220.4212878429429736 ) ) ;
#90144 = CARTESIAN_POINT ( 'NONE',  ( -8.008213785660771578, 1493.854461180789940, 199.7736228595420016 ) ) ;
#90145 = CARTESIAN_POINT ( 'NONE',  ( -19.21356996290061758, 1509.590333268685981, 231.5036793335008838 ) ) ;
#90146 = AXIS2_PLACEMENT_3D ( 'NONE', #89574, #104730, #28019 ) ;
#90147 = CARTESIAN_POINT ( 'NONE',  ( 0.03685098609671132869, 1409.759219108942716, 233.0924633182313812 ) ) ;
#90149 = CARTESIAN_POINT ( 'NONE',  ( -106.1880180564230045, 1391.823619149070055, 306.2181660491010007 ) ) ;
#90148 = CARTESIAN_POINT ( 'NONE',  ( 29.75840146891110649, 1525.320849883649316, 196.2322090936816323 ) ) ;
#90150 = CARTESIAN_POINT ( 'NONE',  ( 10.79885338082780066, 1425.173319402769948, 206.5250427735439871 ) ) ;
#90151 = CARTESIAN_POINT ( 'NONE',  ( -25.13357330590289962, 1509.659395417869973, 222.8360384651579693 ) ) ;
#90152 = CARTESIAN_POINT ( 'NONE',  ( 11.58690141939999840, 1425.690684998030292, 133.5558073867980227 ) ) ;
#90153 = ORIENTED_EDGE ( 'NONE', *, *, #69962, .F. ) ;
#90154 = CARTESIAN_POINT ( 'NONE',  ( 3.114882401830000092, 1426.979439823129951, 214.3676144192479853 ) ) ;
#90155 = CIRCLE ( 'NONE', #40136, 1.000000000000000888 ) ;
#90156 = DIRECTION ( 'NONE',  ( 0.000000000000000000, 0.000000000000000000, -1.000000000000000000 ) ) ;
#90157 = CARTESIAN_POINT ( 'NONE',  ( -85.62862489637198848, 1384.979837283239931, 306.9945860826840658 ) ) ;
#90158 = B_SPLINE_SURFACE_WITH_KNOTS ( 'NONE', 2, 5, ( 
 ( #63988, #88080, #2438, #46082, #4609, #62340 ),
 ( #88628, #12448, #98098, #55032, #45539, #79679 ),
 ( #29255, #21371, #105417, #44981, #20286, #61787 ) ),
 .UNSPECIFIED., .F., .F., .F.,
 ( 3, 3 ),
 ( 6, 6 ),
 ( 1.399803019409999960, 2.016961153140000018 ),
 ( 0.000000000000000000, 1.000000000000000000 ),
 .UNSPECIFIED. ) ;
#90159 = CARTESIAN_POINT ( 'NONE',  ( -10.02009237210000059, 1387.031860423330045, 200.7242823892290176 ) ) ;
#90160 = CARTESIAN_POINT ( 'NONE',  ( 10.85890618524230078, 1422.250279490929870, 211.0007653617559811 ) ) ;
#90162 = ORIENTED_EDGE ( 'NONE', *, *, #17925, .F. ) ;
#90161 = CARTESIAN_POINT ( 'NONE',  ( -15.99559901427390152, 1420.209675652329906, 209.9241255724960240 ) ) ;
#90163 = CARTESIAN_POINT ( 'NONE',  ( 3.972455588910000390, 1429.380171581789909, 216.5671372490689919 ) ) ;
#90164 = CARTESIAN_POINT ( 'NONE',  ( -0.8217888514169999770, 1435.943783413959864, 150.5249316333980119 ) ) ;
#90165 = CARTESIAN_POINT ( 'NONE',  ( -16.91437598810000154, 1417.214259571060211, 207.5096547060990133 ) ) ;
#90166 = CARTESIAN_POINT ( 'NONE',  ( 11.93572966800000046, 1433.501285843680080, 150.1252694811980177 ) ) ;
#90167 = CARTESIAN_POINT ( 'NONE',  ( 14.87514313063500104, 1513.853571676670072, 224.2256597811669963 ) ) ;
#90168 = CARTESIAN_POINT ( 'NONE',  ( 12.98785519611789852, 1415.943166310999914, 196.5430628610019994 ) ) ;
#90169 = CARTESIAN_POINT ( 'NONE',  ( 29.73374635647645547, 1526.349689584397083, 217.2224056390284659 ) ) ;
#90170 = CARTESIAN_POINT ( 'NONE',  ( -109.0592861043541575, 1387.830987840716716, 297.5922214923872389 ) ) ;
#90171 = CARTESIAN_POINT ( 'NONE',  ( 5.943213857399999966, 1419.755023743430002, 231.5246200396979930 ) ) ;
#90172 = CARTESIAN_POINT ( 'NONE',  ( -32.72609422369149001, 1524.152349020271004, 201.1104022277331751 ) ) ;
#90173 = CARTESIAN_POINT ( 'NONE',  ( -1.137296688934999800, 1516.908147884120126, 207.4199954749970232 ) ) ;
#90174 = CARTESIAN_POINT ( 'NONE',  ( 5.826428076080000906, 1473.811884028689974, 218.9454251420289950 ) ) ;
#90175 = CARTESIAN_POINT ( 'NONE',  ( -18.22459200680000180, 1409.714306415329929, 223.2691318219980019 ) ) ;
#90176 = CARTESIAN_POINT ( 'NONE',  ( 14.55375838210000161, 1435.825272921289979, 149.7847056613980214 ) ) ;
#90177 = DIRECTION ( 'NONE',  ( 0.000000000000000000, 0.000000000000000000, 1.000000000000000000 ) ) ;
#90178 = CARTESIAN_POINT ( 'NONE',  ( 37.65047687761219919, 1442.773887286080026, 137.1096749932030150 ) ) ;
#90179 = CARTESIAN_POINT ( 'NONE',  ( 18.80339027203730140, 1425.953307585449693, 225.0197318394450008 ) ) ;
#90180 = CARTESIAN_POINT ( 'NONE',  ( 0.008839277919110500800, 1515.608558013090033, 205.0604244730189976 ) ) ;
#90181 = CARTESIAN_POINT ( 'NONE',  ( -3.968827101022720072, 1521.951704408389787, 229.5396913742049776 ) ) ;
#90182 = CARTESIAN_POINT ( 'NONE',  ( -39.82448890266579866, 1438.723056497909965, 136.0668919366270018 ) ) ;
#90183 = CARTESIAN_POINT ( 'NONE',  ( -3.236789229669999823, 1414.913060387329779, 225.4509929012980081 ) ) ;
#90184 = CARTESIAN_POINT ( 'NONE',  ( 0.2157156553116409969, 1454.149060955749974, 183.2041011444529772 ) ) ;
#90185 = CARTESIAN_POINT ( 'NONE',  ( -11.92059014628319957, 1407.699961494269928, 215.8293613729719880 ) ) ;
#90186 = CARTESIAN_POINT ( 'NONE',  ( 0.05678182167189999713, 1418.511462927230014, 184.6660934127980340 ) ) ;
#90187 = CARTESIAN_POINT ( 'NONE',  ( 18.19590854888143738, 1522.382868172863937, 180.0410247165184501 ) ) ;
#90188 = CARTESIAN_POINT ( 'NONE',  ( -1.427677631911417722, 1483.943482002980318, 198.5321935292907938 ) ) ;
#90189 = CARTESIAN_POINT ( 'NONE',  ( 13.19858043940000059, 1434.900412407629801, 149.0260047559980023 ) ) ;
#90190 = CARTESIAN_POINT ( 'NONE',  ( -36.31760351699959699, 1436.138747409269854, 134.0999999970809995 ) ) ;
#90191 = CARTESIAN_POINT ( 'NONE',  ( 9.343523557230000165, 1442.321883629180093, 184.6435794382980191 ) ) ;
#90192 = ORIENTED_EDGE ( 'NONE', *, *, #68636, .T. ) ;
#90193 = CARTESIAN_POINT ( 'NONE',  ( 0.9648462396720020040, 1486.192668660790105, 197.6233019413989780 ) ) ;
#90194 = CARTESIAN_POINT ( 'NONE',  ( 7.697536492340000258, 1477.591864417890065, 200.7729169044390005 ) ) ;
#90195 = CARTESIAN_POINT ( 'NONE',  ( 40.22845519509999690, 1442.699277658399978, 137.0102247757980081 ) ) ;
#90196 = CARTESIAN_POINT ( 'NONE',  ( -12.16861649890000052, 1490.861372319089924, 207.5435353620889884 ) ) ;
#90197 = CARTESIAN_POINT ( 'NONE',  ( 4.032933083790000595, 1469.757081955990088, 189.5597133099989833 ) ) ;
#90198 = CARTESIAN_POINT ( 'NONE',  ( 14.39191247257890183, 1509.401575546390177, 234.0412317446419763 ) ) ;
#90199 = CARTESIAN_POINT ( 'NONE',  ( 11.43304550802769626, 1407.789912946944924, 269.6098866619304317 ) ) ;
#90200 = CARTESIAN_POINT ( 'NONE',  ( 8.877584795860000710, 1422.885319099519847, 212.4206523501590027 ) ) ;
#90201 = CARTESIAN_POINT ( 'NONE',  ( -12.98673877210000072, 1379.902522067299969, 210.6698428602090019 ) ) ;
#90202 = CARTESIAN_POINT ( 'NONE',  ( -99.14101470300249730, 1384.602434930499840, 310.7191070241219677 ) ) ;
#90203 = CARTESIAN_POINT ( 'NONE',  ( -54.62703117506750061, 1385.036901425090036, 233.1472692318469910 ) ) ;
#90204 = CARTESIAN_POINT ( 'NONE',  ( -12.22107531762499910, 1490.677116594589961, 208.1386805918920118 ) ) ;
#90205 = CARTESIAN_POINT ( 'NONE',  ( -4.923477628844170617, 1508.551704408389924, 206.0739344081519846 ) ) ;
#90206 = CARTESIAN_POINT ( 'NONE',  ( -27.28054590290000192, 1451.100206374529989, 136.3683869527979766 ) ) ;
#90207 = LINE ( 'NONE', #4040, #49969 ) ;
#90208 = CARTESIAN_POINT ( 'NONE',  ( -17.02125645528619913, 1410.875184141109912, 226.2353266115079862 ) ) ;
#90209 = EDGE_CURVE ( 'NONE', #73303, #7907, #75330, .T. ) ;
#90211 = ORIENTED_EDGE ( 'NONE', *, *, #48105, .F. ) ;
#90210 = CARTESIAN_POINT ( 'NONE',  ( 0.5088547212972790446, 1411.680041637540171, 185.0134109359660215 ) ) ;
#90212 = CARTESIAN_POINT ( 'NONE',  ( -109.9849726249999975, 1384.916895159399928, 311.4561123682589709 ) ) ;
#90213 = CARTESIAN_POINT ( 'NONE',  ( 9.751547273671640426, 1469.879570846299885, 211.6488722629640051 ) ) ;
#90214 = CARTESIAN_POINT ( 'NONE',  ( -3.805396659119999914, 1495.647976226690162, 219.6495707272989932 ) ) ;
#90215 = SURFACE_STYLE_FILL_AREA ( #108125 ) ;
#90216 = CARTESIAN_POINT ( 'NONE',  ( -0.2866861870901689646, 1419.027722853580144, 184.6389722060440022 ) ) ;
#90217 = CARTESIAN_POINT ( 'NONE',  ( 0.003562172589289999778, 1467.142144095830190, 235.6416276042979803 ) ) ;
#90218 = ADVANCED_FACE ( 'NONE', ( #99671 ), #99121, .T. ) ;
#90219 = CARTESIAN_POINT ( 'NONE',  ( 19.99392930349999986, 1409.775846518530216, 218.9826064745180076 ) ) ;
#90220 = CARTESIAN_POINT ( 'NONE',  ( -1.798624549303609932, 1414.921120847540124, 185.8456817132880019 ) ) ;
#90221 = CARTESIAN_POINT ( 'NONE',  ( -13.29931690873070060, 1469.324185722580069, 191.9832587503309753 ) ) ;
#90222 = CARTESIAN_POINT ( 'NONE',  ( -17.54372176839999753, 1423.780072466529873, 226.6776802473979728 ) ) ;
#90224 = CARTESIAN_POINT ( 'NONE',  ( 21.38516915557965703, 1522.382868172863937, 180.3939891059721106 ) ) ;
#90223 = LINE ( 'NONE', #49901, #33549 ) ;
#90225 = DIRECTION ( 'NONE',  ( 0.000000000000000000, 0.000000000000000000, -1.000000000000000000 ) ) ;
#90226 = CARTESIAN_POINT ( 'NONE',  ( -101.4843241976999906, 1368.558218059089995, 304.2218459572590064 ) ) ;
#90227 = CARTESIAN_POINT ( 'NONE',  ( 21.62164173326539895, 1517.151704408390060, 208.0273405521070060 ) ) ;
#90228 = DIRECTION ( 'NONE',  ( 0.000000000000000000, 1.000000000000000000, 0.000000000000000000 ) ) ;
#90229 = VECTOR ( 'NONE', #27230, 1000.000000000000000 ) ;
#90230 = CARTESIAN_POINT ( 'NONE',  ( 3.005276066430000448, 1369.205039411269809, 210.6218459616989946 ) ) ;
#90231 = CARTESIAN_POINT ( 'NONE',  ( 2.866857893004999713, 1516.951766529250108, 205.0784797119270024 ) ) ;
#90232 = CARTESIAN_POINT ( 'NONE',  ( -17.86706492440000105, 1424.552609962230008, 227.1966067826979838 ) ) ;
#90233 = ORIENTED_EDGE ( 'NONE', *, *, #10703, .F. ) ;
#90234 = AXIS2_PLACEMENT_3D ( 'NONE', #96504, #11945, #38237 ) ;
#90235 = LINE ( 'NONE', #47706, #70975 ) ;
#90236 = CARTESIAN_POINT ( 'NONE',  ( -4.258475691689660003, 1441.254861102220048, 159.6897597212040125 ) ) ;
#90237 = AXIS2_PLACEMENT_3D ( 'NONE', #65303, #99414, #14862 ) ;
#90239 = EDGE_LOOP ( 'NONE', ( #70501, #16160, #105799, #101578, #4156 ) ) ;
#90238 = CARTESIAN_POINT ( 'NONE',  ( -68.37927156717290700, 1379.746995951000144, 279.9669834283100158 ) ) ;
#90240 = ORIENTED_EDGE ( 'NONE', *, *, #19298, .F. ) ;
#90241 = CARTESIAN_POINT ( 'NONE',  ( 4.270716329343290596, 1515.320037145160768, 207.2788824689123146 ) ) ;
#90242 = ORIENTED_EDGE ( 'NONE', *, *, #99080, .T. ) ;
#90243 = CARTESIAN_POINT ( 'NONE',  ( 0.1723259509675250101, 1485.814687721770042, 221.0067211994579850 ) ) ;
#90244 = CARTESIAN_POINT ( 'NONE',  ( -22.75273496409559826, 1518.913060387330006, 234.5707981297189235 ) ) ;
#90245 =( BOUNDED_SURFACE ( )  B_SPLINE_SURFACE ( 3, 2, ( 
 ( #75219, #39946, #55673 ),
 ( #74118, #41041, #109370 ),
 ( #47252, #21464, #89794 ),
 ( #103137, #52225, #51663 ),
 ( #75760, #24226, #84143 ),
 ( #110456, #66825, #7442 ) ),
 .UNSPECIFIED., .F., .F., .F. ) 
 B_SPLINE_SURFACE_WITH_KNOTS ( ( 4, 2, 4 ),
 ( 3, 3 ),
 ( -1.896842529429832586E-07, 0.001072165293717367192, 0.002144520271687677150 ),
 ( 0.000000000000000000, 0.3183217140536988010 ),
 .UNSPECIFIED. ) 
 GEOMETRIC_REPRESENTATION_ITEM ( )  RATIONAL_B_SPLINE_SURFACE ( (
 ( 1.000000000000000000, 0.9047634226006637803, 0.8701585863180565372),
 ( 1.000000000000000000, 0.9047376462424103760, 0.8701234439506322360),
 ( 1.000000000000000000, 0.9047290734635364817, 0.8701117561962150582),
 ( 1.000000000000000000, 0.9047473679512488820, 0.8701366981062672590),
 ( 1.000000000000000000, 0.9047738115176444662, 0.8701727501162970224),
 ( 1.000000000000000000, 0.9048167665816072569, 0.8702313131850467620) ) ) 
 REPRESENTATION_ITEM ( '' )  SURFACE ( )  );
#90247 = CARTESIAN_POINT ( 'NONE',  ( 0.5363933160299999559, 1508.586927071130049, 180.3878905387979898 ) ) ;
#90246 = CARTESIAN_POINT ( 'NONE',  ( -11.73701142390000030, 1426.696005485330033, 144.1689090389980095 ) ) ;
#90248 = CARTESIAN_POINT ( 'NONE',  ( -1.700259714084999763, 1516.898441858519845, 210.8400494336869997 ) ) ;
#90249 = B_SPLINE_CURVE_WITH_KNOTS ( 'NONE', 3,
 ( #77406, #92532, #7983, #76300, #169, #66280, #75756, #24221, #9094, #109366, #57864, #33729, #85796, #15269, #49460, #25316 ),
 .UNSPECIFIED., .F., .F.,
 ( 4, 3, 3, 3, 3, 4 ),
 ( -7.174280551130140182, -6.801970038525639417, -5.833526344350429937, -4.869644975469700654, -3.907991620792370391, -2.949396961919999782 ),
 .UNSPECIFIED. ) ;
#90250 = CARTESIAN_POINT ( 'NONE',  ( -25.21718682590210037, 1450.979587312889862, 137.5960344802909958 ) ) ;
#90251 = CARTESIAN_POINT ( 'NONE',  ( -107.6068470358870002, 1378.913060387289988, 307.9810573902719852 ) ) ;
#90252 = CARTESIAN_POINT ( 'NONE',  ( 13.94439657179999870, 1410.332512878529997, 228.0517289727980312 ) ) ;
#90253 = CARTESIAN_POINT ( 'NONE',  ( 10.47513610250140026, 1482.040573979539886, 210.7457604718050277 ) ) ;
#90254 =( NAMED_UNIT ( * ) PLANE_ANGLE_UNIT ( ) SI_UNIT ( $, .RADIAN. ) );
#90255 = CARTESIAN_POINT ( 'NONE',  ( 41.40218316853920300, 1445.741963847480065, 134.0999999985380100 ) ) ;
#90256 = CARTESIAN_POINT ( 'NONE',  ( -40.24748973017329945, 1443.039696951350152, 137.0497123184690054 ) ) ;
#90257 = ORIENTED_EDGE ( 'NONE', *, *, #9115, .T. ) ;
#90258 = CARTESIAN_POINT ( 'NONE',  ( -17.11734146840720072, 1420.830825731939967, 201.6585919051609892 ) ) ;
#90259 = CARTESIAN_POINT ( 'NONE',  ( -3.628948333386136760, 1428.810397315499131, 201.2247650147968443 ) ) ;
#90260 = ORIENTED_EDGE ( 'NONE', *, *, #11687, .F. ) ;
#90261 = ORIENTED_EDGE ( 'NONE', *, *, #28676, .F. ) ;
#90262 = CARTESIAN_POINT ( 'NONE',  ( 13.35890006641605865, 1410.752511746112077, 228.3639459599291968 ) ) ;
#90263 = CARTESIAN_POINT ( 'NONE',  ( 31.06561166658629958, 1445.948172529730073, 137.1228041004679881 ) ) ;
#90264 = CARTESIAN_POINT ( 'NONE',  ( -0.005696459569060000581, 1451.697357073530156, 183.0329412725980092 ) ) ;
#90265 = CARTESIAN_POINT ( 'NONE',  ( -3.258850095529999713, 1485.815288458330087, 182.5815364463979904 ) ) ;
#90266 = CARTESIAN_POINT ( 'NONE',  ( 12.24860663770000002, 1442.680101602390096, 186.9125332272980131 ) ) ;
#90267 = CARTESIAN_POINT ( 'NONE',  ( -63.86841275767449133, 1379.736337741658417, 269.9166081863446607 ) ) ;
#90268 = CARTESIAN_POINT ( 'NONE',  ( -0.4093345880009989779, 1463.508080861789949, 199.3143980028889928 ) ) ;
#90269 = TOROIDAL_SURFACE ( 'NONE', #40240, 2.000000000000000000, 1.000000000000000000 ) ;
#90270 = FACE_OUTER_BOUND ( 'NONE', #34084, .T. ) ;
#90271 = CARTESIAN_POINT ( 'NONE',  ( 10.59708812170000058, 1416.824060884929850, 194.4803559377980093 ) ) ;
#90272 = CARTESIAN_POINT ( 'NONE',  ( -86.45468328506269984, 1384.824127158329929, 290.0207638261140346 ) ) ;
#90273 = VERTEX_POINT ( 'NONE', #82889 ) ;
#90274 =( BOUNDED_CURVE ( )  B_SPLINE_CURVE ( 3, ( #69825, #96092, #79309, #61422 ),
 .UNSPECIFIED., .F., .T. ) 
 B_SPLINE_CURVE_WITH_KNOTS ( ( 4, 4 ),
 ( 1.036126831488924926, 2.105455280819345631 ),
 .UNSPECIFIED. ) 
 CURVE ( )  GEOMETRIC_REPRESENTATION_ITEM ( )  RATIONAL_B_SPLINE_CURVE ( ( 1.000000000000000000, 0.9069598485478114203, 0.9069598485478114203, 1.000000000000000000 ) ) 
 REPRESENTATION_ITEM ( '' )  );
#90275 = CARTESIAN_POINT ( 'NONE',  ( 2.291514297774999598, 1517.194972660189933, 201.3955140066269962 ) ) ;
#90276 = CARTESIAN_POINT ( 'NONE',  ( 5.775625077365000415, 1516.745833913490060, 208.3665194962490261 ) ) ;
#90277 = VERTEX_POINT ( 'NONE', #24063 ) ;
#90278 = CARTESIAN_POINT ( 'NONE',  ( 35.20572477793839994, 1440.913060387330006, 261.1485995943819489 ) ) ;
#90279 = CARTESIAN_POINT ( 'NONE',  ( 19.65855403599999818, 1477.370641617730143, 227.1408115753980042 ) ) ;
#90280 = ORIENTED_EDGE ( 'NONE', *, *, #32300, .F. ) ;
#90281 = CARTESIAN_POINT ( 'NONE',  ( -0.03743758868163819808, 1451.696053065270007, 183.0324010646019985 ) ) ;
#90282 = CARTESIAN_POINT ( 'NONE',  ( -15.74506077599999898, 1409.964630928229781, 191.4165501260980022 ) ) ;
#90283 = DIRECTION ( 'NONE',  ( 0.3363363969979660806, -0.9417419115949053898, 0.000000000000000000 ) ) ;
#90284 = CIRCLE ( 'NONE', #67133, 2.000000002117825915 ) ;
#90285 = CARTESIAN_POINT ( 'NONE',  ( -9.511752073085270709, 1460.963492925100127, 207.2886318349059991 ) ) ;
#90286 = CARTESIAN_POINT ( 'NONE',  ( -9.735527157094869821, 1438.291168724430008, 211.0143517203420060 ) ) ;
#90287 = CARTESIAN_POINT ( 'NONE',  ( -5.803572394938940171, 1510.929912129060085, 201.5255253609520025 ) ) ;
#90288 = CARTESIAN_POINT ( 'NONE',  ( 0.7748160517030000527, 1405.993929547030120, 266.9609161638979913 ) ) ;
#90289 = CARTESIAN_POINT ( 'NONE',  ( -5.857434716771726890, 1510.600498191483894, 201.5911444504724841 ) ) ;
#90290 = CARTESIAN_POINT ( 'NONE',  ( -22.66254714602097664, 1523.342713519622748, 181.4291743802705810 ) ) ;
#90292 = CARTESIAN_POINT ( 'NONE',  ( -10.33597699569439676, 1423.067771114430570, 137.1941345535399535 ) ) ;
#90291 = CARTESIAN_POINT ( 'NONE',  ( 12.09637707030000087, 1463.380942464329792, 231.4947967239980073 ) ) ;
#90293 = B_SPLINE_SURFACE_WITH_KNOTS ( 'NONE', 5, 5, ( 
 ( #105407, #97015, #4064, #36542, #11358, #70741 ),
 ( #28140, #104300, #63436, #19735, #89150, #97554 ),
 ( #28699, #71852, #38189, #27589, #53936, #72371 ),
 ( #62905, #62331, #11898, #45528, #44409, #79669 ),
 ( #46624, #95350, #46072, #106501, #18610, #36000 ),
 ( #20277, #79118, #20827, #2974, #88617, #10800 ),
 ( #37092, #71294, #55023, #54481, #80205, #3521 ),
 ( #96455, #70191, #37646, #88070, #61235, #105968 ),
 ( #29246, #44971, #12436, #52810, #86942, #10232 ),
 ( #78549, #1866, #61774, #95898, #19159, #87511 ),
 ( #2426, #29789, #100299, #57225, #65617, #23583 ),
 ( #39292, #6779, #99176, #47157, #13516, #81283 ),
 ( #21906, #31991, #4599, #38733, #82944, #57773 ),
 ( #6234, #72909, #55568, #74564, #49355, #12974 ),
 ( #74011, #108143, #81833, #73466, #75118, #15167 ),
 ( #83484, #40387, #40941, #91892, #91354, #107048 ),
 ( #64524, #108699, #98090, #30882, #63976, #21361 ),
 ( #31436, #99730, #89693, #5138, #90792, #107599 ) ),
 .UNSPECIFIED., .F., .F., .F.,
 ( 6, 3, 3, 3, 3, 6 ),
 ( 6, 6 ),
 ( 3.688330952486170045, 6.839513527549999417, 10.63598301710000094, 15.04879579270000001, 24.05445287550000089, 33.17986963567380343 ),
 ( -0.001310986273832020089, 2.000000000000000000 ),
 .UNSPECIFIED. ) ;
#90294 = CARTESIAN_POINT ( 'NONE',  ( -1.708102627415000185, 1517.199196846569976, 215.6864246554469844 ) ) ;
#90295 = CARTESIAN_POINT ( 'NONE',  ( 22.51756156282889876, 1509.699390964210124, 227.9212218486820234 ) ) ;
#90296 = CARTESIAN_POINT ( 'NONE',  ( -10.48474110849999974, 1480.275079708390194, 208.2232256045050178 ) ) ;
#90297 = CARTESIAN_POINT ( 'NONE',  ( 18.91907327681788686, 1444.756048487146472, 214.3158972188605844 ) ) ;
#90298 = CARTESIAN_POINT ( 'NONE',  ( 0.7572979362240020995, 1516.829948096479939, 212.5714934102470011 ) ) ;
#90299 = EDGE_CURVE ( 'NONE', #46147, #54902, #54000, .T. ) ;
#90300 = CARTESIAN_POINT ( 'NONE',  ( 2.329906356571290083, 1515.372228416479857, 213.3835081553520183 ) ) ;
#90301 = CARTESIAN_POINT ( 'NONE',  ( -10.10004869884733125, 1422.222932908416851, 137.0999999980979851 ) ) ;
#90303 = ORIENTED_EDGE ( 'NONE', *, *, #87792, .T. ) ;
#90302 = CARTESIAN_POINT ( 'NONE',  ( -109.9987472800000035, 1386.462030370639923, 311.2689672492589921 ) ) ;
#90304 = CARTESIAN_POINT ( 'NONE',  ( -7.965810472619998528, 1384.899971912439923, 199.4892297391889997 ) ) ;
#90305 = CARTESIAN_POINT ( 'NONE',  ( 20.03600803810000031, 1452.959368570329843, 217.4640555505980046 ) ) ;
#90306 = ADVANCED_FACE ( 'NONE', ( #14016 ), #27045, .F. ) ;
#90307 = CARTESIAN_POINT ( 'NONE',  ( -11.56636936299999974, 1431.560971557430094, 151.1549291175980159 ) ) ;
#90308 = CARTESIAN_POINT ( 'NONE',  ( -14.35836953849999986, 1415.677402244120003, 204.5300376431989946 ) ) ;
#90309 = EDGE_CURVE ( 'NONE', #85990, #5142, #59369, .T. ) ;
#90310 = CARTESIAN_POINT ( 'NONE',  ( -6.997302092268090412, 1441.814629485520072, 202.4571293489870243 ) ) ;
#90311 = CARTESIAN_POINT ( 'NONE',  ( 2.668886676840000138, 1414.538856421429955, 231.8535933046979949 ) ) ;
#90312 = CYLINDRICAL_SURFACE ( 'NONE', #43044, 2.000000000000003553 ) ;
#90313 = CARTESIAN_POINT ( 'NONE',  ( 12.20364748979999980, 1447.059433187239847, 188.0531537431980098 ) ) ;
#90315 = CARTESIAN_POINT ( 'NONE',  ( 19.08819056019999749, 1456.247773388830183, 225.9807996138980002 ) ) ;
#90314 = CARTESIAN_POINT ( 'NONE',  ( -25.19387440899999930, 1470.081153789430118, 211.8647355342179992 ) ) ;
#90316 = CARTESIAN_POINT ( 'NONE',  ( -1.948797609489999916, 1485.180374433429961, 182.7287261531979823 ) ) ;
#90317 = ORIENTED_EDGE ( 'NONE', *, *, #94887, .F. ) ;
#90318 = CARTESIAN_POINT ( 'NONE',  ( -7.722536802824999214, 1517.050041317280147, 204.5049460973469877 ) ) ;
#90319 = CARTESIAN_POINT ( 'NONE',  ( 7.084264032569999259, 1406.157124000829981, 267.5158752688980144 ) ) ;
#90320 = CARTESIAN_POINT ( 'NONE',  ( -1.842962231260000028, 1515.551704408389924, 212.9514660752490158 ) ) ;
#90321 = CARTESIAN_POINT ( 'NONE',  ( 18.87778356449999961, 1410.875542549930287, 195.0395779401980292 ) ) ;
#90322 = CARTESIAN_POINT ( 'NONE',  ( 21.04721947777625246, 1428.203262266114280, 219.7000736795839657 ) ) ;
#90323 = VECTOR ( 'NONE', #99692, 1000.000000000000000 ) ;
#90324 = DIRECTION ( 'NONE',  ( -0.1612154892182530996, 0.3709952640053770789, 0.9145338047998552433 ) ) ;
#90325 = CARTESIAN_POINT ( 'NONE',  ( 11.60004869885203682, 1424.304602974221552, 137.2803358174371056 ) ) ;
#90326 = CARTESIAN_POINT ( 'NONE',  ( -7.368358975295519642, 1439.428462140772353, 204.4148736406934574 ) ) ;
#90327 = CARTESIAN_POINT ( 'NONE',  ( -1.181727161079999977, 1450.812795825409921, 155.6080925169979707 ) ) ;
#90328 = CARTESIAN_POINT ( 'NONE',  ( -1.591694425982771888, 1451.443140916882612, 183.9247936146681752 ) ) ;
#90329 = CARTESIAN_POINT ( 'NONE',  ( 2.500000000000000000, 1448.894380896710118, 155.6080914321979947 ) ) ;
#90330 = CARTESIAN_POINT ( 'NONE',  ( -14.25441464927300039, 1415.890045859280008, 221.1831556969420092 ) ) ;
#90331 = CARTESIAN_POINT ( 'NONE',  ( 25.91590772989999891, 1441.261220175949802, 138.4451201509980365 ) ) ;
#90332 = CARTESIAN_POINT ( 'NONE',  ( -6.092217317660000298, 1412.362567936729874, 265.6112251771979800 ) ) ;
#90333 = CARTESIAN_POINT ( 'NONE',  ( -12.31045119098629925, 1378.376187953739873, 209.7947064970520046 ) ) ;
#90334 = CARTESIAN_POINT ( 'NONE',  ( 4.242727252399999927, 1441.427684323080030, 162.1744802195979958 ) ) ;
#90335 = CARTESIAN_POINT ( 'NONE',  ( -6.205475772959999858, 1475.744157773729967, 268.4675638380979876 ) ) ;
#90336 = DIRECTION ( 'NONE',  ( -5.980589973904019347E-17, 1.000000000000000000, -1.736889445713099699E-16 ) ) ;
#90337 = DIRECTION ( 'NONE',  ( -0.5877852522924820189, 0.000000000000000000, -0.8090169943749410120 ) ) ;
#90338 = DIRECTION ( 'NONE',  ( 0.02091224828123159837, -0.9990482215818557998, 0.03827961371219689574 ) ) ;
#90339 = CARTESIAN_POINT ( 'NONE',  ( -32.57912550924620376, 1384.818706616959844, 230.9894701418880061 ) ) ;
#90340 = CARTESIAN_POINT ( 'NONE',  ( 33.93019615848955084, 1512.187213306747481, 220.5829544587961095 ) ) ;
#90341 = CARTESIAN_POINT ( 'NONE',  ( 12.26778636213749962, 1416.765224586259819, 223.5774076447450227 ) ) ;
#90342 = CARTESIAN_POINT ( 'NONE',  ( -105.6288279289999963, 1378.913059789030058, 304.0441755682590497 ) ) ;
#90343 = CARTESIAN_POINT ( 'NONE',  ( 32.36539586357643827, 1523.843263703803814, 216.1095015570140276 ) ) ;
#90344 = CARTESIAN_POINT ( 'NONE',  ( 8.392690843783809029, 1511.399183828317064, 204.5144203855979583 ) ) ;
#90345 = CIRCLE ( 'NONE', #88627, 1.999999999999999556 ) ;
#90346 = CARTESIAN_POINT ( 'NONE',  ( -20.46201241340000010, 1410.988590480530092, 198.9701274117980176 ) ) ;
#90347 = CARTESIAN_POINT ( 'NONE',  ( 12.54950410350970103, 1421.558086165679924, 207.1374001497979975 ) ) ;
#90348 = CARTESIAN_POINT ( 'NONE',  ( 19.52361536739011427, 1455.536307519420234, 225.7780045410000582 ) ) ;
#90349 = ORIENTED_EDGE ( 'NONE', *, *, #101594, .F. ) ;
#90350 = EDGE_CURVE ( 'NONE', #61329, #62788, #53933, .T. ) ;
#90351 = CARTESIAN_POINT ( 'NONE',  ( -4.049338806867527119, 1410.430873130929967, 232.1965388422846388 ) ) ;
#90352 = FACE_OUTER_BOUND ( 'NONE', #72351, .T. ) ;
#90353 = AXIS2_PLACEMENT_3D ( 'NONE', #63738, #12198, #98409 ) ;
#90354 = CARTESIAN_POINT ( 'NONE',  ( -18.29179276165280044, 1466.060368039130026, 217.7541609266880016 ) ) ;
#90356 = CARTESIAN_POINT ( 'NONE',  ( -14.56792387476500039, 1513.484013041540038, 193.8069907496669657 ) ) ;
#90355 = CARTESIAN_POINT ( 'NONE',  ( 11.70462718329999952, 1426.716940587629779, 141.8502512716979993 ) ) ;
#90357 = CARTESIAN_POINT ( 'NONE',  ( 2.500000000000000000, 1425.929641636930000, 172.2701767017979932 ) ) ;
#90358 = DIRECTION ( 'NONE',  ( -0.4090087482554232712, -1.225281874271768203E-16, 0.9125304618754006558 ) ) ;
#90359 = CARTESIAN_POINT ( 'NONE',  ( -1.130002532395000037, 1516.621991115350056, 202.1860446705670142 ) ) ;
#90360 = CARTESIAN_POINT ( 'NONE',  ( -6.790918657024139549, 1522.051704408389924, 184.0243675267330161 ) ) ;
#90361 = CARTESIAN_POINT ( 'NONE',  ( 19.38664720319999901, 1498.811923108090014, 221.8202413673990065 ) ) ;
#90362 = CARTESIAN_POINT ( 'NONE',  ( 4.090276254750000007, 1507.742068723129933, 181.5992713909979841 ) ) ;
#90363 = CARTESIAN_POINT ( 'NONE',  ( -17.65294116109440026, 1419.923224108780005, 204.6037421101960376 ) ) ;
#90364 = CARTESIAN_POINT ( 'NONE',  ( -52.99573173910000179, 1376.645807390780192, 254.2473206627590230 ) ) ;
#90365 = CARTESIAN_POINT ( 'NONE',  ( 3.542207350731675586, 1367.916903888309889, 210.6218459617142003 ) ) ;
#90367 = VERTEX_POINT ( 'NONE', #58799 ) ;
#90366 = LINE ( 'NONE', #106088, #44352 ) ;
#90368 = ORIENTED_EDGE ( 'NONE', *, *, #32715, .F. ) ;
#90369 = CARTESIAN_POINT ( 'NONE',  ( -5.492330872600000191, 1396.104856807829947, 199.1956357395080204 ) ) ;
#90370 = CARTESIAN_POINT ( 'NONE',  ( -19.72217329349999915, 1410.523787867230112, 221.4680334561980146 ) ) ;
#90371 = CARTESIAN_POINT ( 'NONE',  ( 1.400808531280000047, 1507.374882240629859, 236.8304372384980070 ) ) ;
#90372 = CARTESIAN_POINT ( 'NONE',  ( -13.46505473512351081, 1444.253858681032625, 169.3609527546826712 ) ) ;
#90373 = DIRECTION ( 'NONE',  ( 0.4999999999998399058, 0.7071067811867739472, -0.4999999999998399058 ) ) ;
#90374 = DIRECTION ( 'NONE',  ( -0.2054769195713296304, -0.000000000000000000, -0.9786619618251631847 ) ) ;
#90376 = CARTESIAN_POINT ( 'NONE',  ( 17.50240768599999797, 1410.866981087730210, 225.6197211887979961 ) ) ;
#90375 = CARTESIAN_POINT ( 'NONE',  ( -7.906113842649999057, 1383.697730676289893, 218.7671565430789826 ) ) ;
#90377 = CARTESIAN_POINT ( 'NONE',  ( -30.61115703708014024, 1523.542365884048195, 196.4197133992117870 ) ) ;
#90378 = CARTESIAN_POINT ( 'NONE',  ( -10.06907521269999961, 1416.520322350429979, 193.4677121538979918 ) ) ;
#90379 = CARTESIAN_POINT ( 'NONE',  ( -40.60083016280549373, 1447.775073852730202, 135.1193631031219979 ) ) ;
#90380 = CARTESIAN_POINT ( 'NONE',  ( 10.25097305582739970, 1396.271032255460113, 213.2864649067509788 ) ) ;
#90381 = CARTESIAN_POINT ( 'NONE',  ( 0.9088213736110000163, 1416.535385209229844, 190.2286903860979805 ) ) ;
#90382 = CARTESIAN_POINT ( 'NONE',  ( 11.26739317570000054, 1429.793092966730001, 151.0732202328979952 ) ) ;
#90383 = CARTESIAN_POINT ( 'NONE',  ( 8.526415735925001016, 1512.074228085009963, 202.6591153066570143 ) ) ;
#90384 = EDGE_LOOP ( 'NONE', ( #45717, #17900, #57426, #3257 ) ) ;
#90385 = CARTESIAN_POINT ( 'NONE',  ( -17.04790460295724230, 1526.208281990537671, 182.6359253440253667 ) ) ;
#90386 = CARTESIAN_POINT ( 'NONE',  ( 21.55489959617532136, 1524.059547553519451, 234.2080540443132861 ) ) ;
#90387 = ORIENTED_EDGE ( 'NONE', *, *, #86501, .T. ) ;
#90388 = VERTEX_POINT ( 'NONE', #7828 ) ;
#90389 = EDGE_CURVE ( 'NONE', #70841, #8770, #17304, .T. ) ;
#90390 = CARTESIAN_POINT ( 'NONE',  ( -19.35824286299009955, 1488.013120477789926, 228.5799778352339899 ) ) ;
#90391 = CARTESIAN_POINT ( 'NONE',  ( -15.31141905560000005, 1459.632573421429925, 229.9709746414979747 ) ) ;
#90392 = CARTESIAN_POINT ( 'NONE',  ( -108.8765025263714250, 1387.919848751604832, 310.7253640878452075 ) ) ;
#90393 = FACE_OUTER_BOUND ( 'NONE', #28678, .T. ) ;
#90394 = CARTESIAN_POINT ( 'NONE',  ( -6.552897405075000847, 1516.858146885269889, 215.6784973415170157 ) ) ;
#90395 = CARTESIAN_POINT ( 'NONE',  ( -12.31717236926220060, 1378.347777968080209, 209.6423893116530337 ) ) ;
#90396 = EDGE_LOOP ( 'NONE', ( #38380, #25179, #106867, #78106 ) ) ;
#90397 = CARTESIAN_POINT ( 'NONE',  ( -17.33117438843089886, 1508.522386692640112, 212.5847705537780143 ) ) ;
#90398 = DIRECTION ( 'NONE',  ( -0.6736849260863841948, 0.000000000000000000, 0.7390186874254148774 ) ) ;
#90399 = CARTESIAN_POINT ( 'NONE',  ( -43.72451106999999837, 1377.617442312380035, 225.9983715054590050 ) ) ;
#90400 = B_SPLINE_CURVE_WITH_KNOTS ( 'NONE', 3,
 ( #60982, #69380, #1615, #18372, #26793, #69938, #36298, #95106, #103489, #29015, #52567, #27903, #79419, #62086, #45280, #71609, #88364, #54238, #62651, #86700, #37410, #11654, #2730, #86150, #104052, #36852, #53690, #63200, #95657, #9994, #78877, #20577, #27343, #18924, #97307, #43607 ),
 .UNSPECIFIED., .F., .F.,
 ( 4, 2, 2, 1, 1, 1, 2, 2, 2, 2, 1, 1, 2, 2, 2, 2, 1, 1, 1, 2, 2, 4 ),
 ( 0.1904315896942847253, 0.2916276409813860493, 0.3422256666249366974, 0.3675246794466333067, 0.3801741858573954302, 0.3864989390627698862, 0.3896613156655327481, 0.3928236922682955545, 0.4940197435555052641, 0.5446177691992000192, 0.5699167820210474522, 0.5825662884320258472, 0.5888910416374537604, 0.5952157948428816736, 0.6964118461295565332, 0.7470098717728940185, 0.7723088845945627057, 0.7849583910053672398, 0.7912831442107969293, 0.7944455208135379198, 0.7976078974162790214, 1.000000000000000000 ),
 .UNSPECIFIED. ) ;
#90401 = AXIS2_PLACEMENT_3D ( 'NONE', #13108, #3110, #54071 ) ;
#90402 = CARTESIAN_POINT ( 'NONE',  ( 17.27338612379999816, 1414.913060387329779, 210.1977510952380044 ) ) ;
#90403 = CARTESIAN_POINT ( 'NONE',  ( -5.011367984924999242, 1516.974592746400049, 205.6720686163770324 ) ) ;
#90404 = ORIENTED_EDGE ( 'NONE', *, *, #4245, .T. ) ;
#90405 = CARTESIAN_POINT ( 'NONE',  ( 2.292217010694999946, 1516.941178807709775, 209.1086494233340147 ) ) ;
#90406 = DIRECTION ( 'NONE',  ( 3.828568698926946970E-16, 0.000000000000000000, -1.000000000000000000 ) ) ;
#90407 = B_SPLINE_SURFACE_WITH_KNOTS ( 'NONE', 5, 1, ( 
 ( #15807, #42157 ),
 ( #25880, #103141 ),
 ( #17467, #102038 ),
 ( #27014, #8537 ),
 ( #77960, #58963 ),
 ( #85241, #60080 ) ),
 .UNSPECIFIED., .F., .F., .F.,
 ( 6, 6 ),
 ( 2, 2 ),
 ( 0.000000000000000000, 3.468500186270000007 ),
 ( 0.000000000000000000, 14.00000000000000000 ),
 .UNSPECIFIED. ) ;
#90408 = CARTESIAN_POINT ( 'NONE',  ( -39.14106390295368243, 1429.794342911720378, 269.5953431606081949 ) ) ;
#90409 = CARTESIAN_POINT ( 'NONE',  ( -0.7002101091710001279, 1408.937512263330063, 232.1050833052979954 ) ) ;
#90411 = VERTEX_POINT ( 'NONE', #33569 ) ;
#90410 = CARTESIAN_POINT ( 'NONE',  ( 2.404972330437235684, 1525.211473355384896, 176.1486567441184832 ) ) ;
#90412 = CARTESIAN_POINT ( 'NONE',  ( -0.01152932003563050117, 1451.938819355580108, 183.0054112925830054 ) ) ;
#90413 = CARTESIAN_POINT ( 'NONE',  ( -31.61895657298340012, 1440.913060388849999, 243.1029565790050242 ) ) ;
#90414 = CARTESIAN_POINT ( 'NONE',  ( -49.74528571340000838, 1383.812288545099818, 260.8378110853589646 ) ) ;
#90415 = CARTESIAN_POINT ( 'NONE',  ( -0.1062606726760350062, 1465.018637258840045, 237.3905034661050024 ) ) ;
#90416 = CARTESIAN_POINT ( 'NONE',  ( 15.45910333959999861, 1409.623955960430067, 270.0849031534979758 ) ) ;
#90417 = CARTESIAN_POINT ( 'NONE',  ( 3.461047291624999911, 1516.858765657450249, 212.5691103191969944 ) ) ;
#90418 = CARTESIAN_POINT ( 'NONE',  ( -60.14896982169999973, 1379.725317057869916, 261.7476106778590292 ) ) ;
#90419 = B_SPLINE_CURVE_WITH_KNOTS ( 'NONE', 3,
 ( #32067, #15245, #31507, #58384, #49437, #75736, #109880, #33160, #24736, #65687, #91432, #14708, #58933, #48897, #93065, #83024, #47775, #5214, #34819, #110426, #77386, #52196, #35938, #103110, #86325 ),
 .UNSPECIFIED., .F., .F.,
 ( 4, 3, 3, 3, 3, 3, 3, 3, 4 ),
 ( -1.000000000000000000, -0.8761102852806710306, -0.6239390062907779200, -0.3603953910640009806, -0.09086183696110827768, 0.1830679867661229032, 0.4571305125683509107, 0.7297053856717570230, 0.9999610272373291586 ),
 .UNSPECIFIED. ) ;
#90420 = CARTESIAN_POINT ( 'NONE',  ( 22.82103900350000103, 1409.709957859030055, 209.1787568684370058 ) ) ;
#90421 = FACE_OUTER_BOUND ( 'NONE', #11594, .T. ) ;
#90422 = CARTESIAN_POINT ( 'NONE',  ( 17.68711869539999881, 1428.828027849089949, 204.9896315466789929 ) ) ;
#90425 = EDGE_CURVE ( 'NONE', #82045, #94134, #682, .T. ) ;
#90424 = CARTESIAN_POINT ( 'NONE',  ( -7.709487050242899819, 1516.551695078709827, 211.8815864275139802 ) ) ;
#90423 = CIRCLE ( 'NONE', #24240, 33.13701971169416538 ) ;
#90426 = CARTESIAN_POINT ( 'NONE',  ( -6.933587693644999383, 1516.542957540330008, 210.8312046333570038 ) ) ;
#90427 = EDGE_CURVE ( 'NONE', #76272, #102730, #45836, .T. ) ;
#90428 = CARTESIAN_POINT ( 'NONE',  ( 0.1674519188599999930, 1419.793575726829886, 184.3767552697979966 ) ) ;
#90429 = CARTESIAN_POINT ( 'NONE',  ( 6.061196268494501105, 1422.611301504031417, 137.0999999981671635 ) ) ;
#90430 = ADVANCED_FACE ( 'NONE', ( #67761 ), #76694, .F. ) ;
#90432 = ORIENTED_EDGE ( 'NONE', *, *, #15951, .F. ) ;
#90431 = CARTESIAN_POINT ( 'NONE',  ( -43.53222241470000142, 1389.577826452589989, 221.0279022753590255 ) ) ;
#90433 = CARTESIAN_POINT ( 'NONE',  ( -34.27198354733999963, 1385.212855379749953, 233.1604131954400145 ) ) ;
#90434 = CARTESIAN_POINT ( 'NONE',  ( 30.31644210120071747, 1523.530870145310473, 195.7504609407426983 ) ) ;
#90435 = EDGE_CURVE ( 'NONE', #56546, #28026, #81900, .T. ) ;
#90436 = CARTESIAN_POINT ( 'NONE',  ( 0.7436338729729999875, 1415.853947014629966, 233.3108650019980246 ) ) ;
#90437 = ADVANCED_FACE ( 'NONE', ( #72191 ), #81416, .F. ) ;
#90438 = VECTOR ( 'NONE', #25278, 1000.000000000000000 ) ;
#90439 = CARTESIAN_POINT ( 'NONE',  ( 7.599227146160510316, 1512.341036968809931, 206.8869228877400133 ) ) ;
#90440 = CARTESIAN_POINT ( 'NONE',  ( 12.09917978440000041, 1426.493404676209821, 204.7338120852189718 ) ) ;
#90441 = CARTESIAN_POINT ( 'NONE',  ( 0.5706190868331736388, 1498.604900413591395, 197.8127445519372429 ) ) ;
#90442 = EDGE_CURVE ( 'NONE', #36663, #86690, #71237, .T. ) ;
#90444 = CARTESIAN_POINT ( 'NONE',  ( 21.84020450211271225, 1523.481610118012213, 183.2638850456620219 ) ) ;
#90443 = CARTESIAN_POINT ( 'NONE',  ( 2.873958851594999864, 1516.588006113850042, 216.0563744999969913 ) ) ;
#90445 = LINE ( 'NONE', #5906, #94297 ) ;
#90446 = CARTESIAN_POINT ( 'NONE',  ( 10.43242597914977665, 1423.400858002167979, 137.2800370846200337 ) ) ;
#90447 = EDGE_LOOP ( 'NONE', ( #49340, #105453, #5350, #41160, #66564 ) ) ;
#90448 = CARTESIAN_POINT ( 'NONE',  ( -5.005071046424999892, 1516.710692850270107, 201.7963041449669959 ) ) ;
#90449 = CARTESIAN_POINT ( 'NONE',  ( -15.18044686046500047, 1511.791180387469922, 220.8782529452670076 ) ) ;
#90450 = VERTEX_POINT ( 'NONE', #63247 ) ;
#90451 = DIRECTION ( 'NONE',  ( 1.776356839400250465E-15, 0.000000000000000000, 1.000000000000000000 ) ) ;
#90452 = CARTESIAN_POINT ( 'NONE',  ( 20.34226454299999887, 1454.597587043530211, 225.1509561457980340 ) ) ;
#90453 = CARTESIAN_POINT ( 'NONE',  ( 10.86847934145580119, 1461.672329020349935, 210.6140132405090242 ) ) ;
#90454 = CARTESIAN_POINT ( 'NONE',  ( 9.085958642259313933, 1425.096540595445731, 195.6575571040253578 ) ) ;
#90455 = ADVANCED_FACE ( 'NONE', ( #78926 ), #2771, .T. ) ;
#90456 = CARTESIAN_POINT ( 'NONE',  ( 1.049495711600000103, 1442.456986865990075, 218.6426261805090121 ) ) ;
#90457 = CARTESIAN_POINT ( 'NONE',  ( 16.63417907921860106, 1421.797052956256721, 227.0536667165849849 ) ) ;
#90458 = B_SPLINE_CURVE_WITH_KNOTS ( 'NONE', 5,
 ( #33026, #57718, #76146, #109211, #16749, #23525 ),
 .UNSPECIFIED., .F., .F.,
 ( 6, 6 ),
 ( -2.000000000000000000, 0.000000000000000000 ),
 .UNSPECIFIED. ) ;
#90459 = CARTESIAN_POINT ( 'NONE',  ( -2.499999995990000112, 1447.656584094229856, 165.9523979493980050 ) ) ;
#90460 = CARTESIAN_POINT ( 'NONE',  ( -20.07368861760000200, 1427.190829891029807, 224.4645657875979907 ) ) ;
#90461 = CARTESIAN_POINT ( 'NONE',  ( 8.332914826467142433, 1487.564149926648042, 202.1864945295145333 ) ) ;
#90462 = CARTESIAN_POINT ( 'NONE',  ( -105.5834716709999981, 1391.919560845880142, 303.0663598160589913 ) ) ;
#90463 = CARTESIAN_POINT ( 'NONE',  ( 18.62849171730000108, 1498.094182759829891, 188.8234950878980101 ) ) ;
#90465 = CARTESIAN_POINT ( 'NONE',  ( -18.52077958148023029, 1436.768619839807798, 212.6474277558114636 ) ) ;
#90464 = CARTESIAN_POINT ( 'NONE',  ( 0.2881515426530549817, 1409.862531727490023, 233.1990202907039986 ) ) ;
#90466 = EDGE_CURVE ( 'NONE', #57273, #6602, #97957, .T. ) ;
#90467 = CARTESIAN_POINT ( 'NONE',  ( -35.00793662113747473, 1457.766281221113786, 269.5316643497311020 ) ) ;
#90468 = ORIENTED_EDGE ( 'NONE', *, *, #71913, .F. ) ;
#90469 = CARTESIAN_POINT ( 'NONE',  ( 19.52205342210000083, 1473.076230373790168, 204.3554439105789982 ) ) ;
#90470 = CARTESIAN_POINT ( 'NONE',  ( -16.45895393019999986, 1508.541852756190110, 213.5615360674089800 ) ) ;
#90471 = DIRECTION ( 'NONE',  ( 1.836970198721029688E-16, 1.000000000000000000, 0.000000000000000000 ) ) ;
#90472 = EDGE_CURVE ( 'NONE', #86613, #3072, #70031, .T. ) ;
#90473 = CARTESIAN_POINT ( 'NONE',  ( 9.490649882959999672, 1424.812065698590004, 209.0802308740339868 ) ) ;
#90474 = CARTESIAN_POINT ( 'NONE',  ( -15.28420222199999934, 1497.713060387329961, 224.4060481839979957 ) ) ;
#90475 = CARTESIAN_POINT ( 'NONE',  ( 1.454962978634650073, 1500.859017483070147, 181.3861282941270190 ) ) ;
#90476 = CARTESIAN_POINT ( 'NONE',  ( -32.38845791999504797, 1523.382868172864164, 202.1182848005516348 ) ) ;
#90477 = CARTESIAN_POINT ( 'NONE',  ( -12.91165256927668992, 1442.897813290883278, 186.4311288414393175 ) ) ;
#90478 = CARTESIAN_POINT ( 'NONE',  ( 2.566893074593609807E-08, 1406.911841303630126, 196.1218459607310081 ) ) ;
#90479 = DIRECTION ( 'NONE',  ( 0.000000000000000000, 1.000000000000000000, 0.000000000000000000 ) ) ;
#90480 = ADVANCED_FACE ( 'NONE', ( #108513 ), #46611, .T. ) ;
#90481 = DIRECTION ( 'NONE',  ( 0.000000000000000000, 1.000000000000000000, 0.000000000000000000 ) ) ;
#90482 = AXIS2_PLACEMENT_3D ( 'NONE', #72539, #49000, #89873 ) ;
#90483 = CARTESIAN_POINT ( 'NONE',  ( -15.03565728386930012, 1415.677402202029953, 207.5762112621430049 ) ) ;
#90484 = CARTESIAN_POINT ( 'NONE',  ( 23.95468325570000090, 1435.352574582540001, 137.1777079961979950 ) ) ;
#90485 = CARTESIAN_POINT ( 'NONE',  ( 6.048624176389999718, 1428.948518799289786, 215.4589177655589936 ) ) ;
#90487 = ORIENTED_EDGE ( 'NONE', *, *, #18138, .T. ) ;
#90486 = CARTESIAN_POINT ( 'NONE',  ( 29.86461515634920971, 1525.960063244517187, 220.9690070206020494 ) ) ;
#90488 = DIRECTION ( 'NONE',  ( -1.755985294532469921E-16, 1.000000000000000000, -1.338183447452831989E-16 ) ) ;
#90489 = CARTESIAN_POINT ( 'NONE',  ( 12.85932411630730066, 1512.319979277509901, 224.2899601613300149 ) ) ;
#90490 = ORIENTED_EDGE ( 'NONE', *, *, #62431, .F. ) ;
#90491 = ORIENTED_EDGE ( 'NONE', *, *, #28433, .F. ) ;
#90492 = CARTESIAN_POINT ( 'NONE',  ( -11.89756941249999933, 1501.968939201889953, 209.9094283132900216 ) ) ;
#90493 = CARTESIAN_POINT ( 'NONE',  ( -7.722580352405000070, 1517.051704408389924, 207.5526846776770071 ) ) ;
#90495 = CARTESIAN_POINT ( 'NONE',  ( -32.03901054920000036, 1451.703008381130076, 250.0966427714979545 ) ) ;
#90494 = CARTESIAN_POINT ( 'NONE',  ( 35.97184424755489829, 1425.113701170736931, 269.5449737053726267 ) ) ;
#90496 = CARTESIAN_POINT ( 'NONE',  ( -19.96856953369999843, 1506.518496045629945, 189.0102800763980042 ) ) ;
#90497 = CARTESIAN_POINT ( 'NONE',  ( -11.23122559239999951, 1433.609634981740101, 151.5769196124979885 ) ) ;
#90498 = CARTESIAN_POINT ( 'NONE',  ( 3.827327205999999649, 1422.542708386029972, 168.6405287067979941 ) ) ;
#90499 = CARTESIAN_POINT ( 'NONE',  ( -19.39146514529999976, 1486.028937747929831, 189.8083660822979937 ) ) ;
#90500 = CARTESIAN_POINT ( 'NONE',  ( -13.80543374319990058, 1434.979599778060219, 148.5369743065390082 ) ) ;
#90501 = PLANE ( 'NONE',  #64320 ) ;
#90502 = CARTESIAN_POINT ( 'NONE',  ( -0.1829789114686829754, 1515.156771665009956, 213.4488861885569975 ) ) ;
#90503 = CARTESIAN_POINT ( 'NONE',  ( -14.72576942166499947, 1512.123542805230272, 221.3115653187670091 ) ) ;
#90504 = CARTESIAN_POINT ( 'NONE',  ( -11.39145936318320018, 1480.805290751239909, 212.2135522325029910 ) ) ;
#90505 = CARTESIAN_POINT ( 'NONE',  ( 3.879721387549549760, 1362.649618568975711, 208.3718459617061285 ) ) ;
#90506 = CARTESIAN_POINT ( 'NONE',  ( -11.01313281335095873, 1509.422798596149732, 237.0272438081198345 ) ) ;
#90507 = EDGE_CURVE ( 'NONE', #39464, #20284, #48613, .T. ) ;
#90508 = AXIS2_PLACEMENT_3D ( 'NONE', #59051, #93172, #84768 ) ;
#90510 = VERTEX_POINT ( 'NONE', #83858 ) ;
#90509 = CARTESIAN_POINT ( 'NONE',  ( 8.938783782526350941E-09, 1406.490650553919977, 266.0111486438349857 ) ) ;
#90511 = ORIENTED_EDGE ( 'NONE', *, *, #4812, .T. ) ;
#90512 = CARTESIAN_POINT ( 'NONE',  ( -12.25782077130000047, 1504.418297784690139, 208.6334560855260065 ) ) ;
#90513 = EDGE_CURVE ( 'NONE', #75598, #73362, #110716, .T. ) ;
#90514 = CARTESIAN_POINT ( 'NONE',  ( -21.45746880365630105, 1505.229108085560028, 215.8103938400879827 ) ) ;
#90515 = CARTESIAN_POINT ( 'NONE',  ( -13.52613638759999937, 1472.406022870030029, 270.2585879644979627 ) ) ;
#90516 = CARTESIAN_POINT ( 'NONE',  ( -11.71397076299980000, 1489.483175994190105, 212.5377881273170146 ) ) ;
#90517 = CARTESIAN_POINT ( 'NONE',  ( 3.229222591820000154, 1433.444289491620111, 155.4497426196979859 ) ) ;
#90518 = CARTESIAN_POINT ( 'NONE',  ( 34.55890087717340009, 1451.246761928099886, 135.9292514245820200 ) ) ;
#90519 = CARTESIAN_POINT ( 'NONE',  ( 4.327610416713549846, 1515.134996992909919, 209.7706221774439825 ) ) ;
#90520 = CARTESIAN_POINT ( 'NONE',  ( -7.243607538500000054, 1479.647667750989967, 210.0496944616339761 ) ) ;
#90521 = CARTESIAN_POINT ( 'NONE',  ( 10.02498596419820132, 1468.967489302699960, 208.7758262183099873 ) ) ;
#90522 = CARTESIAN_POINT ( 'NONE',  ( -4.281982111149999604, 1457.235994440989771, 217.6311433004889864 ) ) ;
#90523 = CARTESIAN_POINT ( 'NONE',  ( 11.15430180702570517, 1364.260116606875727, 210.6218459617030021 ) ) ;
#90524 = CARTESIAN_POINT ( 'NONE',  ( -29.10623605396180125, 1413.506399245979992, 268.1222045722540201 ) ) ;
#90525 = VERTEX_POINT ( 'NONE', #94447 ) ;
#90526 = FACE_OUTER_BOUND ( 'NONE', #80946, .T. ) ;
#90527 = EDGE_LOOP ( 'NONE', ( #95797, #74334, #94803 ) ) ;
#90528 = ORIENTED_EDGE ( 'NONE', *, *, #71923, .T. ) ;
#90529 = CARTESIAN_POINT ( 'NONE',  ( -4.608021707265000266, 1516.660388280709867, 210.8351633799069873 ) ) ;
#90530 = EDGE_CURVE ( 'NONE', #48829, #60488, #73993, .T. ) ;
#90531 = CARTESIAN_POINT ( 'NONE',  ( 33.82133213608769751, 1444.740067931810017, 154.8032509060861912 ) ) ;
#90533 = CARTESIAN_POINT ( 'NONE',  ( -17.64534983439791915, 1419.607322530220472, 207.0962554418724153 ) ) ;
#90532 = CARTESIAN_POINT ( 'NONE',  ( -3.446942109845000157, 1516.842852731759876, 212.3891375753969726 ) ) ;
#90534 = CARTESIAN_POINT ( 'NONE',  ( -6.133587857060000204, 1455.443851699130164, 185.1190063763980049 ) ) ;
#90535 = CARTESIAN_POINT ( 'NONE',  ( -2.080511716054991744, 1450.122691195282641, 182.8668332015829208 ) ) ;
#90536 = ORIENTED_EDGE ( 'NONE', *, *, #36956, .F. ) ;
#90537 = CARTESIAN_POINT ( 'NONE',  ( -26.28380303640000193, 1435.415400226489737, 135.3026382325979853 ) ) ;
#90538 = CARTESIAN_POINT ( 'NONE',  ( 1.710012720495000194, 1517.232977404109988, 201.3945188173769907 ) ) ;
#90539 = EDGE_CURVE ( 'NONE', #18256, #21199, #18065, .T. ) ;
#90540 = DIRECTION ( 'NONE',  ( -0.7067635638050681068, 0.03085854333205623190, -0.7067764959171910499 ) ) ;
#90541 = CARTESIAN_POINT ( 'NONE',  ( -12.94448954231350868, 1512.413060387330006, 185.4271167906579478 ) ) ;
#90542 = CARTESIAN_POINT ( 'NONE',  ( -41.23699424981570161, 1431.252039966480197, 270.0532253150080351 ) ) ;
#90543 = FACE_OUTER_BOUND ( 'NONE', #1506, .T. ) ;
#90544 = CARTESIAN_POINT ( 'NONE',  ( 0.07152419878080000515, 1397.597829884029807, 196.1220380877979892 ) ) ;
#90545 = EDGE_CURVE ( 'NONE', #100973, #71414, #86070, .T. ) ;
#90547 = ORIENTED_EDGE ( 'NONE', *, *, #56189, .T. ) ;
#90546 = CARTESIAN_POINT ( 'NONE',  ( -8.989161040693090854, 1364.724223069021491, 207.6218459616988241 ) ) ;
#90548 = EDGE_LOOP ( 'NONE', ( #26025, #15897, #79408 ) ) ;
#90549 = CARTESIAN_POINT ( 'NONE',  ( 0.2777695833849999629, 1451.683731431829756, 183.0558775174980042 ) ) ;
#90550 = CARTESIAN_POINT ( 'NONE',  ( -29.55269881708357715, 1525.821544997590763, 221.1141083160998448 ) ) ;
#90551 = CARTESIAN_POINT ( 'NONE',  ( -9.123736379228210680, 1384.508619151900120, 199.9712811155520171 ) ) ;
#90552 = CARTESIAN_POINT ( 'NONE',  ( -2.500000000000000000, 1419.383211070329935, 144.0964026338980091 ) ) ;
#90553 = CARTESIAN_POINT ( 'NONE',  ( -0.03226023477341029982, 1410.297896964309984, 185.0217421575940193 ) ) ;
#90554 = CARTESIAN_POINT ( 'NONE',  ( 1.135898785685000023, 1516.958737650239982, 210.2414381519470226 ) ) ;
#90555 = CARTESIAN_POINT ( 'NONE',  ( -68.74502848580000602, 1379.747981523659973, 280.1360247429590231 ) ) ;
#90556 = CARTESIAN_POINT ( 'NONE',  ( 2.746150429200790111, 1440.068830608010103, 157.5210337837320083 ) ) ;
#90557 = CARTESIAN_POINT ( 'NONE',  ( 7.619397864431079803, 1439.068296834260082, 213.8493076897310061 ) ) ;
#90558 = CARTESIAN_POINT ( 'NONE',  ( 11.59504266670000128, 1415.140114704729967, 222.7749241790980079 ) ) ;
#90559 = EDGE_CURVE ( 'NONE', #2539, #60200, #67260, .T. ) ;
#90560 = CARTESIAN_POINT ( 'NONE',  ( 12.09590736490000040, 1445.294669480289940, 186.8687466626980154 ) ) ;
#90561 = CARTESIAN_POINT ( 'NONE',  ( 6.548200587644999793, 1516.632821972880038, 207.9912384682270101 ) ) ;
#90562 = ORIENTED_EDGE ( 'NONE', *, *, #15514, .T. ) ;
#90563 = CARTESIAN_POINT ( 'NONE',  ( -40.71747596209480236, 1438.773003613870060, 135.0584847165220026 ) ) ;
#90564 = CARTESIAN_POINT ( 'NONE',  ( -22.46490035622105452, 1451.676372061169559, 219.5715471896962185 ) ) ;
#90565 = ORIENTED_EDGE ( 'NONE', *, *, #25315, .F. ) ;
#90566 = CARTESIAN_POINT ( 'NONE',  ( 6.714078785831339324, 1456.768705330869352, 227.7987839437156765 ) ) ;
#90567 = EDGE_CURVE ( 'NONE', #94251, #24298, #64695, .T. ) ;
#90568 = CARTESIAN_POINT ( 'NONE',  ( -5.606087537083091377, 1484.450325178786443, 199.4839161291210416 ) ) ;
#90569 = CARTESIAN_POINT ( 'NONE',  ( 13.35004134540000109, 1415.296882282229944, 197.1179729259980036 ) ) ;
#90570 = CARTESIAN_POINT ( 'NONE',  ( -9.093469788365199591, 1384.772129490919951, 199.9460114921000127 ) ) ;
#90571 = CARTESIAN_POINT ( 'NONE',  ( 21.56891374070000111, 1409.666263453530291, 206.3502062819679850 ) ) ;
#90572 = CARTESIAN_POINT ( 'NONE',  ( 16.66257059149999975, 1410.427173608229850, 226.4839827083980026 ) ) ;
#90573 = CARTESIAN_POINT ( 'NONE',  ( 11.59735442540000072, 1491.204275857490074, 206.7872505231089804 ) ) ;
#90574 = CARTESIAN_POINT ( 'NONE',  ( -118.5497409066653773, 1306.913060387289988, 301.4085296778973202 ) ) ;
#90575 = CARTESIAN_POINT ( 'NONE',  ( 23.34191689203280973, 1449.544838690270126, 217.2362966351278430 ) ) ;
#90576 = ADVANCED_FACE ( 'NONE', ( #95025 ), #97225, .T. ) ;
#90577 = CARTESIAN_POINT ( 'NONE',  ( 2.500000000000039968, 1439.311174638779903, 160.3626073483409868 ) ) ;
#90578 = CARTESIAN_POINT ( 'NONE',  ( 2.485845998894999909, 1516.545806094630279, 216.4433018439569878 ) ) ;
#90579 = ORIENTED_EDGE ( 'NONE', *, *, #34447, .T. ) ;
#90580 = CARTESIAN_POINT ( 'NONE',  ( 7.716234671763589681, 1516.809374097749924, 208.6912322278259921 ) ) ;
#90581 = CARTESIAN_POINT ( 'NONE',  ( -4.504196618690000875, 1474.524975280490025, 198.6118189482990033 ) ) ;
#90582 = CARTESIAN_POINT ( 'NONE',  ( -2.500000000000000000, 1448.919575512349866, 183.6707651433980004 ) ) ;
#90583 = EDGE_CURVE ( 'NONE', #109869, #74855, #65861, .T. ) ;
#90584 = ADVANCED_FACE ( 'NONE', ( #71527 ), #20616, .F. ) ;
#90585 = VECTOR ( 'NONE', #94090, 1000.000000000000114 ) ;
#90586 = DIRECTION ( 'NONE',  ( -0.000000000000000000, -1.000000000000000000, -0.000000000000000000 ) ) ;
#90587 =( BOUNDED_CURVE ( )  B_SPLINE_CURVE ( 3, ( #103088, #103661, #26959, #11272 ),
 .UNSPECIFIED., .F., .F. ) 
 B_SPLINE_CURVE_WITH_KNOTS ( ( 4, 4 ),
 ( 4.712388980384689674, 6.283185307179586232 ),
 .UNSPECIFIED. ) 
 CURVE ( )  GEOMETRIC_REPRESENTATION_ITEM ( )  RATIONAL_B_SPLINE_CURVE ( ( 1.000000000000000000, 0.8047378541243649375, 0.8047378541243649375, 1.000000000000000000 ) ) 
 REPRESENTATION_ITEM ( '' )  );
#90588 = CARTESIAN_POINT ( 'NONE',  ( 0.8033873907879990339, 1473.261709371789948, 219.3248484348989962 ) ) ;
#90589 = CARTESIAN_POINT ( 'NONE',  ( 11.60004869885197110, 1426.057405506147461, 138.8677241012580907 ) ) ;
#90590 = CYLINDRICAL_SURFACE ( 'NONE', #65743, 2.000000000000000000 ) ;
#90591 = CARTESIAN_POINT ( 'NONE',  ( 17.80628076561068340, 1423.588752249659819, 226.0326016818666233 ) ) ;
#90592 = CARTESIAN_POINT ( 'NONE',  ( -105.0581303879369983, 1379.236400313860031, 304.0328620142400382 ) ) ;
#90593 = CARTESIAN_POINT ( 'NONE',  ( -21.84020450211325937, 1523.481610118012441, 183.2638850456619366 ) ) ;
#90594 = CARTESIAN_POINT ( 'NONE',  ( 30.04265233421849857, 1440.913060385890049, 238.4851536875560214 ) ) ;
#90595 = CARTESIAN_POINT ( 'NONE',  ( -10.14352525432950003, 1472.500047657160167, 210.0566532823200134 ) ) ;
#90596 = CARTESIAN_POINT ( 'NONE',  ( 10.55744888006389992, 1501.358431704350096, 204.5464156931330137 ) ) ;
#90597 = ORIENTED_EDGE ( 'NONE', *, *, #12098, .F. ) ;
#90598 = ORIENTED_EDGE ( 'NONE', *, *, #82087, .F. ) ;
#90599 = EDGE_CURVE ( 'NONE', #22353, #100464, #41842, .T. ) ;
#90600 = CARTESIAN_POINT ( 'NONE',  ( 10.92990887285729862, 1479.841612654799974, 208.5736869255739805 ) ) ;
#90601 = CARTESIAN_POINT ( 'NONE',  ( -19.09820918671905332, 1485.515190164787555, 189.6361271261989714 ) ) ;
#90602 = CARTESIAN_POINT ( 'NONE',  ( -3.753656485510000085, 1441.439124929289846, 201.1135183436689999 ) ) ;
#90603 = CARTESIAN_POINT ( 'NONE',  ( 7.443252959589999662, 1423.092343121310023, 195.6161912809990326 ) ) ;
#90604 = CARTESIAN_POINT ( 'NONE',  ( 3.313501335607582643, 1397.551704408390151, 215.1871694724064810 ) ) ;
#90605 = EDGE_CURVE ( 'NONE', #8681, #39550, #36497, .T. ) ;
#90606 = CARTESIAN_POINT ( 'NONE',  ( 15.10371975099999986, 1409.440493903229935, 192.9533947891980006 ) ) ;
#90607 = FACE_OUTER_BOUND ( 'NONE', #275, .T. ) ;
#90608 = CARTESIAN_POINT ( 'NONE',  ( -42.86424717262820394, 1383.823646364319757, 247.0049435532770019 ) ) ;
#90609 = CARTESIAN_POINT ( 'NONE',  ( -4.491283723408599826, 1508.884229729929757, 206.6339223154620015 ) ) ;
#90610 = CARTESIAN_POINT ( 'NONE',  ( 5.360860135257599524, 1422.261831586439939, 143.3181667732210087 ) ) ;
#90611 = CARTESIAN_POINT ( 'NONE',  ( -5.385523200472070116, 1511.435001055929888, 200.4690698413500058 ) ) ;
#90612 = CARTESIAN_POINT ( 'NONE',  ( 1.615419329660000125, 1466.293469222530121, 234.8241805934979993 ) ) ;
#90614 = ORIENTED_EDGE ( 'NONE', *, *, #18175, .F. ) ;
#90613 = CARTESIAN_POINT ( 'NONE',  ( -17.17241001986462123, 1512.187213306747481, 238.6251415217917895 ) ) ;
#90615 = CARTESIAN_POINT ( 'NONE',  ( -0.3241128057579999999, 1452.022536283230238, 183.1062973747980038 ) ) ;
#90616 = CARTESIAN_POINT ( 'NONE',  ( -20.42369457250000053, 1378.928569551019791, 210.5700358550290048 ) ) ;
#90617 = CARTESIAN_POINT ( 'NONE',  ( 3.301717781941579943, 1508.551704408389924, 204.2711418796440057 ) ) ;
#90619 = ORIENTED_EDGE ( 'NONE', *, *, #14901, .T. ) ;
#90618 = CARTESIAN_POINT ( 'NONE',  ( -17.57493253053520021, 1415.090956648730071, 208.0895966506530215 ) ) ;
#90620 = CARTESIAN_POINT ( 'NONE',  ( 4.803826041432978755, 1471.771558818840049, 187.6888330202939983 ) ) ;
#90621 = ORIENTED_EDGE ( 'NONE', *, *, #83639, .T. ) ;
#90622 = CARTESIAN_POINT ( 'NONE',  ( -12.02121513377869988, 1389.043580930620010, 215.7482713796579787 ) ) ;
#90623 = CARTESIAN_POINT ( 'NONE',  ( -2.956827888069649912, 1515.222544093250008, 204.7977243774139993 ) ) ;
#90624 = CARTESIAN_POINT ( 'NONE',  ( -5.062212390315069754, 1474.342205398819942, 198.8731691453010058 ) ) ;
#90625 = CARTESIAN_POINT ( 'NONE',  ( -11.60004869885203860, 1426.752153102204375, 134.4009884339467931 ) ) ;
#90626 = CARTESIAN_POINT ( 'NONE',  ( -104.5162234509999877, 1380.028246613130023, 301.8403285842589412 ) ) ;
#90627 = CARTESIAN_POINT ( 'NONE',  ( 4.270716320241006336, 1515.320037165009126, 211.4519800868023083 ) ) ;
#90628 = CARTESIAN_POINT ( 'NONE',  ( 3.350338079455597917, 1523.604703353109699, 242.0808062845893289 ) ) ;
#90629 = CYLINDRICAL_SURFACE ( 'NONE', #89691, 9.999999999999992895 ) ;
#90630 = CARTESIAN_POINT ( 'NONE',  ( 18.28845792193000364, 1425.324260404669985, 225.4739065078200042 ) ) ;
#90631 = DIRECTION ( 'NONE',  ( -0.6709778558543766369, 0.000000000000000000, -0.7414773880254632576 ) ) ;
#90632 = FACE_OUTER_BOUND ( 'NONE', #4142, .T. ) ;
#90633 = CARTESIAN_POINT ( 'NONE',  ( -24.04659120089169733, 1444.796772349889807, 212.0316830080810178 ) ) ;
#90634 = B_SPLINE_CURVE_WITH_KNOTS ( 'NONE', 5,
 ( #13621, #82516, #108256, #73017, #30448, #56767 ),
 .UNSPECIFIED., .F., .F.,
 ( 6, 6 ),
 ( 0.000000000000000000, 1.000000000000000000 ),
 .UNSPECIFIED. ) ;
#90635 = CARTESIAN_POINT ( 'NONE',  ( -4.161598017608739930, 1448.982982409190072, 185.0801973001829879 ) ) ;
#90636 = EDGE_LOOP ( 'NONE', ( #40704, #45566 ) ) ;
#90637 = ORIENTED_EDGE ( 'NONE', *, *, #21709, .F. ) ;
#90638 = CARTESIAN_POINT ( 'NONE',  ( 31.23437356469446868, 1518.913060387330006, 221.8968241038843701 ) ) ;
#90639 = CARTESIAN_POINT ( 'NONE',  ( 18.80348473439820012, 1458.103780993950068, 227.2192783789020041 ) ) ;
#90640 = CARTESIAN_POINT ( 'NONE',  ( -12.47168581320000058, 1435.763300496210150, 150.9715321517980158 ) ) ;
#90641 = CARTESIAN_POINT ( 'NONE',  ( 2.842584659965070124E-10, 1465.638316924609853, 240.1326368917110301 ) ) ;
#90642 = CARTESIAN_POINT ( 'NONE',  ( -20.59684415639999955, 1507.762623716630060, 190.3921826403979765 ) ) ;
#90643 = CARTESIAN_POINT ( 'NONE',  ( -15.50787399150000034, 1420.315084950680102, 211.2763647146890094 ) ) ;
#90644 = CARTESIAN_POINT ( 'NONE',  ( -109.0249265700000052, 1386.996120149900207, 310.9016331512590341 ) ) ;
#90645 = CARTESIAN_POINT ( 'NONE',  ( -8.602963518122210829, 1511.535621886429908, 214.8679164923370024 ) ) ;
#90646 = CARTESIAN_POINT ( 'NONE',  ( -10.84079470823281000, 1361.963018199176304, 209.6218459617033432 ) ) ;
#90647 = CARTESIAN_POINT ( 'NONE',  ( -45.87688764550289733, 1440.254748464500153, 266.4125321213890061 ) ) ;
#90648 = CARTESIAN_POINT ( 'NONE',  ( 2.857353854284549577, 1525.661275128775742, 177.1476418759443163 ) ) ;
#90649 = CARTESIAN_POINT ( 'NONE',  ( -4.044319925355000400, 1517.073005577650065, 208.0013022344469960 ) ) ;
#90650 = CARTESIAN_POINT ( 'NONE',  ( -9.189592411000269578, 1448.419325144910090, 210.4171903414359974 ) ) ;
#90651 = B_SPLINE_CURVE_WITH_KNOTS ( 'NONE', 5,
 ( #97078, #98157, #20344, #71363, #55089, #55641, #21972, #28207, #104922 ),
 .UNSPECIFIED., .F., .F.,
 ( 6, 3, 6 ),
 ( 0.000000000000000000, 0.2390991004796381159, 1.000000000000000000 ),
 .UNSPECIFIED. ) ;
#90652 = CARTESIAN_POINT ( 'NONE',  ( 3.870734350961310355, 1407.691698232470117, 221.6993045718820099 ) ) ;
#90653 = CARTESIAN_POINT ( 'NONE',  ( -13.12797199115260227, 1435.680278977339867, 150.5510888193360017 ) ) ;
#90654 = VECTOR ( 'NONE', #70099, 1000.000000000000114 ) ;
#90655 = LINE ( 'NONE', #78004, #46311 ) ;
#90656 = CARTESIAN_POINT ( 'NONE',  ( 8.320723051859999941, 1424.406562835429895, 91.09139192869778867 ) ) ;
#90657 = CARTESIAN_POINT ( 'NONE',  ( 6.992375725325399749, 1424.886399156210018, 213.2204113455599952 ) ) ;
#90658 = EDGE_LOOP ( 'NONE', ( #29026, #56447, #61734, #12318 ) ) ;
#90659 = CARTESIAN_POINT ( 'NONE',  ( 24.64758684659999943, 1426.171069948330114, 240.2509105673979946 ) ) ;
#90660 = CARTESIAN_POINT ( 'NONE',  ( -28.07142279760000037, 1508.133443487129853, 207.7742737906680190 ) ) ;
#90662 = CYLINDRICAL_SURFACE ( 'NONE', #50425, 0.9999999999999976685 ) ;
#90661 = CARTESIAN_POINT ( 'NONE',  ( -3.541507727459999977, 1499.396715322330010, 181.3063315952979906 ) ) ;
#90663 = CARTESIAN_POINT ( 'NONE',  ( 20.74431190377872269, 1506.539416727910066, 201.5807876387586077 ) ) ;
#90664 = CARTESIAN_POINT ( 'NONE',  ( -4.374510219029999369, 1418.297051469029839, 231.7760247135979910 ) ) ;
#90665 = CARTESIAN_POINT ( 'NONE',  ( 21.03036721537930376, 1456.985417876070187, 226.1578115872349883 ) ) ;
#90666 = CARTESIAN_POINT ( 'NONE',  ( -7.429844844193369546, 1452.653604488170004, 151.4931312769679721 ) ) ;
#90667 = CARTESIAN_POINT ( 'NONE',  ( -18.79678650740000023, 1416.830000968129980, 208.4086244650179935 ) ) ;
#90668 = ORIENTED_EDGE ( 'NONE', *, *, #11999, .T. ) ;
#90669 = CARTESIAN_POINT ( 'NONE',  ( -5.359834938588759812, 1422.451238776880018, 146.6367341849590105 ) ) ;
#90670 = CARTESIAN_POINT ( 'NONE',  ( 11.74132753969999854, 1499.920429264490167, 205.7525976432890218 ) ) ;
#90671 = CARTESIAN_POINT ( 'NONE',  ( 15.88607233163610211, 1422.777081491979970, 229.6788727262410248 ) ) ;
#90672 = CARTESIAN_POINT ( 'NONE',  ( 11.33291839610000018, 1501.995980221090122, 207.2411316382289783 ) ) ;
#90673 = ORIENTED_EDGE ( 'NONE', *, *, #102049, .F. ) ;
#90674 = ORIENTED_EDGE ( 'NONE', *, *, #66723, .F. ) ;
#90675 = CARTESIAN_POINT ( 'NONE',  ( -10.36554740068187108, 1423.171634364120564, 137.2136980898112313 ) ) ;
#90676 = CARTESIAN_POINT ( 'NONE',  ( -23.56284583309999903, 1410.013091502230054, 209.4388942478690012 ) ) ;
#90677 = CARTESIAN_POINT ( 'NONE',  ( -3.775288954430000121, 1424.836333284029934, 185.8533989989979887 ) ) ;
#90678 = CARTESIAN_POINT ( 'NONE',  ( 4.115882519823130359, 1509.032029208890208, 204.7576547855990157 ) ) ;
#90679 = AXIS2_PLACEMENT_3D ( 'NONE', #22506, #63489, #20879 ) ;
#90680 = CARTESIAN_POINT ( 'NONE',  ( -15.22835610959999997, 1415.677402202029953, 206.7258912741390020 ) ) ;
#90681 = CARTESIAN_POINT ( 'NONE',  ( -15.23964492230000012, 1498.344222354329986, 230.9699155403980058 ) ) ;
#90682 = CARTESIAN_POINT ( 'NONE',  ( 16.73628186595829703, 1526.382868172864164, 234.1845039693042452 ) ) ;
#90683 = ORIENTED_EDGE ( 'NONE', *, *, #36631, .T. ) ;
#90684 = CARTESIAN_POINT ( 'NONE',  ( 45.92877942503140076, 1443.730784468270031, 266.6808678471329586 ) ) ;
#90685 = CARTESIAN_POINT ( 'NONE',  ( -12.50317167495700055, 1415.933499560010205, 221.8717862475229765 ) ) ;
#90686 = CARTESIAN_POINT ( 'NONE',  ( -0.2148604818640000025, 1419.222391940929811, 184.6498075250980264 ) ) ;
#90687 = CARTESIAN_POINT ( 'NONE',  ( -7.335901033725000353, 1517.068717944079935, 205.0869373723870126 ) ) ;
#90688 = VERTEX_POINT ( 'NONE', #39532 ) ;
#90689 = CARTESIAN_POINT ( 'NONE',  ( 10.39781522345580100, 1481.413011136829937, 214.7151440750830034 ) ) ;
#90690 = CARTESIAN_POINT ( 'NONE',  ( 13.46741876155364359, 1443.580133104905826, 187.9916346024478457 ) ) ;
#90691 = ORIENTED_EDGE ( 'NONE', *, *, #20066, .T. ) ;
#90692 = VERTEX_POINT ( 'NONE', #30011 ) ;
#90693 = CARTESIAN_POINT ( 'NONE',  ( 3.406450987864870328, 1507.508084575899829, 220.3277226881679951 ) ) ;
#90694 = ADVANCED_FACE ( 'NONE', ( #13748 ), #107279, .F. ) ;
#90695 = CARTESIAN_POINT ( 'NONE',  ( -30.90487439922522483, 1525.907212628473872, 216.4335774778785151 ) ) ;
#90696 = CARTESIAN_POINT ( 'NONE',  ( -13.58541698226610173, 1512.759354980439866, 193.8094473928580044 ) ) ;
#90697 = CARTESIAN_POINT ( 'NONE',  ( 9.593413928111729660, 1452.578050990920019, 150.7562495203559934 ) ) ;
#90698 = EDGE_CURVE ( 'NONE', #82691, #49611, #101914, .T. ) ;
#90699 = CARTESIAN_POINT ( 'NONE',  ( -1.664499176201119805E-05, 1409.781082070230013, 270.0713786264859664 ) ) ;
#90700 = CARTESIAN_POINT ( 'NONE',  ( 1.407091184820499885, 1474.938609241890163, 220.4531082379680242 ) ) ;
#90701 = CARTESIAN_POINT ( 'NONE',  ( 19.07040306792730888, 1456.402085735674746, 225.8083803216468084 ) ) ;
#90702 = CARTESIAN_POINT ( 'NONE',  ( -10.97972313751300177, 1432.951242176940013, 151.7695334411729959 ) ) ;
#90703 = CARTESIAN_POINT ( 'NONE',  ( 0.03404606575480032676, 1410.028338985503296, 233.1847745296862513 ) ) ;
#90705 = CARTESIAN_POINT ( 'NONE',  ( -105.7715901379339982, 1391.141931180460006, 306.3730337667240065 ) ) ;
#90704 = CARTESIAN_POINT ( 'NONE',  ( -2.198507585695390212E-07, 1408.626123741879837, 268.3915997536489613 ) ) ;
#90706 = TOROIDAL_SURFACE ( 'NONE', #42432, 32.13701971169416538, 1.000000000000000000 ) ;
#90707 = CARTESIAN_POINT ( 'NONE',  ( 12.36845973521560005, 1427.047203898280031, 206.6331761361700217 ) ) ;
#90708 = EDGE_CURVE ( 'NONE', #100027, #81793, #28566, .T. ) ;
#90709 = CARTESIAN_POINT ( 'NONE',  ( -9.773688900458409989, 1440.083893828079908, 206.9335397354529960 ) ) ;
#90710 = B_SPLINE_CURVE_WITH_KNOTS ( 'NONE', 3,
 ( #589, #9513, #87906, #11195, #18442, #68907 ),
 .UNSPECIFIED., .F., .F.,
 ( 4, 2, 4 ),
 ( 0.000000000000000000, 0.5000000000000000000, 1.000000000000000000 ),
 .UNSPECIFIED. ) ;
#90711 = CARTESIAN_POINT ( 'NONE',  ( 11.79165762230000070, 1429.416862815430022, 146.4064176768980019 ) ) ;
#90712 = EDGE_LOOP ( 'NONE', ( #71751, #53000, #3766, #81990, #95613 ) ) ;
#90713 = CARTESIAN_POINT ( 'NONE',  ( 19.02913997119999934, 1436.609546585119915, 214.3676144198679765 ) ) ;
#90714 = DIRECTION ( 'NONE',  ( 4.336808689942001466E-16, -0.02617694830786544691, 0.9996573249755575929 ) ) ;
#90715 = AXIS2_PLACEMENT_3D ( 'NONE', #59521, #86356, #178 ) ;
#90716 = CARTESIAN_POINT ( 'NONE',  ( -77.89391513553759694, 1384.999643260920038, 302.3909578806699869 ) ) ;
#90717 = EDGE_CURVE ( 'NONE', #96418, #78070, #24363, .T. ) ;
#90718 = CARTESIAN_POINT ( 'NONE',  ( -8.508434771949998421, 1386.782168888490105, 200.0040007541689988 ) ) ;
#90719 = CARTESIAN_POINT ( 'NONE',  ( 10.14664409362030106, 1422.547896506549932, 210.8756393921580070 ) ) ;
#90721 = VERTEX_POINT ( 'NONE', #67508 ) ;
#90720 = CARTESIAN_POINT ( 'NONE',  ( 11.02200761809709917, 1424.480284645659822, 203.1122766956139856 ) ) ;
#90722 = CARTESIAN_POINT ( 'NONE',  ( 4.085147076609999317, 1428.826406437490050, 216.3215770461389980 ) ) ;
#90723 = CARTESIAN_POINT ( 'NONE',  ( -0.8348477807080000312, 1443.913060387330006, 150.8032249175980155 ) ) ;
#90724 = CARTESIAN_POINT ( 'NONE',  ( -16.77180262980000336, 1417.238431246169966, 208.0779775581890192 ) ) ;
#90725 = CARTESIAN_POINT ( 'NONE',  ( -13.31089767776890120, 1503.456584347970193, 208.6977459380580058 ) ) ;
#90726 = CARTESIAN_POINT ( 'NONE',  ( 11.49747572422220188, 1414.913060387329779, 220.3427040978150160 ) ) ;
#90727 = CARTESIAN_POINT ( 'NONE',  ( 13.15726446870029953, 1414.972329067380088, 197.7171628163160051 ) ) ;
#90728 =( BOUNDED_CURVE ( )  B_SPLINE_CURVE ( 3, ( #62727, #71115, #11728, #71683 ),
 .UNSPECIFIED., .F., .T. ) 
 B_SPLINE_CURVE_WITH_KNOTS ( ( 4, 4 ),
 ( 1.013149129984646013, 2.128443654157999632 ),
 .UNSPECIFIED. ) 
 CURVE ( )  GEOMETRIC_REPRESENTATION_ITEM ( )  RATIONAL_B_SPLINE_CURVE ( ( 1.000000000000000000, 0.8990016712204955684, 0.8990016712204955684, 1.000000000000000000 ) ) 
 REPRESENTATION_ITEM ( '' )  );
#90729 = CARTESIAN_POINT ( 'NONE',  ( 8.562022419562680398, 1436.588812126380162, 208.1472598823880276 ) ) ;
#90730 = CARTESIAN_POINT ( 'NONE',  ( 31.81407709660769001, 1512.187213306747481, 196.2902540610627682 ) ) ;
#90731 = CARTESIAN_POINT ( 'NONE',  ( 10.96771871715767155, 1512.594959757391052, 225.0393121556896290 ) ) ;
#90732 = CARTESIAN_POINT ( 'NONE',  ( -19.90023153800419564, 1526.278758871496166, 235.2784539741628578 ) ) ;
#90733 = CARTESIAN_POINT ( 'NONE',  ( 1.959285284397550120, 1474.800623515119923, 220.3715842348549927 ) ) ;
#90734 = CARTESIAN_POINT ( 'NONE',  ( -17.32164063149999933, 1410.015194788730014, 225.5041473358979829 ) ) ;
#90735 = AXIS2_PLACEMENT_3D ( 'NONE', #50946, #34129, #554 ) ;
#90737 = ADVANCED_FACE ( 'NONE', ( #8117 ), #3694, .T. ) ;
#90736 = EDGE_CURVE ( 'NONE', #41530, #75664, #84371, .T. ) ;
#90738 = CARTESIAN_POINT ( 'NONE',  ( -4.922266137120000273, 1497.746000166390104, 220.5680551797990177 ) ) ;
#90739 = CYLINDRICAL_SURFACE ( 'NONE', #62161, 2.000000000000001776 ) ;
#90740 = FACE_OUTER_BOUND ( 'NONE', #70928, .T. ) ;
#90741 = CARTESIAN_POINT ( 'NONE',  ( 21.83550407203906119, 1523.678648413191468, 183.2743720722706655 ) ) ;
#90742 = CARTESIAN_POINT ( 'NONE',  ( 1.491125504899999843, 1515.528285129289998, 205.0771167131389916 ) ) ;
#90743 = CARTESIAN_POINT ( 'NONE',  ( 12.56817824281639950, 1426.998444030340124, 206.1059456672400074 ) ) ;
#90744 = CARTESIAN_POINT ( 'NONE',  ( -8.886125802571559262, 1432.346591486940042, 153.1913712024140182 ) ) ;
#90745 = EDGE_CURVE ( 'NONE', #96193, #98249, #109294, .T. ) ;
#90746 = CARTESIAN_POINT ( 'NONE',  ( -1.387158262170000045, 1415.426952351230057, 227.4696213630980139 ) ) ;
#90747 = DIRECTION ( 'NONE',  ( -1.000000000000000000, 0.000000000000000000, 0.000000000000000000 ) ) ;
#90748 = CARTESIAN_POINT ( 'NONE',  ( -13.32225628249999971, 1409.200806412430211, 203.4621145805880076 ) ) ;
#90749 = CARTESIAN_POINT ( 'NONE',  ( -17.25136325379999747, 1416.823872462129884, 202.8337460093080153 ) ) ;
#90750 = CARTESIAN_POINT ( 'NONE',  ( -28.49243283392089765, 1509.649079667319938, 211.1281934096199961 ) ) ;
#90751 = CARTESIAN_POINT ( 'NONE',  ( 11.87541216019999979, 1433.006892857880075, 148.5014493308979979 ) ) ;
#90752 = CARTESIAN_POINT ( 'NONE',  ( -28.14147886860000369, 1436.374928695000108, 136.6909279132979975 ) ) ;
#90753 = CARTESIAN_POINT ( 'NONE',  ( -4.390466737189999691, 1449.947854720489886, 190.5483265708990075 ) ) ;
#90754 = ORIENTED_EDGE ( 'NONE', *, *, #17967, .T. ) ;
#90755 = CARTESIAN_POINT ( 'NONE',  ( -1.637258856660000150, 1483.893433971690001, 198.5669146070989939 ) ) ;
#90756 = CARTESIAN_POINT ( 'NONE',  ( -4.758677794462281341, 1427.076634120264089, 137.0999999980979567 ) ) ;
#90757 = CARTESIAN_POINT ( 'NONE',  ( -104.0156867654433057, 1380.207460468658610, 306.5247186736235108 ) ) ;
#90758 = CARTESIAN_POINT ( 'NONE',  ( -11.59964767839999844, 1491.341587614589798, 206.7829318209490168 ) ) ;
#90759 = CARTESIAN_POINT ( 'NONE',  ( 21.97938480441199971, 1506.433683733499947, 208.7396655020440051 ) ) ;
#90760 = CARTESIAN_POINT ( 'NONE',  ( 13.87299426750780107, 1509.389572371919940, 234.2955350557650149 ) ) ;
#90761 = AXIS2_PLACEMENT_3D ( 'NONE', #89923, #90471, #12116 ) ;
#90762 = CARTESIAN_POINT ( 'NONE',  ( 40.50390548520631029, 1425.157017824941704, 269.1155397953845636 ) ) ;
#90763 = CARTESIAN_POINT ( 'NONE',  ( 8.405796826027030377, 1426.718799454960163, 211.2874649559879856 ) ) ;
#90764 = CARTESIAN_POINT ( 'NONE',  ( 31.41104781486823327, 1511.187213306747708, 215.9140555522422460 ) ) ;
#90765 = CARTESIAN_POINT ( 'NONE',  ( 2.500000015409999943, 1439.638673630699941, 183.2818205602979731 ) ) ;
#90766 = CARTESIAN_POINT ( 'NONE',  ( -52.24432420902090257, 1385.027339147369958, 228.9037425557689858 ) ) ;
#90767 = CARTESIAN_POINT ( 'NONE',  ( -16.87900699709518193, 1524.382868172804365, 237.0109764097493326 ) ) ;
#90768 = CARTESIAN_POINT ( 'NONE',  ( -4.878845441898269186, 1508.551704408389924, 205.9013857386030111 ) ) ;
#90769 = CARTESIAN_POINT ( 'NONE',  ( -27.52167012590000184, 1451.951932214330100, 134.9033768147980084 ) ) ;
#90770 = CARTESIAN_POINT ( 'NONE',  ( -15.99309461030230040, 1409.852751965980133, 226.2723575830249843 ) ) ;
#90772 = ORIENTED_EDGE ( 'NONE', *, *, #44085, .T. ) ;
#90771 = CARTESIAN_POINT ( 'NONE',  ( 1.766195777250000098, 1508.139388919589919, 217.9383592619290084 ) ) ;
#90773 = DIRECTION ( 'NONE',  ( 0.3363363926273127968, -0.9417419131558525391, -2.375999277009924068E-08 ) ) ;
#90774 = CARTESIAN_POINT ( 'NONE',  ( 11.27533154505640134, 1471.493970385359944, 211.0173010655499866 ) ) ;
#90775 = CARTESIAN_POINT ( 'NONE',  ( 18.11996117484120106, 1430.141981561779858, 211.0753063895589889 ) ) ;
#90776 = CARTESIAN_POINT ( 'NONE',  ( -109.3084789200000131, 1384.717857449120174, 311.2599033892590228 ) ) ;
#90777 = CARTESIAN_POINT ( 'NONE',  ( -0.1321314129836040074, 1420.447759805389978, 182.9787002574440180 ) ) ;
#90778 = CARTESIAN_POINT ( 'NONE',  ( 1.010913760600000044, 1465.039206930530099, 236.8418874943980086 ) ) ;
#90779 = CARTESIAN_POINT ( 'NONE',  ( 23.03460887469999818, 1411.077649166529909, 213.3831903349580159 ) ) ;
#90780 = DIRECTION ( 'NONE',  ( -0.3596128954806624978, -0.9141289860956119950, -0.1872078048154584839 ) ) ;
#90781 = CARTESIAN_POINT ( 'NONE',  ( -20.45337306669999933, 1467.535200901489816, 211.3000096380390005 ) ) ;
#90782 = CARTESIAN_POINT ( 'NONE',  ( -17.64330431710000013, 1423.732166419529904, 226.4225726569979997 ) ) ;
#90784 = FACE_OUTER_BOUND ( 'NONE', #102508, .T. ) ;
#90783 = CARTESIAN_POINT ( 'NONE',  ( -3.864359895900485231, 1511.505225070758115, 200.9696564112188923 ) ) ;
#90785 = CARTESIAN_POINT ( 'NONE',  ( 26.64849719969200237, 1469.324131025480028, 209.0880383046890074 ) ) ;
#90786 = CARTESIAN_POINT ( 'NONE',  ( -128.5457199608244139, 1340.114449826971168, 295.9477014321976753 ) ) ;
#90787 = CARTESIAN_POINT ( 'NONE',  ( -1732.234191736389675, 11221.53578756870047, -1992.291823225089274 ) ) ;
#90788 = CARTESIAN_POINT ( 'NONE',  ( -23.42267346790000104, 1430.824238628630155, 212.0368849710979759 ) ) ;
#90789 = VECTOR ( 'NONE', #13879, 1000.000000000000000 ) ;
#90790 = CARTESIAN_POINT ( 'NONE',  ( -5.243603173628749836, 1374.986671669950056, 203.4237121730149909 ) ) ;
#90791 = CARTESIAN_POINT ( 'NONE',  ( 1.702754371344999962, 1517.014196759610059, 205.6580786742169948 ) ) ;
#90792 = CARTESIAN_POINT ( 'NONE',  ( -3.324249965575039933, 1484.702398424410148, 183.3514200912059664 ) ) ;
#90793 = ORIENTED_EDGE ( 'NONE', *, *, #100062, .F. ) ;
#90794 = DIRECTION ( 'NONE',  ( -0.8907681516580484571, 1.273087901431153894E-31, 0.4544580288560254311 ) ) ;
#90795 = CARTESIAN_POINT ( 'NONE',  ( -4.222047166393189777, 1441.600308170239941, 167.9930962660010039 ) ) ;
#90798 = ORIENTED_EDGE ( 'NONE', *, *, #68643, .T. ) ;
#90797 = CARTESIAN_POINT ( 'NONE',  ( -68.07780588669999133, 1379.747638516110101, 279.5234925687589680 ) ) ;
#90796 = AXIS2_PLACEMENT_3D ( 'NONE', #62895, #36533, #37081 ) ;
#90799 = VERTEX_POINT ( 'NONE', #26006 ) ;
#90800 = CARTESIAN_POINT ( 'NONE',  ( -17.31663237150539558, 1423.877172976356860, 228.8047162730268838 ) ) ;
#90801 = ORIENTED_EDGE ( 'NONE', *, *, #17302, .F. ) ;
#90802 = VECTOR ( 'NONE', #12036, 1000.000000000000000 ) ;
#90803 = CARTESIAN_POINT ( 'NONE',  ( 7.817147020270110325, 1507.298329231454545, 182.8873992028549651 ) ) ;
#90804 = CARTESIAN_POINT ( 'NONE',  ( 12.22918170280000005, 1500.524921488590053, 208.3556390005750245 ) ) ;
#90806 = CARTESIAN_POINT ( 'NONE',  ( 16.06732615789859508, 1409.482374878060000, 192.8457122857769832 ) ) ;
#90805 = CARTESIAN_POINT ( 'NONE',  ( -11.74384639166921218, 1426.275853339841206, 144.6945198498246725 ) ) ;
#90807 = CARTESIAN_POINT ( 'NONE',  ( 6.563915523884999992, 1517.184063036290127, 210.2461356256870033 ) ) ;
#90808 = CARTESIAN_POINT ( 'NONE',  ( 33.92724809123075858, 1436.576393223097966, 136.5094752661439657 ) ) ;
#90809 = CARTESIAN_POINT ( 'NONE',  ( -14.29934916198160089, 1379.719590493410124, 208.2697206714749996 ) ) ;
#90810 = CARTESIAN_POINT ( 'NONE',  ( 12.44780704128189974, 1501.268281525590055, 211.7240718234590133 ) ) ;
#90811 = SHAPE_DEFINITION_REPRESENTATION ( #73286, #105979 ) ;
#90812 = CARTESIAN_POINT ( 'NONE',  ( 38.37377460181989619, 1450.184294006789969, 134.0999999983419855 ) ) ;
#90813 = DIRECTION ( 'NONE',  ( -0.000000000000000000, -1.000000000000000000, -0.000000000000000000 ) ) ;
#90814 = ORIENTED_EDGE ( 'NONE', *, *, #1747, .F. ) ;
#90815 = CARTESIAN_POINT ( 'NONE',  ( -0.03315026662488079756, 1502.038609099889982, 233.2541149014899986 ) ) ;
#90816 = CARTESIAN_POINT ( 'NONE',  ( -2.134964941497456969, 1389.913060387289988, 210.4225860197314830 ) ) ;
#90817 = ORIENTED_EDGE ( 'NONE', *, *, #13025, .F. ) ;
#90818 = ORIENTED_EDGE ( 'NONE', *, *, #2988, .T. ) ;
#90819 = CARTESIAN_POINT ( 'NONE',  ( -6.126746181595000174, 1514.923664147150021, 217.2480802176870043 ) ) ;
#90820 = CARTESIAN_POINT ( 'NONE',  ( 16.58691039599694150, 1514.105081323590866, 194.9569398562394724 ) ) ;
#90821 = CARTESIAN_POINT ( 'NONE',  ( -0.03576358831780000053, 1452.355416418630057, 183.2659201527980031 ) ) ;
#90822 = VECTOR ( 'NONE', #33469, 1000.000000000000114 ) ;
#90823 = CARTESIAN_POINT ( 'NONE',  ( -3.156350064089999741, 1484.702381841229908, 183.3290672668979937 ) ) ;
#90824 = CARTESIAN_POINT ( 'NONE',  ( -2.500000000000000000, 1439.547542131649834, 164.8613965946329927 ) ) ;
#90825 = CARTESIAN_POINT ( 'NONE',  ( -3.347801439371857146, 1523.456924617337108, 242.0893193391915474 ) ) ;
#90826 = CARTESIAN_POINT ( 'NONE',  ( 38.81202645930000017, 1436.797832437240231, 134.0999985825980332 ) ) ;
#90827 = CARTESIAN_POINT ( 'NONE',  ( -3.034926079678203159, 1369.200812461396481, 210.6218459616991936 ) ) ;
#90828 = FACE_OUTER_BOUND ( 'NONE', #23202, .T. ) ;
#90829 = FACE_OUTER_BOUND ( 'NONE', #81506, .T. ) ;
#90830 = CARTESIAN_POINT ( 'NONE',  ( -80.12204894687070578, 1384.794894040560166, 283.2630655434839468 ) ) ;
#90831 = ORIENTED_EDGE ( 'NONE', *, *, #89059, .F. ) ;
#90832 = CARTESIAN_POINT ( 'NONE',  ( 4.487249753806469954, 1509.038615938009798, 205.6342535008409982 ) ) ;
#90833 = CARTESIAN_POINT ( 'NONE',  ( 1.704170714124999986, 1516.927039499179955, 208.3639196453299860 ) ) ;
#90834 = ORIENTED_EDGE ( 'NONE', *, *, #72040, .T. ) ;
#90835 = CARTESIAN_POINT ( 'NONE',  ( 33.89753131429299771, 1440.913060387330006, 259.1515849714069759 ) ) ;
#90836 = CARTESIAN_POINT ( 'NONE',  ( -0.0002035883165944741776, 1452.365207701825739, 153.7261367825575178 ) ) ;
#90837 = ORIENTED_EDGE ( 'NONE', *, *, #104085, .F. ) ;
#90838 = CARTESIAN_POINT ( 'NONE',  ( 0.05421983196053539733, 1451.175530199109971, 182.5313573697069955 ) ) ;
#90839 = CARTESIAN_POINT ( 'NONE',  ( -16.66257565289999931, 1410.427174256630224, 191.7597267753979793 ) ) ;
#90840 = CARTESIAN_POINT ( 'NONE',  ( -109.1111611177930030, 1384.583257041720117, 311.2497810013429671 ) ) ;
#90841 = CARTESIAN_POINT ( 'NONE',  ( -10.76391066127440155, 1462.897227275840123, 206.5781441640729952 ) ) ;
#90842 = CARTESIAN_POINT ( 'NONE',  ( 21.13431379670319998, 1409.651086887829933, 206.4149708788170301 ) ) ;
#90843 = CARTESIAN_POINT ( 'NONE',  ( -10.16240527536719895, 1472.558926193989919, 209.8189312950259762 ) ) ;
#90844 = CARTESIAN_POINT ( 'NONE',  ( -1.449529204450000108, 1508.614376975429877, 180.2799702684980048 ) ) ;
#90845 = CARTESIAN_POINT ( 'NONE',  ( -6.123056464990721537, 1510.784366232218872, 201.6446126835382131 ) ) ;
#90846 = CARTESIAN_POINT ( 'NONE',  ( -22.41686883764639759, 1524.667648926078755, 181.9773018742353372 ) ) ;
#90848 = CARTESIAN_POINT ( 'NONE',  ( -11.60004869886543410, 1424.050231871397045, 137.1752122141798225 ) ) ;
#90847 = CARTESIAN_POINT ( 'NONE',  ( 12.94229023090000119, 1461.456462053329915, 233.4393938603979848 ) ) ;
#90849 = CARTESIAN_POINT ( 'NONE',  ( -0.3402596924234728704, 1410.306538769425742, 233.2121123280315942 ) ) ;
#90850 = CARTESIAN_POINT ( 'NONE',  ( 1.129386202275000084, 1516.613712827999962, 216.4452363774470030 ) ) ;
#90851 = ORIENTED_EDGE ( 'NONE', *, *, #77435, .T. ) ;
#90852 = CARTESIAN_POINT ( 'NONE',  ( -0.4586520875518777518, 1486.396701128719542, 181.7766115271735714 ) ) ;
#90853 = B_SPLINE_CURVE_WITH_KNOTS ( 'NONE', 3,
 ( #41782, #42335, #92731, #7080, #17093, #16006, #33924, #110639, #76487, #75937 ),
 .UNSPECIFIED., .F., .F.,
 ( 4, 2, 2, 2, 4 ),
 ( 0.000000000000000000, 0.0007403986298595332041, 0.001480797259719066408, 0.002221195889578599612, 0.002961594519438132816 ),
 .UNSPECIFIED. ) ;
#90854 = CARTESIAN_POINT ( 'NONE',  ( -0.1511123393328930031, 1507.449223653020226, 180.8591688853359756 ) ) ;
#90855 = EDGE_CURVE ( 'NONE', #52731, #1004, #2045, .T. ) ;
#90856 = CARTESIAN_POINT ( 'NONE',  ( 2.428364288097684565, 1516.533847659095727, 216.8308657282840954 ) ) ;
#90857 = CARTESIAN_POINT ( 'NONE',  ( 5.011367946795000528, 1516.974592746400049, 212.5716232859570027 ) ) ;
#90858 = CARTESIAN_POINT ( 'NONE',  ( 3.983717799493539324, 1515.551844914359890, 211.4517850689670126 ) ) ;
#90859 = CARTESIAN_POINT ( 'NONE',  ( -116.0327476856711257, 1378.813060387289852, 302.7835693414463663 ) ) ;
#90861 = ORIENTED_EDGE ( 'NONE', *, *, #42023, .F. ) ;
#90860 = CARTESIAN_POINT ( 'NONE',  ( 3.487585849221220169, 1508.611352722540005, 213.7999951158270164 ) ) ;
#90862 = LINE ( 'NONE', #100372, #28105 ) ;
#90863 = CARTESIAN_POINT ( 'NONE',  ( 20.68004892169999920, 1453.350765365529924, 221.6396287865980241 ) ) ;
#90864 = ADVANCED_FACE ( 'NONE', ( #93230 ), #85017, .F. ) ;
#90865 = CARTESIAN_POINT ( 'NONE',  ( -11.84725155179999945, 1430.949263877939984, 150.2388512889980063 ) ) ;
#90866 = DIRECTION ( 'NONE',  ( 0.000000000000000000, 1.000000000000000000, 0.000000000000000000 ) ) ;
#90867 = CARTESIAN_POINT ( 'NONE',  ( -5.750181936253229154, 1442.413653245499972, 201.3643156640750078 ) ) ;
#90868 = CARTESIAN_POINT ( 'NONE',  ( 9.330551562259142173, 1426.784206974829885, 151.9956406576650352 ) ) ;
#90869 = VECTOR ( 'NONE', #66536, 1000.000000000000000 ) ;
#90870 = CARTESIAN_POINT ( 'NONE',  ( 12.59633922020000085, 1445.148044568509931, 187.0941081104979844 ) ) ;
#90872 = CARTESIAN_POINT ( 'NONE',  ( -10.20774725584609932, 1481.348133439640151, 206.3586384583620088 ) ) ;
#90871 = CARTESIAN_POINT ( 'NONE',  ( -20.34050849710000008, 1457.444417593830167, 224.6898825346980288 ) ) ;
#90873 = DIRECTION ( 'NONE',  ( -0.5877852522924785772, 0.000000000000000000, 0.8090169943749434545 ) ) ;
#90874 = EDGE_LOOP ( 'NONE', ( #33653, #99343, #3480, #9382 ) ) ;
#90876 = CIRCLE ( 'NONE', #99816, 2.000000000000003553 ) ;
#90875 = CARTESIAN_POINT ( 'NONE',  ( -0.01322039564809850132, 1516.939819969850078, 205.0847949345169923 ) ) ;
#90877 = CARTESIAN_POINT ( 'NONE',  ( 4.994452949999999447, 1405.913965673130178, 267.8435537567980305 ) ) ;
#90878 = CARTESIAN_POINT ( 'NONE',  ( 0.09447546337450000997, 1408.916359543229873, 186.4601785166979937 ) ) ;
#90879 = CIRCLE ( 'NONE', #31883, 1.000000000000000888 ) ;
#90880 = FACE_OUTER_BOUND ( 'NONE', #95782, .T. ) ;
#90881 = CARTESIAN_POINT ( 'NONE',  ( 23.62109726877421423, 1434.135449394258558, 214.7287868320940447 ) ) ;
#90882 = CARTESIAN_POINT ( 'NONE',  ( -0.6806208766845354141, 1463.451559807898320, 199.3558502068030407 ) ) ;
#90883 = CARTESIAN_POINT ( 'NONE',  ( -1.594806016870000009, 1450.591479615480011, 183.0618219514980183 ) ) ;
#90884 = EDGE_CURVE ( 'NONE', #78014, #72991, #423, .T. ) ;
#90885 = B_SPLINE_CURVE_WITH_KNOTS ( 'NONE', 3,
 ( #17338, #91870, #7320, #42029, #23558, #24635, #93512, #8966, #94069, #24095, #51532, #8404, #33600, #7862, #40, #41483, #34171, #75644, #92969, #16241, #31964, #50987, #15144, #59953, #109243, #110327, #100807, #50446, #84570, #25197, #58284, #92409, #109783, #76178, #49886, #67795, #101905, #85116, #42576, #20125, #95187, #36927, #104686, #1146, #593, #86226 ),
 .UNSPECIFIED., .F., .F.,
 ( 4, 3, 3, 3, 3, 3, 3, 3, 3, 3, 3, 3, 3, 3, 3, 4 ),
 ( -11.22311477689549974, -10.99415920655549961, -10.18995056570000024, -9.361206530017639693, -8.517487667444680000, -7.615611964294410008, -6.760125105125089462, -5.916206473942639654, -5.089590486009999637, -4.554350324856789811, -3.682921093262059742, -2.834315530205490319, -1.999665612459999409, -1.587483130849479451, -0.7852278221460000651, 0.000000000000000000 ),
 .UNSPECIFIED. ) ;
#90886 = CARTESIAN_POINT ( 'NONE',  ( -5.292981110492219976, 1440.702993122236194, 202.0789376815712899 ) ) ;
#90887 = CARTESIAN_POINT ( 'NONE',  ( -2.428387260106030343, 1449.547206808950023, 154.5200478772810015 ) ) ;
#90888 = CARTESIAN_POINT ( 'NONE',  ( -1.569676819536519385, 1450.891569726948546, 183.4696716048479459 ) ) ;
#90889 = CARTESIAN_POINT ( 'NONE',  ( -19.87804702706843685, 1485.311229468551801, 190.7217664356889486 ) ) ;
#90890 = CARTESIAN_POINT ( 'NONE',  ( -14.45750500688560081, 1416.828039245989885, 221.3916439204320170 ) ) ;
#90891 = CARTESIAN_POINT ( 'NONE',  ( -12.05448508470000135, 1501.734409265689919, 211.4994548164490027 ) ) ;
#90892 = CARTESIAN_POINT ( 'NONE',  ( -5.969073325650000150, 1428.313923095629889, 209.1218459616979999 ) ) ;
#90893 = B_SPLINE_CURVE_WITH_KNOTS ( 'NONE', 3,
 ( #34224, #103638, #85172, #8458, #50496, #77344, #76782, #77889, #7913, #76234, #100, #102513, #68409, #26935, #16837, #42084, #101963, #110380, #60561, #647, #94122, #25250, #9020, #15735, #51039, #43193, #34778, #68964, #103066, #94681, #52148, #86281, #9567, #43737, #84073, #45948, #2853, #54365, #46510, #53257, #70619, #36427, #19621, #104739, #104190, #63321, #53822, #89030, #97440, #105855, #28583, #71737, #80643, #27472, #87961 ),
 .UNSPECIFIED., .F., .F.,
 ( 4, 2, 2, 2, 1, 1, 1, 1, 2, 2, 2, 2, 1, 1, 1, 2, 2, 2, 1, 1, 1, 1, 2, 2, 2, 2, 2, 1, 1, 1, 1, 2, 2, 2, 4 ),
 ( 0.000000000000000000, 0.1249999999999774070, 0.1874999999999732714, 0.2187499999999759637, 0.2343749999999773515, 0.2421874999999807654, 0.2460937499999825417, 0.2480468749999878431, 0.2490234374999844291, 0.2499999999999810707, 0.3125000000001457723, 0.3437500000002332023, 0.3593750000002768896, 0.3671875000002988165, 0.3710937500003113065, 0.3730468750003188005, 0.3750000000003263501, 0.4375000000002042255, 0.4687500000001482148, 0.4843750000001165734, 0.4921875000001021960, 0.4960937500000987543, 0.4980468750001019740, 0.5000000000001052491, 0.6249999999999911182, 0.6874999999999353850, 0.7187499999999140687, 0.7343749999999044098, 0.7421874999998996358, 0.7460937499999017453, 0.7480468749999027445, 0.7490234374999034106, 0.7499999999999039657, 0.8749999999999519273, 1.000000000000000000 ),
 .UNSPECIFIED. ) ;
#90894 = B_SPLINE_CURVE_WITH_KNOTS ( 'NONE', 3,
 ( #41744, #84832, #110055, #41201 ),
 .UNSPECIFIED., .F., .F.,
 ( 4, 4 ),
 ( 0.000000000000000000, 1.000000000000000000 ),
 .UNSPECIFIED. ) ;
#90895 = CARTESIAN_POINT ( 'NONE',  ( 22.75273496409597485, 1512.187213306747481, 234.5707981297185825 ) ) ;
#90896 = CARTESIAN_POINT ( 'NONE',  ( 13.04207810306199988, 1409.368499790489750, 192.3005055522939983 ) ) ;
#90897 = CARTESIAN_POINT ( 'NONE',  ( -4.991737838419999740, 1475.878694619930002, 267.5267923144979818 ) ) ;
#90899 = CIRCLE ( 'NONE', #28325, 30.13701971169416183 ) ;
#90898 = DIRECTION ( 'NONE',  ( -0.7636119845522929550, -0.004098122786836628888, -0.6456624059349689304 ) ) ;
#90900 = DIRECTION ( 'NONE',  ( 0.000000000000000000, 0.000000000000000000, -1.000000000000000000 ) ) ;
#90901 = CARTESIAN_POINT ( 'NONE',  ( -11.21032122992201785, 1517.151704408390060, 229.8720270527158220 ) ) ;
#90902 = CARTESIAN_POINT ( 'NONE',  ( -43.62562285640520088, 1384.770753572229978, 248.8406183467260178 ) ) ;
#90903 = CARTESIAN_POINT ( 'NONE',  ( -106.7351624162349992, 1391.913060387289988, 302.3468487761870165 ) ) ;
#90904 = CARTESIAN_POINT ( 'NONE',  ( -0.5779273184081722414, 1519.551704408389924, 186.0802614738061607 ) ) ;
#90905 = CARTESIAN_POINT ( 'NONE',  ( 1.338019250827790163, 1431.361302059610125, 218.5179660117710227 ) ) ;
#90906 = CARTESIAN_POINT ( 'NONE',  ( -20.70484064406418412, 1525.907212628473644, 185.0411015109856692 ) ) ;
#90907 = CARTESIAN_POINT ( 'NONE',  ( 8.133924938042731867, 1511.520894735510410, 205.3152396615298585 ) ) ;
#90908 =( BOUNDED_CURVE ( )  B_SPLINE_CURVE ( 3, ( #95639, #96195, #37394, #44148 ),
 .UNSPECIFIED., .F., .F. ) 
 B_SPLINE_CURVE_WITH_KNOTS ( ( 4, 4 ),
 ( 6.251003116154824291, 6.262497214195333228 ),
 .UNSPECIFIED. ) 
 CURVE ( )  GEOMETRIC_REPRESENTATION_ITEM ( )  RATIONAL_B_SPLINE_CURVE ( ( 1.000000000000000000, 0.9999889905061551953, 0.9999889905061551953, 1.000000000000000000 ) ) 
 REPRESENTATION_ITEM ( '' )  );
#90909 = CARTESIAN_POINT ( 'NONE',  ( -18.08393550219999923, 1409.544565332530055, 197.0250912618979839 ) ) ;
#90910 = CARTESIAN_POINT ( 'NONE',  ( 12.82193333132650004, 1421.326950664900096, 205.6957921146359922 ) ) ;
#90911 = CARTESIAN_POINT ( 'NONE',  ( 19.28229067004766861, 1456.003485696241569, 225.1845458337684249 ) ) ;
#90912 = ORIENTED_EDGE ( 'NONE', *, *, #19692, .T. ) ;
#90913 = CARTESIAN_POINT ( 'NONE',  ( -2.642706046298320732, 1410.383226565404584, 232.6286052421928048 ) ) ;
#90914 = CARTESIAN_POINT ( 'NONE',  ( -13.59112270319939952, 1508.247351304150015, 209.6221426111970061 ) ) ;
#90915 = CARTESIAN_POINT ( 'NONE',  ( -9.573053049599600683, 1423.428031588070098, 192.3355779375469865 ) ) ;
#90917 = CARTESIAN_POINT ( 'NONE',  ( -15.36700635076499921, 1514.600163677630007, 193.5017378528669667 ) ) ;
#90916 = CARTESIAN_POINT ( 'NONE',  ( 10.74308370929999867, 1424.967654141830053, 139.6357132919980018 ) ) ;
#90918 = CARTESIAN_POINT ( 'NONE',  ( 16.85976061912576185, 1525.821544997590308, 236.1944305375346858 ) ) ;
#90919 = DIRECTION ( 'NONE',  ( 0.000000000000000000, 1.000000000000000000, 0.000000000000000000 ) ) ;
#90920 = CARTESIAN_POINT ( 'NONE',  ( -4.254366313090000240, 1454.573790823890022, 200.5971711135589999 ) ) ;
#90921 = CARTESIAN_POINT ( 'NONE',  ( -2.291676311554999845, 1516.534976163889951, 201.8006522243570089 ) ) ;
#90922 = CARTESIAN_POINT ( 'NONE',  ( 7.798665745000000982, 1426.844771716620244, 212.1118124881890026 ) ) ;
#90923 = CARTESIAN_POINT ( 'NONE',  ( -2.409586283469999923, 1426.663880916129983, 144.1938086916980239 ) ) ;
#90924 = CARTESIAN_POINT ( 'NONE',  ( 15.47073870303499987, 1511.939906524110256, 196.6289149681670096 ) ) ;
#90925 = CARTESIAN_POINT ( 'NONE',  ( -17.29057999663249845, 1420.088377186219759, 204.6564600065449895 ) ) ;
#90926 = CARTESIAN_POINT ( 'NONE',  ( 8.985389986235038126E-14, 1377.122490972250034, 211.4935542023889923 ) ) ;
#90927 = CARTESIAN_POINT ( 'NONE',  ( 21.91792290201540183, 1509.678451720530120, 227.8819227092559743 ) ) ;
#90929 = ORIENTED_EDGE ( 'NONE', *, *, #9658, .F. ) ;
#90928 = CARTESIAN_POINT ( 'NONE',  ( -19.20715834270519906, 1379.591600376749966, 212.8172136241779810 ) ) ;
#90930 = ORIENTED_EDGE ( 'NONE', *, *, #4296, .F. ) ;
#90931 = CARTESIAN_POINT ( 'NONE',  ( -5.776215096199999621, 1396.296062264229931, 198.6637670462979770 ) ) ;
#90932 = CARTESIAN_POINT ( 'NONE',  ( -21.01722066690000190, 1410.567592102230037, 218.3378942615279925 ) ) ;
#90933 = CARTESIAN_POINT ( 'NONE',  ( -5.779603138333690993, 1516.738222555248967, 201.4074744776068258 ) ) ;
#90934 = CARTESIAN_POINT ( 'NONE',  ( -12.73809752124026495, 1445.003929500445793, 169.4561374448583990 ) ) ;
#90935 = CARTESIAN_POINT ( 'NONE',  ( -25.23570363969999875, 1509.794310577129863, 194.6260395679979922 ) ) ;
#90936 = CARTESIAN_POINT ( 'NONE',  ( -7.891777524685001488, 1512.314860029340025, 212.0638756013070179 ) ) ;
#90938 = CARTESIAN_POINT ( 'NONE',  ( 17.60601737500000041, 1410.887304148830026, 224.8084147167980120 ) ) ;
#90937 = CARTESIAN_POINT ( 'NONE',  ( 0.7910245917146940808, 1426.918876941764893, 134.0999999980980135 ) ) ;
#90939 = B_SPLINE_CURVE_WITH_KNOTS ( 'NONE', 3,
 ( #57488, #82669, #32800, #67540 ),
 .UNSPECIFIED., .F., .F.,
 ( 4, 4 ),
 ( 0.000000000000000000, 1.000000000000000000 ),
 .UNSPECIFIED. ) ;
#90940 = CARTESIAN_POINT ( 'NONE',  ( -30.31644210120141381, 1523.530870145310473, 195.7504609407442615 ) ) ;
#90941 = CARTESIAN_POINT ( 'NONE',  ( -7.723894028380000165, 1416.216596894529857, 192.5579729901980102 ) ) ;
#90942 = CARTESIAN_POINT ( 'NONE',  ( -17.26926088820000160, 1417.734849473969916, 207.2874629064689884 ) ) ;
#90943 = CARTESIAN_POINT ( 'NONE',  ( 11.06592217088270047, 1396.299490904690174, 209.4166363852829988 ) ) ;
#90944 = CARTESIAN_POINT ( 'NONE',  ( 1.326919707080000066, 1414.988017870030035, 191.7691690602979691 ) ) ;
#90945 = CARTESIAN_POINT ( 'NONE',  ( 11.25166810410000018, 1428.703240696229841, 150.5458012123980041 ) ) ;
#90946 = CARTESIAN_POINT ( 'NONE',  ( 5.938657822353222038, 1509.124927619275013, 180.2982783801607525 ) ) ;
#90947 = ORIENTED_EDGE ( 'NONE', *, *, #1108, .T. ) ;
#90948 = CARTESIAN_POINT ( 'NONE',  ( 13.46829667242139905, 1436.161474321959986, 150.5249941659139949 ) ) ;
#90949 = CARTESIAN_POINT ( 'NONE',  ( 22.08622291482331690, 1523.456872492435195, 184.4183880513174927 ) ) ;
#90950 = ORIENTED_EDGE ( 'NONE', *, *, #52303, .T. ) ;
#90951 = VERTEX_POINT ( 'NONE', #72872 ) ;
#90952 = CARTESIAN_POINT ( 'NONE',  ( -16.76078030769999927, 1420.494757909599912, 203.1294657649889928 ) ) ;
#90953 = CARTESIAN_POINT ( 'NONE',  ( -14.92438935200000039, 1460.034730670430008, 231.4439065160979965 ) ) ;
#90954 = PRESENTATION_LAYER_ASSIGNMENT (  '', '', ( #74907 ) ) ;
#90955 = CARTESIAN_POINT ( 'NONE',  ( -13.49161259159999915, 1434.822352678170091, 195.9491175140979919 ) ) ;
#90956 = CARTESIAN_POINT ( 'NONE',  ( -4.034280953785000179, 1517.049325831759916, 216.0701676760970145 ) ) ;
#90957 = CARTESIAN_POINT ( 'NONE',  ( -12.63123455407130002, 1379.447564691009802, 208.9815245622429813 ) ) ;
#90958 = EDGE_LOOP ( 'NONE', ( #29503, #18862, #48141, #57472 ) ) ;
#90959 = FACE_OUTER_BOUND ( 'NONE', #72950, .T. ) ;
#90960 = CARTESIAN_POINT ( 'NONE',  ( 2.500000000000000000, 1448.534146728170072, 160.0811088377199951 ) ) ;
#90961 = CARTESIAN_POINT ( 'NONE',  ( -55.86512535760000020, 1379.936376805820146, 252.9328197421589834 ) ) ;
#90962 = AXIS2_PLACEMENT_3D ( 'NONE', #14000, #82325, #22943 ) ;
#90963 = CARTESIAN_POINT ( 'NONE',  ( 6.935133380425000382, 1516.613881697390070, 205.8602099992770036 ) ) ;
#90964 = ORIENTED_EDGE ( 'NONE', *, *, #15183, .F. ) ;
#90965 = CARTESIAN_POINT ( 'NONE',  ( -4.618583430005000601, 1516.939762005280045, 209.1349059721700030 ) ) ;
#90966 = CARTESIAN_POINT ( 'NONE',  ( -8.681250099826490541, 1451.825605612139952, 205.8309633687780149 ) ) ;
#90967 = CARTESIAN_POINT ( 'NONE',  ( -10.92882029718542825, 1411.379195557904040, 269.3492646456201669 ) ) ;
#90968 = CARTESIAN_POINT ( 'NONE',  ( 6.479185118354999773, 1511.503799556579906, 216.5023728028170069 ) ) ;
#90970 = ORIENTED_EDGE ( 'NONE', *, *, #43865, .T. ) ;
#90969 = CARTESIAN_POINT ( 'NONE',  ( -30.47387511496757639, 1525.394057003703438, 196.7420889653906215 ) ) ;
#90971 = CARTESIAN_POINT ( 'NONE',  ( -5.932239102140000497, 1391.413060387289988, 209.1218459572589836 ) ) ;
#90972 = CARTESIAN_POINT ( 'NONE',  ( -28.02863369646679814, 1440.913060388819986, 231.2731264215370004 ) ) ;
#90973 = CARTESIAN_POINT ( 'NONE',  ( -59.29940820010000380, 1384.093480151519998, 279.8903676332589612 ) ) ;
#90974 = CARTESIAN_POINT ( 'NONE',  ( -0.1290038325305789824, 1466.767347909359842, 235.6227026514060015 ) ) ;
#90975 = VECTOR ( 'NONE', #50222, 1000.000000000000000 ) ;
#90976 = CARTESIAN_POINT ( 'NONE',  ( 13.22859383683809931, 1410.662777231539849, 270.3663857566149886 ) ) ;
#90977 = CARTESIAN_POINT ( 'NONE',  ( -7.323974644434999348, 1516.647924054489977, 213.1579656147470132 ) ) ;
#90978 = CARTESIAN_POINT ( 'NONE',  ( 23.93604199780000030, 1410.398478142230033, 208.8934000136680140 ) ) ;
#90979 = CYLINDRICAL_SURFACE ( 'NONE', #55351, 1.463110112870021462 ) ;
#90980 = CARTESIAN_POINT ( 'NONE',  ( 12.10943595246970084, 1492.670318175190232, 211.5635330023629876 ) ) ;
#90981 = CARTESIAN_POINT ( 'NONE',  ( -11.60004869885203682, 1425.894669202444675, 137.5118601406020673 ) ) ;
#90982 = CARTESIAN_POINT ( 'NONE',  ( 7.726331925474999807, 1517.194972660189933, 211.4133602680070112 ) ) ;
#90983 = CARTESIAN_POINT ( 'NONE',  ( 4.254228409968599856, 1420.739899128549951, 185.5486331039510048 ) ) ;
#90984 = CARTESIAN_POINT ( 'NONE',  ( 0.1144970540559999972, 1419.768045047230089, 184.3728024650980046 ) ) ;
#90985 = CARTESIAN_POINT ( 'NONE',  ( -14.03738926715088020, 1486.050909705618778, 185.7519581601395373 ) ) ;
#90987 = ORIENTED_EDGE ( 'NONE', *, *, #17644, .T. ) ;
#90986 = CARTESIAN_POINT ( 'NONE',  ( -39.01488008110000294, 1388.283545533540064, 213.2677783093589881 ) ) ;
#90988 = CARTESIAN_POINT ( 'NONE',  ( -51.04972207953789365, 1385.115692561849983, 263.8849342485610237 ) ) ;
#90989 = CARTESIAN_POINT ( 'NONE',  ( 18.64672481350000055, 1416.851343894929869, 209.6839434898159880 ) ) ;
#90990 = CARTESIAN_POINT ( 'NONE',  ( -17.33645362950000290, 1414.996442546130083, 207.8511177337479978 ) ) ;
#90991 = CARTESIAN_POINT ( 'NONE',  ( -4.619855912889999416, 1417.833749415829971, 234.7627619328980018 ) ) ;
#90992 = FACE_OUTER_BOUND ( 'NONE', #33821, .T. ) ;
#90993 = CARTESIAN_POINT ( 'NONE',  ( 11.67793025129999940, 1421.804042185309982, 204.2098866971190034 ) ) ;
#90994 = CARTESIAN_POINT ( 'NONE',  ( 3.932771983779999925, 1448.980696587250122, 184.2693349551980191 ) ) ;
#90996 = DIRECTION ( 'NONE',  ( 0.000000000000000000, -1.000000000000000000, 0.000000000000000000 ) ) ;
#90995 = CARTESIAN_POINT ( 'NONE',  ( -6.553524415734999664, 1516.882690742909972, 216.0660777183969969 ) ) ;
#90997 = CARTESIAN_POINT ( 'NONE',  ( -26.24366108068827685, 1450.757924316903200, 136.5808154326949477 ) ) ;
#90998 = CARTESIAN_POINT ( 'NONE',  ( 11.13967540296130032, 1470.272324673559979, 206.9144120771860003 ) ) ;
#90999 = ORIENTED_EDGE ( 'NONE', *, *, #7669, .F. ) ;
#91000 = CARTESIAN_POINT ( 'NONE',  ( 4.616272296565000488, 1517.030858226499959, 201.7868885755270014 ) ) ;
#91001 = CARTESIAN_POINT ( 'NONE',  ( 10.46969661486759939, 1481.045827775979888, 207.7546358525030143 ) ) ;
#91002 = ORIENTED_EDGE ( 'NONE', *, *, #6527, .T. ) ;
#91003 = CARTESIAN_POINT ( 'NONE',  ( 0.08715897492290000659, 1457.824249707829949, 229.0178643556979807 ) ) ;
#91004 = CIRCLE ( 'NONE', #10608, 26.00000000000000711 ) ;
#91005 = CARTESIAN_POINT ( 'NONE',  ( 24.32474686429999977, 1445.057405757869901, 214.3193390981779771 ) ) ;
#91006 = CARTESIAN_POINT ( 'NONE',  ( 10.85999110878850082, 1461.697261943650119, 210.6766943065500186 ) ) ;
#91007 = CARTESIAN_POINT ( 'NONE',  ( 8.693632405113794093, 1424.753903042060301, 195.7638379925143965 ) ) ;
#91008 = CARTESIAN_POINT ( 'NONE',  ( 2.563330864020000099, 1442.944485697089931, 217.6409014154289991 ) ) ;
#91009 = CARTESIAN_POINT ( 'NONE',  ( 3.846235792629999928, 1440.870317293109792, 184.3772602386979997 ) ) ;
#91010 = CARTESIAN_POINT ( 'NONE',  ( 18.18716276245509889, 1472.405785144279889, 200.2358052267980213 ) ) ;
#91011 = CARTESIAN_POINT ( 'NONE',  ( -19.04818187609999924, 1425.840467097430064, 224.4548499685980119 ) ) ;
#91012 = CIRCLE ( 'NONE', #8756, 1.999999999999999556 ) ;
#91013 = CARTESIAN_POINT ( 'NONE',  ( 7.620481068300741789, 1487.192915415723746, 201.4288594422998244 ) ) ;
#91014 = CARTESIAN_POINT ( 'NONE',  ( -105.5401914130000023, 1388.839035077719927, 299.4423369547589573 ) ) ;
#91015 = CARTESIAN_POINT ( 'NONE',  ( 18.43597720400000028, 1478.525022087329944, 189.5193842725980176 ) ) ;
#91016 = CARTESIAN_POINT ( 'NONE',  ( 0.2256679910384030152, 1409.089073560189945, 232.6561860856899955 ) ) ;
#91017 = CARTESIAN_POINT ( 'NONE',  ( -38.47038145532883391, 1453.194700005767572, 269.5842303393881139 ) ) ;
#91018 = VERTEX_POINT ( 'NONE', #18170 ) ;
#91019 = B_SPLINE_CURVE_WITH_KNOTS ( 'NONE', 5,
 ( #10961, #77203, #71463, #43046, #19889, #3135, #68814, #110784, #2584, #51435, #101812, #92874, #27749, #37267, #53532, #11514, #16690, #68269, #102377, #45689, #84480, #28309, #87672, #96060, #85565, #54095, #7768 ),
 .UNSPECIFIED., .F., .F.,
 ( 6, 3, 3, 3, 3, 3, 3, 3, 6 ),
 ( 0.000000000000000000, 0.2707461590965168363, 0.3916971170454437989, 0.4318029489778890673, 0.5054684918763174828, 0.5530467713704623200, 0.6440574843390157733, 0.7475457811094275984, 1.000000000000000000 ),
 .UNSPECIFIED. ) ;
#91020 = CARTESIAN_POINT ( 'NONE',  ( -105.0271776439999911, 1379.361271506249977, 303.6846696449590013 ) ) ;
#91021 = CARTESIAN_POINT ( 'NONE',  ( -43.73032397436223562, 1431.081481799955782, 269.0283264950530224 ) ) ;
#91022 = EDGE_CURVE ( 'NONE', #89999, #13894, #43253, .T. ) ;
#91023 = CARTESIAN_POINT ( 'NONE',  ( 11.23532873895420181, 1470.432715234180023, 207.3851918988540035 ) ) ;
#91024 = CARTESIAN_POINT ( 'NONE',  ( -5.552493783490000112, 1484.291247502590068, 199.5131655642589976 ) ) ;
#91025 = CARTESIAN_POINT ( 'NONE',  ( -0.02607537583049999996, 1415.758200151029996, 233.4550498395979901 ) ) ;
#91026 = CARTESIAN_POINT ( 'NONE',  ( -13.13904713841083272, 1444.767805270108965, 186.4863153449116453 ) ) ;
#91027 = CARTESIAN_POINT ( 'NONE',  ( -9.088229089533928828, 1438.332110391349943, 209.8720988501380020 ) ) ;
#91028 = CARTESIAN_POINT ( 'NONE',  ( -4.429773623542629934, 1508.551704408389924, 213.9240755698690180 ) ) ;
#91029 = CIRCLE ( 'NONE', #89279, 1.999999999999912514 ) ;
#91030 = CARTESIAN_POINT ( 'NONE',  ( 11.60004869885203682, 1411.254281879943164, 134.0999999980979851 ) ) ;
#91031 = CARTESIAN_POINT ( 'NONE',  ( -15.11464394393560084, 1415.677402202029953, 207.9357332300280063 ) ) ;
#91032 = AXIS2_PLACEMENT_3D ( 'NONE', #59810, #67665, #43554 ) ;
#91033 = CARTESIAN_POINT ( 'NONE',  ( 24.99158728859999812, 1436.290377140129749, 137.7556578815979833 ) ) ;
#91034 = DIRECTION ( 'NONE',  ( -0.9993779840209169318, 0.0009463042317009218206, 0.03525265327019708878 ) ) ;
#91036 = ORIENTED_EDGE ( 'NONE', *, *, #21057, .T. ) ;
#91035 = CARTESIAN_POINT ( 'NONE',  ( -14.79762023470000187, 1410.816705584730016, 226.7256837507980265 ) ) ;
#91037 = CARTESIAN_POINT ( 'NONE',  ( -113.4000000000000057, 1383.459135650929966, 297.2218459572590064 ) ) ;
#91038 = CARTESIAN_POINT ( 'NONE',  ( 13.77006422079479897, 1512.900351074060154, 224.4275834823730236 ) ) ;
#91039 = ORIENTED_EDGE ( 'NONE', *, *, #27175, .T. ) ;
#91040 = ORIENTED_EDGE ( 'NONE', *, *, #11516, .T. ) ;
#91041 = CARTESIAN_POINT ( 'NONE',  ( -11.55195656709999952, 1501.414664579589726, 210.2508352412490069 ) ) ;
#91042 = CARTESIAN_POINT ( 'NONE',  ( -9.803834995107230554, 1517.151704408390060, 196.6215198571080123 ) ) ;
#91044 = CARTESIAN_POINT ( 'NONE',  ( -22.11712025990000186, 1461.968260157729901, 248.4077083967980286 ) ) ;
#91043 = CARTESIAN_POINT ( 'NONE',  ( 2.011313522410000054, 1455.968210837190099, 218.7648719726389857 ) ) ;
#91045 = CARTESIAN_POINT ( 'NONE',  ( -19.49548631520000086, 1491.251290675329983, 189.4511891077980010 ) ) ;
#91046 = CARTESIAN_POINT ( 'NONE',  ( -11.07768414439999916, 1433.779967063539971, 151.7039717618979751 ) ) ;
#91047 = CARTESIAN_POINT ( 'NONE',  ( 3.448830483803564828, 1511.187213306747708, 175.1594891075192209 ) ) ;
#91048 = CARTESIAN_POINT ( 'NONE',  ( -5.199570078000000706, 1391.913060387289988, 203.8075142969990168 ) ) ;
#91049 = CIRCLE ( 'NONE', #21330, 1.000000000000000888 ) ;
#91050 = CARTESIAN_POINT ( 'NONE',  ( 9.659982096821350339, 1463.878250764609902, 210.8181782570380278 ) ) ;
#91051 = CARTESIAN_POINT ( 'NONE',  ( -25.97380345099999843, 1440.631369481410047, 137.9741832456979864 ) ) ;
#91052 = CARTESIAN_POINT ( 'NONE',  ( -0.9184306762050470363, 1515.115092018379983, 213.4499776085069982 ) ) ;
#91053 = CARTESIAN_POINT ( 'NONE',  ( 7.848979634317430509, 1517.051704408389924, 215.9448598632019980 ) ) ;
#91054 = CARTESIAN_POINT ( 'NONE',  ( 2.392895678049999919, 1449.650479641829861, 182.2220820520979885 ) ) ;
#91055 = CARTESIAN_POINT ( 'NONE',  ( -0.6983432080223432870, 1362.279204239127239, 208.3718459617061285 ) ) ;
#91056 = CARTESIAN_POINT ( 'NONE',  ( 22.52609270013210008, 1509.699688878029974, 227.6602567939980020 ) ) ;
#91058 = ORIENTED_EDGE ( 'NONE', *, *, #16095, .F. ) ;
#91057 = CARTESIAN_POINT ( 'NONE',  ( 3.287954922066450199E-10, 1411.119718540189751, 255.8594453057300200 ) ) ;
#91059 = ORIENTED_EDGE ( 'NONE', *, *, #105682, .T. ) ;
#91060 = CARTESIAN_POINT ( 'NONE',  ( -11.84615870340000043, 1505.361144464890003, 208.3660837394670295 ) ) ;
#91061 = ADVANCED_FACE ( 'NONE', ( #30295 ), #43104, .T. ) ;
#91062 = ADVANCED_FACE ( 'NONE', ( #10899 ), #47509, .T. ) ;
#91063 = CARTESIAN_POINT ( 'NONE',  ( -13.70067222254309947, 1504.052900633450008, 227.6557303632510241 ) ) ;
#91064 = CARTESIAN_POINT ( 'NONE',  ( -8.103048356079998626, 1472.070011036030110, 270.3694265424979903 ) ) ;
#91065 = CARTESIAN_POINT ( 'NONE',  ( 0.000000000000000000, 1514.413060387330006, 209.1218459616979999 ) ) ;
#91066 = CARTESIAN_POINT ( 'NONE',  ( -122.4487580624584382, 1378.528619065188877, 299.2784868977452675 ) ) ;
#91067 = ADVANCED_FACE ( 'NONE', ( #31952 ), #50061, .F. ) ;
#91068 = CARTESIAN_POINT ( 'NONE',  ( 34.51399565513580114, 1450.846036594779889, 136.1540978105180102 ) ) ;
#91070 = EDGE_CURVE ( 'NONE', #74400, #49086, #84677, .T. ) ;
#91069 = CARTESIAN_POINT ( 'NONE',  ( 0.3162628321739870407, 1451.008570913309995, 181.9092865251629973 ) ) ;
#91071 = CARTESIAN_POINT ( 'NONE',  ( -8.849931646880000002, 1384.677929302499933, 199.9332806424890236 ) ) ;
#91072 = CARTESIAN_POINT ( 'NONE',  ( 6.225972109890000716, 1494.795958560490135, 219.7811165620990153 ) ) ;
#91073 = CARTESIAN_POINT ( 'NONE',  ( -4.923014981580000615, 1458.312473659190118, 217.7805121944490168 ) ) ;
#91074 = CARTESIAN_POINT ( 'NONE',  ( 10.95460019480790592, 1366.206855798723154, 210.6218459617030021 ) ) ;
#91075 = CARTESIAN_POINT ( 'NONE',  ( -37.39809849698710309, 1420.331652018609930, 268.7662396804499849 ) ) ;
#91076 = EDGE_LOOP ( 'NONE', ( #23047, #25496, #63048, #67632, #95393, #78120, #45416 ) ) ;
#91077 = CARTESIAN_POINT ( 'NONE',  ( -3.533503288940170073, 1491.923507061140072, 181.6243563976589996 ) ) ;
#91078 = ORIENTED_EDGE ( 'NONE', *, *, #372, .F. ) ;
#91079 = ORIENTED_EDGE ( 'NONE', *, *, #43333, .T. ) ;
#91080 = CARTESIAN_POINT ( 'NONE',  ( 1.718203463455000080, 1516.898441858519845, 210.8221056461869978 ) ) ;
#91081 = CARTESIAN_POINT ( 'NONE',  ( -8.828681655797659289, 1447.722821479130062, 212.1466095620490080 ) ) ;
#91082 = CARTESIAN_POINT ( 'NONE',  ( 40.97446893530570122, 1444.174879737809988, 136.8850285840350125 ) ) ;
#91084 = CARTESIAN_POINT ( 'NONE',  ( 19.63722818094939981, 1521.951704408389787, 218.2362632588020119 ) ) ;
#91083 = CARTESIAN_POINT ( 'NONE',  ( 7.336844642415000450, 1517.106845464700200, 212.5753907958570039 ) ) ;
#91085 = CARTESIAN_POINT ( 'NONE',  ( -16.81040325900000099, 1455.454303044529979, 189.6281205366979918 ) ) ;
#91086 = AXIS2_PLACEMENT_3D ( 'NONE', #57000, #34949, #42809 ) ;
#91087 = CARTESIAN_POINT ( 'NONE',  ( -12.53380499169999851, 1442.773887286369927, 181.5854552579979782 ) ) ;
#91088 = B_SPLINE_SURFACE_WITH_KNOTS ( 'NONE', 5, 1, ( 
 ( #16362, #84140 ),
 ( #67375, #42152 ),
 ( #94191, #76303 ),
 ( #102033, #25319 ),
 ( #24760, #50561 ),
 ( #75217, #76861 ),
 ( #109368, #22143 ),
 ( #50007, #100926 ),
 ( #84687, #172 ) ),
 .UNSPECIFIED., .F., .F., .F.,
 ( 6, 3, 6 ),
 ( 2, 2 ),
 ( 0.000000000000000000, 3.733858336720000004, 7.455685587529999658 ),
 ( 0.000000000000000000, 14.00000000000000000 ),
 .UNSPECIFIED. ) ;
#91089 = ORIENTED_EDGE ( 'NONE', *, *, #27586, .T. ) ;
#91090 = CARTESIAN_POINT ( 'NONE',  ( -10.79382269979189957, 1414.913060387349788, 196.1395788316550011 ) ) ;
#91091 = EDGE_CURVE ( 'NONE', #74077, #104782, #26299, .T. ) ;
#91092 = B_SPLINE_CURVE_WITH_KNOTS ( 'NONE', 5,
 ( #21732, #45886, #105790, #54839, #72200, #29604, #56482, #11715, #63791 ),
 .UNSPECIFIED., .F., .F.,
 ( 6, 3, 6 ),
 ( 0.000000000000000000, 0.4491568913793235751, 1.000000000000000000 ),
 .UNSPECIFIED. ) ;
#91093 = CARTESIAN_POINT ( 'NONE',  ( -7.331812124104999384, 1516.906641539930206, 202.5676945058570197 ) ) ;
#91094 = AXIS2_PLACEMENT_3D ( 'NONE', #21190, #55400, #89531 ) ;
#91095 = B_SPLINE_SURFACE_WITH_KNOTS ( 'NONE', 5, 5, ( 
 ( #58688, #31264, #58140, #59249, #99556, #57600 ),
 ( #92821, #24498, #74947, #65446, #76028, #31816 ),
 ( #108524, #16092, #22840, #33449, #84959, #75499 ),
 ( #15541, #100661, #101202, #93367, #6065, #109094 ),
 ( #41872, #50830, #57046, #14994, #101758, #48644 ),
 ( #91171, #40218, #16633, #32376, #23944, #74399 ),
 ( #92272, #7171, #66004, #25046, #8253, #73840 ),
 ( #100124, #23408, #49741, #83868, #50300, #41330 ),
 ( #109633, #84427, #32907, #67099, #7713, #102314 ) ),
 .UNSPECIFIED., .F., .F., .F.,
 ( 6, 3, 6 ),
 ( 6, 6 ),
 ( 3.881604426910000072, 7.667864109139999940, 12.69765133870000007 ),
 ( 0.000000000000000000, 2.000000000000000000 ),
 .UNSPECIFIED. ) ;
#91096 = DIRECTION ( 'NONE',  ( 0.000000000000000000, 0.000000000000000000, -1.000000000000000000 ) ) ;
#91097 = EDGE_CURVE ( 'NONE', #104566, #2114, #206, .T. ) ;
#91098 = CARTESIAN_POINT ( 'NONE',  ( -18.05215045752869685, 1384.529053208030064, 201.2145023365150109 ) ) ;
#91099 = CARTESIAN_POINT ( 'NONE',  ( 0.03232804668210000759, 1407.837594160830122, 195.9367397046979988 ) ) ;
#91100 = CARTESIAN_POINT ( 'NONE',  ( -2.664535259099599458E-15, 1405.913060387330006, 209.1218459616979999 ) ) ;
#91101 = AXIS2_PLACEMENT_3D ( 'NONE', #101355, #51543, #52106 ) ;
#91103 = EDGE_LOOP ( 'NONE', ( #13517, #66726, #72480, #49539 ) ) ;
#91102 = CARTESIAN_POINT ( 'NONE',  ( -9.936738324559998503, 1364.340818343090177, 207.6218459616989946 ) ) ;
#91104 = ORIENTED_EDGE ( 'NONE', *, *, #57754, .T. ) ;
#91106 = ADVANCED_FACE ( 'NONE', ( #103568 ), #95179, .F. ) ;
#91105 = CARTESIAN_POINT ( 'NONE',  ( 0.2703871436749999968, 1452.337177918929910, 183.2881653520979910 ) ) ;
#91107 = CARTESIAN_POINT ( 'NONE',  ( 21.12212911287011607, 1511.187213306747708, 182.4210318429774134 ) ) ;
#91108 = CARTESIAN_POINT ( 'NONE',  ( -6.871715297790212063, 1521.804095990991300, 183.7897170437400973 ) ) ;
#91109 = CARTESIAN_POINT ( 'NONE',  ( 19.41157449629999832, 1457.417846740989944, 209.1218459616989946 ) ) ;
#91110 = FACE_OUTER_BOUND ( 'NONE', #18516, .T. ) ;
#91112 = CARTESIAN_POINT ( 'NONE',  ( 3.269025135755000200, 1517.026534522949987, 210.2412850599169758 ) ) ;
#91111 = AXIS2_PLACEMENT_3D ( 'NONE', #30554, #56318, #90451 ) ;
#91113 = CARTESIAN_POINT ( 'NONE',  ( 6.164918445296012628, 1460.089225756436917, 201.7079981919788167 ) ) ;
#91114 = CARTESIAN_POINT ( 'NONE',  ( -1.782112605382539794, 1484.239369046139927, 182.8010181983919722 ) ) ;
#91115 = CARTESIAN_POINT ( 'NONE',  ( -14.87168878229999969, 1430.147188444230096, 221.8136313627980201 ) ) ;
#91116 = DIRECTION ( 'NONE',  ( 1.224646799147350002E-16, -1.836970198721029688E-16, -1.000000000000000000 ) ) ;
#91117 = CARTESIAN_POINT ( 'NONE',  ( 7.656028667734999793, 1510.967342883699985, 204.6265760743969793 ) ) ;
#91118 = CARTESIAN_POINT ( 'NONE',  ( 0.7350231981660010350, 1516.970035769810011, 206.8242163110469960 ) ) ;
#91119 = VERTEX_POINT ( 'NONE', #43675 ) ;
#91120 = CARTESIAN_POINT ( 'NONE',  ( -36.37832872588079169, 1435.767865734240104, 134.7398496865939990 ) ) ;
#91121 = CARTESIAN_POINT ( 'NONE',  ( -10.10379226119999885, 1472.617050353389914, 207.7708162939690055 ) ) ;
#91122 = CARTESIAN_POINT ( 'NONE',  ( -0.2572001039731363070, 1516.857224341873234, 201.6176683814753403 ) ) ;
#91123 = ORIENTED_EDGE ( 'NONE', *, *, #7129, .F. ) ;
#91124 = CARTESIAN_POINT ( 'NONE',  ( 2.787053946926249637, 1424.897258074847059, 183.3886486283980162 ) ) ;
#91125 = CARTESIAN_POINT ( 'NONE',  ( -24.67353296015457076, 1509.777057924631208, 225.1797433603865386 ) ) ;
#91126 = CARTESIAN_POINT ( 'NONE',  ( 13.76900370180000088, 1415.553739807329976, 196.8536881224979993 ) ) ;
#91127 = CARTESIAN_POINT ( 'NONE',  ( -1.906499846882070084E-08, 1509.038615934239942, 201.6090957241369779 ) ) ;
#91128 = CARTESIAN_POINT ( 'NONE',  ( -20.81306254345079765, 1578.884139733799884, 163.1496826969390384 ) ) ;
#91129 = CARTESIAN_POINT ( 'NONE',  ( 17.48729376020000004, 1410.446401242629918, 225.6075485739979740 ) ) ;
#91130 = CARTESIAN_POINT ( 'NONE',  ( 7.424447884040000112, 1487.091156260190019, 201.2206016250389951 ) ) ;
#91131 = CARTESIAN_POINT ( 'NONE',  ( 2.382436964801011303, 1426.901689560120076, 137.0999999980980135 ) ) ;
#91132 = CARTESIAN_POINT ( 'NONE',  ( 22.77112932521035304, 1451.090417561717004, 218.6197847536123788 ) ) ;
#91133 = CIRCLE ( 'NONE', #3581, 41.12363927708771882 ) ;
#91134 = DIRECTION ( 'NONE',  ( -0.9996573249755569268, 0.02617694830788839730, -1.272313417210569287E-16 ) ) ;
#91135 = DIRECTION ( 'NONE',  ( 0.8750399157388792926, -0.3840929811364761082, 0.2945805962812040324 ) ) ;
#91136 = CARTESIAN_POINT ( 'NONE',  ( 0.01073129396420149928, 1516.939491476980038, 216.4539099096770087 ) ) ;
#91137 = EDGE_LOOP ( 'NONE', ( #62772, #71334, #25365, #95250 ) ) ;
#91138 = CARTESIAN_POINT ( 'NONE',  ( 7.714513390629210932, 1516.743641023210103, 208.4557674029649945 ) ) ;
#91139 = CARTESIAN_POINT ( 'NONE',  ( -26.02835829340000018, 1468.278484548229926, 269.9886483896979712 ) ) ;
#91140 = DIRECTION ( 'NONE',  ( 0.9824080081115887930, -2.243614313870717968E-31, 0.1867471702549210744 ) ) ;
#91141 = CARTESIAN_POINT ( 'NONE',  ( -15.86751291366650030, 1508.452568328270218, 214.6320188443539791 ) ) ;
#91142 = CARTESIAN_POINT ( 'NONE',  ( 1.498519443250000194, 1473.533415296189787, 219.2408100347990114 ) ) ;
#91143 = CARTESIAN_POINT ( 'NONE',  ( 6.500314218507900144, 1509.153493339920033, 179.5230332626949803 ) ) ;
#91144 = CARTESIAN_POINT ( 'NONE',  ( 11.60004869885203682, 1425.888728951611938, 137.5022903913526591 ) ) ;
#91145 = CARTESIAN_POINT ( 'NONE',  ( 2.933420754659926466, 1417.794866989897400, 234.2124010178503113 ) ) ;
#91146 = AXIS2_PLACEMENT_3D ( 'NONE', #83338, #98482, #21750 ) ;
#91147 = CARTESIAN_POINT ( 'NONE',  ( -2.500000000000000000, 1424.046630307830128, 154.4234530583979961 ) ) ;
#91148 = CARTESIAN_POINT ( 'NONE',  ( -0.8168837593883370163, 1455.407754195820189, 198.6297299609340143 ) ) ;
#91149 = LINE ( 'NONE', #32885, #100585 ) ;
#91150 = CARTESIAN_POINT ( 'NONE',  ( 28.79543911281049873, 1440.913060387340010, 234.2238028330110069 ) ) ;
#91152 = CARTESIAN_POINT ( 'NONE',  ( -6.475563477829999748, 1476.191846288490069, 217.2936124755890148 ) ) ;
#91151 = CARTESIAN_POINT ( 'NONE',  ( -9.839566507713760402, 1471.648513791290043, 211.6171294469720010 ) ) ;
#91153 = CARTESIAN_POINT ( 'NONE',  ( 2.782628547279999864, 1480.749758698789947, 229.4592195060989752 ) ) ;
#91154 = ORIENTED_EDGE ( 'NONE', *, *, #104403, .F. ) ;
#91155 = ORIENTED_EDGE ( 'NONE', *, *, #51331, .F. ) ;
#91156 = CARTESIAN_POINT ( 'NONE',  ( 13.51610093808350221, 1442.913060377700731, 206.7785865123596807 ) ) ;
#91157 = EDGE_CURVE ( 'NONE', #944, #14800, #105708, .T. ) ;
#91158 = CARTESIAN_POINT ( 'NONE',  ( -9.840693639790396574, 1506.501081010019561, 228.8468162685099685 ) ) ;
#91159 = CARTESIAN_POINT ( 'NONE',  ( -1.730029831119999972, 1444.010312626490077, 199.6239785729489995 ) ) ;
#91160 = CARTESIAN_POINT ( 'NONE',  ( 11.37179842121179973, 1502.689078123959916, 211.1467236230820106 ) ) ;
#91161 = EDGE_CURVE ( 'NONE', #89473, #96332, #34710, .T. ) ;
#91162 = CARTESIAN_POINT ( 'NONE',  ( -11.78824854703250047, 1517.051704408389924, 206.8304425649369875 ) ) ;
#91163 = CARTESIAN_POINT ( 'NONE',  ( 10.70745313423520173, 1422.293419597579941, 211.2167388469730156 ) ) ;
#91164 = CARTESIAN_POINT ( 'NONE',  ( -16.64885258016277803, 1526.344110814222404, 234.9109520333565797 ) ) ;
#91165 = CARTESIAN_POINT ( 'NONE',  ( 0.9261100251351479518, 1508.551704408389924, 219.8874203466220081 ) ) ;
#91166 = CARTESIAN_POINT ( 'NONE',  ( -41.53790650758289615, 1383.825758773150028, 244.5308847209749956 ) ) ;
#91167 = CARTESIAN_POINT ( 'NONE',  ( -4.427981762014999489, 1510.423579818969984, 201.5728291684769999 ) ) ;
#91168 = CARTESIAN_POINT ( 'NONE',  ( -14.46947201719999931, 1471.323284330429715, 193.8233120731979966 ) ) ;
#91169 = CARTESIAN_POINT ( 'NONE',  ( -12.68115466278469938, 1502.671228371769985, 209.0114104908589638 ) ) ;
#91170 = CARTESIAN_POINT ( 'NONE',  ( -113.4000000000000057, 1390.913060387289988, 304.2218459572590064 ) ) ;
#91172 = ORIENTED_EDGE ( 'NONE', *, *, #8363, .T. ) ;
#91171 = CARTESIAN_POINT ( 'NONE',  ( -0.2871112535150010525, 1455.269628498290103, 218.5715099901590008 ) ) ;
#91173 = AXIS2_PLACEMENT_3D ( 'NONE', #40403, #83500, #109283 ) ;
#91174 = EDGE_CURVE ( 'NONE', #11504, #79125, #59328, .T. ) ;
#91175 = CARTESIAN_POINT ( 'NONE',  ( -16.32897964160000370, 1384.525298249519892, 200.5993092285889929 ) ) ;
#91176 = CARTESIAN_POINT ( 'NONE',  ( 2.640559408228119853, 1508.551704408389924, 204.1382632388410059 ) ) ;
#91177 = ORIENTED_EDGE ( 'NONE', *, *, #42524, .T. ) ;
#91178 = ORIENTED_EDGE ( 'NONE', *, *, #26821, .T. ) ;
#91179 = PRODUCT_DEFINITION_SHAPE ( 'NONE', 'NONE',  #110834 ) ;
#91180 = CARTESIAN_POINT ( 'NONE',  ( -7.567236696338139446, 1385.515642188830270, 219.0512315761490072 ) ) ;
#91181 = CARTESIAN_POINT ( 'NONE',  ( -4.261662194147370464, 1515.372228416580128, 206.7919396095460058 ) ) ;
#91182 = CARTESIAN_POINT ( 'NONE',  ( -0.5621806508122783042, 1416.843574565329845, 227.7683146822559763 ) ) ;
#91183 = AXIS2_PLACEMENT_3D ( 'NONE', #93982, #86694, #8868 ) ;
#91184 = CARTESIAN_POINT ( 'NONE',  ( -5.070280933269999402, 1462.534208498590033, 200.7832906722389907 ) ) ;
#91185 = CARTESIAN_POINT ( 'NONE',  ( -106.5438666130000058, 1380.603607321050049, 299.5701110033589316 ) ) ;
#91186 = CARTESIAN_POINT ( 'NONE',  ( 3.712013955199999771, 1466.291930614589774, 219.5294839965989979 ) ) ;
#91187 = CARTESIAN_POINT ( 'NONE',  ( -5.134308048384249940E-13, 1492.051704408390151, 209.1218459616989946 ) ) ;
#91188 = CARTESIAN_POINT ( 'NONE',  ( 1.642074464903110043, 1408.970402891180129, 194.2161375618219950 ) ) ;
#91189 = CARTESIAN_POINT ( 'NONE',  ( 18.80464029359000122, 1425.800308749483975, 225.6068200636500194 ) ) ;
#91190 = CARTESIAN_POINT ( 'NONE',  ( 2.412180996239999597, 1419.421713268930034, 185.1536642287979930 ) ) ;
#91191 = CARTESIAN_POINT ( 'NONE',  ( -66.90724276829999440, 1379.748944712210005, 276.4281807783590352 ) ) ;
#91192 = CIRCLE ( 'NONE', #19655, 1.000000000000000888 ) ;
#91193 = B_SPLINE_CURVE_WITH_KNOTS ( 'NONE', 5,
 ( #93947, #51409, #75529, #16126, #17770, #51973 ),
 .UNSPECIFIED., .F., .F.,
 ( 6, 6 ),
 ( 0.000000000000000000, 1.000000000000000000 ),
 .UNSPECIFIED. ) ;
#91194 = CARTESIAN_POINT ( 'NONE',  ( -3.365813053994819892, 1449.482398035879896, 184.7700481427870045 ) ) ;
#91195 = EDGE_LOOP ( 'NONE', ( #76245, #51728, #25146, #51357 ) ) ;
#91196 = ADVANCED_FACE ( 'NONE', ( #1135 ), #97540, .T. ) ;
#91197 = CARTESIAN_POINT ( 'NONE',  ( -6.232532191338900240, 1398.098440470949981, 197.7132727547819968 ) ) ;
#91198 = CARTESIAN_POINT ( 'NONE',  ( 19.38194617106359985, 1456.050539493930046, 227.4026333903129853 ) ) ;
#91199 = CARTESIAN_POINT ( 'NONE',  ( -12.70521320840000001, 1434.771930543859980, 150.2289112725980260 ) ) ;
#91200 = CARTESIAN_POINT ( 'NONE',  ( -4.034698761822709636E-10, 1466.818507878050013, 244.3811635369520161 ) ) ;
#91201 = CARTESIAN_POINT ( 'NONE',  ( -20.47924549841579989, 1503.953507240960107, 190.5028550971699985 ) ) ;
#91202 = PLANE ( 'NONE',  #78639 ) ;
#91203 = CARTESIAN_POINT ( 'NONE',  ( -109.5704612849999933, 1384.938891529579905, 311.3082982532590108 ) ) ;
#91204 = CARTESIAN_POINT ( 'NONE',  ( -0.1801023543370000035, 1476.672953218830116, 182.1974262930980046 ) ) ;
#91205 = CARTESIAN_POINT ( 'NONE',  ( -10.14614043715151581, 1361.444406935758934, 208.3718459617010978 ) ) ;
#91206 = CARTESIAN_POINT ( 'NONE',  ( -45.84755609590860104, 1440.256076863080125, 268.7565746053210205 ) ) ;
#91207 = CARTESIAN_POINT ( 'NONE',  ( -20.86430737430000448, 1507.787508480630095, 191.9680527028979782 ) ) ;
#91208 = ADVANCED_FACE ( 'NONE', ( #41275 ), #72534, .T. ) ;
#91209 = CARTESIAN_POINT ( 'NONE',  ( -7.339749373344999661, 1517.224900789629828, 207.4124613591469881 ) ) ;
#91210 = VECTOR ( 'NONE', #47812, 1000.000000000000000 ) ;
#91211 = CARTESIAN_POINT ( 'NONE',  ( 5.683171320879200294, 1409.111521102960069, 222.7165751117499894 ) ) ;
#91212 = CARTESIAN_POINT ( 'NONE',  ( 29.37542415142989327, 1526.382868172864164, 200.9849896654459087 ) ) ;
#91213 = B_SPLINE_SURFACE_WITH_KNOTS ( 'NONE', 5, 5, ( 
 ( #47851, #108855, #100991, #6402, #41660, #48976, #83108, #81985, #83648 ),
 ( #75816, #90383, #48421, #6943, #92595, #64679, #98796, #5293, #39451 ),
 ( #65220, #14232, #82564, #51727, #16421, #77475, #69091, #52836, #8592 ),
 ( #42764, #102634, #76924, #76363, #35461, #25935, #61258, #69651, #78013 ),
 ( #43870, #86963, #110512, #60131, #233, #52287, #59572, #94816, #1320 ),
 ( #776, #33794, #103772, #86412, #34905, #34360, #18093, #17524, #50614 ),
 ( #10254, #18637, #102100, #44430, #85862, #93152, #43327, #27075, #9163 ),
 ( #94250, #103192, #84746, #9702, #26497, #78574, #59027, #16966, #60693 ),
 ( #33245, #95373, #67435, #8044, #101533, #24822, #42212, #67988, #25380 ) ),
 .UNSPECIFIED., .F., .F., .F.,
 ( 6, 3, 6 ),
 ( 6, 3, 6 ),
 ( 3.580107477810000383, 6.558749095569999632, 9.700153431689999550 ),
 ( 0.000000000000000000, 0.5000000000000000000, 1.000000000000000000 ),
 .UNSPECIFIED. ) ;
#91214 = CARTESIAN_POINT ( 'NONE',  ( 8.963481490043514910, 1426.098811295182031, 225.6675240377605292 ) ) ;
#91215 = CARTESIAN_POINT ( 'NONE',  ( 7.490788429555370165, 1425.317015923290001, 212.2654107691739966 ) ) ;
#91216 = ADVANCED_FACE ( 'NONE', ( #65947 ), #86745, .T. ) ;
#91217 = EDGE_LOOP ( 'NONE', ( #54171, #38734 ) ) ;
#91218 = CARTESIAN_POINT ( 'NONE',  ( 31.69751081770000312, 1436.813883501469945, 244.1892870132980136 ) ) ;
#91219 = CARTESIAN_POINT ( 'NONE',  ( -9.975542809210001138, 1421.165924026620132, 193.6282031886989898 ) ) ;
#91221 = CARTESIAN_POINT ( 'NONE',  ( -15.05672298745219884, 1512.222316757829958, 221.7473544089129973 ) ) ;
#91220 = CARTESIAN_POINT ( 'NONE',  ( -1.525257681609999860, 1486.442310458030079, 181.6794219812979918 ) ) ;
#91222 = CARTESIAN_POINT ( 'NONE',  ( -20.70484064406422320, 1525.907212628473644, 185.0411015109855839 ) ) ;
#91223 = CIRCLE ( 'NONE', #84031, 4.250000000000000000 ) ;
#91224 = CARTESIAN_POINT ( 'NONE',  ( -4.104542198569999911, 1419.727281559329867, 225.2064028888979976 ) ) ;
#91225 = CARTESIAN_POINT ( 'NONE',  ( -4.636950470105315247, 1378.041548212150929, 214.3403514578957925 ) ) ;
#91226 = CARTESIAN_POINT ( 'NONE',  ( -19.56170200118970115, 1452.229950700849940, 143.7718973678339864 ) ) ;
#91227 = DIRECTION ( 'NONE',  ( 0.000000000000000000, -1.000000000000000000, 6.123233995736769734E-17 ) ) ;
#91228 = ORIENTED_EDGE ( 'NONE', *, *, #2530, .T. ) ;
#91229 = CARTESIAN_POINT ( 'NONE',  ( -3.179033943583710276, 1457.997354099609993, 219.3203918230290128 ) ) ;
#91230 = CARTESIAN_POINT ( 'NONE',  ( 17.29882006758069934, 1523.542365884050241, 237.3908737315652786 ) ) ;
#91231 = FACE_OUTER_BOUND ( 'NONE', #32399, .T. ) ;
#91232 = CARTESIAN_POINT ( 'NONE',  ( 9.772933234099999922, 1463.374803562589932, 209.6899480743859954 ) ) ;
#91233 = ORIENTED_EDGE ( 'NONE', *, *, #23447, .F. ) ;
#91234 = ORIENTED_EDGE ( 'NONE', *, *, #97083, .T. ) ;
#91235 = EDGE_CURVE ( 'NONE', #33528, #79144, #33909, .T. ) ;
#91236 = CARTESIAN_POINT ( 'NONE',  ( -62.44985522310000192, 1384.688102815929824, 249.3037632142590212 ) ) ;
#91237 = CARTESIAN_POINT ( 'NONE',  ( -23.76160520478569893, 1410.154579653240035, 209.1277447343530014 ) ) ;
#91238 = ORIENTED_EDGE ( 'NONE', *, *, #67827, .T. ) ;
#91239 = FACE_OUTER_BOUND ( 'NONE', #60056, .T. ) ;
#91240 = CARTESIAN_POINT ( 'NONE',  ( -9.638115897709079505, 1516.551188146539971, 203.7504991310609910 ) ) ;
#91241 = EDGE_CURVE ( 'NONE', #76367, #64503, #101616, .T. ) ;
#91242 = CARTESIAN_POINT ( 'NONE',  ( -3.894297052259999781, 1498.349224807129985, 236.2074788674979970 ) ) ;
#91243 = CARTESIAN_POINT ( 'NONE',  ( -18.37208795600000144, 1410.877977816430075, 224.1326316794980187 ) ) ;
#91244 = CARTESIAN_POINT ( 'NONE',  ( 44.21373685866610259, 1449.831903069469945, 266.2301373114850094 ) ) ;
#91245 = DIRECTION ( 'NONE',  ( -0.5369043659965772042, -0.4884709562386981840, 0.6878443331779838799 ) ) ;
#91246 = CARTESIAN_POINT ( 'NONE',  ( -6.499023713309999728, 1427.690723050089900, 203.8816284302589850 ) ) ;
#91247 =( BOUNDED_CURVE ( )  B_SPLINE_CURVE ( 3, ( #48843, #81857, #40959, #100320 ),
 .UNSPECIFIED., .F., .F. ) 
 B_SPLINE_CURVE_WITH_KNOTS ( ( 4, 4 ),
 ( 3.086775739023659870, 3.394672873780574918 ),
 .UNSPECIFIED. ) 
 CURVE ( )  GEOMETRIC_REPRESENTATION_ITEM ( )  RATIONAL_B_SPLINE_CURVE ( ( 1.000000000000000000, 0.9921155365922033065, 0.9921155365922033065, 1.000000000000000000 ) ) 
 REPRESENTATION_ITEM ( '' )  );
#91248 = CARTESIAN_POINT ( 'NONE',  ( 4.609996581545000360, 1516.769879638719885, 205.6626893540170329 ) ) ;
#91249 = EDGE_LOOP ( 'NONE', ( #74705, #107401, #107439, #55290 ) ) ;
#91250 = CARTESIAN_POINT ( 'NONE',  ( -0.2331143941452460122, 1408.921200921389982, 231.7611568498559791 ) ) ;
#91251 = DIRECTION ( 'NONE',  ( -0.6736849260863841948, 0.000000000000000000, 0.7390186874254148774 ) ) ;
#91252 = CARTESIAN_POINT ( 'NONE',  ( 13.49429930720275017, 1443.686343019639480, 188.0286533011901042 ) ) ;
#91253 = ORIENTED_EDGE ( 'NONE', *, *, #93511, .F. ) ;
#91254 = ORIENTED_EDGE ( 'NONE', *, *, #27606, .T. ) ;
#91255 = DIRECTION ( 'NONE',  ( -4.110483225678505215E-05, -1.788365258186560565E-06, 0.9999999991535972743 ) ) ;
#91256 = CARTESIAN_POINT ( 'NONE',  ( 7.735002320672926146, 1435.902786767089538, 205.2877876006086808 ) ) ;
#91257 = B_SPLINE_SURFACE_WITH_KNOTS ( 'NONE', 5, 5, ( 
 ( #85278, #2435, #51707, #70747, #104858, #43309 ),
 ( #85847, #9146, #760, #34888, #103178, #60676 ),
 ( #94802, #18077, #52272, #105414, #5145, #88077 ),
 ( #11365, #98646, #28706, #71300, #79675, #30341 ),
 ( #46079, #71858, #4606, #88624, #38740, #80763 ),
 ( #20834, #55576, #3528, #89700, #62911, #11904 ),
 ( #80210, #30889, #105975, #107606, #96462, #98095 ),
 ( #97022, #21368, #29252, #37100, #37653, #12444 ),
 ( #55029, #2980, #72918, #4071, #12981, #38196 ),
 ( #81840, #89156, #39300, #63985, #45536, #47711 ),
 ( #63443, #97561, #46629, #72379, #106507, #29797 ),
 ( #20283, #47164, #54489, #81292, #73473, #107057 ) ),
 .UNSPECIFIED., .F., .F., .F.,
 ( 6, 3, 3, 6 ),
 ( 6, 6 ),
 ( 37.11367623070000121, 43.72652432289999780, 46.71962562659999918, 49.71279531210000613 ),
 ( 0.000000000000000000, 2.000000000000000000 ),
 .UNSPECIFIED. ) ;
#91258 = CARTESIAN_POINT ( 'NONE',  ( -12.33871149695520053, 1512.142158944850053, 194.2604755866809967 ) ) ;
#91259 = CARTESIAN_POINT ( 'NONE',  ( 9.850217353651350649, 1503.174886245870084, 217.1987157647029960 ) ) ;
#91260 = VECTOR ( 'NONE', #85571, 1000.000000000000000 ) ;
#91261 = FACE_OUTER_BOUND ( 'NONE', #19048, .T. ) ;
#91262 = CARTESIAN_POINT ( 'NONE',  ( -3.263756439183980174, 1476.410057112220102, 220.1266873629019756 ) ) ;
#91263 = CARTESIAN_POINT ( 'NONE',  ( -108.4300409128252767, 1381.105006665046176, 298.0805022167543257 ) ) ;
#91264 =( GEOMETRIC_REPRESENTATION_CONTEXT ( 3 ) GLOBAL_UNCERTAINTY_ASSIGNED_CONTEXT ( ( #89367 ) ) GLOBAL_UNIT_ASSIGNED_CONTEXT ( ( #19752, #88636, #46091 ) ) REPRESENTATION_CONTEXT ( 'NONE', 'WORKASPACE' ) );
#91265 = CARTESIAN_POINT ( 'NONE',  ( 10.16454034401940021, 1479.821216484649995, 205.9845809784859796 ) ) ;
#91266 = DIRECTION ( 'NONE',  ( -0.02616798426500965835, 0.9993150019883683122, -0.02616798426500970692 ) ) ;
#91268 = CARTESIAN_POINT ( 'NONE',  ( 16.43752752869999867, 1507.637957906029897, 193.5312328863980156 ) ) ;
#91267 = CARTESIAN_POINT ( 'NONE',  ( 30.01482722728456665, 1525.231909165051093, 196.6362179804465882 ) ) ;
#91269 = CARTESIAN_POINT ( 'NONE',  ( 10.82434022283250030, 1423.324388501479916, 206.8207127886749959 ) ) ;
#91270 = CARTESIAN_POINT ( 'NONE',  ( -24.61162824655679771, 1509.291569965729877, 222.5955736776400045 ) ) ;
#91271 = CARTESIAN_POINT ( 'NONE',  ( 11.01124415049999961, 1428.984115384829920, 91.31218443469779800 ) ) ;
#91272 = ORIENTED_EDGE ( 'NONE', *, *, #20626, .T. ) ;
#91273 = CARTESIAN_POINT ( 'NONE',  ( 18.51068734469999910, 1475.362681785890118, 218.3399159096489939 ) ) ;
#91274 = CARTESIAN_POINT ( 'NONE',  ( -0.01912654351157340102, 1347.931987472819856, 209.1220808601199792 ) ) ;
#91275 = CARTESIAN_POINT ( 'NONE',  ( -90.01380978207909322, 1384.969498126610006, 308.7154665456239968 ) ) ;
#91276 = CARTESIAN_POINT ( 'NONE',  ( -9.221393643380000782, 1387.134211727530101, 200.5164217425590039 ) ) ;
#91277 = CARTESIAN_POINT ( 'NONE',  ( 10.31326332856479944, 1422.496447624620032, 210.6272975906319971 ) ) ;
#91279 = ORIENTED_EDGE ( 'NONE', *, *, #78052, .F. ) ;
#91278 = CARTESIAN_POINT ( 'NONE',  ( 11.42162556611340030, 1422.176594433650052, 203.3886333800170121 ) ) ;
#91280 = CARTESIAN_POINT ( 'NONE',  ( 1.680959541130000012, 1430.284313584789970, 217.4307392857090235 ) ) ;
#91281 = CARTESIAN_POINT ( 'NONE',  ( -2.488082932330000219, 1441.600846913620217, 150.5962877614979902 ) ) ;
#91282 = CARTESIAN_POINT ( 'NONE',  ( -14.35446004689999810, 1416.822692864329838, 221.5782750974979933 ) ) ;
#91283 = CARTESIAN_POINT ( 'NONE',  ( 11.22261500629999986, 1433.988530975800131, 151.5940001495979743 ) ) ;
#91284 = CARTESIAN_POINT ( 'NONE',  ( 5.757839680140000027, 1468.063065669429989, 262.6648722463980334 ) ) ;
#91285 = CARTESIAN_POINT ( 'NONE',  ( 15.72751745975079984, 1517.051704408389924, 206.8816388537309763 ) ) ;
#91286 = CARTESIAN_POINT ( 'NONE',  ( -11.60004869885203682, 1428.983126981193436, 134.0999999980979851 ) ) ;
#91287 = CARTESIAN_POINT ( 'NONE',  ( -4.035334156310671716, 1456.652990358677243, 217.7497121191034353 ) ) ;
#91288 = CARTESIAN_POINT ( 'NONE',  ( -109.7434571511378323, 1386.572387547986409, 297.1542559680822819 ) ) ;
#91289 = CARTESIAN_POINT ( 'NONE',  ( 11.92849869075366698, 1511.839858410422266, 224.1270719350856098 ) ) ;
#91290 = EDGE_CURVE ( 'NONE', #61519, #72801, #56896, .T. ) ;
#91291 = CARTESIAN_POINT ( 'NONE',  ( -32.10255801038886858, 1525.211477436245787, 201.2198389390407272 ) ) ;
#91292 = CARTESIAN_POINT ( 'NONE',  ( 0.5697990016583959205, 1450.893162567740092, 181.2939912002310052 ) ) ;
#91293 = CARTESIAN_POINT ( 'NONE',  ( -17.92837075459999951, 1410.035885881930199, 224.4980084594979814 ) ) ;
#91294 = CARTESIAN_POINT ( 'NONE',  ( -20.49359230279999977, 1486.268284136490138, 212.0880304968289636 ) ) ;
#91295 = CARTESIAN_POINT ( 'NONE',  ( 34.33069675793380071, 1442.322945860919845, 137.1732133209670224 ) ) ;
#91296 = DIRECTION ( 'NONE',  ( -0.03173147633638266629, -0.9969860201949399814, -0.07079540200725242816 ) ) ;
#91297 = CARTESIAN_POINT ( 'NONE',  ( 9.726491193908251375E-12, 1408.913060387299993, 194.1220083575990145 ) ) ;
#91298 = CARTESIAN_POINT ( 'NONE',  ( 12.74682077097699917, 1426.700036781529889, 204.1990136926680179 ) ) ;
#91299 = CARTESIAN_POINT ( 'NONE',  ( 18.28863234242390234, 1430.119122075690029, 201.0315569595829857 ) ) ;
#91300 = CARTESIAN_POINT ( 'NONE',  ( -9.959064579650000582, 1415.087818611729972, 222.8661268712980075 ) ) ;
#91301 = CARTESIAN_POINT ( 'NONE',  ( 0.2077598587401390251, 1458.608988913009853, 183.0127631382089817 ) ) ;
#91303 = ORIENTED_EDGE ( 'NONE', *, *, #102111, .F. ) ;
#91302 = CARTESIAN_POINT ( 'NONE',  ( -2.814434489400770012, 1407.025243844600027, 222.1218459754350363 ) ) ;
#91304 = CARTESIAN_POINT ( 'NONE',  ( 0.4435022289555869968, 1418.672171135500093, 184.7048927309859891 ) ) ;
#91305 = AXIS2_PLACEMENT_3D ( 'NONE', #26672, #110136, #109595 ) ;
#91306 = EDGE_CURVE ( 'NONE', #104116, #9907, #69987, .T. ) ;
#91307 = CARTESIAN_POINT ( 'NONE',  ( -28.79711193535739966, 1509.835383000219963, 211.3965062070199963 ) ) ;
#91308 = CARTESIAN_POINT ( 'NONE',  ( 11.94118163750000150, 1433.615363880359837, 149.1895118235980249 ) ) ;
#91309 = CARTESIAN_POINT ( 'NONE',  ( -26.81573373259999826, 1435.593055354309854, 136.1631887211979688 ) ) ;
#91310 = CARTESIAN_POINT ( 'NONE',  ( 11.78238822100000149, 1440.882651071759938, 188.1224418543980335 ) ) ;
#91311 = EDGE_LOOP ( 'NONE', ( #65382, #9887, #32138, #26868, #1044 ) ) ;
#91312 = CARTESIAN_POINT ( 'NONE',  ( -17.05900707844612185, 1524.678872986499300, 181.0478682887629702 ) ) ;
#91313 = CARTESIAN_POINT ( 'NONE',  ( 9.682949316780000260, 1479.800193431990010, 204.8983903314390034 ) ) ;
#91314 = CARTESIAN_POINT ( 'NONE',  ( -105.1388918222897502, 1380.999031973004776, 308.5443376699517444 ) ) ;
#91315 = CARTESIAN_POINT ( 'NONE',  ( -11.02925645290000034, 1492.700458242990180, 208.1688302671739734 ) ) ;
#91316 = CARTESIAN_POINT ( 'NONE',  ( -1.371718781699999834, 1452.291798068730031, 183.7871359344979965 ) ) ;
#91317 = B_SPLINE_CURVE_WITH_KNOTS ( 'NONE', 3,
 ( #85724, #44864, #86283, #52150 ),
 .UNSPECIFIED., .F., .F.,
 ( 4, 4 ),
 ( 0.000000000000000000, 1.000000000000000000 ),
 .UNSPECIFIED. ) ;
#91318 = CARTESIAN_POINT ( 'NONE',  ( -111.0888070733315516, 1304.231242809270043, 299.9912356824837616 ) ) ;
#91319 = CARTESIAN_POINT ( 'NONE',  ( 40.52588777580712076, 1425.188750968595741, 269.1149643231569826 ) ) ;
#91320 = CARTESIAN_POINT ( 'NONE',  ( -19.95761699851187387, 1506.164913903586239, 189.0205224701858526 ) ) ;
#91321 = CARTESIAN_POINT ( 'NONE',  ( 20.61690388284639042, 1509.299818271619188, 189.0201435835461439 ) ) ;
#91322 = CARTESIAN_POINT ( 'NONE',  ( 8.652776089875690246, 1511.435001055579960, 203.7363227723449768 ) ) ;
#91323 = CARTESIAN_POINT ( 'NONE',  ( -61.39718882775409980, 1385.068252780349894, 247.0266603675090096 ) ) ;
#91324 = LINE ( 'NONE', #74542, #83707 ) ;
#91325 = CARTESIAN_POINT ( 'NONE',  ( -4.714156601264419599, 1508.551704408389924, 205.4956836294300047 ) ) ;
#91326 = EDGE_LOOP ( 'NONE', ( #108403, #74548, #9419, #23631 ) ) ;
#91327 = CARTESIAN_POINT ( 'NONE',  ( -28.81018896820719988, 1509.453431482950009, 208.7252267088939846 ) ) ;
#91328 = CARTESIAN_POINT ( 'NONE',  ( -15.92445961705290003, 1410.432587407550045, 226.6488369890140007 ) ) ;
#91330 = ORIENTED_EDGE ( 'NONE', *, *, #5020, .F. ) ;
#91329 = CARTESIAN_POINT ( 'NONE',  ( 12.45662858640000081, 1427.088122356749864, 206.6493127654890145 ) ) ;
#91331 = CARTESIAN_POINT ( 'NONE',  ( -11.82552473729999853, 1507.579552363830089, 183.2239286378979841 ) ) ;
#91332 = CARTESIAN_POINT ( 'NONE',  ( 40.27307890487595898, 1443.616175311578900, 137.1168156925720893 ) ) ;
#91333 = CARTESIAN_POINT ( 'NONE',  ( 21.59613673650000010, 1509.442267771630213, 226.5610156191980025 ) ) ;
#91334 = CARTESIAN_POINT ( 'NONE',  ( -109.4795670820000026, 1384.638871926420052, 311.2744876122590085 ) ) ;
#91335 = LINE ( 'NONE', #81818, #46456 ) ;
#91336 = CIRCLE ( 'NONE', #43068, 4.250000000000000000 ) ;
#91337 = CARTESIAN_POINT ( 'NONE',  ( 2.219943772349999733, 1464.863888256930068, 237.3912208446979832 ) ) ;
#91338 = EDGE_CURVE ( 'NONE', #7555, #66010, #53672, .T. ) ;
#91339 = CARTESIAN_POINT ( 'NONE',  ( 19.70825520289999844, 1410.962810032930065, 220.5533580383980166 ) ) ;
#91340 = B_SPLINE_SURFACE_WITH_KNOTS ( 'NONE', 5, 5, ( 
 ( #85216, #109347, #76838, #109884, #151, #58937, #68454, #17440, #85775, #9076, #43243, #18009, #35379, #10743, #1807, #29186, #86330, #53307, #96954, #69568, #104793 ),
 ( #20220, #70680, #54421, #28636, #77935, #1242, #103687, #20761, #87449, #52748, #2913, #26988, #44916, #46008, #61176, #88553, #105907, #95294, #79608, #37585, #9615 ),
 ( #79063, #18555, #86882, #10176, #44350, #78493, #61715, #35944, #70130, #80138, #43785, #104241, #62841, #37030, #28079, #27532, #95836, #11836, #19104, #2368, #3457 ),
 ( #63377, #71788, #36482, #97493, #62267, #96397, #19672, #53877, #88015, #11299, #45467, #71223, #105347, #81226, #48203, #106444, #72312, #39225, #46559, #72850, #80695 ),
 ( #5074, #4541, #90171, #99669, #4005, #31928, #55504, #14571, #74512, #99119, #29726, #30272, #39792, #38131, #63912, #98581, #21847, #82342, #98026, #47643, #12373 ),
 ( #57167, #13454, #107538, #64465, #14014, #40331, #81771, #21300, #73399, #89632, #56044, #47099, #12920, #5641, #73951, #38675, #30826, #106985, #65002, #108642, #22397 ) ),
 .UNSPECIFIED., .F., .F., .F.,
 ( 6, 6 ),
 ( 6, 3, 3, 3, 3, 3, 6 ),
 ( 1.704359096279999930, 13.41865417910000069 ),
 ( 27.98477882999999977, 34.32981118040000013, 36.68144354599999701, 37.85725972880000256, 39.03307591160000101, 39.85395972119999897, 40.67484353080000403 ),
 .UNSPECIFIED. ) ;
#91341 = CARTESIAN_POINT ( 'NONE',  ( -2.923659802470610192, 1410.372349471019788, 186.6137880374459996 ) ) ;
#91342 = CARTESIAN_POINT ( 'NONE',  ( -20.44684673909999617, 1467.336849514990035, 211.2727642411090017 ) ) ;
#91343 = CARTESIAN_POINT ( 'NONE',  ( -17.85622223500000061, 1424.491927465330036, 227.8867262256979984 ) ) ;
#91345 = CARTESIAN_POINT ( 'NONE',  ( 22.01621720475775135, 1506.474306125260682, 208.9595913853024456 ) ) ;
#91344 = CARTESIAN_POINT ( 'NONE',  ( 12.17073519972539941, 1499.730396604210000, 205.6506567772970016 ) ) ;
#91346 = FACE_OUTER_BOUND ( 'NONE', #48869, .T. ) ;
#91347 = CARTESIAN_POINT ( 'NONE',  ( -119.4939992282775023, 1358.631207110791138, 300.8926790057503240 ) ) ;
#91348 = EDGE_CURVE ( 'NONE', #75020, #72755, #39537, .T. ) ;
#91349 = CARTESIAN_POINT ( 'NONE',  ( 24.50927534411190933, 1509.771934658697091, 192.7779650040213539 ) ) ;
#91350 = CARTESIAN_POINT ( 'NONE',  ( -1.392294270230000075, 1415.872631189930189, 233.2008784669980059 ) ) ;
#91351 = CARTESIAN_POINT ( 'NONE',  ( -5.986709854329999914, 1361.264879806969930, 210.6218459616991936 ) ) ;
#91352 = EDGE_CURVE ( 'NONE', #83528, #33967, #84287, .T. ) ;
#91353 = CARTESIAN_POINT ( 'NONE',  ( 0.7356989345870019736, 1517.020847257979995, 205.6609797614169963 ) ) ;
#91354 = CARTESIAN_POINT ( 'NONE',  ( -5.351895964595500210, 1484.703362324490172, 183.6627706421859898 ) ) ;
#91355 = ORIENTED_EDGE ( 'NONE', *, *, #3509, .F. ) ;
#91356 = CIRCLE ( 'NONE', #52045, 30.13701971169416183 ) ;
#91357 = CARTESIAN_POINT ( 'NONE',  ( -109.1253053317170014, 1384.665560649159943, 311.2565095416410372 ) ) ;
#91358 = CARTESIAN_POINT ( 'NONE',  ( -4.241168549582178926, 1441.430627509509804, 162.5672745638440233 ) ) ;
#91360 = ORIENTED_EDGE ( 'NONE', *, *, #35240, .T. ) ;
#91359 = CARTESIAN_POINT ( 'NONE',  ( -68.71179394108339977, 1379.747778244289975, 280.3126260626940507 ) ) ;
#91361 = EDGE_CURVE ( 'NONE', #78418, #33692, #9134, .T. ) ;
#91362 = ORIENTED_EDGE ( 'NONE', *, *, #99531, .F. ) ;
#91363 = CARTESIAN_POINT ( 'NONE',  ( -8.640836516204634776, 1381.414239460393446, 218.0276686012663845 ) ) ;
#91364 = ORIENTED_EDGE ( 'NONE', *, *, #38006, .T. ) ;
#91365 = CARTESIAN_POINT ( 'NONE',  ( 1.318491153889610024, 1485.468798185310106, 220.9179226408149930 ) ) ;
#91366 = FACE_OUTER_BOUND ( 'NONE', #106541, .T. ) ;
#91368 = CARTESIAN_POINT ( 'NONE',  ( 16.24165198109999864, 1409.730207214729944, 192.2072427057979951 ) ) ;
#91367 = CARTESIAN_POINT ( 'NONE',  ( -20.59685312423998127, 1507.762914175841161, 190.3821643482645811 ) ) ;
#91369 = CARTESIAN_POINT ( 'NONE',  ( -2.865636847234999784, 1516.815173273089840, 210.2578502442970318 ) ) ;
#91370 = CARTESIAN_POINT ( 'NONE',  ( 40.14987069115329632, 1439.836753192460037, 136.5114502648049779 ) ) ;
#91371 = CARTESIAN_POINT ( 'NONE',  ( -106.8945970612549985, 1378.913060387289988, 307.0349506131610156 ) ) ;
#91372 = CARTESIAN_POINT ( 'NONE',  ( -2.330134118790000208, 1515.551704408389924, 212.9514660756190096 ) ) ;
#91373 = CARTESIAN_POINT ( 'NONE',  ( 17.11398521796633432, 1460.311162561034280, 228.6660193555352407 ) ) ;
#91374 = CARTESIAN_POINT ( 'NONE',  ( -31.92108011125334599, 1512.187213306747481, 220.9591791661900686 ) ) ;
#91375 = VECTOR ( 'NONE', #75876, 1000.000000000000000 ) ;
#91376 = CARTESIAN_POINT ( 'NONE',  ( 1.876675108085915644, 1395.978595326182813, 220.1335329578695621 ) ) ;
#91377 = ORIENTED_EDGE ( 'NONE', *, *, #17075, .T. ) ;
#91378 = CARTESIAN_POINT ( 'NONE',  ( 9.992001554820001630, 1491.422527302990147, 188.4943246008990059 ) ) ;
#91379 = CARTESIAN_POINT ( 'NONE',  ( -19.16952157780000121, 1456.627486491929858, 228.8719534504979833 ) ) ;
#91380 = VERTEX_POINT ( 'NONE', #85948 ) ;
#91381 = EDGE_LOOP ( 'NONE', ( #13803, #89457, #42, #103018 ) ) ;
#91382 = CARTESIAN_POINT ( 'NONE',  ( 13.41947731569904079, 1410.754602942108477, 228.3337818491096414 ) ) ;
#91383 = CARTESIAN_POINT ( 'NONE',  ( 18.19590854888164699, 1522.862737210649584, 238.2026672068774360 ) ) ;
#91384 = VECTOR ( 'NONE', #7701, 1000.000000000000000 ) ;
#91385 = CARTESIAN_POINT ( 'NONE',  ( 12.52351530970569904, 1500.052013425719906, 207.1430829055039737 ) ) ;
#91386 = CARTESIAN_POINT ( 'NONE',  ( -19.39503999260000100, 1507.708763760590045, 209.4440057405769835 ) ) ;
#91387 = CARTESIAN_POINT ( 'NONE',  ( -2.500000000000280220, 1439.222456145959995, 159.1125091106669913 ) ) ;
#91388 = EDGE_CURVE ( 'NONE', #74525, #95777, #100328, .T. ) ;
#91389 = CARTESIAN_POINT ( 'NONE',  ( 3.970164549720000213, 1515.569681836989957, 210.2459363763389888 ) ) ;
#91390 = CARTESIAN_POINT ( 'NONE',  ( -14.47191441250000032, 1379.648773486759865, 208.1784591346629725 ) ) ;
#91391 = CARTESIAN_POINT ( 'NONE',  ( 42.60628463550120415, 1443.705283444789984, 134.7402669369780028 ) ) ;
#91392 = CARTESIAN_POINT ( 'NONE',  ( -15.74179306318853833, 1484.201616316254785, 223.2977079293126224 ) ) ;
#91393 = CARTESIAN_POINT ( 'NONE',  ( 26.91754656130000001, 1437.398890514510185, 136.8530043402979857 ) ) ;
#91394 = ADVANCED_FACE ( 'NONE', ( #10336 ), #9787, .F. ) ;
#91395 = CARTESIAN_POINT ( 'NONE',  ( 3.877170719089999995, 1415.932617989529945, 191.1210336056979884 ) ) ;
#91396 = CARTESIAN_POINT ( 'NONE',  ( -77.91920755176590774, 1384.783552880790239, 280.1696958822980150 ) ) ;
#91397 = EDGE_LOOP ( 'NONE', ( #37808, #84595, #6737, #54562, #42193 ) ) ;
#91398 = CARTESIAN_POINT ( 'NONE',  ( 4.616272296565000488, 1517.030858226499959, 201.7868885755270014 ) ) ;
#91399 = CARTESIAN_POINT ( 'NONE',  ( 4.031168767865001001, 1516.805675336850072, 208.3649472324300120 ) ) ;
#91400 = VERTEX_POINT ( 'NONE', #42849 ) ;
#91401 = CARTESIAN_POINT ( 'NONE',  ( 40.88256439680969834, 1440.913060387330006, 268.3738206050749682 ) ) ;
#91402 = VECTOR ( 'NONE', #96395, 1000.000000000000000 ) ;
#91403 = CARTESIAN_POINT ( 'NONE',  ( -0.0005080901876549786828, 1451.974260998641057, 153.9770172106709936 ) ) ;
#91404 = ORIENTED_EDGE ( 'NONE', *, *, #80321, .T. ) ;
#91405 = CARTESIAN_POINT ( 'NONE',  ( 4.517196230222682019, 1522.051704408389924, 227.6318199458918343 ) ) ;
#91406 = CARTESIAN_POINT ( 'NONE',  ( 0.000000000000000000, 1511.187213306747708, 209.1218459616979999 ) ) ;
#91407 = CARTESIAN_POINT ( 'NONE',  ( -4.082703448014748382, 1515.071394417499505, 212.7081850046428713 ) ) ;
#91408 = DIRECTION ( 'NONE',  ( -0.2054769195713296304, 0.000000000000000000, -0.9786619618251631847 ) ) ;
#91409 = CARTESIAN_POINT ( 'NONE',  ( -5.615127104817688952, 1507.508085020990166, 198.8434247404759958 ) ) ;
#91410 = CARTESIAN_POINT ( 'NONE',  ( 12.84239221398829933, 1435.935692713660046, 150.8114773724069835 ) ) ;
#91411 = CARTESIAN_POINT ( 'NONE',  ( 30.02767535379999941, 1414.536195395429786, 266.6069031101980045 ) ) ;
#91412 = CARTESIAN_POINT ( 'NONE',  ( -12.40432178540000052, 1434.419968829250138, 147.8552690333980308 ) ) ;
#91413 = DIRECTION ( 'NONE',  ( -2.460711850760000078E-19, 5.183526052191769474E-17, 1.000000000000000000 ) ) ;
#91415 = CARTESIAN_POINT ( 'NONE',  ( -11.60004869885203505, 1422.462482050413655, 137.0350105543709844 ) ) ;
#91414 = CARTESIAN_POINT ( 'NONE',  ( 14.78718726039999787, 1460.545059401930075, 230.6966295517979688 ) ) ;
#91416 = CARTESIAN_POINT ( 'NONE',  ( 20.13561634019999858, 1473.995504141989841, 210.1093940072919963 ) ) ;
#91417 = DIRECTION ( 'NONE',  ( -1.040834085586083310E-14, 0.000000000000000000, 1.000000000000000000 ) ) ;
#91418 = VERTEX_POINT ( 'NONE', #52372 ) ;
#91419 = CIRCLE ( 'NONE', #244, 8.000000000000007105 ) ;
#91420 = B_SPLINE_CURVE_WITH_KNOTS ( 'NONE', 3,
 ( #59246, #93365, #50828, #3214, #18305, #11588, #96703, #96135, #60909, #78229, #19974, #62015, #1542, #107152, #38838, #78791 ),
 .UNSPECIFIED., .F., .F.,
 ( 4, 2, 1, 1, 2, 2, 2, 2, 4 ),
 ( 0.000000000000000000, 0.2500000000001725287, 0.3750000000000902056, 0.4375000000000508482, 0.4687499999998230860, 0.4999999999995953792, 0.6249999999999499289, 0.7500000000003045342, 1.000000000000000000 ),
 .UNSPECIFIED. ) ;
#91421 = DIRECTION ( 'NONE',  ( -1.000000000000000000, 0.000000000000000000, 0.000000000000000000 ) ) ;
#91422 = CARTESIAN_POINT ( 'NONE',  ( -0.06741725946591989316, 1508.620385720349987, 180.1145002095929897 ) ) ;
#91423 = CARTESIAN_POINT ( 'NONE',  ( 16.70757379908175722, 1449.396063251830583, 219.0502673354835679 ) ) ;
#91424 = CARTESIAN_POINT ( 'NONE',  ( 4.041472473744999405, 1516.858649670339901, 213.1514186109370144 ) ) ;
#91425 = CARTESIAN_POINT ( 'NONE',  ( 18.51562415000000072, 1509.322649222929840, 187.7614736601980212 ) ) ;
#91426 = CARTESIAN_POINT ( 'NONE',  ( -11.44617051164304833, 1425.796922195610705, 139.1405492985841477 ) ) ;
#91428 = ORIENTED_EDGE ( 'NONE', *, *, #14328, .F. ) ;
#91427 = CARTESIAN_POINT ( 'NONE',  ( -11.63277241116059990, 1501.279596332750089, 211.2803251540719884 ) ) ;
#91429 = CARTESIAN_POINT ( 'NONE',  ( -2.038646110889565932, 1525.960063244516959, 177.0579350083065435 ) ) ;
#91430 = CARTESIAN_POINT ( 'NONE',  ( 16.70417082779999873, 1456.998411956430118, 221.6179017295980032 ) ) ;
#91431 = CARTESIAN_POINT ( 'NONE',  ( -11.57526502019999981, 1432.244206860189934, 151.1962845448979920 ) ) ;
#91432 = CARTESIAN_POINT ( 'NONE',  ( 19.08296562770900096, 1456.929326075580093, 225.1994806392700070 ) ) ;
#91433 = CARTESIAN_POINT ( 'NONE',  ( -4.881006452805260132, 1440.913765093959910, 201.7555229531890291 ) ) ;
#91434 = DIRECTION ( 'NONE',  ( -1.000000000000000000, 0.000000000000000000, 0.000000000000000000 ) ) ;
#91435 = CARTESIAN_POINT ( 'NONE',  ( 16.83198307402578564, 1526.000688113713295, 182.3274564795797801 ) ) ;
#91436 = CARTESIAN_POINT ( 'NONE',  ( 12.40489012449999962, 1446.137994316120057, 188.0544017187980046 ) ) ;
#91438 = FACE_OUTER_BOUND ( 'NONE', #71034, .T. ) ;
#91437 = CARTESIAN_POINT ( 'NONE',  ( -20.58707005339999796, 1482.729478077029853, 226.3829017035980087 ) ) ;
#91439 = CARTESIAN_POINT ( 'NONE',  ( -1.687592144759999968, 1484.749778137530029, 182.6858646861979878 ) ) ;
#91440 = ORIENTED_EDGE ( 'NONE', *, *, #18594, .T. ) ;
#91441 = CARTESIAN_POINT ( 'NONE',  ( 7.322709686834999232, 1516.596789218710001, 205.8608388005369818 ) ) ;
#91442 = CARTESIAN_POINT ( 'NONE',  ( 7.054183505060000137, 1406.398142208129912, 266.9413180379979735 ) ) ;
#91443 = CARTESIAN_POINT ( 'NONE',  ( 38.64637139974560398, 1443.913060387190171, 137.1864063390110005 ) ) ;
#91444 = CARTESIAN_POINT ( 'NONE',  ( 10.95543255003150129, 1490.155657787360042, 208.9951350640439784 ) ) ;
#91445 = CARTESIAN_POINT ( 'NONE',  ( 22.91305534397972465, 1432.047512284617142, 216.2803340805854475 ) ) ;
#91446 = DIRECTION ( 'NONE',  ( 0.000000000000000000, 1.000000000000000000, 0.000000000000000000 ) ) ;
#91447 = CARTESIAN_POINT ( 'NONE',  ( 9.788553136239070085, 1435.243871060430138, 208.4607419252359932 ) ) ;
#91448 = VECTOR ( 'NONE', #68994, 1000.000000000000114 ) ;
#91449 = CARTESIAN_POINT ( 'NONE',  ( -8.881784197000000993E-16, 1392.213060387289943, 209.1218459616989946 ) ) ;
#91450 = CARTESIAN_POINT ( 'NONE',  ( -1.459574862452099886, 1450.689303299579933, 154.7904098955449967 ) ) ;
#91451 = CARTESIAN_POINT ( 'NONE',  ( -1.561820929657351309, 1450.950381850439953, 183.5281567525138655 ) ) ;
#91452 = LINE ( 'NONE', #22550, #49732 ) ;
#91453 = CARTESIAN_POINT ( 'NONE',  ( -2.034008778210000035, 1508.605352629489971, 220.7050406583989854 ) ) ;
#91454 = CARTESIAN_POINT ( 'NONE',  ( -11.62426067770000060, 1501.026510252989965, 213.4445963220190094 ) ) ;
#91455 = CARTESIAN_POINT ( 'NONE',  ( -17.83186622659999898, 1434.542072767570062, 214.3676144203579952 ) ) ;
#91456 = CARTESIAN_POINT ( 'NONE',  ( -27.08287658454329971, 1507.996869902240178, 211.2978356732120062 ) ) ;
#91457 = CARTESIAN_POINT ( 'NONE',  ( 2.500000002550000211, 1439.653804531360038, 157.1389828242980116 ) ) ;
#91458 = AXIS2_PLACEMENT_3D ( 'NONE', #36124, #69184, #1413 ) ;
#91459 = CARTESIAN_POINT ( 'NONE',  ( -3.436075876849999933, 1475.886457539630101, 267.2300234903979685 ) ) ;
#91460 = CARTESIAN_POINT ( 'NONE',  ( 20.20959865099471031, 1511.187213306747708, 182.0120230947219966 ) ) ;
#91461 = CARTESIAN_POINT ( 'NONE',  ( -8.377805553860001808, 1439.624828044090009, 206.1458839272790158 ) ) ;
#91462 = CARTESIAN_POINT ( 'NONE',  ( 17.71056690938649680, 1414.273744580000084, 224.2882958007120067 ) ) ;
#91463 = CARTESIAN_POINT ( 'NONE',  ( -51.76569597015449631, 1384.731644114589926, 265.3596788363910264 ) ) ;
#91464 = CARTESIAN_POINT ( 'NONE',  ( 16.78507865760100159, 1507.483738429089954, 193.5970331257109933 ) ) ;
#91465 = CARTESIAN_POINT ( 'NONE',  ( 12.04503635791889948, 1491.368323112810003, 206.7127955739260017 ) ) ;
#91466 = CARTESIAN_POINT ( 'NONE',  ( 32.05702909905449616, 1524.477587234266366, 216.6895769861147301 ) ) ;
#91467 = CARTESIAN_POINT ( 'NONE',  ( 8.566419661001074104, 1511.406468244436383, 203.9918518157900280 ) ) ;
#91468 = CARTESIAN_POINT ( 'NONE',  ( -20.12576653420000028, 1409.615867641330169, 201.4144580155179938 ) ) ;
#91469 = CIRCLE ( 'NONE', #66482, 1.000000000000000888 ) ;
#91470 = CARTESIAN_POINT ( 'NONE',  ( 12.91552263953340152, 1421.111598984989996, 204.2664607796000098 ) ) ;
#91471 = CARTESIAN_POINT ( 'NONE',  ( -30.65556899779999966, 1416.265499210330063, 269.9312797238980011 ) ) ;
#91472 = ADVANCED_FACE ( 'NONE', ( #68615 ), #106489, .T. ) ;
#91473 = ORIENTED_EDGE ( 'NONE', *, *, #45377, .T. ) ;
#91474 = CARTESIAN_POINT ( 'NONE',  ( -2.869563509691151371, 1410.390895325194833, 232.5635847210010070 ) ) ;
#91475 = CARTESIAN_POINT ( 'NONE',  ( -7.548952336147771724, 1510.510563530936906, 214.7720805601384768 ) ) ;
#91476 = CARTESIAN_POINT ( 'NONE',  ( -13.32685111460899918, 1469.522659984069833, 191.9925937506160096 ) ) ;
#91478 = CARTESIAN_POINT ( 'NONE',  ( -12.26117242810740038, 1377.986604079799918, 210.3392675169330346 ) ) ;
#91477 = CARTESIAN_POINT ( 'NONE',  ( 11.67374344909999984, 1426.737914103830008, 139.6438984324979913 ) ) ;
#91479 = CARTESIAN_POINT ( 'NONE',  ( 16.54281257266469751, 1524.843416604499225, 237.3982989049651167 ) ) ;
#91480 = CARTESIAN_POINT ( 'NONE',  ( -123.2094608543100094, 1377.418846546390114, 298.8629130685190489 ) ) ;
#91481 = CARTESIAN_POINT ( 'NONE',  ( -5.104341685840000586, 1454.049460953489870, 201.0800892362090053 ) ) ;
#91482 = CARTESIAN_POINT ( 'NONE',  ( 1.709384572955000126, 1517.224900789629828, 201.7820965968870155 ) ) ;
#91483 = CARTESIAN_POINT ( 'NONE',  ( 7.925563889120000205, 1426.364738259879914, 211.7377644087189879 ) ) ;
#91484 = CARTESIAN_POINT ( 'NONE',  ( -12.87605230667369405, 1398.294690222690406, 210.9476564090868749 ) ) ;
#91485 = CARTESIAN_POINT ( 'NONE',  ( 16.38335852923500013, 1512.258183966700017, 197.2512110842670268 ) ) ;
#91486 = CARTESIAN_POINT ( 'NONE',  ( -21.69813442400969805, 1417.904383893920112, 208.5544938348409687 ) ) ;
#91487 = CARTESIAN_POINT ( 'NONE',  ( -18.12558133263030058, 1378.944431349770184, 212.8996372240309825 ) ) ;
#91488 = CIRCLE ( 'NONE', #73687, 2.000000000000011102 ) ;
#91489 = CARTESIAN_POINT ( 'NONE',  ( 2.836810703500213027, 1368.016923498806364, 210.6218459617142003 ) ) ;
#91491 = ORIENTED_EDGE ( 'NONE', *, *, #42812, .T. ) ;
#91490 = CARTESIAN_POINT ( 'NONE',  ( -52.42853552719999755, 1379.742143313350198, 249.9106425961589935 ) ) ;
#91492 = VERTEX_POINT ( 'NONE', #54583 ) ;
#91494 = EDGE_CURVE ( 'NONE', #2433, #69308, #105516, .T. ) ;
#91493 = CARTESIAN_POINT ( 'NONE',  ( 11.45756101023500051, 1434.780485529720181, 151.4565597636700147 ) ) ;
#91495 = CARTESIAN_POINT ( 'NONE',  ( -12.38973388049999969, 1396.865112417229966, 211.4033042261380047 ) ) ;
#91496 = CARTESIAN_POINT ( 'NONE',  ( -20.64057905079999955, 1409.633845290530189, 214.6320756031479959 ) ) ;
#91497 = VERTEX_POINT ( 'NONE', #29340 ) ;
#91498 = CARTESIAN_POINT ( 'NONE',  ( -12.57974774915637717, 1445.046023591448829, 169.4706963785791061 ) ) ;
#91499 = LINE ( 'NONE', #81974, #6419 ) ;
#91500 = CARTESIAN_POINT ( 'NONE',  ( -15.20906659412241702, 1416.167321952329530, 211.8455853713288946 ) ) ;
#91502 = CARTESIAN_POINT ( 'NONE',  ( 17.93995879599999910, 1421.703940548830133, 225.5244287617980206 ) ) ;
#91501 = CARTESIAN_POINT ( 'NONE',  ( 2.175596292269999843, 1445.361571848690119, 200.0046556085490010 ) ) ;
#91503 = CARTESIAN_POINT ( 'NONE',  ( 1.315358370620000050, 1449.240786182220063, 183.5913257811980088 ) ) ;
#91504 = CARTESIAN_POINT ( 'NONE',  ( -5.534144808426719742, 1464.371868907480120, 199.5915608675260273 ) ) ;
#91505 = EDGE_CURVE ( 'NONE', #6406, #100495, #16291, .T. ) ;
#91506 = CARTESIAN_POINT ( 'NONE',  ( -17.35635886029999853, 1417.798318063129955, 207.1516956251389843 ) ) ;
#91507 = CARTESIAN_POINT ( 'NONE',  ( 10.75712941972539838, 1396.288707624410108, 206.5173657439860335 ) ) ;
#91508 = LINE ( 'NONE', #76361, #26556 ) ;
#91509 = CARTESIAN_POINT ( 'NONE',  ( 11.80251472770000021, 1427.996663069729948, 148.7256247452979778 ) ) ;
#91510 = CARTESIAN_POINT ( 'NONE',  ( 1.716045945209999868, 1509.007693206030126, 179.5167849949980052 ) ) ;
#91511 = ORIENTED_EDGE ( 'NONE', *, *, #8534, .T. ) ;
#91512 = CARTESIAN_POINT ( 'NONE',  ( 12.95810389287730047, 1435.988623967140029, 150.7629203163199918 ) ) ;
#91513 = VERTEX_POINT ( 'NONE', #89253 ) ;
#91514 = EDGE_LOOP ( 'NONE', ( #45769, #2356, #51821, #89587, #87428 ) ) ;
#91515 = CARTESIAN_POINT ( 'NONE',  ( -17.75009271329319915, 1468.179955452010063, 228.4966567787849954 ) ) ;
#91516 = CARTESIAN_POINT ( 'NONE',  ( -5.135155612019999261, 1464.351819601929947, 236.1467049461980139 ) ) ;
#91517 = CARTESIAN_POINT ( 'NONE',  ( -109.0049894526701024, 1387.725350813251225, 310.8181635293149725 ) ) ;
#91518 = CARTESIAN_POINT ( 'NONE',  ( 5.780861236055000241, 1516.783701990830195, 216.0610654530370027 ) ) ;
#91519 = DIRECTION ( 'NONE',  ( -0.2054769195713179730, -0.000000000000000000, -0.9786619618251657382 ) ) ;
#91520 = COLOUR_RGB ( '', 0.09019608, 0.27058824, 0.51372549) ;
#91521 = ORIENTED_EDGE ( 'NONE', *, *, #49492, .F. ) ;
#91522 = CARTESIAN_POINT ( 'NONE',  ( -11.41402558200000072, 1500.969830860790125, 208.5831166258960252 ) ) ;
#91523 = CARTESIAN_POINT ( 'NONE',  ( 2.500000000000000000, 1448.210448412289907, 170.5244215879980061 ) ) ;
#91524 = CARTESIAN_POINT ( 'NONE',  ( -51.56180980459999574, 1375.317619266380007, 241.8087128081590151 ) ) ;
#91525 = ADVANCED_FACE ( 'NONE', ( #37207 ), #46724, .T. ) ;
#91526 = ORIENTED_EDGE ( 'NONE', *, *, #80879, .F. ) ;
#91527 = CARTESIAN_POINT ( 'NONE',  ( -0.01327408612949850138, 1516.939877939420057, 205.6663500982469941 ) ) ;
#91528 = ORIENTED_EDGE ( 'NONE', *, *, #71923, .F. ) ;
#91529 = CARTESIAN_POINT ( 'NONE',  ( -5.781585816274999345, 1516.939646076049939, 209.1342929058909874 ) ) ;
#91530 = CARTESIAN_POINT ( 'NONE',  ( -20.18532072600000049, 1508.602711282829887, 229.1243101363980088 ) ) ;
#91531 = CARTESIAN_POINT ( 'NONE',  ( -29.88849338478334161, 1419.495351112958360, 269.4696191733103205 ) ) ;
#91532 = CARTESIAN_POINT ( 'NONE',  ( 6.088832710385000624, 1511.778199792620171, 217.5949148583070212 ) ) ;
#91534 = ORIENTED_EDGE ( 'NONE', *, *, #80321, .F. ) ;
#91533 = CARTESIAN_POINT ( 'NONE',  ( -1.190628175403880107, 1414.913057834419988, 226.0043277146490084 ) ) ;
#91535 = CARTESIAN_POINT ( 'NONE',  ( 24.59498516420000058, 1440.913044728469913, 213.3385258196480265 ) ) ;
#91536 = CARTESIAN_POINT ( 'NONE',  ( -27.79719865735470208, 1440.913060392109855, 230.3218327024129906 ) ) ;
#91537 = CARTESIAN_POINT ( 'NONE',  ( -43.14264924749999608, 1384.135846318449921, 247.4751904553590123 ) ) ;
#91538 = CARTESIAN_POINT ( 'NONE',  ( 20.58082067220000155, 1494.260204254890141, 204.7904675245989665 ) ) ;
#91539 = CIRCLE ( 'NONE', #32548, 2.000000000000002220 ) ;
#91540 = CARTESIAN_POINT ( 'NONE',  ( 4.958608739790000719, 1408.764127645530152, 270.4263178542980768 ) ) ;
#91541 = CARTESIAN_POINT ( 'NONE',  ( -4.030514550714999977, 1516.901952101700090, 213.7446888144170032 ) ) ;
#91542 = CARTESIAN_POINT ( 'NONE',  ( 22.69544225309999774, 1409.705575941829920, 209.0104250642420141 ) ) ;
#91543 = CARTESIAN_POINT ( 'NONE',  ( -21.68655196239999938, 1509.722744064730023, 188.6979275785979837 ) ) ;
#91544 = CARTESIAN_POINT ( 'NONE',  ( -1.349081561059999990, 1443.127676870989944, 219.0403161255090083 ) ) ;
#91545 = CARTESIAN_POINT ( 'NONE',  ( -7.710855588274700523, 1516.603953730829971, 210.3964488831069843 ) ) ;
#91546 = CARTESIAN_POINT ( 'NONE',  ( -7.710967015764999211, 1516.608208975040043, 210.2506035313070072 ) ) ;
#91547 = CARTESIAN_POINT ( 'NONE',  ( -22.08327125186908191, 1523.604703353109699, 233.8169256665491105 ) ) ;
#91548 = CARTESIAN_POINT ( 'NONE',  ( 0.09565136837490001431, 1420.220989488129817, 183.9056119367980102 ) ) ;
#91549 = CARTESIAN_POINT ( 'NONE',  ( -11.67160011230928340, 1486.022816546380454, 184.5451946457169186 ) ) ;
#91551 = ORIENTED_EDGE ( 'NONE', *, *, #9807, .F. ) ;
#91550 = CARTESIAN_POINT ( 'NONE',  ( -72.88336126909999280, 1389.495380267770088, 278.2578877944589522 ) ) ;
#91553 = CIRCLE ( 'NONE', #66559, 39.37709583113206691 ) ;
#91552 = CARTESIAN_POINT ( 'NONE',  ( -41.62168732680330407, 1385.172644076110146, 245.0246584883539924 ) ) ;
#91554 = CARTESIAN_POINT ( 'NONE',  ( 45.31156206859999713, 1446.488581015689988, 266.2044087351980011 ) ) ;
#91555 = DIRECTION ( 'NONE',  ( 0.4794255386042019507, 0.000000000000000000, -0.8775825618903732028 ) ) ;
#91556 = B_SPLINE_CURVE_WITH_KNOTS ( 'NONE', 3,
 ( #42884, #68651, #9821, #51275, #102752, #15994, #84856, #110079, #110629, #69199, #25500, #51841, #59691, #52404, #94935, #103306, #7613, #349, #93803, #41769, #50196, #8156, #33354, #17080, #67549 ),
 .UNSPECIFIED., .F., .F.,
 ( 4, 1, 1, 2, 2, 2, 1, 2, 2, 2, 2, 2, 2, 4 ),
 ( 0.000000000000000000, 0.1250000000001981193, 0.1875000000002736422, 0.2187500000002864931, 0.2500000000002993716, 0.3750000000003361200, 0.4375000000003544387, 0.4687500000003027578, 0.5000000000002510214, 0.6250000000002813305, 0.6875000000002928768, 0.7500000000003043121, 0.8750000000001521006, 1.000000000000000000 ),
 .UNSPECIFIED. ) ;
#91557 = CARTESIAN_POINT ( 'NONE',  ( -3.331783404088239919, 1517.151704408390060, 220.8088060444078451 ) ) ;
#91558 = CARTESIAN_POINT ( 'NONE',  ( -5.451409632509999881, 1437.905383012069933, 154.7243395035980029 ) ) ;
#91559 = CARTESIAN_POINT ( 'NONE',  ( 11.67048048849999908, 1421.742781192700249, 203.8252195604689803 ) ) ;
#91560 = CARTESIAN_POINT ( 'NONE',  ( 0.3987454328862090058, 1452.975505999449979, 183.2778484764669997 ) ) ;
#91562 = CARTESIAN_POINT ( 'NONE',  ( -8.861701196289999416, 1384.879576664679917, 218.6850102892290124 ) ) ;
#91561 = CARTESIAN_POINT ( 'NONE',  ( 5.780232077335000440, 1516.760434454289907, 216.4486414936069991 ) ) ;
#91563 = CARTESIAN_POINT ( 'NONE',  ( 0.8871466948159980603, 1460.711025077289833, 228.7960624615990071 ) ) ;
#91564 = CARTESIAN_POINT ( 'NONE',  ( 10.04184886183580083, 1469.459372728499829, 207.3535612217320079 ) ) ;
#91565 = VERTEX_POINT ( 'NONE', #47257 ) ;
#91566 = CARTESIAN_POINT ( 'NONE',  ( -1.130607502004999931, 1516.632821972880038, 202.5736453444569918 ) ) ;
#91567 = CARTESIAN_POINT ( 'NONE',  ( -16.88678284756500148, 1513.362623229679912, 222.0540973537669913 ) ) ;
#91568 = VECTOR ( 'NONE', #56593, 1000.000000000000227 ) ;
#91569 = CARTESIAN_POINT ( 'NONE',  ( -0.1694244116599999961, 1487.208880437030075, 230.4477740473979850 ) ) ;
#91570 = CARTESIAN_POINT ( 'NONE',  ( 23.13311796429999845, 1449.197330723620098, 218.1771922301180098 ) ) ;
#91571 =( BOUNDED_CURVE ( )  B_SPLINE_CURVE ( 3, ( #33859, #85353, #110574, #102696 ),
 .UNSPECIFIED., .F., .F. ) 
 B_SPLINE_CURVE_WITH_KNOTS ( ( 4, 4 ),
 ( 1.083108237977496113, 1.126222521644246077 ),
 .UNSPECIFIED. ) 
 CURVE ( )  GEOMETRIC_REPRESENTATION_ITEM ( )  RATIONAL_B_SPLINE_CURVE ( ( 1.000000000000000000, 0.9998451025440023843, 0.9998451025440023843, 1.000000000000000000 ) ) 
 REPRESENTATION_ITEM ( '' )  );
#91572 = CARTESIAN_POINT ( 'NONE',  ( -12.78943302956389871, 1502.708798875820094, 209.0180534851929792 ) ) ;
#91573 = CARTESIAN_POINT ( 'NONE',  ( 8.380001589455886801, 1424.398767409684297, 195.8291005401241591 ) ) ;
#91574 = VECTOR ( 'NONE', #22450, 1000.000000000000000 ) ;
#91575 = CARTESIAN_POINT ( 'NONE',  ( 25.25200551730000242, 1450.804230319249882, 137.6134878989979882 ) ) ;
#91576 = CARTESIAN_POINT ( 'NONE',  ( 15.58582549078360380, 1420.996909499524236, 227.6524987713947894 ) ) ;
#91577 = CARTESIAN_POINT ( 'NONE',  ( -38.64637139473789773, 1443.913060387190171, 137.1864063576500143 ) ) ;
#91578 = CARTESIAN_POINT ( 'NONE',  ( -19.44347141579999771, 1426.034560796430014, 223.5248983639980054 ) ) ;
#91579 = CARTESIAN_POINT ( 'NONE',  ( -28.97201236651673995, 1467.320980035921593, 269.3759728919557688 ) ) ;
#91580 = CARTESIAN_POINT ( 'NONE',  ( -105.3239982070000025, 1388.772974685380177, 299.3169349243589750 ) ) ;
#91581 = CARTESIAN_POINT ( 'NONE',  ( 12.71733191150000053, 1509.357159403529977, 183.2206200378979872 ) ) ;
#91582 = CARTESIAN_POINT ( 'NONE',  ( -106.1567761860000019, 1391.062835315139864, 301.1121260340589743 ) ) ;
#91583 = CARTESIAN_POINT ( 'NONE',  ( -35.02259794696599471, 1457.750285243617100, 269.5318678299763064 ) ) ;
#91584 = ORIENTED_EDGE ( 'NONE', *, *, #22823, .F. ) ;
#91585 = DIRECTION ( 'NONE',  ( 1.755985294532469921E-16, -1.000000000000000000, 1.338183447452831989E-16 ) ) ;
#91586 = CARTESIAN_POINT ( 'NONE',  ( 6.599306557268372231, 1506.776553301877129, 187.7051843307115462 ) ) ;
#91587 = CARTESIAN_POINT ( 'NONE',  ( -17.43549125882602979, 1525.211477436245787, 237.2113384875502788 ) ) ;
#91588 = CARTESIAN_POINT ( 'NONE',  ( -0.2027342012590000186, 1416.110316472029808, 233.5455375878979964 ) ) ;
#91589 = CARTESIAN_POINT ( 'NONE',  ( -13.42860621949387934, 1443.470021403052897, 187.0641147421139578 ) ) ;
#91590 = CARTESIAN_POINT ( 'NONE',  ( -9.956881614119650337, 1438.965782279799896, 209.6194444277939795 ) ) ;
#91591 = CARTESIAN_POINT ( 'NONE',  ( -4.077241479695540960, 1515.224507089990084, 212.7046478782430086 ) ) ;
#91592 = CARTESIAN_POINT ( 'NONE',  ( -3.565261586666695681, 1415.863973584654332, 232.5973463957437843 ) ) ;
#91593 = LINE ( 'NONE', #22701, #103327 ) ;
#91594 = DIRECTION ( 'NONE',  ( 1.000000000000000000, 0.000000000000000000, 0.000000000000000000 ) ) ;
#91595 = CARTESIAN_POINT ( 'NONE',  ( -12.53380499174499896, 1442.773887286369927, 169.4755105688890069 ) ) ;
#91597 = EDGE_LOOP ( 'NONE', ( #95592, #32594, #85118, #59758 ) ) ;
#91596 = CARTESIAN_POINT ( 'NONE',  ( 21.38516915557965703, 1512.187213306747481, 180.3939891059721106 ) ) ;
#91598 = CARTESIAN_POINT ( 'NONE',  ( 0.05152562430226129836, 1416.529254608160045, 190.9681162060270196 ) ) ;
#91599 = CARTESIAN_POINT ( 'NONE',  ( 21.94594828856675051, 1509.533994805570501, 226.8419239637491955 ) ) ;
#91600 = ORIENTED_EDGE ( 'NONE', *, *, #73887, .F. ) ;
#91601 = ORIENTED_EDGE ( 'NONE', *, *, #110159, .T. ) ;
#91602 = CARTESIAN_POINT ( 'NONE',  ( 16.93365818059630001, 1414.971717244350202, 209.8484561376429838 ) ) ;
#91603 = CARTESIAN_POINT ( 'NONE',  ( -20.07149347155893437, 1526.186458717540972, 233.0642689910355898 ) ) ;
#91605 = CARTESIAN_POINT ( 'NONE',  ( -25.74056221470000239, 1442.596569739780080, 220.8687942055980216 ) ) ;
#91604 = CARTESIAN_POINT ( 'NONE',  ( 41.26157930654738237, 1435.022522197726857, 269.6335040890825780 ) ) ;
#91606 = CARTESIAN_POINT ( 'NONE',  ( -6.344682030749999591, 1447.083671391689904, 215.8265176690789815 ) ) ;
#91607 = CARTESIAN_POINT ( 'NONE',  ( -11.88353474240000018, 1433.300648518049911, 150.2496884404980051 ) ) ;
#91608 = CARTESIAN_POINT ( 'NONE',  ( -15.69795926856320101, 1521.951704408389787, 195.4758181589010064 ) ) ;
#91609 = CARTESIAN_POINT ( 'NONE',  ( 27.15450531368009734, 1482.666413628910050, 209.4389354641179750 ) ) ;
#91610 = CARTESIAN_POINT ( 'NONE',  ( -26.84000540299999926, 1441.581970623780080, 137.4710795974980329 ) ) ;
#91611 = CARTESIAN_POINT ( 'NONE',  ( -14.40908221889993790, 1429.715078873349512, 222.2182523075439633 ) ) ;
#91612 = CARTESIAN_POINT ( 'NONE',  ( -4.378216884482949212, 1453.707746088449994, 199.6107954155660025 ) ) ;
#91613 = CARTESIAN_POINT ( 'NONE',  ( 1.940237629179999868, 1450.366509861609757, 181.9011059340980125 ) ) ;
#91614 = CARTESIAN_POINT ( 'NONE',  ( 7.970805622722147099, 1364.587178592252030, 208.3718459617061285 ) ) ;
#91615 = CARTESIAN_POINT ( 'NONE',  ( -10.85473188425545565, 1509.417389448126414, 237.0896451841293526 ) ) ;
#91617 = ORIENTED_EDGE ( 'NONE', *, *, #77428, .F. ) ;
#91616 = CARTESIAN_POINT ( 'NONE',  ( 1.565460387769590331E-08, 1407.727994899569921, 263.5611240349619493 ) ) ;
#91618 = VERTEX_POINT ( 'NONE', #20378 ) ;
#91619 = EDGE_CURVE ( 'NONE', #96103, #70084, #107515, .T. ) ;
#91620 = CARTESIAN_POINT ( 'NONE',  ( -11.82802681128099920, 1429.780949742419807, 149.3576024833930092 ) ) ;
#91621 = CARTESIAN_POINT ( 'NONE',  ( -13.58959795930000070, 1505.039793835389901, 227.7961552795990201 ) ) ;
#91622 = CARTESIAN_POINT ( 'NONE',  ( -6.437126621210000010, 1473.252205434630241, 270.3863109987980238 ) ) ;
#91623 = CARTESIAN_POINT ( 'NONE',  ( -2.876354336597070294, 1474.536642632726171, 218.9936859356158152 ) ) ;
#91624 = CARTESIAN_POINT ( 'NONE',  ( -124.0634771228999682, 1314.643966242389070, 301.4990132218018175 ) ) ;
#91625 = LINE ( 'NONE', #55296, #34032 ) ;
#91626 = CARTESIAN_POINT ( 'NONE',  ( 0.000000000000000000, 1405.413060387330006, 209.1218459616979999 ) ) ;
#91627 = CARTESIAN_POINT ( 'NONE',  ( 7.105427357599999217E-15, 1405.913060387330006, 137.0999999980979851 ) ) ;
#91628 = EDGE_CURVE ( 'NONE', #56546, #11723, #36651, .T. ) ;
#91629 = LINE ( 'NONE', #14905, #12705 ) ;
#91630 = CARTESIAN_POINT ( 'NONE',  ( -3.084096054229999773, 1457.182013962589963, 218.2582502859689839 ) ) ;
#91631 = CARTESIAN_POINT ( 'NONE',  ( 9.984115569220000097, 1365.258395869459946, 207.6218459616989946 ) ) ;
#91632 = CARTESIAN_POINT ( 'NONE',  ( -28.98944848162919996, 1413.705768742049941, 268.7096924078339839 ) ) ;
#91633 = ORIENTED_EDGE ( 'NONE', *, *, #105010, .T. ) ;
#91634 = CARTESIAN_POINT ( 'NONE',  ( -4.329358020582379396, 1515.068258693859889, 210.7645756910659998 ) ) ;
#91635 = ORIENTED_EDGE ( 'NONE', *, *, #83599, .F. ) ;
#91636 = EDGE_LOOP ( 'NONE', ( #18638, #29687, #19558, #27246, #100720 ) ) ;
#91637 = CARTESIAN_POINT ( 'NONE',  ( -6.933616859135000254, 1516.548716157039962, 211.4141532006069895 ) ) ;
#91638 = CARTESIAN_POINT ( 'NONE',  ( -8.582505635693420842, 1448.408617315599940, 212.2769557201809789 ) ) ;
#91639 = CARTESIAN_POINT ( 'NONE',  ( 41.62830255093239629, 1444.039180007019922, 135.9573986949209825 ) ) ;
#91641 = FACE_OUTER_BOUND ( 'NONE', #65455, .T. ) ;
#91640 = CARTESIAN_POINT ( 'NONE',  ( 5.786527562335000319, 1517.025653221279981, 212.5728793591970032 ) ) ;
#91642 = CARTESIAN_POINT ( 'NONE',  ( -9.692726333870000488, 1440.427639384229906, 186.8581189109980301 ) ) ;
#91643 = AXIS2_PLACEMENT_3D ( 'NONE', #66533, #83850, #74378 ) ;
#91644 = CARTESIAN_POINT ( 'NONE',  ( -18.58720762869999987, 1416.311719779230089, 208.5274638254259969 ) ) ;
#91645 = ORIENTED_EDGE ( 'NONE', *, *, #57841, .T. ) ;
#91646 = CARTESIAN_POINT ( 'NONE',  ( -26.49726434420000132, 1436.728585065589868, 136.8015681357979929 ) ) ;
#91647 = CARTESIAN_POINT ( 'NONE',  ( -4.036748876935000396, 1516.667393516340098, 202.1854475764570225 ) ) ;
#91648 = B_SPLINE_CURVE_WITH_KNOTS ( 'NONE', 3,
 ( #106129, #20442, #98269, #90969, #3697, #56836, #13140, #38359, #31063, #39477 ),
 .UNSPECIFIED., .F., .F.,
 ( 4, 2, 2, 2, 4 ),
 ( 3.469446951953614189E-17, 0.0007406479101619073066, 0.001481295820323779919, 0.002221943730485652531, 0.002962591640647525143 ),
 .UNSPECIFIED. ) ;
#91649 = CARTESIAN_POINT ( 'NONE',  ( -41.14893945019565535, 1446.681898757845147, 135.2730607365670608 ) ) ;
#91650 = CARTESIAN_POINT ( 'NONE',  ( 0.9227939322070656258, 1508.990480019933557, 238.8126630289496575 ) ) ;
#91651 = CARTESIAN_POINT ( 'NONE',  ( -27.35670215475310130, 1417.239247989339901, 269.9340778386260240 ) ) ;
#91652 = CARTESIAN_POINT ( 'NONE',  ( -21.01415622427472485, 1517.151704408390060, 217.3717009491090835 ) ) ;
#91653 = CARTESIAN_POINT ( 'NONE',  ( -5.033438044520000432, 1397.146222143329851, 197.2622438200980071 ) ) ;
#91655 = ORIENTED_EDGE ( 'NONE', *, *, #104765, .F. ) ;
#91654 = CARTESIAN_POINT ( 'NONE',  ( 30.47385413848734004, 1525.394081235439444, 196.7421045368866146 ) ) ;
#91656 = ORIENTED_EDGE ( 'NONE', *, *, #39222, .F. ) ;
#91657 = CARTESIAN_POINT ( 'NONE',  ( 0.3552831700869999998, 1450.900653625639961, 181.9147599137979796 ) ) ;
#91658 = CARTESIAN_POINT ( 'NONE',  ( 3.809629103879523804, 1425.717714542633303, 185.2543070201454043 ) ) ;
#91659 = CARTESIAN_POINT ( 'NONE',  ( 10.91833819165210073, 1460.842557474800060, 208.3727220096430131 ) ) ;
#91660 = CARTESIAN_POINT ( 'NONE',  ( -24.46729980500000323, 1435.535532743930162, 137.3091962579979963 ) ) ;
#91661 = CARTESIAN_POINT ( 'NONE',  ( -0.4542904894729999921, 1486.188528289530041, 181.7644461267980205 ) ) ;
#91662 = CARTESIAN_POINT ( 'NONE',  ( -4.026614517785000125, 1516.699825673279975, 210.8361802174170236 ) ) ;
#91663 = CARTESIAN_POINT ( 'NONE',  ( 3.062858194097104914, 1458.818553845532279, 199.9951087153910976 ) ) ;
#91664 = CARTESIAN_POINT ( 'NONE',  ( 5.449707646490000279, 1437.831544062859848, 154.7230940508980268 ) ) ;
#91665 = CARTESIAN_POINT ( 'NONE',  ( 8.472423600081759432, 1438.684924725989958, 211.2764949506089920 ) ) ;
#91666 = DIRECTION ( 'NONE',  ( -1.000000000000000000, -5.823966869780190178E-19, 4.137698748469999823E-18 ) ) ;
#91667 = CARTESIAN_POINT ( 'NONE',  ( 8.100204432595001336, 1511.336728379370243, 204.5829771873069944 ) ) ;
#91668 = CARTESIAN_POINT ( 'NONE',  ( -7.339749373344999661, 1517.224900789629828, 207.4124613591469881 ) ) ;
#91669 = ORIENTED_EDGE ( 'NONE', *, *, #96732, .T. ) ;
#91670 = CARTESIAN_POINT ( 'NONE',  ( -2.745249273916440469, 1451.958939284520056, 184.7272525765399962 ) ) ;
#91671 = CARTESIAN_POINT ( 'NONE',  ( -9.522283751578990874, 1439.330121708799879, 208.4248680932010132 ) ) ;
#91672 = CARTESIAN_POINT ( 'NONE',  ( -19.60719674227114240, 1457.056223723324820, 225.8784467642674656 ) ) ;
#91673 = EDGE_LOOP ( 'NONE', ( #13010, #51382, #90079, #23433, #67861 ) ) ;
#91674 = CARTESIAN_POINT ( 'NONE',  ( -3.232732302729357521, 1524.860077346004800, 241.7126682117879284 ) ) ;
#91675 = CARTESIAN_POINT ( 'NONE',  ( -22.66501075923255826, 1509.725766826326435, 228.1954490747540376 ) ) ;
#91676 = CARTESIAN_POINT ( 'NONE',  ( -4.148978217093812759, 1439.755697323768118, 185.4934640260758556 ) ) ;
#91677 = CARTESIAN_POINT ( 'NONE',  ( -7.012921583605000286, 1508.551704408389924, 209.1218459511669892 ) ) ;
#91678 = CARTESIAN_POINT ( 'NONE',  ( 24.13017307760000207, 1452.070412388429986, 136.4016798020979877 ) ) ;
#91679 = CARTESIAN_POINT ( 'NONE',  ( 3.472242611860356210, 1450.898212748911419, 184.0506856000464779 ) ) ;
#91680 = CARTESIAN_POINT ( 'NONE',  ( 6.289965333610000542, 1487.835111632490225, 199.7689564727890001 ) ) ;
#91681 = CARTESIAN_POINT ( 'NONE',  ( 2.387854443607448918, 1426.854124017601634, 138.5187392187245052 ) ) ;
#91682 = CARTESIAN_POINT ( 'NONE',  ( 23.07346110646793491, 1450.308246357729104, 217.9087771107495541 ) ) ;
#91683 = CARTESIAN_POINT ( 'NONE',  ( -11.94206337009999963, 1438.199233188169956, 150.9847479746979957 ) ) ;
#91684 = CARTESIAN_POINT ( 'NONE',  ( -8.888009947380730580, 1385.310821826299843, 218.6609850379070110 ) ) ;
#91685 = CARTESIAN_POINT ( 'NONE',  ( -6.940473372275000052, 1516.833525648419936, 215.6778681647369922 ) ) ;
#91686 = ORIENTED_EDGE ( 'NONE', *, *, #39244, .F. ) ;
#91687 = CARTESIAN_POINT ( 'NONE',  ( -17.28245522079999930, 1417.580815317299994, 206.4386048391490078 ) ) ;
#91688 = DIRECTION ( 'NONE',  ( 3.446748568029901836E-05, -0.9328683086395049839, -0.3602175974991528862 ) ) ;
#91689 = CARTESIAN_POINT ( 'NONE',  ( -16.33552025180029688, 1508.551704408389924, 213.4320397940620069 ) ) ;
#91690 = CARTESIAN_POINT ( 'NONE',  ( -16.32932620218339892, 1508.453868990269939, 214.1093932417330166 ) ) ;
#91691 = EDGE_CURVE ( 'NONE', #78256, #46740, #32321, .T. ) ;
#91692 = CARTESIAN_POINT ( 'NONE',  ( -3.028748347090000070, 1475.522729171590072, 219.1245829792990207 ) ) ;
#91693 = CARTESIAN_POINT ( 'NONE',  ( -20.86254339170000094, 1504.682062816289999, 214.2159060785090219 ) ) ;
#91694 = CARTESIAN_POINT ( 'NONE',  ( 11.60004869885203505, 1426.109591897770542, 139.1549358429673759 ) ) ;
#91695 = DIRECTION ( 'NONE',  ( 0.000000000000000000, 0.000000000000000000, -1.000000000000000000 ) ) ;
#91696 = B_SPLINE_CURVE_WITH_KNOTS ( 'NONE', 3,
 ( #110783, #25102, #49789, #34074, #109684, #57654, #50887, #83923, #101810, #59308, #93421, #75549, #42472, #83364, #50353, #108577, #32428, #91766, #68267 ),
 .UNSPECIFIED., .F., .F.,
 ( 4, 3, 3, 3, 3, 3, 4 ),
 ( -1.000000000000000000, -0.7168501403031710684, -0.3505194570518059827, -0.001863983869921592706, 0.3397317646628350563, 0.6718016826570070155, 1.000000000000000000 ),
 .UNSPECIFIED. ) ;
#91697 = CARTESIAN_POINT ( 'NONE',  ( 17.14350470404602333, 1422.299115860800157, 226.7520998961785494 ) ) ;
#91698 = EDGE_CURVE ( 'NONE', #77826, #5707, #108808, .T. ) ;
#91699 = CARTESIAN_POINT ( 'NONE',  ( -0.9914680223604751541, 1455.336337171600235, 198.6483182256660029 ) ) ;
#91700 = DIRECTION ( 'NONE',  ( -0.000000000000000000, -1.000000000000000000, -0.000000000000000000 ) ) ;
#91702 = EDGE_CURVE ( 'NONE', #100110, #105489, #55675, .T. ) ;
#91701 = CARTESIAN_POINT ( 'NONE',  ( 28.40112187179950354, 1440.913060387299993, 232.7382060992320021 ) ) ;
#91704 = CARTESIAN_POINT ( 'NONE',  ( 4.327511837212730583, 1515.138761592180117, 208.5315405873499799 ) ) ;
#91703 = CARTESIAN_POINT ( 'NONE',  ( -10.08495433981949851, 1472.385695682990217, 210.5310355009019929 ) ) ;
#91705 = CARTESIAN_POINT ( 'NONE',  ( 12.90626675129999867, 1419.889181702930046, 222.0924173487979658 ) ) ;
#91706 = ORIENTED_EDGE ( 'NONE', *, *, #57560, .T. ) ;
#91707 = ORIENTED_EDGE ( 'NONE', *, *, #30538, .F. ) ;
#91708 = CARTESIAN_POINT ( 'NONE',  ( 10.68372146313839899, 1480.504181365129853, 209.2647601501510053 ) ) ;
#91709 = CARTESIAN_POINT ( 'NONE',  ( -19.67951034195003146, 1485.238740488470739, 190.3370758437304175 ) ) ;
#91710 = CARTESIAN_POINT ( 'NONE',  ( -0.3788383082595139784, 1408.926289712549988, 186.6322538385570056 ) ) ;
#91711 = CARTESIAN_POINT ( 'NONE',  ( 8.890886715069999724, 1425.078558200960060, 195.7078080160990226 ) ) ;
#91712 = CARTESIAN_POINT ( 'NONE',  ( -230.7985005798999794, 11216.44053380570040, 2175.332171792929785 ) ) ;
#91713 = CARTESIAN_POINT ( 'NONE',  ( 14.43289921540000087, 1509.539432541030010, 235.4218729623979982 ) ) ;
#91714 = CARTESIAN_POINT ( 'NONE',  ( -31.33756686635731015, 1523.580204110584191, 221.9021554030055938 ) ) ;
#91715 = CARTESIAN_POINT ( 'NONE',  ( -52.16017755504229569, 1383.808392896499981, 265.7696805365019941 ) ) ;
#91716 = CARTESIAN_POINT ( 'NONE',  ( -4.461625834204999919, 1510.696675236759802, 201.5656797203170072 ) ) ;
#91717 = DIRECTION ( 'NONE',  ( -1.755985294532464991E-16, 1.000000000000000000, -1.338183447452830017E-16 ) ) ;
#91718 = CARTESIAN_POINT ( 'NONE',  ( -11.77312369862629993, 1501.973685400810155, 208.8494367388649948 ) ) ;
#91719 = CARTESIAN_POINT ( 'NONE',  ( 10.58757398251879955, 1491.532463854900016, 212.1720164327929865 ) ) ;
#91721 = VERTEX_POINT ( 'NONE', #109376 ) ;
#91720 = DIRECTION ( 'NONE',  ( 5.204170427930416866E-14, 0.000000000000000000, 1.000000000000000000 ) ) ;
#91722 = CARTESIAN_POINT ( 'NONE',  ( 31.50799703744283420, 1526.382868172863937, 216.4233194664827238 ) ) ;
#91723 = CARTESIAN_POINT ( 'NONE',  ( -49.74528571340000838, 1383.812288545099818, 260.8378110853589646 ) ) ;
#91724 = CARTESIAN_POINT ( 'NONE',  ( -2.762666289370000250, 1431.313464822989999, 217.0512884656089909 ) ) ;
#91725 = ORIENTED_EDGE ( 'NONE', *, *, #89051, .T. ) ;
#91726 = VERTEX_POINT ( 'NONE', #57873 ) ;
#91727 = EDGE_CURVE ( 'NONE', #21912, #88646, #6349, .T. ) ;
#91728 = CARTESIAN_POINT ( 'NONE',  ( -7.614648265717109510, 1386.000035739249824, 218.9991509990680072 ) ) ;
#91729 = CYLINDRICAL_SURFACE ( 'NONE', #60525, 4.999999999999991118 ) ;
#91731 = CARTESIAN_POINT ( 'NONE',  ( -16.50400130224786466, 1525.907212628473644, 181.9890130758379030 ) ) ;
#91730 = CYLINDRICAL_SURFACE ( 'NONE', #85351, 1.749999999999997558 ) ;
#91732 = CARTESIAN_POINT ( 'NONE',  ( -8.170216832330000400, 1462.724072430790102, 203.3866392159690122 ) ) ;
#91733 = CARTESIAN_POINT ( 'NONE',  ( -106.9986950340000078, 1380.006134006080174, 299.5043260916589816 ) ) ;
#91734 = CARTESIAN_POINT ( 'NONE',  ( 3.235048515759559873, 1466.472015849239824, 219.6884157167970102 ) ) ;
#91735 = CARTESIAN_POINT ( 'NONE',  ( -13.54908436191989907, 1508.551704408389924, 216.1707514617089885 ) ) ;
#91736 = CARTESIAN_POINT ( 'NONE',  ( 3.933988272389480123, 1409.050438284940128, 194.6660132622929780 ) ) ;
#91737 = CARTESIAN_POINT ( 'NONE',  ( 0.2331197489560000169, 1408.921201108330024, 186.4825419995979985 ) ) ;
#91738 = DIRECTION ( 'NONE',  ( -0.000000000000000000, -1.000000000000000000, -0.000000000000000000 ) ) ;
#91739 = CARTESIAN_POINT ( 'NONE',  ( 3.097291077214380017, 1433.546567555699994, 201.1395984631290048 ) ) ;
#91740 = CARTESIAN_POINT ( 'NONE',  ( -3.119435209982429846, 1441.198230638479799, 165.1033167001029938 ) ) ;
#91741 = DIRECTION ( 'NONE',  ( -1.000000000000000000, 0.000000000000000000, 0.000000000000000000 ) ) ;
#91742 = EDGE_LOOP ( 'NONE', ( #4605, #71247, #37651 ) ) ;
#91743 = CARTESIAN_POINT ( 'NONE',  ( -15.90990259576500065, 1515.867682058960099, 224.3246417466669982 ) ) ;
#91744 = CARTESIAN_POINT ( 'NONE',  ( 19.22912473335630423, 1456.153986460939905, 226.8534579158520046 ) ) ;
#91745 = CARTESIAN_POINT ( 'NONE',  ( -12.78772699639999999, 1434.671431919079851, 149.7610961743979772 ) ) ;
#91746 = CARTESIAN_POINT ( 'NONE',  ( -8.321770097687579715E-10, 1467.826180283610029, 247.7074370028710177 ) ) ;
#91747 = CARTESIAN_POINT ( 'NONE',  ( -1.842962231260000028, 1515.551704408389924, 212.9514660752490158 ) ) ;
#91748 = EDGE_CURVE ( 'NONE', #72812, #64568, #26973, .T. ) ;
#91749 = DIRECTION ( 'NONE',  ( 1.000000000000000000, 0.000000000000000000, 0.000000000000000000 ) ) ;
#91750 = CARTESIAN_POINT ( 'NONE',  ( -4.390466737189999691, 1449.947854720489886, 190.5483265708990075 ) ) ;
#91751 = CARTESIAN_POINT ( 'NONE',  ( -1.466185886320000131, 1484.851694392830041, 182.4600082771979999 ) ) ;
#91752 = CARTESIAN_POINT ( 'NONE',  ( -9.895196081809372046, 1362.408266275323513, 207.6218459616987673 ) ) ;
#91753 = FACE_OUTER_BOUND ( 'NONE', #95800, .T. ) ;
#91754 = CARTESIAN_POINT ( 'NONE',  ( 13.60272764034519888, 1508.889111070959871, 233.6609499386090079 ) ) ;
#91755 = CARTESIAN_POINT ( 'NONE',  ( -7.845640617949999118, 1425.340740689890026, 205.7634566372090319 ) ) ;
#91756 = CARTESIAN_POINT ( 'NONE',  ( -7.339107240745000205, 1517.203017563489766, 207.9963360818169917 ) ) ;
#91757 = CARTESIAN_POINT ( 'NONE',  ( -21.03123196678649975, 1507.789098018889945, 192.1781278620359785 ) ) ;
#91758 = CARTESIAN_POINT ( 'NONE',  ( 29.74444329484277105, 1526.348417187222140, 201.0223654199409111 ) ) ;
#91759 = DIRECTION ( 'NONE',  ( -1.755985294532469921E-16, 1.000000000000000000, -1.338183447452831989E-16 ) ) ;
#91760 = CARTESIAN_POINT ( 'NONE',  ( 7.126030816970708948, 1424.920809236449941, 212.9863649234119976 ) ) ;
#91761 = ORIENTED_EDGE ( 'NONE', *, *, #31050, .T. ) ;
#91762 = CARTESIAN_POINT ( 'NONE',  ( -7.369671095600000695E-09, 1422.147183830129961, 212.8701394402079927 ) ) ;
#91763 = CARTESIAN_POINT ( 'NONE',  ( -28.13115138559999906, 1508.134099163530209, 208.1186796399779837 ) ) ;
#91765 = CARTESIAN_POINT ( 'NONE',  ( 7.878537825433329367, 1517.051704408389924, 200.0586249522280013 ) ) ;
#91764 = CARTESIAN_POINT ( 'NONE',  ( -3.527537870079999749, 1486.454657621929982, 181.8568875002980292 ) ) ;
#91766 = CARTESIAN_POINT ( 'NONE',  ( -2.850245122384609697, 1419.522424184869806, 186.1943312919690072 ) ) ;
#91767 = CARTESIAN_POINT ( 'NONE',  ( -26.35128651260000154, 1437.443204552669840, 225.2418051465980113 ) ) ;
#91768 = CARTESIAN_POINT ( 'NONE',  ( -29.51860354171773082, 1509.963695514703204, 206.5604812588238985 ) ) ;
#91769 = CARTESIAN_POINT ( 'NONE',  ( -21.13360565959400006, 1452.175058615539911, 141.7927856989660143 ) ) ;
#91770 = CARTESIAN_POINT ( 'NONE',  ( 29.26105829599999808, 1451.435244290330047, 136.0815397235980129 ) ) ;
#91771 = EDGE_LOOP ( 'NONE', ( #8812, #107990 ) ) ;
#91772 = CARTESIAN_POINT ( 'NONE',  ( -5.367153005107930142, 1426.308048638930131, 152.5548644906199911 ) ) ;
#91773 = DIRECTION ( 'NONE',  ( 0.9455185755993178454, 0.000000000000000000, -0.3255681544571539243 ) ) ;
#91774 = CARTESIAN_POINT ( 'NONE',  ( 16.73020750861299888, 1423.490444015980074, 228.1585555744700002 ) ) ;
#91775 = CARTESIAN_POINT ( 'NONE',  ( 10.44621597880000152, 1461.871091769490022, 210.5497379424390090 ) ) ;
#91776 = ORIENTED_EDGE ( 'NONE', *, *, #703, .F. ) ;
#91777 = EDGE_LOOP ( 'NONE', ( #75024, #56829, #74309, #93016 ) ) ;
#91778 = CARTESIAN_POINT ( 'NONE',  ( -73.11457663749999369, 1384.756954744069844, 272.3426209276589702 ) ) ;
#91779 = CARTESIAN_POINT ( 'NONE',  ( -23.49170351482609931, 1410.011808632399834, 209.6547519446870069 ) ) ;
#91780 = EDGE_CURVE ( 'NONE', #59183, #1876, #48631, .T. ) ;
#91781 = VERTEX_POINT ( 'NONE', #107708 ) ;
#91782 = CARTESIAN_POINT ( 'NONE',  ( 4.429773098726779601, 1508.551704408389924, 204.3196138220149862 ) ) ;
#91783 = CARTESIAN_POINT ( 'NONE',  ( -105.2826783650000095, 1379.306804825290101, 305.8448452370589621 ) ) ;
#91784 = EDGE_CURVE ( 'NONE', #37972, #48060, #50390, .T. ) ;
#91785 = CARTESIAN_POINT ( 'NONE',  ( -4.792740298340000038, 1507.637309065929912, 236.3818457613980115 ) ) ;
#91786 = CARTESIAN_POINT ( 'NONE',  ( -18.04342283379999756, 1410.879798814630021, 224.6982261388980078 ) ) ;
#91787 = ORIENTED_EDGE ( 'NONE', *, *, #15607, .F. ) ;
#91788 = CARTESIAN_POINT ( 'NONE',  ( 41.71199689262579824, 1455.342431078719983, 268.8818206049920150 ) ) ;
#91789 = B_SPLINE_CURVE_WITH_KNOTS ( 'NONE', 3,
 ( #29819, #44439, #78582, #45004, #73497, #74593, #30366, #108729, #13547, #91385, #47732, #98674, #48293, #82976, #49387, #55604, #107631, #56129, #82436 ),
 .UNSPECIFIED., .F., .F.,
 ( 4, 3, 3, 3, 3, 3, 4 ),
 ( -7.762943616236829492, -7.540944356910980417, -6.384229433512970786, -5.472533626251030014, -4.715605178811290266, -3.910860172016169756, -3.182123501529999565 ),
 .UNSPECIFIED. ) ;
#91790 = CARTESIAN_POINT ( 'NONE',  ( -4.679794214673830055, 1508.610718243669908, 205.2601826376400140 ) ) ;
#91791 = CARTESIAN_POINT ( 'NONE',  ( 0.006268853705600000749, 1420.201965319130068, 183.8994898050980282 ) ) ;
#91792 = CARTESIAN_POINT ( 'NONE',  ( -1.133517003235000153, 1516.713079096360161, 204.5117660986770147 ) ) ;
#91793 = ORIENTED_EDGE ( 'NONE', *, *, #85923, .F. ) ;
#91794 = CARTESIAN_POINT ( 'NONE',  ( 6.201377858498039686, 1483.628135010170126, 219.2029351982129981 ) ) ;
#91795 = CARTESIAN_POINT ( 'NONE',  ( 15.29490961578690111, 1512.594488815709838, 195.7754158856819799 ) ) ;
#91796 = CARTESIAN_POINT ( 'NONE',  ( 5.405194353942709640, 1478.857543658343957, 200.1157415609600321 ) ) ;
#91797 = ORIENTED_EDGE ( 'NONE', *, *, #12860, .F. ) ;
#91798 = CARTESIAN_POINT ( 'NONE',  ( -10.51062080119100095, 1480.296605995150003, 210.9546507189759836 ) ) ;
#91799 = CARTESIAN_POINT ( 'NONE',  ( 5.482251411591255064, 1434.591294175683743, 202.5885199238377368 ) ) ;
#91800 = CARTESIAN_POINT ( 'NONE',  ( -12.37943801505299923, 1512.150422497879845, 194.2281132779359893 ) ) ;
#91801 = CARTESIAN_POINT ( 'NONE',  ( 9.661401783296120982, 1503.269051499499938, 217.4307197796210005 ) ) ;
#91802 = B_SPLINE_CURVE_WITH_KNOTS ( 'NONE', 3,
 ( #69477, #61620, #52111, #94640, #45376, #35292, #2820, #36394, #62180, #19585, #87358, #10654, #87926, #96306, #79516, #103598, #71136, #34738, #17915, #9532, #86241, #43700, #26898, #86797, #61087, #10088, #44262, #78404, #44823, #95752, #78976, #21053, #51117, #76866, #720, #43269 ),
 .UNSPECIFIED., .F., .F.,
 ( 4, 2, 2, 1, 1, 1, 1, 1, 2, 2, 2, 2, 2, 2, 1, 1, 1, 2, 2, 2, 2, 4 ),
 ( 0.000000000000000000, 0.1250000000010887402, 0.1875000000016285029, 0.2187500000019007851, 0.2343750000020369817, 0.2421875000021050661, 0.2460937500021389279, 0.2480468750021558033, 0.2490234375021619373, 0.2500000000021680435, 0.3750000000025698887, 0.4375000000027749469, 0.4687500000028848590, 0.4843750000029383163, 0.4921875000029651281, 0.4960937500029829472, 0.4980468750029918845, 0.4990234375029963809, 0.5000000000030008218, 0.6250000000022466473, 0.7500000000014925838, 1.000000000000000000 ),
 .UNSPECIFIED. ) ;
#91803 = CARTESIAN_POINT ( 'NONE',  ( 7.374483138519999592, 1422.905762710230192, 195.5806561682990150 ) ) ;
#91804 = CARTESIAN_POINT ( 'NONE',  ( 22.63852601520000007, 1409.703615135929795, 209.5818420717589845 ) ) ;
#91805 = CARTESIAN_POINT ( 'NONE',  ( -10.88362670706469970, 1492.306448310009955, 203.4235623022770199 ) ) ;
#91806 = CARTESIAN_POINT ( 'NONE',  ( 10.60329135936409983, 1479.127526841280087, 205.9829681192889836 ) ) ;
#91807 = CARTESIAN_POINT ( 'NONE',  ( 2.005245171522929581, 1408.983085091729890, 186.9291916408829763 ) ) ;
#91809 = CARTESIAN_POINT ( 'NONE',  ( 10.20313649189779959, 1171.102791779800100, 156.7234425824970003 ) ) ;
#91808 = FACE_OUTER_BOUND ( 'NONE', #5908, .T. ) ;
#91810 = CARTESIAN_POINT ( 'NONE',  ( 10.66776494137399922, 1424.286284822849893, 206.6302607443430190 ) ) ;
#91811 = CARTESIAN_POINT ( 'NONE',  ( -10.69978296939999929, 1378.845154982549957, 215.3071352179290159 ) ) ;
#91812 = EDGE_CURVE ( 'NONE', #105548, #8134, #25323, .T. ) ;
#91813 = CARTESIAN_POINT ( 'NONE',  ( 11.84242369139999873, 1431.324257919750153, 147.6543138610979895 ) ) ;
#91814 = ORIENTED_EDGE ( 'NONE', *, *, #238, .T. ) ;
#91815 = CARTESIAN_POINT ( 'NONE',  ( 12.70951029399999932, 1416.237488680629895, 222.2791103869979850 ) ) ;
#91816 = CARTESIAN_POINT ( 'NONE',  ( -11.63668813159994286, 1425.864839735430678, 144.1681848196939768 ) ) ;
#91817 = CARTESIAN_POINT ( 'NONE',  ( -109.1309839890330124, 1384.924126711810004, 311.2646841801559958 ) ) ;
#91818 = B_SPLINE_CURVE_WITH_KNOTS ( 'NONE', 3,
 ( #6449, #40595, #22656, #101035, #32197, #66380, #76403, #99381, #57429, #24334, #50121, #16466, #48469, #42256, #8088, #92102, #15378, #58515, #65818, #49567, #101582, #83696 ),
 .UNSPECIFIED., .F., .F.,
 ( 4, 2, 2, 2, 2, 2, 2, 2, 2, 2, 4 ),
 ( 3.231953689032543100E-05, 0.0004825677620379821304, 0.0009328159871856388230, 0.001383064212333296600, 0.001608188324907083204, 0.001833312437480870243, 0.002058436550054657064, 0.002283560662628443452, 0.002733808887776098193, 0.003184057112923752934, 0.003634305338071407675 ),
 .UNSPECIFIED. ) ;
#91819 = EDGE_CURVE ( 'NONE', #39980, #45174, #85876, .T. ) ;
#91820 = CARTESIAN_POINT ( 'NONE',  ( -8.672397137009999923, 1387.672506191870070, 200.2132856537890007 ) ) ;
#91821 = CARTESIAN_POINT ( 'NONE',  ( 4.758677794462281341, 1427.076634120264089, 137.0999999980979567 ) ) ;
#91822 = CARTESIAN_POINT ( 'NONE',  ( 11.36942005508340081, 1422.263558134510049, 203.3812548922369956 ) ) ;
#91823 = ADVANCED_FACE ( 'NONE', ( #92005 ), #19721, .T. ) ;
#91824 = CARTESIAN_POINT ( 'NONE',  ( -11.01419074117260166, 1462.544645942729858, 208.2905843779830093 ) ) ;
#91825 = DIRECTION ( 'NONE',  ( 8.881784197000000007E-16, -1.000000000000000000, 1.836970198721029688E-16 ) ) ;
#91826 = CARTESIAN_POINT ( 'NONE',  ( -8.097663848092500061, 1477.149761026620126, 215.6266069428237699 ) ) ;
#91827 = CARTESIAN_POINT ( 'NONE',  ( 11.93819009070000092, 1433.480077612689911, 149.8972056143980183 ) ) ;
#91828 = CARTESIAN_POINT ( 'NONE',  ( 34.97756116859999764, 1449.243413927999882, 262.6648722511980054 ) ) ;
#91829 = CARTESIAN_POINT ( 'NONE',  ( 1.108081647679679982, 1450.800742795999895, 181.4825116590070024 ) ) ;
#91830 = CARTESIAN_POINT ( 'NONE',  ( -11.60004869885205636, 1428.977684734793911, 135.1000015630646089 ) ) ;
#91831 = CARTESIAN_POINT ( 'NONE',  ( -5.164876290100000489, 1519.913060387329779, 231.9023197776979828 ) ) ;
#91832 = CIRCLE ( 'NONE', #48948, 1.999999999999999556 ) ;
#91833 = CARTESIAN_POINT ( 'NONE',  ( 6.558237873239729510, 1465.446384999080010, 217.0856503752089850 ) ) ;
#91834 = EDGE_CURVE ( 'NONE', #67570, #94817, #62975, .T. ) ;
#91835 = CARTESIAN_POINT ( 'NONE',  ( 22.98253439269999987, 1410.218983183530099, 207.4712557340779995 ) ) ;
#91836 = B_SPLINE_CURVE_WITH_KNOTS ( 'NONE', 3,
 ( #26984, #61173, #94726, #85213, #102008, #18004, #95288, #25846, #34268, #84663, #52197, #69007, #690, #86326, #110427, #58934, #68450, #93066, #1238, #85771, #60048, #35375, #103111, #25292, #43781 ),
 .UNSPECIFIED., .F., .F.,
 ( 4, 3, 3, 3, 3, 3, 3, 3, 4 ),
 ( -7.276689993590000682, -7.237684796489060268, -6.557067735913999940, -5.837445478237999197, -5.133895891482029405, -5.098374790361580366, -4.440006559831749300, -3.663150781442820136, -2.991101461899999592 ),
 .UNSPECIFIED. ) ;
#91837 = DIRECTION ( 'NONE',  ( 0.9066646370135239552, -0.3866611060802799260, -0.1686784664203160033 ) ) ;
#91838 = CARTESIAN_POINT ( 'NONE',  ( -17.84188412740000018, 1410.460489672530230, 225.0030837357979863 ) ) ;
#91839 = CARTESIAN_POINT ( 'NONE',  ( 20.06299576540000018, 1508.017094725129937, 189.2032669109979963 ) ) ;
#91840 = EDGE_CURVE ( 'NONE', #52837, #98127, #44445, .T. ) ;
#91841 = CARTESIAN_POINT ( 'NONE',  ( -1.906561486464399589E-08, 1509.038615934239942, 204.6345961781970004 ) ) ;
#91842 = CARTESIAN_POINT ( 'NONE',  ( 2.566893074593609807E-08, 1406.911841303630126, 196.1218459607310081 ) ) ;
#91843 = CARTESIAN_POINT ( 'NONE',  ( -2.314969334973925541, 1525.402221411349728, 174.6257708845644174 ) ) ;
#91844 = DIRECTION ( 'NONE',  ( -0.2767035999362660315, -0.4514656066772200216, 0.8483006093183480534 ) ) ;
#91845 = B_SPLINE_CURVE_WITH_KNOTS ( 'NONE', 3,
 ( #15433, #16521, #69187, #93257, #883, #84308, #18195, #69752, #60227, #52392, #335, #85394, #85966, #78113, #101635, #59677, #33898, #26599, #35556, #15980, #76462, #33341, #84842, #92702, #50181, #1417, #68093, #102206, #7600, #67536, #110615, #102738, #59135, #86515, #94346, #9808, #25486, #93789, #41754, #103293, #75913, #17623, #26033, #17064, #24925, #68638, #50712, #51261, #103870, #110065, #77575, #8690, #8142, #60796, #35006, #42872 ),
 .UNSPECIFIED., .F., .F.,
 ( 4, 2, 2, 1, 2, 2, 2, 1, 1, 2, 2, 2, 2, 1, 1, 2, 2, 2, 2, 2, 1, 1, 2, 2, 2, 2, 1, 1, 1, 2, 2, 2, 4 ),
 ( 0.000000000000000000, 0.03125000000081699925, 0.04687500000111776560, 0.05468750000126820776, 0.05859375000134336986, 0.06250000000141853196, 0.09375000000176267334, 0.1093750000018305218, 0.1171875000017644497, 0.1210937500016381063, 0.1250000000015117629, 0.1875000000004202749, 0.2187499999998744615, 0.2343749999996015687, 0.2421874999994600985, 0.2460937499993843258, 0.2499999999993085253, 0.3749999999989888644, 0.4374999999987320143, 0.4687499999985955679, 0.4843749999984700016, 0.4921874999984772181, 0.4960937499985410559, 0.4999999999986049493, 0.6250000000006696865, 0.6875000000017634783, 0.7187500000022626345, 0.7343750000025426328, 0.7421875000026716407, 0.7460937500027362557, 0.7500000000028008706, 0.8750000000014004353, 1.000000000000000000 ),
 .UNSPECIFIED. ) ;
#91847 = EDGE_CURVE ( 'NONE', #6679, #27843, #8539, .T. ) ;
#91846 = CARTESIAN_POINT ( 'NONE',  ( -6.036595121079999515, 1415.425582719929707, 225.8522314191980058 ) ) ;
#91848 = CARTESIAN_POINT ( 'NONE',  ( 0.1723280242880049773, 1478.963607770360113, 182.1389088959510048 ) ) ;
#91850 = ORIENTED_EDGE ( 'NONE', *, *, #80218, .T. ) ;
#91849 = CARTESIAN_POINT ( 'NONE',  ( -2.803523226207980112, 1407.337701542270224, 222.1242196241450131 ) ) ;
#91851 = CARTESIAN_POINT ( 'NONE',  ( -16.90742463042001376, 1444.994950788469623, 162.4348201727408991 ) ) ;
#91852 = DIRECTION ( 'NONE',  ( 1.836970198721029688E-16, 1.000000000000000000, -7.703719777548939991E-34 ) ) ;
#91853 = CARTESIAN_POINT ( 'NONE',  ( 11.87950672170000033, 1433.311310111189869, 147.9453571599980251 ) ) ;
#91854 = CARTESIAN_POINT ( 'NONE',  ( -41.46889560185230295, 1441.954934107629924, 134.0999999980859911 ) ) ;
#91855 = CARTESIAN_POINT ( 'NONE',  ( -109.5357277100000033, 1384.884655545610030, 297.1232340666590517 ) ) ;
#91856 = ORIENTED_EDGE ( 'NONE', *, *, #30249, .F. ) ;
#91857 = B_SPLINE_SURFACE_WITH_KNOTS ( 'NONE', 5, 5, ( 
 ( #62568, #96688, #102844, #60327, #51926, #86068 ),
 ( #43528, #983, #35108, #26701, #71525, #55805 ),
 ( #37329, #4286, #3751, #89922, #13196, #81508 ),
 ( #72589, #88830, #64199, #98321, #28930, #46852 ),
 ( #46307, #56338, #30572, #22139, #38414, #37882 ),
 ( #12672, #80980, #21044, #97221, #47386, #29461 ),
 ( #105645, #4810, #21600, #38956, #73705, #63121 ),
 ( #64762, #73135, #5371, #47930, #12115, #80436 ),
 ( #106718, #39530, #72066, #90470, #13746, #30008 ) ),
 .UNSPECIFIED., .F., .F., .F.,
 ( 6, 3, 6 ),
 ( 6, 6 ),
 ( 62.33963421229999824, 67.09990280889999781, 77.98062232429998630 ),
 ( 0.000000000000000000, 1.000000000000000000 ),
 .UNSPECIFIED. ) ;
#91858 = EDGE_CURVE ( 'NONE', #96482, #65697, #67384, .T. ) ;
#91859 = CARTESIAN_POINT ( 'NONE',  ( 10.46072157490000087, 1479.162298522890069, 206.0231600751390033 ) ) ;
#91860 = CARTESIAN_POINT ( 'NONE',  ( -103.5791577002006392, 1379.885278930973300, 304.2740119158704601 ) ) ;
#91861 = CARTESIAN_POINT ( 'NONE',  ( -12.23489726360000063, 1490.237666927790087, 209.6382998835400144 ) ) ;
#91862 = B_SPLINE_CURVE_WITH_KNOTS ( 'NONE', 3,
 ( #54707, #18845, #63124, #70968, #21049, #53041 ),
 .UNSPECIFIED., .F., .F.,
 ( 4, 2, 4 ),
 ( -1.131363979615749172E-05, 0.001067788114096062963, 0.002146889867988283161 ),
 .UNSPECIFIED. ) ;
#91863 = ADVANCED_FACE ( 'NONE', ( #103143 ), #18782, .T. ) ;
#91864 = CARTESIAN_POINT ( 'NONE',  ( 3.083943351259999854, 1469.624425254990001, 189.3818552890990077 ) ) ;
#91865 = CARTESIAN_POINT ( 'NONE',  ( -46.15243904500000127, 1440.913037427970266, 268.2044236447979983 ) ) ;
#91866 = CARTESIAN_POINT ( 'NONE',  ( -16.81641964920000021, 1417.207246461349996, 207.8736676468290057 ) ) ;
#91867 = CARTESIAN_POINT ( 'NONE',  ( -12.27511545770000012, 1378.749906411379925, 210.4255720796790285 ) ) ;
#91868 = CARTESIAN_POINT ( 'NONE',  ( 2.500000000000000000, 1439.615672362369878, 182.7715267708979923 ) ) ;
#91869 = CARTESIAN_POINT ( 'NONE',  ( -65.40580218510729082, 1385.088756549790105, 255.9493206941889696 ) ) ;
#91870 = CARTESIAN_POINT ( 'NONE',  ( -11.66480462916690009, 1391.913060387289988, 209.7483395150459842 ) ) ;
#91871 = CARTESIAN_POINT ( 'NONE',  ( 10.05007022209490053, 1424.553937115210147, 207.8952550960959798 ) ) ;
#91872 = ORIENTED_EDGE ( 'NONE', *, *, #95259, .F. ) ;
#91873 = EDGE_CURVE ( 'NONE', #82777, #3107, #47128, .T. ) ;
#91874 = CARTESIAN_POINT ( 'NONE',  ( -29.31938507799999982, 1451.735856109730094, 135.7220070057980195 ) ) ;
#91875 = CARTESIAN_POINT ( 'NONE',  ( -15.82357197924079806, 1409.473877788359914, 225.4813571472639921 ) ) ;
#91877 = VERTEX_POINT ( 'NONE', #55538 ) ;
#91876 = FACE_OUTER_BOUND ( 'NONE', #23373, .T. ) ;
#91878 = CARTESIAN_POINT ( 'NONE',  ( 4.527727924400000603, 1473.939356039790027, 219.1579490833989894 ) ) ;
#91879 = CARTESIAN_POINT ( 'NONE',  ( 10.51038035267259829, 1471.685921060520059, 212.2896990852769932 ) ) ;
#91880 = CARTESIAN_POINT ( 'NONE',  ( 16.93236825731289841, 1416.913057013589878, 210.7966595891460031 ) ) ;
#91881 = DIRECTION ( 'NONE',  ( -0.9786619618251627406, 0.000000000000000000, 0.2054769195713317953 ) ) ;
#91882 = CARTESIAN_POINT ( 'NONE',  ( -0.07495072822490929376, 1420.236531064540031, 183.6031585757189930 ) ) ;
#91883 = CARTESIAN_POINT ( 'NONE',  ( 19.61574826060000021, 1409.598057419529823, 218.7671105721680078 ) ) ;
#91884 = CARTESIAN_POINT ( 'NONE',  ( -1.977028453051359991, 1417.217131934150075, 185.9238632041590051 ) ) ;
#91885 = CARTESIAN_POINT ( 'NONE',  ( -17.72483192860000045, 1424.402862424130035, 227.6947415401980095 ) ) ;
#91886 = CARTESIAN_POINT ( 'NONE',  ( -4.668584239039048178, 1511.396718925044297, 200.7090070923989629 ) ) ;
#91887 = CARTESIAN_POINT ( 'NONE',  ( 2.500000000000000000, 1425.929641634319978, 183.3886485707629959 ) ) ;
#91888 = CARTESIAN_POINT ( 'NONE',  ( -123.8569892972415545, 1368.558218059090223, 298.5091666679153946 ) ) ;
#91889 = CARTESIAN_POINT ( 'NONE',  ( 23.32695134950520099, 1509.740226291735098, 190.9604462070601016 ) ) ;
#91890 = CARTESIAN_POINT ( 'NONE',  ( -9.498196251736658269, 1449.159077731892467, 207.4992946632423241 ) ) ;
#91891 = CARTESIAN_POINT ( 'NONE',  ( -0.01328397755539850039, 1516.939580991450157, 205.8601936452070049 ) ) ;
#91892 = CARTESIAN_POINT ( 'NONE',  ( -5.376660071774439942, 1485.139014803799910, 183.5235869889660023 ) ) ;
#91893 = ORIENTED_EDGE ( 'NONE', *, *, #10293, .F. ) ;
#91894 = CARTESIAN_POINT ( 'NONE',  ( -109.1178393244110083, 1384.617941813639845, 311.2528399063589859 ) ) ;
#91895 = CARTESIAN_POINT ( 'NONE',  ( -4.227095715345259741, 1441.558630613729974, 165.7615266881739728 ) ) ;
#91897 = EDGE_LOOP ( 'NONE', ( #7022, #83837, #10548, #2981 ) ) ;
#91896 = CARTESIAN_POINT ( 'NONE',  ( -68.69558181574110733, 1379.747740281419965, 280.2958428208029886 ) ) ;
#91898 = CARTESIAN_POINT ( 'NONE',  ( -15.63365311440000127, 1422.686384262629872, 229.4762402829979919 ) ) ;
#91899 = ORIENTED_EDGE ( 'NONE', *, *, #3750, .F. ) ;
#91900 = CARTESIAN_POINT ( 'NONE',  ( -2.423738817658458888, 1456.568741658530826, 199.9484635142324578 ) ) ;
#91901 = CARTESIAN_POINT ( 'NONE',  ( 11.53251555600000167, 1501.193729600089910, 207.9797876773089911 ) ) ;
#91903 = CARTESIAN_POINT ( 'NONE',  ( 16.10936821303920041, 1409.855324947380041, 191.9958954789800032 ) ) ;
#91902 = CARTESIAN_POINT ( 'NONE',  ( -11.73848972823176062, 1426.695089812134484, 144.2749369092671827 ) ) ;
#91904 = CARTESIAN_POINT ( 'NONE',  ( 1.137296650804999976, 1516.908147884120126, 210.8236964273370120 ) ) ;
#91905 = EDGE_CURVE ( 'NONE', #92411, #71735, #1836, .T. ) ;
#91906 =( BOUNDED_CURVE ( )  B_SPLINE_CURVE ( 3, ( #57680, #47604, #48165, #72813 ),
 .UNSPECIFIED., .F., .F. ) 
 B_SPLINE_CURVE_WITH_KNOTS ( ( 4, 4 ),
 ( 4.170645138360129955, 5.254132885623210569 ),
 .UNSPECIFIED. ) 
 CURVE ( )  GEOMETRIC_REPRESENTATION_ITEM ( )  RATIONAL_B_SPLINE_CURVE ( ( 1.000000000000000000, 0.9045405262885497510, 0.9045405262885497510, 1.000000000000000000 ) ) 
 REPRESENTATION_ITEM ( '' )  );
#91907 = CARTESIAN_POINT ( 'NONE',  ( 41.10105618305409791, 1442.565812537450029, 136.7947891895450141 ) ) ;
#91908 = CARTESIAN_POINT ( 'NONE',  ( 33.91369278643569629, 1437.010534640189690, 136.5611839302279691 ) ) ;
#91909 = CARTESIAN_POINT ( 'NONE',  ( 11.26937486967429969, 1478.652699849539886, 205.8601904136019982 ) ) ;
#91910 = CARTESIAN_POINT ( 'NONE',  ( 12.61287423918429873, 1500.964026500809950, 210.7122643477439965 ) ) ;
#91911 = DIRECTION ( 'NONE',  ( 0.000000000000000000, 0.000000000000000000, 1.000000000000000000 ) ) ;
#91912 = CARTESIAN_POINT ( 'NONE',  ( 34.05830400097580224, 1451.723718204009856, 134.0999999980979851 ) ) ;
#91913 = PLANE ( 'NONE',  #38216 ) ;
#91914 = ORIENTED_EDGE ( 'NONE', *, *, #52786, .F. ) ;
#91915 = FACE_OUTER_BOUND ( 'NONE', #106407, .T. ) ;
#91916 = FACE_OUTER_BOUND ( 'NONE', #42365, .T. ) ;
#91917 = VERTEX_POINT ( 'NONE', #11869 ) ;
#91918 = ORIENTED_EDGE ( 'NONE', *, *, #102104, .F. ) ;
#91919 = CIRCLE ( 'NONE', #84793, 17.27637083661241135 ) ;
#91920 = CYLINDRICAL_SURFACE ( 'NONE', #3789, 1.455175085940000335 ) ;
#91921 = FACE_OUTER_BOUND ( 'NONE', #41551, .T. ) ;
#91922 = EDGE_CURVE ( 'NONE', #56404, #60533, #46469, .T. ) ;
#91923 = CARTESIAN_POINT ( 'NONE',  ( -0.07496883016649999454, 1450.915678356330091, 181.8856722418979928 ) ) ;
#91924 = CARTESIAN_POINT ( 'NONE',  ( -3.260695655560000183, 1485.137811735230116, 183.2004311182980132 ) ) ;
#91925 = DIRECTION ( 'NONE',  ( 0.000000000000000000, -1.000000000000000000, 0.000000000000000000 ) ) ;
#91926 = CARTESIAN_POINT ( 'NONE',  ( 3.028596170552124711, 1468.380354110695180, 218.6645797360170889 ) ) ;
#91927 = AXIS2_PLACEMENT_3D ( 'NONE', #84191, #93677, #109959 ) ;
#91928 = CARTESIAN_POINT ( 'NONE',  ( 11.91277487560000026, 1442.215011169370200, 187.5867736087979836 ) ) ;
#91929 = CARTESIAN_POINT ( 'NONE',  ( 40.71747595839759981, 1448.637563203230002, 135.3769927381360105 ) ) ;
#91930 = CARTESIAN_POINT ( 'NONE',  ( 4.363122683464830232, 1421.971318488559973, 183.8271341761570170 ) ) ;
#91931 = CARTESIAN_POINT ( 'NONE',  ( 26.87614569890000027, 1439.497608261269761, 137.1020444149980051 ) ) ;
#91932 = CARTESIAN_POINT ( 'NONE',  ( -11.15533026760000013, 1391.364751240080068, 214.3594460478390147 ) ) ;
#91933 = CARTESIAN_POINT ( 'NONE',  ( -79.74970074852699042, 1384.793032888219841, 282.7736550586030262 ) ) ;
#91934 = EDGE_LOOP ( 'NONE', ( #50054, #106289, #31440, #82843 ) ) ;
#91935 = CARTESIAN_POINT ( 'NONE',  ( -7.330554171554999776, 1516.857992118400034, 201.7925428541169879 ) ) ;
#91936 = CARTESIAN_POINT ( 'NONE',  ( -3.267039729984999585, 1517.012231669750008, 208.3862772893259887 ) ) ;
#91937 = ORIENTED_EDGE ( 'NONE', *, *, #61786, .T. ) ;
#91938 = CARTESIAN_POINT ( 'NONE',  ( 39.78035207931749540, 1440.913060387330006, 267.1197271637229278 ) ) ;
#91939 = EDGE_CURVE ( 'NONE', #2071, #101781, #7444, .T. ) ;
#91940 = CARTESIAN_POINT ( 'NONE',  ( -0.0002562030068480412176, 1452.575673631712561, 153.5027436610795917 ) ) ;
#91941 = ORIENTED_EDGE ( 'NONE', *, *, #107044, .T. ) ;
#91942 = CARTESIAN_POINT ( 'NONE',  ( -13.36846539809999967, 1415.041103189330215, 220.6286931108980127 ) ) ;
#91943 = CARTESIAN_POINT ( 'NONE',  ( 6.177825127070350142, 1429.592228316399996, 216.3189436702849946 ) ) ;
#91944 = CARTESIAN_POINT ( 'NONE',  ( -17.12577710671219933, 1420.218837620449904, 204.3128004817139924 ) ) ;
#91945 = CARTESIAN_POINT ( 'NONE',  ( -18.02257621027615642, 1526.382868172863937, 182.8951942368373977 ) ) ;
#91946 = CARTESIAN_POINT ( 'NONE',  ( 21.74459043622260168, 1409.809204975360217, 206.3233155530909926 ) ) ;
#91947 = ADVANCED_FACE ( 'NONE', ( #71259 ), #22863, .F. ) ;
#91948 = CARTESIAN_POINT ( 'NONE',  ( 10.81671648281710141, 1470.126838882340053, 207.0136797372550177 ) ) ;
#91949 = CARTESIAN_POINT ( 'NONE',  ( -31.81407709660786409, 1512.187213306747481, 196.2902540610632229 ) ) ;
#91950 = CARTESIAN_POINT ( 'NONE',  ( -5.963459923460841416, 1510.663752962396302, 201.6086580195713793 ) ) ;
#91951 = CARTESIAN_POINT ( 'NONE',  ( 25.71940137246620139, 1482.323570389569795, 206.2243813634200080 ) ) ;
#91953 = CARTESIAN_POINT ( 'NONE',  ( 2.487935150835943077, 1508.884207226184117, 213.6131390771874692 ) ) ;
#91952 = CARTESIAN_POINT ( 'NONE',  ( 14.85640376749999980, 1461.023002278929880, 230.2637214827979903 ) ) ;
#91954 = CARTESIAN_POINT ( 'NONE',  ( -4.363122647530000009, 1414.776585547029981, 163.8086717993979846 ) ) ;
#91955 = CARTESIAN_POINT ( 'NONE',  ( 2.291047489114999891, 1516.524310051880093, 216.8306159772470210 ) ) ;
#91956 = VERTEX_POINT ( 'NONE', #90764 ) ;
#91957 = CARTESIAN_POINT ( 'NONE',  ( -17.66551557795533611, 1517.051704408389924, 200.3426142980791269 ) ) ;
#91958 = CARTESIAN_POINT ( 'NONE',  ( -0.1147649368047699986, 1508.126957518789823, 180.5760551733519890 ) ) ;
#91959 = CARTESIAN_POINT ( 'NONE',  ( 2.106986098057376910, 1516.527651687830030, 216.8307034810665357 ) ) ;
#91960 = CARTESIAN_POINT ( 'NONE',  ( -4.998515195425000002, 1516.787536375099990, 213.1617432482970003 ) ) ;
#91961 = EDGE_CURVE ( 'NONE', #86293, #18369, #87054, .T. ) ;
#91962 = CARTESIAN_POINT ( 'NONE',  ( 18.49117119079999938, 1508.844092021829965, 188.2543554912979857 ) ) ;
#91963 = CARTESIAN_POINT ( 'NONE',  ( -10.92124405496922002, 1424.881793267335979, 138.2645581544207971 ) ) ;
#91965 = VERTEX_POINT ( 'NONE', #13485 ) ;
#91964 = CARTESIAN_POINT ( 'NONE',  ( 4.115862957632160146, 1509.032029411810072, 213.4860450609340319 ) ) ;
#91966 = CARTESIAN_POINT ( 'NONE',  ( -9.094256809820000953, 1384.874748782070128, 199.9429996847190125 ) ) ;
#91967 = CARTESIAN_POINT ( 'NONE',  ( 25.89198661300000026, 1442.605201390229922, 221.6500998664980102 ) ) ;
#91968 = EDGE_CURVE ( 'NONE', #49270, #65505, #34346, .T. ) ;
#91969 = CARTESIAN_POINT ( 'NONE',  ( -11.85363313409999897, 1431.417378487679798, 150.3276964087979763 ) ) ;
#91970 = CARTESIAN_POINT ( 'NONE',  ( 11.73709356400000026, 1426.695943141129874, 144.1748013759980154 ) ) ;
#91971 = CARTESIAN_POINT ( 'NONE',  ( -6.879245333380899829, 1439.807514724469911, 203.6160362513539894 ) ) ;
#91972 = CARTESIAN_POINT ( 'NONE',  ( 9.267034410570261116, 1423.582047773290014, 146.9531695596949987 ) ) ;
#91973 = CARTESIAN_POINT ( 'NONE',  ( 7.805005982189999969, 1501.592229086989846, 206.4628694365890169 ) ) ;
#91974 = CARTESIAN_POINT ( 'NONE',  ( 12.65231296470000188, 1445.580367743630177, 187.9555106065979828 ) ) ;
#91975 = EDGE_CURVE ( 'NONE', #80209, #67449, #24093, .T. ) ;
#91977 = CARTESIAN_POINT ( 'NONE',  ( -10.06498070994410021, 1481.481372748229887, 205.8729891504069940 ) ) ;
#91976 = CARTESIAN_POINT ( 'NONE',  ( -22.31028234190000248, 1482.724791558229981, 223.3675453720979931 ) ) ;
#91978 = CARTESIAN_POINT ( 'NONE',  ( -33.91369114349999592, 1451.728768196330066, 134.7155300131979914 ) ) ;
#91979 = ORIENTED_EDGE ( 'NONE', *, *, #68499, .F. ) ;
#91980 = CARTESIAN_POINT ( 'NONE',  ( 2.284199363404999961, 1516.940296199220029, 205.8526610237369994 ) ) ;
#91981 = CARTESIAN_POINT ( 'NONE',  ( 4.911197430519999685, 1406.966595134230147, 269.6424802271980070 ) ) ;
#91982 = CARTESIAN_POINT ( 'NONE',  ( 0.1980232598670000066, 1409.427787371929981, 185.2209094312979971 ) ) ;
#91983 = CARTESIAN_POINT ( 'NONE',  ( 0.1720217706479290065, 1499.798427092860038, 209.5061785884660139 ) ) ;
#91984 = ADVANCED_FACE ( 'NONE', ( #39820 ), #29586, .T. ) ;
#91985 = CARTESIAN_POINT ( 'NONE',  ( 21.45878957224126538, 1428.925085783155055, 219.0154504687402834 ) ) ;
#91986 = CARTESIAN_POINT ( 'NONE',  ( 2.837607610297419924, 1454.387933475150021, 218.0768438231829975 ) ) ;
#91987 = CARTESIAN_POINT ( 'NONE',  ( 7.499999980935001531, 1516.051704408390151, 209.1218459511669892 ) ) ;
#91988 = CARTESIAN_POINT ( 'NONE',  ( 8.038768963489999919, 1463.606875709430142, 235.5281748529980064 ) ) ;
#91989 = CARTESIAN_POINT ( 'NONE',  ( -9.447779140010000631, 1460.630169784690224, 214.7547266466890221 ) ) ;
#91990 = CARTESIAN_POINT ( 'NONE',  ( -12.71224440519999987, 1445.116720337619881, 186.6519215034980164 ) ) ;
#91991 = CARTESIAN_POINT ( 'NONE',  ( -19.82693296922757753, 1485.723221708761912, 190.4380495410725302 ) ) ;
#91992 = CARTESIAN_POINT ( 'NONE',  ( -13.43786151985979949, 1415.007830321470010, 220.3585435133520036 ) ) ;
#91993 = CARTESIAN_POINT ( 'NONE',  ( -4.261736558349999981, 1515.372048625790057, 210.9648096574089777 ) ) ;
#91994 = CARTESIAN_POINT ( 'NONE',  ( -5.411583886059999848, 1438.069580177289936, 208.0725929255889923 ) ) ;
#91995 = EDGE_CURVE ( 'NONE', #5297, #80757, #104509, .T. ) ;
#91996 = B_SPLINE_SURFACE_WITH_KNOTS ( 'NONE', 5, 5, ( 
 ( #64110, #61493, #44689, #99319, #95623, #53087, #73047, #90371, #78834 ),
 ( #2145, #13649, #62052, #104576, #96177, #19452, #11079, #45246, #80892 ),
 ( #98231, #103207, #3562, #95390, #62941, #9718, #80243, #69106, #86428 ),
 ( #11933, #11396, #103790, #86980, #95939, #43884, #97052, #69668, #27090 ),
 ( #10269, #52304, #104337, #1906, #71333, #96493, #88107, #19772, #20316 ),
 ( #26513, #35475, #54521, #46113, #18654, #70231, #94832, #88656, #60711 ) ),
 .UNSPECIFIED., .F., .F., .F.,
 ( 6, 6 ),
 ( 6, 3, 6 ),
 ( 1.103913001820000073, 5.464014710059999835 ),
 ( 0.000000000000000000, 1.000000000000000000, 2.000000000000000000 ),
 .UNSPECIFIED. ) ;
#91997 = AXIS2_PLACEMENT_3D ( 'NONE', #24993, #7119, #33399 ) ;
#91998 = CARTESIAN_POINT ( 'NONE',  ( 3.915802106908682578, 1515.051704408389924, 204.7920544193095509 ) ) ;
#91999 = CARTESIAN_POINT ( 'NONE',  ( -2.500000000000000000, 1432.302173844710069, 157.4936352153980010 ) ) ;
#92000 = CARTESIAN_POINT ( 'NONE',  ( -4.911878354730000673, 1474.859473121729934, 269.6424781226980372 ) ) ;
#92001 = CARTESIAN_POINT ( 'NONE',  ( 0.1681681984989999989, 1405.973120458229914, 146.1721969590979882 ) ) ;
#92002 = CARTESIAN_POINT ( 'NONE',  ( -13.41825681932545145, 1513.652787279354925, 192.3476914628060399 ) ) ;
#92004 = EDGE_CURVE ( 'NONE', #75732, #81986, #62902, .T. ) ;
#92003 = CIRCLE ( 'NONE', #22437, 1.999999999999999556 ) ;
#92005 = FACE_OUTER_BOUND ( 'NONE', #54840, .T. ) ;
#92006 = CARTESIAN_POINT ( 'NONE',  ( -55.97596842464690070, 1384.712463620669951, 273.6909236772529539 ) ) ;
#92007 = CARTESIAN_POINT ( 'NONE',  ( -9.771541787747370478, 1462.553260899800080, 206.2413424840439973 ) ) ;
#92008 = AXIS2_PLACEMENT_3D ( 'NONE', #69298, #87752, #1534 ) ;
#92009 = DIRECTION ( 'NONE',  ( -0.9455185755993178454, 0.000000000000000000, 0.3255681544571537578 ) ) ;
#92010 = B_SPLINE_SURFACE_WITH_KNOTS ( 'NONE', 5, 5, ( 
 ( #57911, #32690, #49511, #47841, #39438, #92583 ),
 ( #24274, #15854, #50059, #84187, #41647, #101521 ),
 ( #13651, #73613, #107742, #99321, #22595, #56798 ),
 ( #90935, #74163, #78003, #51710, #94237, #103760 ),
 ( #85281, #110500, #17512, #25367, #1309, #8580 ),
 ( #67977, #36012, #34344, #43856, #68522, #35449 ) ),
 .UNSPECIFIED., .F., .F., .F.,
 ( 6, 6 ),
 ( 6, 6 ),
 ( 63.41643075169999832, 77.02573483309998892 ),
 ( 0.000000000000000000, 2.000000000000000000 ),
 .UNSPECIFIED. ) ;
#92011 = CARTESIAN_POINT ( 'NONE',  ( -24.83894917540860092, 1457.427378167110191, 211.2740613720590090 ) ) ;
#92012 = CARTESIAN_POINT ( 'NONE',  ( 32.85805783624310550, 1523.678648413191922, 217.1983043299902647 ) ) ;
#92013 = CARTESIAN_POINT ( 'NONE',  ( -13.62133678120479985, 1452.879579795280051, 223.2680741433150047 ) ) ;
#92014 = CARTESIAN_POINT ( 'NONE',  ( -18.72568150940000109, 1410.063174156229934, 196.5773035203979759 ) ) ;
#92015 = FACE_OUTER_BOUND ( 'NONE', #18493, .T. ) ;
#92016 = B_SPLINE_CURVE_WITH_KNOTS ( 'NONE', 5,
 ( #105595, #29409, #71474, #70916, #54107, #96072 ),
 .UNSPECIFIED., .F., .F.,
 ( 6, 6 ),
 ( 0.000000000000000000, 1.000000000000000000 ),
 .UNSPECIFIED. ) ;
#92017 = CARTESIAN_POINT ( 'NONE',  ( -15.03721467795600120, 1422.461604470153816, 229.1222033841939947 ) ) ;
#92018 = CARTESIAN_POINT ( 'NONE',  ( -22.73294892570000059, 1411.115434492829991, 269.4808104911980422 ) ) ;
#92019 = VERTEX_POINT ( 'NONE', #35274 ) ;
#92020 = B_SPLINE_SURFACE_WITH_KNOTS ( 'NONE', 5, 1, ( 
 ( #16572, #102262 ),
 ( #33395, #940 ),
 ( #24988, #103354 ),
 ( #25542, #396 ),
 ( #69246, #50769 ),
 ( #9322, #67590 ) ),
 .UNSPECIFIED., .F., .F., .F.,
 ( 6, 6 ),
 ( 2, 2 ),
 ( 0.000000000000000000, 3.604516979870000082 ),
 ( 0.000000000000000000, 14.00000000000000000 ),
 .UNSPECIFIED. ) ;
#92021 = CARTESIAN_POINT ( 'NONE',  ( -7.736485947205265390, 1410.556087339033184, 230.7423858731618793 ) ) ;
#92022 = CARTESIAN_POINT ( 'NONE',  ( -19.86527982506180479, 1442.216701827569977, 212.8358345280389869 ) ) ;
#92023 = CARTESIAN_POINT ( 'NONE',  ( -13.59015224396020116, 1508.309004612710169, 209.6873486301020080 ) ) ;
#92024 = CARTESIAN_POINT ( 'NONE',  ( -18.32377786701850297, 1464.077817828640036, 217.4721512911559955 ) ) ;
#92026 = CARTESIAN_POINT ( 'NONE',  ( -2.487935060306839752, 1508.611350403544293, 204.4436907971870312 ) ) ;
#92025 = CARTESIAN_POINT ( 'NONE',  ( 11.64207462749999955, 1426.343247851129945, 137.4322893907980188 ) ) ;
#92027 = LINE ( 'NONE', #39418, #43267 ) ;
#92028 = CARTESIAN_POINT ( 'NONE',  ( -7.457021550593670334, 1517.051697240460271, 204.7417221852770126 ) ) ;
#92029 = CARTESIAN_POINT ( 'NONE',  ( -8.716383294119999903, 1450.962816624490188, 203.1307156043189934 ) ) ;
#92030 = CARTESIAN_POINT ( 'NONE',  ( -0.7538707734179979081, 1516.719999691880048, 202.1833671473370089 ) ) ;
#92031 = LINE ( 'NONE', #83081, #92904 ) ;
#92032 = CARTESIAN_POINT ( 'NONE',  ( -13.53550618839999942, 1416.067629290630066, 221.7501982114980308 ) ) ;
#92033 = CARTESIAN_POINT ( 'NONE',  ( 15.46083481443499963, 1513.125294087170005, 194.9058848310670271 ) ) ;
#92034 = CARTESIAN_POINT ( 'NONE',  ( -21.51775564986490252, 1417.978020122130147, 208.5749635269120006 ) ) ;
#92035 = CARTESIAN_POINT ( 'NONE',  ( -34.44898256530730407, 1379.727502236150031, 221.8237690217300155 ) ) ;
#92036 = CARTESIAN_POINT ( 'NONE',  ( 20.10171151328989936, 1507.852744525929893, 228.9948058528690069 ) ) ;
#92038 = ORIENTED_EDGE ( 'NONE', *, *, #8949, .T. ) ;
#92037 = CARTESIAN_POINT ( 'NONE',  ( -36.56818187949999555, 1379.727990716889963, 223.6839165909590008 ) ) ;
#92039 = EDGE_LOOP ( 'NONE', ( #11797, #102244, #33418, #20129, #24306 ) ) ;
#92040 = CARTESIAN_POINT ( 'NONE',  ( 11.97977764410059898, 1433.676209271590096, 150.1594973095589864 ) ) ;
#92041 = CARTESIAN_POINT ( 'NONE',  ( -7.156127822910000269, 1396.223004704730101, 218.8316158439280059 ) ) ;
#92042 = CARTESIAN_POINT ( 'NONE',  ( -18.89832309190000004, 1409.737660254029834, 221.9605378414980237 ) ) ;
#92043 = ORIENTED_EDGE ( 'NONE', *, *, #54284, .T. ) ;
#92044 = CARTESIAN_POINT ( 'NONE',  ( -13.49166848079650016, 1444.154048989462581, 169.3566495046044054 ) ) ;
#92045 = CARTESIAN_POINT ( 'NONE',  ( -0.1620860067307069718, 1416.842625005220043, 227.3681785903409889 ) ) ;
#92046 = CARTESIAN_POINT ( 'NONE',  ( -7.615555667685000252, 1511.534866634170157, 211.9602929371470168 ) ) ;
#92048 = CARTESIAN_POINT ( 'NONE',  ( 17.09785234980000013, 1424.306259183129896, 226.8830076123979893 ) ) ;
#92047 = CARTESIAN_POINT ( 'NONE',  ( 2.895368129540000002, 1444.422959043590026, 200.6322053094490059 ) ) ;
#92049 = VECTOR ( 'NONE', #104175, 999.9999999999998863 ) ;
#92050 = CARTESIAN_POINT ( 'NONE',  ( 14.94681733220000197, 1488.165501005629721, 187.6195381541980112 ) ) ;
#92051 = CARTESIAN_POINT ( 'NONE',  ( -11.45334864920000051, 1414.913060387329779, 196.1469376852979849 ) ) ;
#92052 = DIRECTION ( 'NONE',  ( 0.000000000000000000, 0.000000000000000000, -1.000000000000000000 ) ) ;
#92053 = CARTESIAN_POINT ( 'NONE',  ( 10.99229733427299927, 1396.296919868740133, 207.7930052487479884 ) ) ;
#92054 = CARTESIAN_POINT ( 'NONE',  ( -1.366628593397161140, 1414.941152333554328, 226.2919196448577566 ) ) ;
#92055 = CARTESIAN_POINT ( 'NONE',  ( 10.96256097240000038, 1431.846305526410106, 151.7537324878979916 ) ) ;
#92056 = CARTESIAN_POINT ( 'NONE',  ( 5.486049730215052378, 1509.110800823655609, 180.1874592187983524 ) ) ;
#92057 = ORIENTED_EDGE ( 'NONE', *, *, #29551, .F. ) ;
#92058 = CARTESIAN_POINT ( 'NONE',  ( 13.00447142352859942, 1434.790086459339818, 149.3565780673969812 ) ) ;
#92059 = VERTEX_POINT ( 'NONE', #17335 ) ;
#92060 = ORIENTED_EDGE ( 'NONE', *, *, #78018, .F. ) ;
#92061 = CARTESIAN_POINT ( 'NONE',  ( -18.24651515909999944, 1497.962091606229933, 229.4161187919980023 ) ) ;
#92062 = CARTESIAN_POINT ( 'NONE',  ( -11.01432655910000058, 1463.805739907729958, 231.7836158196980136 ) ) ;
#92063 = B_SPLINE_CURVE_WITH_KNOTS ( 'NONE', 5,
 ( #4424, #10613, #87319, #20632, #44782, #12250, #36353, #96831, #46439 ),
 .UNSPECIFIED., .F., .F.,
 ( 6, 3, 6 ),
 ( -167.5214206057449928, -163.5285714420000147, -95.54118695260000038 ),
 .UNSPECIFIED. ) ;
#92064 = CARTESIAN_POINT ( 'NONE',  ( -109.8609801027910322, 1385.943261636451552, 311.3663857728728885 ) ) ;
#92065 = CARTESIAN_POINT ( 'NONE',  ( -2.289624470354999719, 1517.154223579619838, 215.6854418399169901 ) ) ;
#92066 = CARTESIAN_POINT ( 'NONE',  ( -6.907011062519999633, 1472.523400736590020, 209.7330543039639963 ) ) ;
#92067 = EDGE_LOOP ( 'NONE', ( #25841, #24825, #869, #57293 ) ) ;
#92068 = CARTESIAN_POINT ( 'NONE',  ( -11.60945018750000024, 1501.942143215190072, 208.6602335187679671 ) ) ;
#92069 = DIRECTION ( 'NONE',  ( 0.000000000000000000, 1.000000000000000000, 0.000000000000000000 ) ) ;
#92070 = CARTESIAN_POINT ( 'NONE',  ( -11.47183536569999873, 1375.342188321910044, 208.5259290606699949 ) ) ;
#92071 = ORIENTED_EDGE ( 'NONE', *, *, #3648, .T. ) ;
#92072 = CARTESIAN_POINT ( 'NONE',  ( 4.997250153905000047, 1516.727068157269969, 205.8570671527170077 ) ) ;
#92073 = ORIENTED_EDGE ( 'NONE', *, *, #63186, .F. ) ;
#92074 = CARTESIAN_POINT ( 'NONE',  ( -6.949703372784999722, 1517.130100026000036, 208.3827239650380250 ) ) ;
#92075 = CARTESIAN_POINT ( 'NONE',  ( -8.826855412864000883, 1451.573000863549851, 206.2801294249610180 ) ) ;
#92076 = CARTESIAN_POINT ( 'NONE',  ( -16.41715922884294088, 1412.832312668764416, 269.3709241187901284 ) ) ;
#92077 = CARTESIAN_POINT ( 'NONE',  ( -0.9647690717699999308, 1408.946750865729882, 231.5874088180979982 ) ) ;
#92079 = ORIENTED_EDGE ( 'NONE', *, *, #30850, .F. ) ;
#92078 = CARTESIAN_POINT ( 'NONE',  ( -1.003994675859730012, 1414.971993471370070, 226.2520308800979763 ) ) ;
#92080 = CARTESIAN_POINT ( 'NONE',  ( -0.01299678013268519908, 1452.713242787300032, 183.2314067176189667 ) ) ;
#92081 = CARTESIAN_POINT ( 'NONE',  ( -27.33609021896520019, 1440.913060404380076, 228.3511589320279995 ) ) ;
#92082 = AXIS2_PLACEMENT_3D ( 'NONE', #106930, #30220, #66070 ) ;
#92083 = CARTESIAN_POINT ( 'NONE',  ( -36.16775626039999736, 1384.153367539769988, 235.4370147729590030 ) ) ;
#92084 = CARTESIAN_POINT ( 'NONE',  ( -0.5359182486523100808, 1465.001494122579970, 237.3401029919169787 ) ) ;
#92085 = CARTESIAN_POINT ( 'NONE',  ( 7.932946949084449528, 1410.936298116179842, 269.3426690103589749 ) ) ;
#92086 = CARTESIAN_POINT ( 'NONE',  ( -2.480187054844999572, 1517.025470194390209, 213.7472054950769973 ) ) ;
#92087 = CARTESIAN_POINT ( 'NONE',  ( 22.81351936760000143, 1409.709713646930140, 209.2743772224270060 ) ) ;
#92088 = CARTESIAN_POINT ( 'NONE',  ( -20.85386846230000302, 1509.307898977730019, 189.1594074083980104 ) ) ;
#92089 = CARTESIAN_POINT ( 'NONE',  ( 12.32478205772809865, 1492.212416795640138, 209.6735840658209895 ) ) ;
#92090 = CARTESIAN_POINT ( 'NONE',  ( 21.59395510246053007, 1525.159177407156676, 184.7447231557273142 ) ) ;
#92091 = CARTESIAN_POINT ( 'NONE',  ( -4.997718276504999224, 1516.693851263360102, 210.2547950466569944 ) ) ;
#92092 = CARTESIAN_POINT ( 'NONE',  ( -3.484501540619901583, 1447.229515926233262, 154.8508231829048327 ) ) ;
#92093 = CARTESIAN_POINT ( 'NONE',  ( -17.39681893400159041, 1503.136625852793486, 222.8800851632994693 ) ) ;
#92094 = CARTESIAN_POINT ( 'NONE',  ( -15.43014126019903642, 1486.078120340402620, 186.6022703082439023 ) ) ;
#92096 = ORIENTED_EDGE ( 'NONE', *, *, #66097, .F. ) ;
#92095 = CARTESIAN_POINT ( 'NONE',  ( -62.45667138380000694, 1385.073369564110180, 249.3006260568589880 ) ) ;
#92097 = CARTESIAN_POINT ( 'NONE',  ( -39.07382109423490135, 1385.187229302069909, 240.5099285539480150 ) ) ;
#92098 = EDGE_CURVE ( 'NONE', #23328, #63792, #33058, .T. ) ;
#92099 = B_SPLINE_SURFACE_WITH_KNOTS ( 'NONE', 5, 5, ( 
 ( #4285, #88829, #99410, #107276, #21599, #56889, #55804, #63120, #48498 ),
 ( #30571, #12671, #82065, #29460, #91020, #20492, #38413, #64761, #80435 ),
 ( #54702, #98872, #82638, #5370, #3749, #39529, #73704, #37881, #72065 ),
 ( #24511, #56497, #74413, #48658, #32922, #6078, #76045, #40230, #15007 ),
 ( #58701, #14465, #82784, #65461, #108538, #99019, #90626, #82233, #99568 ),
 ( #92833, #49753, #107980, #31828, #22853, #73853, #66015, #67112, #41343 ),
 ( #40783, #13906, #74960, #48093, #100137, #109109, #57617, #49205, #22295 ),
 ( #15553, #23423, #91733, #7188, #91185, #83333, #32388, #66571, #58153 ),
 ( #5532, #6629, #100676, #23958, #92283, #83883, #75512, #39685, #101214 ),
 ( #16109, #109646, #50313, #84442, #7726, #41887, #31277, #57058, #110189 ),
 ( #33462, #35690, #68772, #76591, #69321, #69880, #9390, #78809, #25616 ),
 ( #59808, #101770, #61474, #43553, #18869, #93927, #77702, #53066, #110742 ),
 ( #60924, #103428, #78245, #17194, #84974, #463, #8268, #27293, #1013 ),
 ( #87204, #60357, #25061, #44667, #67663, #35139, #51391, #52512, #85524 ),
 ( #16648, #8818, #77160, #42433, #59263, #93381, #43003, #95601, #26736 ),
 ( #34586, #86642, #102873, #10495, #50844, #26170, #94479, #34034, #68224 ),
 ( #17752, #2122, #95053, #18321, #9937, #44110, #102330, #1557, #103995 ),
 ( #51955, #86096, #104555, #11603, #96718, #81006, #54182, #13225, #88310 ) ),
 .UNSPECIFIED., .F., .F., .F.,
 ( 6, 3, 3, 3, 3, 6 ),
 ( 6, 3, 6 ),
 ( 26.14460235269999799, 29.70143520729999764, 36.87935098730000050, 40.57606074569999777, 43.18675127440000239, 48.00176651980000031 ),
 ( 0.000000000000000000, 1.000000000000000000, 2.000000000000000000 ),
 .UNSPECIFIED. ) ;
#92100 = CARTESIAN_POINT ( 'NONE',  ( 45.67186676709999915, 1443.699405974909951, 266.1886920326980430 ) ) ;
#92101 = EDGE_CURVE ( 'NONE', #18078, #75732, #95054, .T. ) ;
#92102 = CARTESIAN_POINT ( 'NONE',  ( -4.240793048770994389, 1370.422564428242140, 208.5825087046766555 ) ) ;
#92103 = CARTESIAN_POINT ( 'NONE',  ( -10.37900483499999993, 1419.722126144429922, 232.2032976616980022 ) ) ;
#92104 = DIRECTION ( 'NONE',  ( -1.755985294532469921E-16, 1.000000000000000000, -1.338183447452831989E-16 ) ) ;
#92105 = CARTESIAN_POINT ( 'NONE',  ( -23.86676970839999612, 1446.511384828899963, 213.7383374791680239 ) ) ;
#92106 = CARTESIAN_POINT ( 'NONE',  ( 12.49293096393500058, 1511.939906524110256, 224.5925846732669982 ) ) ;
#92108 = CARTESIAN_POINT ( 'NONE',  ( -7.769184196640000373, 1384.903524103370046, 218.9178905665889943 ) ) ;
#92107 = CARTESIAN_POINT ( 'NONE',  ( 17.60627508980000044, 1410.895669370830092, 224.8086596393980017 ) ) ;
#92109 = DIRECTION ( 'NONE',  ( 1.000000000000000000, 2.249639673992789970E-32, 1.224646799147350002E-16 ) ) ;
#92110 = CARTESIAN_POINT ( 'NONE',  ( 10.85845406881951192, 1424.793774302243946, 138.1921923613813590 ) ) ;
#92111 = EDGE_LOOP ( 'NONE', ( #56988, #58859, #47066, #85452 ) ) ;
#92112 = CARTESIAN_POINT ( 'NONE',  ( -5.005700239535000762, 1516.732530461250008, 202.1838802717869896 ) ) ;
#92113 = CARTESIAN_POINT ( 'NONE',  ( -16.11449822786499908, 1514.335759350750095, 224.1254885330670277 ) ) ;
#92114 = CARTESIAN_POINT ( 'NONE',  ( 7.512750208045280154, 1509.038615934079871, 214.6352815289239970 ) ) ;
#92115 = EDGE_CURVE ( 'NONE', #53391, #2813, #14549, .T. ) ;
#92116 = VECTOR ( 'NONE', #1729, 1000.000000000000227 ) ;
#92117 = CARTESIAN_POINT ( 'NONE',  ( 21.39322610469999830, 1453.000988217330132, 223.2795384177979940 ) ) ;
#92118 = CARTESIAN_POINT ( 'NONE',  ( 10.93592733551849960, 1461.398175533179938, 209.9040846029700162 ) ) ;
#92119 = DIRECTION ( 'NONE',  ( -0.1867471702549219348, 2.391457216852619248E-16, 0.9824080081115885710 ) ) ;
#92120 = CARTESIAN_POINT ( 'NONE',  ( 4.487574688360000508, 1465.989648107290122, 219.2141235446990208 ) ) ;
#92121 = DIRECTION ( 'NONE',  ( 0.000000000000000000, 1.000000000000000000, 0.000000000000000000 ) ) ;
#92122 = CARTESIAN_POINT ( 'NONE',  ( 27.32003778001789840, 1435.451595106259902, 135.2710127990389992 ) ) ;
#92123 = CARTESIAN_POINT ( 'NONE',  ( -38.64678288070560086, 1443.959461592480011, 137.1848748001749811 ) ) ;
#92124 = CARTESIAN_POINT ( 'NONE',  ( -21.78955385629999952, 1429.676808758129937, 218.6229220870480106 ) ) ;
#92125 = CARTESIAN_POINT ( 'NONE',  ( -23.69366750909999908, 1436.553436369609926, 140.6102976164979736 ) ) ;
#92126 = CARTESIAN_POINT ( 'NONE',  ( -104.6872550750000102, 1390.001717484610026, 301.9815041924589991 ) ) ;
#92127 = CARTESIAN_POINT ( 'NONE',  ( -16.23351320129999920, 1415.813397303330021, 226.8799459504980121 ) ) ;
#92128 = CARTESIAN_POINT ( 'NONE',  ( -106.7924537439999995, 1391.913060387289988, 301.4346793793589541 ) ) ;
#92129 = AXIS2_PLACEMENT_3D ( 'NONE', #32020, #57800, #74043 ) ;
#92130 = CARTESIAN_POINT ( 'NONE',  ( -33.53568936489296703, 1459.273957448159308, 269.5121044595919670 ) ) ;
#92131 = ORIENTED_EDGE ( 'NONE', *, *, #7641, .F. ) ;
#92132 = LINE ( 'NONE', #15407, #55184 ) ;
#92133 = CARTESIAN_POINT ( 'NONE',  ( 1.090037377353519974E-11, 1406.777728848529932, 269.6500679732980075 ) ) ;
#92134 = CARTESIAN_POINT ( 'NONE',  ( -3.487587101833019787, 1509.038630936360050, 213.6090953315220133 ) ) ;
#92135 = CARTESIAN_POINT ( 'NONE',  ( -13.91344329490000042, 1453.313060387329870, 223.0352892571980021 ) ) ;
#92136 = CARTESIAN_POINT ( 'NONE',  ( -15.40184547864896203, 1451.472071962601376, 222.6652460525484685 ) ) ;
#92137 = CARTESIAN_POINT ( 'NONE',  ( -29.28982059419999828, 1509.872724137230080, 209.1124962506749796 ) ) ;
#92138 = B_SPLINE_SURFACE_WITH_KNOTS ( 'NONE', 5, 5, ( 
 ( #103033, #86246, #76202, #33084, #42598, #7340 ),
 ( #41505, #26331, #77315, #59973, #94089, #33623 ),
 ( #8427, #76752, #67273, #101367, #94648, #16804 ),
 ( #62, #8988, #51007, #17920, #101931, #25218 ),
 ( #17360, #93534, #9537, #24116, #92988, #68377 ),
 ( #43705, #43159, #102485, #15706, #60526, #109265 ),
 ( #613, #85140, #92430, #34744, #32550, #66725 ),
 ( #59422, #84590, #100828, #7881, #75663, #58308 ),
 ( #49908, #84042, #24657, #58858, #16263, #50466 ) ),
 .UNSPECIFIED., .F., .F., .F.,
 ( 6, 3, 6 ),
 ( 6, 6 ),
 ( 8.507271964660001018, 19.64990296329999708, 30.22064862610000091 ),
 ( -8.673617379890000077E-19, 2.000000000000000000 ),
 .UNSPECIFIED. ) ;
#92139 = ADVANCED_FACE ( 'NONE', ( #17895 ), #80754, .T. ) ;
#92140 = CARTESIAN_POINT ( 'NONE',  ( -9.441857781927620152, 1438.488253401759948, 210.2256333341519792 ) ) ;
#92141 = CARTESIAN_POINT ( 'NONE',  ( -3.368596972435520254, 1515.551842520359969, 212.9003872916790101 ) ) ;
#92142 = CARTESIAN_POINT ( 'NONE',  ( -3.722981371187852773, 1415.895496273001299, 232.5493218368858663 ) ) ;
#92143 = CARTESIAN_POINT ( 'NONE',  ( -38.22966134359450763, 1444.824641043700012, 137.0630644298269942 ) ) ;
#92144 = CARTESIAN_POINT ( 'NONE',  ( 18.80585470380003699, 1425.655286308133100, 226.1606062853977903 ) ) ;
#92146 = EDGE_CURVE ( 'NONE', #103948, #53297, #67246, .T. ) ;
#92145 = CARTESIAN_POINT ( 'NONE',  ( -5.476857725019999457, 1435.904609370590151, 210.5194640658390028 ) ) ;
#92148 = EDGE_LOOP ( 'NONE', ( #4378, #19477, #110642, #31305 ) ) ;
#92147 = CARTESIAN_POINT ( 'NONE',  ( -14.24542985449999932, 1409.914296747629805, 226.6445893585980116 ) ) ;
#92149 = CARTESIAN_POINT ( 'NONE',  ( -0.08492873674538491124, 1416.830086716310007, 191.0182577611500108 ) ) ;
#92150 = CARTESIAN_POINT ( 'NONE',  ( 21.46972926610340338, 1509.114287161091397, 226.4513171853454878 ) ) ;
#92151 = ORIENTED_EDGE ( 'NONE', *, *, #65494, .F. ) ;
#92152 = ORIENTED_EDGE ( 'NONE', *, *, #18790, .F. ) ;
#92153 = CARTESIAN_POINT ( 'NONE',  ( 16.96258009527109678, 1415.088012641449950, 208.8510795922890111 ) ) ;
#92154 = CARTESIAN_POINT ( 'NONE',  ( 19.41157449629999832, 1457.417846740989944, 209.1218459616989946 ) ) ;
#92156 = CARTESIAN_POINT ( 'NONE',  ( 4.556270434109999981E-09, 1462.105318172430088, 225.2361590696979761 ) ) ;
#92155 = CARTESIAN_POINT ( 'NONE',  ( 2.702615377909999950, 1455.790727295790020, 218.5929249907289886 ) ) ;
#92157 = CARTESIAN_POINT ( 'NONE',  ( -2.874710529609999732, 1443.868727023889960, 218.3772876226990149 ) ) ;
#92158 = CARTESIAN_POINT ( 'NONE',  ( -11.86100656449999846, 1433.089193586070223, 150.2744710860979751 ) ) ;
#92159 = CARTESIAN_POINT ( 'NONE',  ( -7.567241880450000124, 1385.515695150829970, 219.0512258816089854 ) ) ;
#92160 = CARTESIAN_POINT ( 'NONE',  ( 9.604328208296740499, 1464.024737802830032, 211.1412599434549691 ) ) ;
#92161 = CARTESIAN_POINT ( 'NONE',  ( 6.808211076640000137, 1424.384911292389916, 213.4787420407489833 ) ) ;
#92162 = CARTESIAN_POINT ( 'NONE',  ( -24.74889967529999879, 1438.379598184860015, 210.4710876470479946 ) ) ;
#92163 = FACE_BOUND ( 'NONE', #51858, .T. ) ;
#92164 = CARTESIAN_POINT ( 'NONE',  ( 2.701075187949999901, 1449.975605856229777, 183.4649351312980059 ) ) ;
#92165 = B_SPLINE_CURVE_WITH_KNOTS ( 'NONE', 3,
 ( #30787, #72270, #12884, #108041, #91794, #23488, #15070, #89593, #81730, #5038, #82302, #63872, #56561, #4503, #97987, #82844, #21254, #38637, #106945, #90133, #55465, #30230, #73357, #56009, #22916, #64967, #39183, #64420, #90689, #49267, #100203, #38094, #65522, #106404, #5601, #39750, #98542, #21809, #6135, #73913, #31337, #99629, #13416 ),
 .UNSPECIFIED., .F., .F.,
 ( 4, 3, 3, 3, 3, 3, 3, 3, 3, 3, 3, 3, 3, 3, 4 ),
 ( 1.211046054640000118E-15, 1.449501323476880099, 2.863878615477850165, 4.272680454590320309, 5.675359640844769515, 7.071450696628339472, 8.457216201530728839, 9.836649899322781110, 11.20677902970780160, 11.59601058781499994, 12.87235518899669984, 14.20837703717869971, 15.54023549398300119, 16.81434485064450257, 17.59284132270000001 ),
 .UNSPECIFIED. ) ;
#92167 = CARTESIAN_POINT ( 'NONE',  ( 7.782994496996333389, 1364.555819372772248, 209.6218459617148824 ) ) ;
#92166 = B_SPLINE_CURVE_WITH_KNOTS ( 'NONE', 3,
 ( #89430, #35859, #86244, #27441 ),
 .UNSPECIFIED., .F., .F.,
 ( 4, 4 ),
 ( 0.9448711999806849171, 1.000000000000000000 ),
 .UNSPECIFIED. ) ;
#92168 = CARTESIAN_POINT ( 'NONE',  ( -27.67602665774289861, 1509.991482826411129, 197.5435719732463156 ) ) ;
#92170 = EDGE_LOOP ( 'NONE', ( #30632, #23878, #30768, #20426 ) ) ;
#92169 = FACE_OUTER_BOUND ( 'NONE', #6192, .T. ) ;
#92171 = VERTEX_POINT ( 'NONE', #77292 ) ;
#92172 = CARTESIAN_POINT ( 'NONE',  ( -11.84382825295330122, 1430.801220114690068, 149.7666669350089990 ) ) ;
#92173 = AXIS2_PLACEMENT_3D ( 'NONE', #45220, #46330, #4833 ) ;
#92174 = CARTESIAN_POINT ( 'NONE',  ( 13.94277550940000054, 1500.493050397790057, 227.7144758862989988 ) ) ;
#92175 = CARTESIAN_POINT ( 'NONE',  ( -5.012278527039999432, 1473.692053561029752, 270.2879168812979742 ) ) ;
#92176 = CARTESIAN_POINT ( 'NONE',  ( -1.556584322539999787, 1415.163755998629995, 226.9904013962980116 ) ) ;
#92177 = CARTESIAN_POINT ( 'NONE',  ( -130.5852908491499988, 1331.448250124730066, 304.2218459572590064 ) ) ;
#92178 = CARTESIAN_POINT ( 'NONE',  ( 40.43717099943859949, 1446.119067000189943, 136.7611679657780144 ) ) ;
#92179 = CARTESIAN_POINT ( 'NONE',  ( 16.66821264700000071, 1497.713060387329961, 193.8376437397980112 ) ) ;
#92180 = CARTESIAN_POINT ( 'NONE',  ( -7.965810903780000451, 1384.899971913130003, 199.4892300885790064 ) ) ;
#92181 = CARTESIAN_POINT ( 'NONE',  ( 18.28301776585879779, 1431.668727188719913, 208.6526615892310019 ) ) ;
#92182 = CARTESIAN_POINT ( 'NONE',  ( -18.04400385319999955, 1497.713060387329961, 196.8245703038979855 ) ) ;
#92183 = CARTESIAN_POINT ( 'NONE',  ( 9.671060821791741091, 1366.060403940048218, 210.6218459616991936 ) ) ;
#92184 = CARTESIAN_POINT ( 'NONE',  ( -39.66812107539500687, 1422.901596644940128, 268.6990807517719304 ) ) ;
#92185 = EDGE_LOOP ( 'NONE', ( #36287, #88336, #11435, #18906 ) ) ;
#92186 = DIRECTION ( 'NONE',  ( -1.755985294532469921E-16, 1.000000000000000000, -1.338183447452831989E-16 ) ) ;
#92187 = ORIENTED_EDGE ( 'NONE', *, *, #29727, .F. ) ;
#92188 = ORIENTED_EDGE ( 'NONE', *, *, #82507, .T. ) ;
#92189 = CARTESIAN_POINT ( 'NONE',  ( 4.043366220174999803, 1516.951766529250108, 211.9887038632370206 ) ) ;
#92190 = CARTESIAN_POINT ( 'NONE',  ( 4.363119589138680254, 1423.854801764450031, 183.5697712894070150 ) ) ;
#92191 = CARTESIAN_POINT ( 'NONE',  ( 7.107370174153629705, 1424.720561740850144, 194.0450910679149956 ) ) ;
#92193 = CARTESIAN_POINT ( 'NONE',  ( -2.500000000000000000, 1439.615672362369878, 170.5246407198980023 ) ) ;
#92192 = CARTESIAN_POINT ( 'NONE',  ( -2.284199401535000007, 1516.940296199220029, 212.3910308785969789 ) ) ;
#92194 = CARTESIAN_POINT ( 'NONE',  ( -4.582611926280000247, 1470.461621793529957, 184.1408639795980093 ) ) ;
#92195 = CARTESIAN_POINT ( 'NONE',  ( 1.925297170580940076, 1519.551704408389924, 230.6853930747409720 ) ) ;
#92196 = ORIENTED_EDGE ( 'NONE', *, *, #39862, .T. ) ;
#92197 = CARTESIAN_POINT ( 'NONE',  ( -26.54855949080000244, 1435.424486255840065, 135.3738653627980000 ) ) ;
#92198 = CIRCLE ( 'NONE', #43928, 1.999999999999998668 ) ;
#92199 = CARTESIAN_POINT ( 'NONE',  ( 2.871580388595000422, 1517.129577905929864, 202.1716309988170224 ) ) ;
#92200 = CARTESIAN_POINT ( 'NONE',  ( 1.546896728100281004, 1416.831922880601041, 190.2226035042538683 ) ) ;
#92202 = VECTOR ( 'NONE', #51864, 1000.000000000000227 ) ;
#92201 = CARTESIAN_POINT ( 'NONE',  ( -29.53767091413150325, 1384.555073608529938, 205.3427205205709924 ) ) ;
#92203 = CARTESIAN_POINT ( 'NONE',  ( -33.93501299241329860, 1421.187233221759925, 270.1375433979869740 ) ) ;
#92204 = CARTESIAN_POINT ( 'NONE',  ( -17.84338787571960694, 1523.382868172864164, 180.3600277896300383 ) ) ;
#92206 = ORIENTED_EDGE ( 'NONE', *, *, #84884, .F. ) ;
#92205 = CARTESIAN_POINT ( 'NONE',  ( -15.74154698502330163, 1459.394320999469983, 230.7248352790539911 ) ) ;
#92207 = EDGE_LOOP ( 'NONE', ( #62613, #68739, #103301, #76114 ) ) ;
#92208 = CARTESIAN_POINT ( 'NONE',  ( -31.23437356469455040, 1512.187213306747481, 195.3468678195118287 ) ) ;
#92209 = DIRECTION ( 'NONE',  ( -0.000000000000000000, -1.000000000000000000, -0.000000000000000000 ) ) ;
#92210 = CARTESIAN_POINT ( 'NONE',  ( 3.365542939320150140, 1426.305845304849754, 191.3806609882720124 ) ) ;
#92211 = CARTESIAN_POINT ( 'NONE',  ( -24.86449449159999858, 1436.143114817140031, 137.8606781676980120 ) ) ;
#92212 = CARTESIAN_POINT ( 'NONE',  ( -24.44980076159999882, 1442.538154569769858, 211.0821171723179930 ) ) ;
#92213 = CARTESIAN_POINT ( 'NONE',  ( 0.01319650876840149957, 1516.941178807709775, 211.4140629809269853 ) ) ;
#92214 = CARTESIAN_POINT ( 'NONE',  ( 6.459044766406664806, 1460.224289355106748, 201.9543198508955584 ) ) ;
#92215 = CARTESIAN_POINT ( 'NONE',  ( -2.684419367044589944, 1484.261477463810024, 183.2784813993209809 ) ) ;
#92216 = CARTESIAN_POINT ( 'NONE',  ( 5.859507211404899607, 1440.154374017829923, 216.2888686505930025 ) ) ;
#92217 = CARTESIAN_POINT ( 'NONE',  ( 3.829620113550000315, 1515.551704408389924, 211.2083941403789993 ) ) ;
#92218 =( BOUNDED_SURFACE ( )  B_SPLINE_SURFACE ( 5, 2, ( 
 ( #97008, #88064, #63969, #29782, #20271, #71844, #105962 ),
 ( #63429, #12969, #79663, #20819, #2967, #54472, #71288 ),
 ( #105401, #55016, #98084, #11349, #72365, #88610, #46064 ),
 ( #21355, #80197, #89143, #12429, #44964, #80749, #106496 ),
 ( #55562, #107042, #64518, #4058, #81277, #89687, #53359 ),
 ( #87504, #65612, #90226, #15161, #5130, #24111, #91888 ),
 ( #33078, #84038, #13511, #47699, #99724, #48815, #30877 ),
 ( #23017, #99170, #65057, #22452, #14069, #57221, #91347 ),
 ( #81827, #31430, #58303, #73461, #7336, #49903, #39286 ),
 ( #14628, #107592, #66718, #41500, #5697, #56653, #90786 ),
 ( #32545, #74560, #75659, #6772, #92425, #108137, #109800 ),
 ( #67269, #100824, #40936, #48258, #75114, #82401, #40383 ),
 ( #15700, #39842, #21901, #82937, #83479, #74005, #6228 ),
 ( #109261, #49352, #108693, #56098, #31985, #66175, #100295 ),
 ( #23576, #57769, #78405, #60518, #25213, #35856, #51003 ),
 ( #34739, #69478, #102481, #68929, #1717, #51549, #85134 ) ),
 .UNSPECIFIED., .F., .F., .F. ) 
 B_SPLINE_SURFACE_WITH_KNOTS ( ( 6, 3, 3, 1, 3, 6 ),
 ( 3, 2, 2, 3 ),
 ( 0.4214913904879999951, 6.500000000000000000, 18.08975840989999995, 46.86861349480000172, 60.45619974110000072, 75.86994138869999915 ),
 ( 5.770213214419189995, 6.283185307179590673, 7.853981633974480125, 8.911805878012440729 ),
 .UNSPECIFIED. ) 
 GEOMETRIC_REPRESENTATION_ITEM ( )  RATIONAL_B_SPLINE_SURFACE ( (
 ( 0.8711730249283579086, 0.9043503954986760185, 1.000000000000000000, 0.7071067811865480168, 1.000000000000000000, 0.8027563838226109416, 0.8711730262223410515),
 ( 0.8711730249283579086, 0.9043503954986760185, 1.000000000000000000, 0.7071067811865480168, 1.000000000000000000, 0.8027563838226109416, 0.8711730262223410515),
 ( 0.8711730249283579086, 0.9043503954986760185, 1.000000000000000000, 0.7071067811865480168, 1.000000000000000000, 0.8027563838226109416, 0.8711730262223410515),
 ( 0.8711730249283579086, 0.9043503954986760185, 1.000000000000000000, 0.7071067811865480168, 1.000000000000000000, 0.8027563838226109416, 0.8711730262223410515),
 ( 0.8711730249283579086, 0.9043503954986760185, 1.000000000000000000, 0.7071067811865480168, 1.000000000000000000, 0.8027563838226109416, 0.8711730262223410515),
 ( 0.8711730249283579086, 0.9043503954986760185, 1.000000000000000000, 0.7071067811865480168, 1.000000000000000000, 0.8027563838226109416, 0.8711730262223410515),
 ( 0.8711730249283579086, 0.9043503954986760185, 1.000000000000000000, 0.7071067811865480168, 1.000000000000000000, 0.8027563838226109416, 0.8711730262223410515),
 ( 0.8711730249283579086, 0.9043503954986760185, 1.000000000000000000, 0.7071067811865480168, 1.000000000000000000, 0.8027563838226109416, 0.8711730262223410515),
 ( 0.8711730249283579086, 0.9043503954986760185, 1.000000000000000000, 0.7071067811865480168, 1.000000000000000000, 0.8027563838226109416, 0.8711730262223410515),
 ( 0.8711730249283579086, 0.9043503954986760185, 1.000000000000000000, 0.7071067811865480168, 1.000000000000000000, 0.8027563838226109416, 0.8711730262223410515),
 ( 0.8711730249283579086, 0.9043503954986760185, 1.000000000000000000, 0.7071067811865480168, 1.000000000000000000, 0.8027563838226109416, 0.8711730262223410515),
 ( 0.8711730249283579086, 0.9043503954986760185, 1.000000000000000000, 0.7071067811865480168, 1.000000000000000000, 0.8027563838226109416, 0.8711730262223410515),
 ( 0.8711730249283579086, 0.9043503954986760185, 1.000000000000000000, 0.7071067811865480168, 1.000000000000000000, 0.8027563838226109416, 0.8711730262223410515),
 ( 0.8711730249283579086, 0.9043503954986760185, 1.000000000000000000, 0.7071067811865480168, 1.000000000000000000, 0.8027563838226109416, 0.8711730262223410515),
 ( 0.8711730249283579086, 0.9043503954986760185, 1.000000000000000000, 0.7071067811865480168, 1.000000000000000000, 0.8027563838226109416, 0.8711730262223410515),
 ( 0.8711730249283579086, 0.9043503954986760185, 1.000000000000000000, 0.7071067811865480168, 1.000000000000000000, 0.8027563838226109416, 0.8711730262223410515) ) ) 
 REPRESENTATION_ITEM ( '' )  SURFACE ( )  );
#92219 = CARTESIAN_POINT ( 'NONE',  ( 0.7352271172030020452, 1516.963431999339946, 207.4067364850470199 ) ) ;
#92220 = ORIENTED_EDGE ( 'NONE', *, *, #102340, .F. ) ;
#92221 = CARTESIAN_POINT ( 'NONE',  ( -7.966081143649218710, 1384.918389534460175, 199.4892681243580057 ) ) ;
#92222 = CARTESIAN_POINT ( 'NONE',  ( -10.46967383089999970, 1471.722673347089767, 207.5079226880490069 ) ) ;
#92223 = CARTESIAN_POINT ( 'NONE',  ( -5.959028607229999608, 1385.182909178320187, 218.5168903876589752 ) ) ;
#92224 = VERTEX_POINT ( 'NONE', #101341 ) ;
#92225 = CARTESIAN_POINT ( 'NONE',  ( 7.287315400159999790, 1481.177127506090073, 208.3645142728410065 ) ) ;
#92226 = CARTESIAN_POINT ( 'NONE',  ( -23.32592407598632533, 1509.740261108241157, 227.2847643979908980 ) ) ;
#92227 = CARTESIAN_POINT ( 'NONE',  ( 15.76891116102829926, 1459.304365935679925, 229.4386636210950030 ) ) ;
#92228 = CARTESIAN_POINT ( 'NONE',  ( -17.68146714750000115, 1417.155949729040003, 208.4269447418569996 ) ) ;
#92229 = CARTESIAN_POINT ( 'NONE',  ( 12.00387303569999986, 1415.296882282229944, 222.4718873070980294 ) ) ;
#92230 = CARTESIAN_POINT ( 'NONE',  ( 4.765390666840000122, 1487.224757102889726, 198.9594462837989965 ) ) ;
#92231 = CARTESIAN_POINT ( 'NONE',  ( 0.2751658889820000065, 1506.798305107329952, 186.8348836488979998 ) ) ;
#92232 = CARTESIAN_POINT ( 'NONE',  ( 23.29879903081510761, 1449.672675653727538, 217.3473003333802751 ) ) ;
#92234 = CARTESIAN_POINT ( 'NONE',  ( -11.98951922200000020, 1442.759074889710064, 150.6922381223979812 ) ) ;
#92233 = CARTESIAN_POINT ( 'NONE',  ( 5.007588646914999941, 1516.804776704140068, 214.8970827629769644 ) ) ;
#92235 = CARTESIAN_POINT ( 'NONE',  ( 33.91369968912619726, 1451.728767897860052, 134.7155302171979940 ) ) ;
#92236 = CARTESIAN_POINT ( 'NONE',  ( -4.034280953785000179, 1517.049325831759916, 216.0701676760970145 ) ) ;
#92237 = ORIENTED_EDGE ( 'NONE', *, *, #58517, .F. ) ;
#92238 = CARTESIAN_POINT ( 'NONE',  ( -12.61640448640000045, 1416.837080243330092, 194.9197993102980035 ) ) ;
#92239 = CARTESIAN_POINT ( 'NONE',  ( 16.14455737950000724, 1409.476838739224604, 193.1641866934976406 ) ) ;
#92240 = CARTESIAN_POINT ( 'NONE',  ( 2.226504434969999835, 1420.543949298730013, 184.8375689860979776 ) ) ;
#92241 = VECTOR ( 'NONE', #3146, 1000.000000000000000 ) ;
#92242 = EDGE_CURVE ( 'NONE', #39868, #2574, #87959, .T. ) ;
#92243 = AXIS2_PLACEMENT_3D ( 'NONE', #64667, #98785, #22047 ) ;
#92244 = CARTESIAN_POINT ( 'NONE',  ( 0.3242204524379989627, 1473.869303647089964, 219.3860063639990017 ) ) ;
#92245 = CARTESIAN_POINT ( 'NONE',  ( 2.458491834123362807, 1524.872178180562969, 175.9022251074391932 ) ) ;
#92246 = CARTESIAN_POINT ( 'NONE',  ( -7.545064063707340729, 1384.907232462019920, 219.0876311385090105 ) ) ;
#92247 = CARTESIAN_POINT ( 'NONE',  ( -11.19405031572889975, 1471.333863838639900, 206.8852767382200284 ) ) ;
#92248 = CARTESIAN_POINT ( 'NONE',  ( -6.390565317395836331, 1508.334948605542195, 219.9846009609073860 ) ) ;
#92249 = CARTESIAN_POINT ( 'NONE',  ( 17.36345563492336197, 1422.678662251234528, 226.5855745038400073 ) ) ;
#92250 = CARTESIAN_POINT ( 'NONE',  ( 1.665775206630939920, 1456.320421830250098, 198.6701496495810204 ) ) ;
#92251 = EDGE_CURVE ( 'NONE', #25680, #5162, #75412, .T. ) ;
#92252 = FACE_OUTER_BOUND ( 'NONE', #46582, .T. ) ;
#92253 = CARTESIAN_POINT ( 'NONE',  ( 38.29114240145940329, 1440.913060381290052, 256.7438938512759705 ) ) ;
#92255 = CARTESIAN_POINT ( 'NONE',  ( 4.327620191588789744, 1515.134623705510194, 208.4650689536229891 ) ) ;
#92254 = CARTESIAN_POINT ( 'NONE',  ( -10.52544773458219929, 1471.060235731149987, 210.0669986522439956 ) ) ;
#92256 = CARTESIAN_POINT ( 'NONE',  ( -5.100957845159999948, 1482.122785942490054, 228.9672709512990139 ) ) ;
#92257 = ORIENTED_EDGE ( 'NONE', *, *, #80132, .T. ) ;
#92258 = EDGE_LOOP ( 'NONE', ( #21027, #41509, #21367, #88194 ) ) ;
#92259 = CARTESIAN_POINT ( 'NONE',  ( -14.30333153811707447, 1506.380977071295547, 225.8074781016927943 ) ) ;
#92260 = CARTESIAN_POINT ( 'NONE',  ( -13.59512407998240135, 1507.703338069740084, 209.3532897553030239 ) ) ;
#92261 = CARTESIAN_POINT ( 'NONE',  ( 11.50463699793380101, 1502.210269078540250, 211.3057782935299826 ) ) ;
#92262 = CARTESIAN_POINT ( 'NONE',  ( 1970.639179128770138, -8387.357407334289746, 416.8689628978009978 ) ) ;
#92263 = CARTESIAN_POINT ( 'NONE',  ( 17.56614062935820542, 1509.646347970504848, 233.5045441439745559 ) ) ;
#92265 = AXIS2_PLACEMENT_3D ( 'NONE', #73536, #47222, #81348 ) ;
#92264 = CARTESIAN_POINT ( 'NONE',  ( -30.61443310214863445, 1523.462669333488066, 221.8243310972612221 ) ) ;
#92266 = CARTESIAN_POINT ( 'NONE',  ( -3.829620113550000315, 1515.551704408389924, 207.2788837304390199 ) ) ;
#92267 = CARTESIAN_POINT ( 'NONE',  ( -46.21053394692320637, 1383.818180755360117, 253.5808621639829994 ) ) ;
#92268 = VECTOR ( 'NONE', #63418, 1000.000000000000000 ) ;
#92269 = CARTESIAN_POINT ( 'NONE',  ( -15.59042067090000039, 1507.631725798030175, 192.4853000667980041 ) ) ;
#92270 = CARTESIAN_POINT ( 'NONE',  ( 32.86802468386292730, 1512.187213306747481, 217.2040256693915410 ) ) ;
#92271 = CARTESIAN_POINT ( 'NONE',  ( 10.84203907937230049, 1491.933390519110162, 211.8638197534569940 ) ) ;
#92273 = ORIENTED_EDGE ( 'NONE', *, *, #60388, .T. ) ;
#92272 = CARTESIAN_POINT ( 'NONE',  ( 0.2489532241669990265, 1455.106714014390036, 218.5657548107290040 ) ) ;
#92274 = CARTESIAN_POINT ( 'NONE',  ( 33.28034951413929576, 1522.382868172863937, 217.4407153818819722 ) ) ;
#92275 = CARTESIAN_POINT ( 'NONE',  ( -62.44985522310000192, 1384.688102815929824, 249.3037632142590212 ) ) ;
#92276 = CARTESIAN_POINT ( 'NONE',  ( 8.360512069408569502, 1436.611072127150010, 207.0360533130520082 ) ) ;
#92277 = ORIENTED_EDGE ( 'NONE', *, *, #58984, .F. ) ;
#92278 = VERTEX_POINT ( 'NONE', #77833 ) ;
#92279 = CARTESIAN_POINT ( 'NONE',  ( -21.50574124000000253, 1505.376505907290039, 210.1536426368190007 ) ) ;
#92280 = CARTESIAN_POINT ( 'NONE',  ( 34.26962912923569604, 1437.033889869800078, 136.5514234110600000 ) ) ;
#92281 = DIRECTION ( 'NONE',  ( -5.980589973904019347E-17, 1.000000000000000000, -1.736889445713099699E-16 ) ) ;
#92282 = CARTESIAN_POINT ( 'NONE',  ( -5.890030312369999521, 1462.819977020890065, 201.3180516141489704 ) ) ;
#92283 = CARTESIAN_POINT ( 'NONE',  ( -107.1973146609999930, 1381.194866720909886, 298.8585007089590135 ) ) ;
#92284 = DIRECTION ( 'NONE',  ( 0.000000000000000000, -1.000000000000000000, 0.000000000000000000 ) ) ;
#92285 = CARTESIAN_POINT ( 'NONE',  ( 1.338895077072802531, 1526.382868172864164, 178.6697305272271024 ) ) ;
#92286 = DIRECTION ( 'NONE',  ( 0.000000000000000000, 0.000000000000000000, -1.000000000000000000 ) ) ;
#92287 = CARTESIAN_POINT ( 'NONE',  ( 4.781276783620000081, 1452.020048942890071, 190.5513815401990030 ) ) ;
#92288 = CARTESIAN_POINT ( 'NONE',  ( 0.8274403209489998856, 1409.880679658830104, 185.1639250197980004 ) ) ;
#92289 = CARTESIAN_POINT ( 'NONE',  ( -113.4000000000000057, 1391.913060387289988, 306.7218459572590064 ) ) ;
#92290 = CARTESIAN_POINT ( 'NONE',  ( 3.771470575086420141, 1431.990137918330220, 200.6994607577710212 ) ) ;
#92291 = CARTESIAN_POINT ( 'NONE',  ( -3.116026071596179836, 1441.256293133330018, 168.7233834905880201 ) ) ;
#92292 = CARTESIAN_POINT ( 'NONE',  ( 32.86470158750944393, 1523.580203803270933, 217.2021180890986614 ) ) ;
#92293 = EDGE_LOOP ( 'NONE', ( #24687, #95554, #106406, #100207 ) ) ;
#92294 = CARTESIAN_POINT ( 'NONE',  ( -22.08327125186962192, 1523.604703353109699, 184.4267662568474009 ) ) ;
#92295 = FACE_OUTER_BOUND ( 'NONE', #1485, .T. ) ;
#92296 = DIRECTION ( 'NONE',  ( -1.000000000000000000, 0.000000000000000000, 0.000000000000000000 ) ) ;
#92297 = CARTESIAN_POINT ( 'NONE',  ( -2.207267873112999722E-10, 1469.464448464210136, 252.5672569689040188 ) ) ;
#92298 = CARTESIAN_POINT ( 'NONE',  ( -2.562340869413339828, 1517.151704408390060, 196.2891841806521711 ) ) ;
#92299 = CARTESIAN_POINT ( 'NONE',  ( -0.6907574904219989653, 1475.844123532889853, 198.0538682590990049 ) ) ;
#92300 = CARTESIAN_POINT ( 'NONE',  ( -105.2357120539999897, 1390.250932512190047, 306.4420972570590038 ) ) ;
#92301 = CARTESIAN_POINT ( 'NONE',  ( -7.951026619593350553, 1511.645702024530010, 215.1361908920979999 ) ) ;
#92302 = CARTESIAN_POINT ( 'NONE',  ( -8.602688007017421867, 1361.384357301913269, 207.6218459616987673 ) ) ;
#92303 = CARTESIAN_POINT ( 'NONE',  ( -45.67167540701009898, 1440.701191047660132, 266.1885089217859672 ) ) ;
#92304 = CARTESIAN_POINT ( 'NONE',  ( 3.787233628934549845, 1428.472671622899952, 216.4667291094249890 ) ) ;
#92305 = CARTESIAN_POINT ( 'NONE',  ( -8.046515503210001086, 1425.053020564090048, 207.2502090198989890 ) ) ;
#92306 = CARTESIAN_POINT ( 'NONE',  ( 4.031168767865001001, 1516.805675336850072, 208.3649472324300120 ) ) ;
#92307 = CARTESIAN_POINT ( 'NONE',  ( 5.091542648593849307, 1407.116995818669920, 221.1537445908610096 ) ) ;
#92308 = CARTESIAN_POINT ( 'NONE',  ( 5.035044309065482615, 1424.909721106467032, 226.7892474147294308 ) ) ;
#92309 = CARTESIAN_POINT ( 'NONE',  ( 7.335500683392449872, 1425.052454098660064, 212.5855600729070147 ) ) ;
#92310 = CARTESIAN_POINT ( 'NONE',  ( -26.61818857643220326, 1451.071572817590095, 136.3881969644360197 ) ) ;
#92311 = ORIENTED_EDGE ( 'NONE', *, *, #68464, .T. ) ;
#92312 = CARTESIAN_POINT ( 'NONE',  ( 21.37677629770000109, 1428.055008772630117, 225.6922921337979915 ) ) ;
#92314 = DIRECTION ( 'NONE',  ( 0.000000000000000000, -0.7071067811865474617, -0.7071067811865474617 ) ) ;
#92313 = CARTESIAN_POINT ( 'NONE',  ( -1.477410530420000034, 1458.407133990929879, 182.8647753367980044 ) ) ;
#92315 = CARTESIAN_POINT ( 'NONE',  ( -1.658081806242819971E-15, 1375.886883438980021, 209.1218459572589836 ) ) ;
#92316 = CARTESIAN_POINT ( 'NONE',  ( -20.99439929906685975, 1454.025623455535424, 225.3869460591365623 ) ) ;
#92317 = CARTESIAN_POINT ( 'NONE',  ( -28.15442856212169787, 1509.896234822020006, 200.8410265843269826 ) ) ;
#92318 = CARTESIAN_POINT ( 'NONE',  ( -15.88438700284329919, 1452.358365370260117, 147.2139129419049937 ) ) ;
#92319 = CARTESIAN_POINT ( 'NONE',  ( -25.73472869180000089, 1440.328566752500137, 138.3426558852979724 ) ) ;
#92320 = ORIENTED_EDGE ( 'NONE', *, *, #93379, .F. ) ;
#92321 = CARTESIAN_POINT ( 'NONE',  ( -5.359994163131460709, 1422.229041729120127, 144.9878932283519930 ) ) ;
#92322 = CARTESIAN_POINT ( 'NONE',  ( 17.17241001986483795, 1512.187213306747481, 179.6185504016043240 ) ) ;
#92323 = CARTESIAN_POINT ( 'NONE',  ( 16.22918548398149952, 1421.473783082869886, 227.2926025833970129 ) ) ;
#92324 = CARTESIAN_POINT ( 'NONE',  ( 9.835001303689999474, 1462.581801261389955, 210.2517437191489762 ) ) ;
#92325 = ORIENTED_EDGE ( 'NONE', *, *, #41428, .F. ) ;
#92326 = EDGE_LOOP ( 'NONE', ( #95785, #7697, #31021, #80720 ) ) ;
#92327 = CARTESIAN_POINT ( 'NONE',  ( -39.76976369060000138, 1384.853131567590026, 212.4474779504389801 ) ) ;
#92328 = CARTESIAN_POINT ( 'NONE',  ( -24.06092262379999980, 1410.732887028930008, 209.4001518044459829 ) ) ;
#92329 = CARTESIAN_POINT ( 'NONE',  ( -4.095484028299999579, 1423.950387520030063, 184.1987660818980146 ) ) ;
#92330 = DIRECTION ( 'NONE',  ( 0.000000000000000000, 1.000000000000000000, 0.000000000000000000 ) ) ;
#92331 = CARTESIAN_POINT ( 'NONE',  ( -8.828869558830000130, 1428.756629641229893, 91.31218443469779800 ) ) ;
#92332 = CARTESIAN_POINT ( 'NONE',  ( -2.316151605259999968, 1498.351462479429983, 236.5782940619979797 ) ) ;
#92334 = AXIS2_PLACEMENT_3D ( 'NONE', #85572, #91925, #15198 ) ;
#92333 = CARTESIAN_POINT ( 'NONE',  ( -20.46972343990000098, 1415.849044050329894, 220.3380584269980034 ) ) ;
#92335 = ORIENTED_EDGE ( 'NONE', *, *, #50002, .T. ) ;
#92336 = CARTESIAN_POINT ( 'NONE',  ( 45.72863391218620421, 1443.707261214470009, 268.7602522196279438 ) ) ;
#92337 = CARTESIAN_POINT ( 'NONE',  ( -10.86466539000899978, 1391.913060387130145, 205.6479294918659946 ) ) ;
#92338 = CARTESIAN_POINT ( 'NONE',  ( -0.006904034787109999440, 1420.198046511930215, 183.9035050854979829 ) ) ;
#92339 = CARTESIAN_POINT ( 'NONE',  ( -2.878693287274999957, 1516.766397346390022, 205.0941487061870134 ) ) ;
#92340 = ORIENTED_EDGE ( 'NONE', *, *, #59839, .F. ) ;
#92341 = CARTESIAN_POINT ( 'NONE',  ( 18.71873819915595405, 1458.256924698515377, 227.3233249423684015 ) ) ;
#92342 = CARTESIAN_POINT ( 'NONE',  ( 0.03085303418417100277, 1444.874163974749990, 199.0604885470160070 ) ) ;
#92343 = DIRECTION ( 'NONE',  ( 0.000000000000000000, 0.000000000000000000, 1.000000000000000000 ) ) ;
#92344 = ORIENTED_EDGE ( 'NONE', *, *, #19121, .F. ) ;
#92345 = CARTESIAN_POINT ( 'NONE',  ( -10.59763471844589944, 1480.490663172710128, 210.4673335203119962 ) ) ;
#92346 = CARTESIAN_POINT ( 'NONE',  ( 26.69869368971990298, 1451.980701177230003, 134.9228189439619996 ) ) ;
#92347 = CARTESIAN_POINT ( 'NONE',  ( -12.97811974145500002, 1512.378201925219855, 193.9098824635940161 ) ) ;
#92349 = CARTESIAN_POINT ( 'NONE',  ( 10.89674973356500054, 1502.604160945439844, 215.7130242589950058 ) ) ;
#92348 = CIRCLE ( 'NONE', #88779, 2.000000000000000000 ) ;
#92350 = CARTESIAN_POINT ( 'NONE',  ( 8.017723747350000707, 1421.540647238610063, 195.9972256206989982 ) ) ;
#92351 = CARTESIAN_POINT ( 'NONE',  ( -1.708172839108350161, 1432.537737004170140, 218.4855024170419995 ) ) ;
#92352 = CARTESIAN_POINT ( 'NONE',  ( 10.03970810010159909, 1480.319677133890082, 205.9223887158739785 ) ) ;
#92353 = CARTESIAN_POINT ( 'NONE',  ( 2.021802345552520030, 1408.983663280989958, 186.9337625968530006 ) ) ;
#92355 = CARTESIAN_POINT ( 'NONE',  ( -18.56260928087826656, 1424.353331803792344, 224.9312564898113749 ) ) ;
#92354 = CARTESIAN_POINT ( 'NONE',  ( -2.632747685671117832, 1375.413060387289988, 207.6835693458863830 ) ) ;
#92356 = CARTESIAN_POINT ( 'NONE',  ( 12.45662817246929954, 1427.088122696140090, 206.6493147128259977 ) ) ;
#92357 = CARTESIAN_POINT ( 'NONE',  ( -13.12553963729999928, 1379.406087309789882, 211.7521819623089812 ) ) ;
#92358 = CARTESIAN_POINT ( 'NONE',  ( 9.584198994920001269, 1428.531551829730233, 147.0197059986979866 ) ) ;
#92359 = ORIENTED_EDGE ( 'NONE', *, *, #62608, .F. ) ;
#92360 = CARTESIAN_POINT ( 'NONE',  ( 11.96392952312509905, 1414.971349104630008, 220.7371169548410137 ) ) ;
#92361 = CARTESIAN_POINT ( 'NONE',  ( 11.04095755852680050, 1432.346658633729930, 151.7150567104229992 ) ) ;
#92362 = CARTESIAN_POINT ( 'NONE',  ( 32.36513277069983019, 1523.847248782568613, 202.1343718111426426 ) ) ;
#92363 = CARTESIAN_POINT ( 'NONE',  ( -12.91306700440000022, 1390.089741809970064, 205.6071646888290161 ) ) ;
#92364 = CARTESIAN_POINT ( 'NONE',  ( 10.08433468493209872, 1427.583401277489884, 210.6616427254850237 ) ) ;
#92365 = CARTESIAN_POINT ( 'NONE',  ( 11.78821558584650120, 1425.864958446819855, 202.8633695863799744 ) ) ;
#92366 = CARTESIAN_POINT ( 'NONE',  ( 7.512750207965000371, 1509.038615934239942, 209.1218459511669892 ) ) ;
#92367 = CARTESIAN_POINT ( 'NONE',  ( 1.532107773980000135E-14, 1465.000168611230038, 255.3819207742980097 ) ) ;
#92368 = CARTESIAN_POINT ( 'NONE',  ( -22.01759379845357500, 1509.573295812402421, 191.3436680351161669 ) ) ;
#92369 = CARTESIAN_POINT ( 'NONE',  ( -20.59664500270120158, 1507.763472350329948, 190.3621299389660066 ) ) ;
#92370 = ADVANCED_FACE ( 'NONE', ( #84567 ), #27122, .F. ) ;
#92371 = CARTESIAN_POINT ( 'NONE',  ( 30.40113727430000168, 1448.202175313850148, 255.3819207682979595 ) ) ;
#92372 = CARTESIAN_POINT ( 'NONE',  ( -10.16653193143260125, 1461.891276504430152, 209.1676276534749945 ) ) ;
#92373 = CARTESIAN_POINT ( 'NONE',  ( -16.87240959569610155, 1409.502257913620042, 196.1298155364530089 ) ) ;
#92374 = CARTESIAN_POINT ( 'NONE',  ( -107.7676061301826280, 1389.569596624323367, 298.7085081970911915 ) ) ;
#92375 = CARTESIAN_POINT ( 'NONE',  ( 5.314820689285160604, 1466.895574952380002, 217.5561230666059771 ) ) ;
#92376 = CARTESIAN_POINT ( 'NONE',  ( -17.51176841079999846, 1485.959496867730195, 188.3680485027980183 ) ) ;
#92377 = CARTESIAN_POINT ( 'NONE',  ( -17.71193100849139768, 1519.551704408389924, 221.5709757781449980 ) ) ;
#92378 = CARTESIAN_POINT ( 'NONE',  ( -18.09437733770000278, 1410.908168226329963, 224.6134321192979826 ) ) ;
#92379 = CARTESIAN_POINT ( 'NONE',  ( 23.79684662030000197, 1410.916736074229902, 210.7771579475879946 ) ) ;
#92380 = AXIS2_PLACEMENT_3D ( 'NONE', #46166, #3611, #63526 ) ;
#92381 = CARTESIAN_POINT ( 'NONE',  ( 0.9412110656418017918, 1477.897737442060588, 198.7439859402530828 ) ) ;
#92382 = CARTESIAN_POINT ( 'NONE',  ( -17.41349417983979819, 1410.020399789049861, 193.4350316837939943 ) ) ;
#92383 = CARTESIAN_POINT ( 'NONE',  ( 1.098845374075520025E-07, 1407.083025879190018, 196.1147840738369723 ) ) ;
#92384 = CARTESIAN_POINT ( 'NONE',  ( -0.4681535437661719090, 1524.397344074316607, 173.8154889443011371 ) ) ;
#92385 = CARTESIAN_POINT ( 'NONE',  ( 2.740701587498710179, 1426.136123854220159, 188.7843822190389744 ) ) ;
#92386 = CARTESIAN_POINT ( 'NONE',  ( -12.50239388149999975, 1416.520646107730045, 222.1348954077979840 ) ) ;
#92387 = CARTESIAN_POINT ( 'NONE',  ( -15.00704310973959998, 1421.341523247710029, 203.5123511438659705 ) ) ;
#92388 = CARTESIAN_POINT ( 'NONE',  ( 0.2071197430525490157, 1458.969830049299844, 182.9972804725040021 ) ) ;
#92390 = VERTEX_POINT ( 'NONE', #16238 ) ;
#92389 = DIRECTION ( 'NONE',  ( -1.000000000000000000, 0.000000000000000000, 0.000000000000000000 ) ) ;
#92391 = CARTESIAN_POINT ( 'NONE',  ( -18.64337105059427913, 1443.913060387330233, 162.1710875046049694 ) ) ;
#92392 = CARTESIAN_POINT ( 'NONE',  ( 0.6370436997427018078, 1522.051704408389924, 200.3909606286928238 ) ) ;
#92393 = CARTESIAN_POINT ( 'NONE',  ( 12.40399033819999985, 1434.420133248469938, 149.8851994706980122 ) ) ;
#92394 = CARTESIAN_POINT ( 'NONE',  ( -41.65423399716719643, 1444.110307754890073, 134.0999999982789745 ) ) ;
#92395 = DIRECTION ( 'NONE',  ( 0.000000000000000000, 0.000000000000000000, -1.000000000000000000 ) ) ;
#92396 = ORIENTED_EDGE ( 'NONE', *, *, #88452, .T. ) ;
#92397 = CARTESIAN_POINT ( 'NONE',  ( -16.62424264452936029, 1524.075132568165600, 180.5391555246563087 ) ) ;
#92398 = CARTESIAN_POINT ( 'NONE',  ( 22.75273496409597485, 1511.187213306747708, 234.5707981297185825 ) ) ;
#92399 = DIRECTION ( 'NONE',  ( -0.3170185151553819858, -0.9051242360756870386, -0.2832832122048195012 ) ) ;
#92400 = CARTESIAN_POINT ( 'NONE',  ( -6.232532001854649728, 1405.413060387330006, 197.7132726571231558 ) ) ;
#92401 = EDGE_CURVE ( 'NONE', #11383, #575, #50984, .T. ) ;
#92402 = CARTESIAN_POINT ( 'NONE',  ( -1.204685347530000117, 1506.953552699789952, 221.9093730674989899 ) ) ;
#92403 = CARTESIAN_POINT ( 'NONE',  ( -107.3835680070587983, 1379.994974221857547, 309.2994170105861258 ) ) ;
#92404 = CARTESIAN_POINT ( 'NONE',  ( -14.01398736212220086, 1379.590348564800024, 211.9184487047760115 ) ) ;
#92405 = VECTOR ( 'NONE', #69819, 1000.000000000000000 ) ;
#92406 = CARTESIAN_POINT ( 'NONE',  ( -14.18177803620000077, 1380.146094623469935, 210.8656358578390098 ) ) ;
#92407 = CARTESIAN_POINT ( 'NONE',  ( 2.500000007239999711, 1434.165708943269919, 183.5270322547980015 ) ) ;
#92408 = CARTESIAN_POINT ( 'NONE',  ( -57.68740113826780203, 1385.050377599670128, 239.1317386132739955 ) ) ;
#92409 = CARTESIAN_POINT ( 'NONE',  ( -10.64049728136139983, 1391.913060387289988, 213.3044660420850107 ) ) ;
#92410 = CARTESIAN_POINT ( 'NONE',  ( 11.13275964168929910, 1426.431015207049768, 207.0489135758679993 ) ) ;
#92411 = VERTEX_POINT ( 'NONE', #85113 ) ;
#92412 = CARTESIAN_POINT ( 'NONE',  ( 11.87713710604131379, 1433.166847837657770, 149.9793738463967259 ) ) ;
#92413 = CARTESIAN_POINT ( 'NONE',  ( -16.12920693297470009, 1409.501579173550226, 225.4780555564630049 ) ) ;
#92415 = EDGE_LOOP ( 'NONE', ( #57387, #37955, #67908, #6088 ) ) ;
#92414 = CARTESIAN_POINT ( 'NONE',  ( 2.500000000000000000, 1418.913060387330006, 172.2701767054979882 ) ) ;
#92416 = DIRECTION ( 'NONE',  ( -1.000000000000000000, 0.000000000000000000, 0.000000000000000000 ) ) ;
#92417 = CARTESIAN_POINT ( 'NONE',  ( -19.85273216998108126, 1410.967088625417546, 221.2148261137424754 ) ) ;
#92418 = CARTESIAN_POINT ( 'NONE',  ( 15.81201445386249915, 1506.433683730510211, 224.3933755863170063 ) ) ;
#92419 = CARTESIAN_POINT ( 'NONE',  ( -0.08981465318181031110, 1420.356465652879933, 183.3314806077030141 ) ) ;
#92420 = DIRECTION ( 'NONE',  ( 0.000000000000000000, 0.000000000000000000, 1.000000000000000000 ) ) ;
#92421 = CARTESIAN_POINT ( 'NONE',  ( 15.52404075915854165, 1511.843510977572350, 197.7123968315431171 ) ) ;
#92422 = CARTESIAN_POINT ( 'NONE',  ( -15.96680046119999830, 1422.914845696529937, 228.4252575972979855 ) ) ;
#92423 = CARTESIAN_POINT ( 'NONE',  ( -3.208454056331284665, 1511.804172066353431, 201.1704017881504569 ) ) ;
#92424 = CARTESIAN_POINT ( 'NONE',  ( 9.103282207110000357, 1450.329653372990151, 206.7256654112989906 ) ) ;
#92425 = CARTESIAN_POINT ( 'NONE',  ( -113.4000000000000057, 1331.448250124730066, 287.0365551081090416 ) ) ;
#92426 = CARTESIAN_POINT ( 'NONE',  ( 6.553899686920000356, 1408.913060387329779, 225.8798606464979741 ) ) ;
#92427 = CARTESIAN_POINT ( 'NONE',  ( 0.01997215604490120214, 1457.681682718290176, 199.5608357732290017 ) ) ;
#92428 = CARTESIAN_POINT ( 'NONE',  ( 4.609064303374999838, 1516.723920667490120, 206.2441009858569885 ) ) ;
#92429 = AXIS2_PLACEMENT_3D ( 'NONE', #70098, #86856, #18524 ) ;
#92430 = CARTESIAN_POINT ( 'NONE',  ( 3.116049927029999722, 1446.579647245350088, 167.4613963303980029 ) ) ;
#92431 = ORIENTED_EDGE ( 'NONE', *, *, #65688, .T. ) ;
#92432 = CARTESIAN_POINT ( 'NONE',  ( -4.363122647530000009, 1416.108409730630001, 162.4768476156980057 ) ) ;
#92433 = CARTESIAN_POINT ( 'NONE',  ( -7.105427357599999217E-15, 1420.413060387330006, 188.2701767054980166 ) ) ;
#92435 = ORIENTED_EDGE ( 'NONE', *, *, #71827, .T. ) ;
#92434 = CARTESIAN_POINT ( 'NONE',  ( -68.48768668117180880, 1379.747307472329794, 280.1013031988870239 ) ) ;
#92436 = CARTESIAN_POINT ( 'NONE',  ( -17.51974517380610052, 1417.750436891259824, 206.7510270525189924 ) ) ;
#92437 = ORIENTED_EDGE ( 'NONE', *, *, #6044, .F. ) ;
#92438 = CARTESIAN_POINT ( 'NONE',  ( -16.78598030348177161, 1513.543684532448196, 222.3294674479041930 ) ) ;
#92439 = EDGE_CURVE ( 'NONE', #35481, #100091, #93772, .T. ) ;
#92440 = CARTESIAN_POINT ( 'NONE',  ( 11.70063000989999935, 1500.556383425389868, 207.1978923261789873 ) ) ;
#92442 = CARTESIAN_POINT ( 'NONE',  ( 16.40909233880620022, 1410.440661368950032, 191.7158404879280056 ) ) ;
#92441 = CARTESIAN_POINT ( 'NONE',  ( -11.13193939202500005, 1425.173970145079920, 142.6750931195440160 ) ) ;
#92443 = ADVANCED_FACE ( 'NONE', ( #48661 ), #90629, .T. ) ;
#92444 = CARTESIAN_POINT ( 'NONE',  ( 6.563254890855000134, 1517.139039350860003, 211.6051684241269868 ) ) ;
#92445 = CARTESIAN_POINT ( 'NONE',  ( 40.27241789890000234, 1443.136959010180135, 137.0603092562980123 ) ) ;
#92446 = ADVANCED_FACE ( 'NONE', ( #98480 ), #90072, .T. ) ;
#92447 = CARTESIAN_POINT ( 'NONE',  ( -45.31147080460000609, 1435.337549144299828, 266.2043115811979987 ) ) ;
#92448 = CARTESIAN_POINT ( 'NONE',  ( -5.923682464646780943, 1522.051704408389924, 223.8623791742500089 ) ) ;
#92449 = ADVANCED_FACE ( 'NONE', ( #13353 ), #47546, .T. ) ;
#92450 = CARTESIAN_POINT ( 'NONE',  ( 14.99814013759614539, 1461.964485411068381, 230.0038671489789976 ) ) ;
#92451 = CONTEXT_DEPENDENT_SHAPE_REPRESENTATION ( #82040, #37477 ) ;
#92452 = EDGE_CURVE ( 'NONE', #5500, #44794, #40454, .T. ) ;
#92453 = CARTESIAN_POINT ( 'NONE',  ( 36.14177852621219955, 1451.331926750559887, 134.0999999986410103 ) ) ;
#92454 = CARTESIAN_POINT ( 'NONE',  ( -40.20798285448640286, 1442.677115920979986, 137.0083301852329782 ) ) ;
#92455 = VERTEX_POINT ( 'NONE', #33466 ) ;
#92456 = CARTESIAN_POINT ( 'NONE',  ( 10.99044244102760004, 1479.494692313550104, 229.8297415043770116 ) ) ;
#92457 = CARTESIAN_POINT ( 'NONE',  ( 2.921131820879320440, 1415.930151663460038, 231.8786077272699799 ) ) ;
#92458 = ORIENTED_EDGE ( 'NONE', *, *, #53718, .T. ) ;
#92459 = ORIENTED_EDGE ( 'NONE', *, *, #91157, .F. ) ;
#92460 = CARTESIAN_POINT ( 'NONE',  ( -29.41270317694913672, 1509.945394547169371, 211.3255468430687927 ) ) ;
#92461 = CARTESIAN_POINT ( 'NONE',  ( 10.55680192255090155, 1452.714797730689952, 209.8973982115319927 ) ) ;
#92462 = CARTESIAN_POINT ( 'NONE',  ( -5.389604961048250154, 1507.858604756060004, 220.8468629847619980 ) ) ;
#92463 = CARTESIAN_POINT ( 'NONE',  ( 4.500000000000000000, 1425.929641636930000, 126.8043280305979863 ) ) ;
#92464 = CARTESIAN_POINT ( 'NONE',  ( 4.274335294360000148, 1515.341803653790066, 210.5964280301390090 ) ) ;
#92465 = AXIS2_PLACEMENT_3D ( 'NONE', #27847, #18866, #8815 ) ;
#92466 = CARTESIAN_POINT ( 'NONE',  ( -12.33854995039999913, 1378.601075279359975, 208.9290456525660034 ) ) ;
#92467 = CARTESIAN_POINT ( 'NONE',  ( 42.60628463180059811, 1443.705283475309898, 134.4205488470810224 ) ) ;
#92468 = CARTESIAN_POINT ( 'NONE',  ( 12.78723757108998704, 1416.835806623466169, 222.7043020517274670 ) ) ;
#92469 = CARTESIAN_POINT ( 'NONE',  ( 25.20424027759999674, 1437.598577823609958, 138.0428463375980073 ) ) ;
#92470 = CARTESIAN_POINT ( 'NONE',  ( -11.02757116259999925, 1391.621866938430003, 214.2885041620889979 ) ) ;
#92471 = EDGE_CURVE ( 'NONE', #6406, #14678, #2124, .T. ) ;
#92472 = CARTESIAN_POINT ( 'NONE',  ( -68.65280262021799729, 1384.728655164589782, 263.0730744108470276 ) ) ;
#92473 = ORIENTED_EDGE ( 'NONE', *, *, #58529, .F. ) ;
#92474 = CARTESIAN_POINT ( 'NONE',  ( 2.872208710164999790, 1517.145312756229941, 201.7840522196070197 ) ) ;
#92475 = CARTESIAN_POINT ( 'NONE',  ( -1.135898823814999847, 1516.958737650239982, 208.0022537503870126 ) ) ;
#92476 = VERTEX_POINT ( 'NONE', #67116 ) ;
#92477 = CARTESIAN_POINT ( 'NONE',  ( 11.75840501554399964, 1426.865784514229972, 145.6544800655120184 ) ) ;
#92478 = CARTESIAN_POINT ( 'NONE',  ( 4.668464111452093945, 1511.396722025383042, 217.5346420084381407 ) ) ;
#92479 = ORIENTED_EDGE ( 'NONE', *, *, #47144, .T. ) ;
#92480 = CARTESIAN_POINT ( 'NONE',  ( -13.72467564589999967, 1416.021639796329964, 221.7306982637980184 ) ) ;
#92481 = CARTESIAN_POINT ( 'NONE',  ( -11.86607447778760083, 1432.335962723229841, 150.0622432091620055 ) ) ;
#92482 = CARTESIAN_POINT ( 'NONE',  ( 21.83117874278439174, 1524.760046179776054, 233.6180677221980488 ) ) ;
#92483 = EDGE_CURVE ( 'NONE', #69558, #34577, #43971, .T. ) ;
#92484 = CARTESIAN_POINT ( 'NONE',  ( -10.82265089720440088, 1462.846529889819976, 206.8444605232329820 ) ) ;
#92485 = CARTESIAN_POINT ( 'NONE',  ( 21.69166379610710038, 1409.783307410840052, 206.3313277539500348 ) ) ;
#92486 = CARTESIAN_POINT ( 'NONE',  ( 10.42328684261450178, 1469.828409879329911, 207.1733329790250195 ) ) ;
#92487 = CARTESIAN_POINT ( 'NONE',  ( -11.16643438350000039, 1471.372555911289965, 206.7508257855590159 ) ) ;
#92488 = ADVANCED_FACE ( 'NONE', ( #9805 ), #93285, .T. ) ;
#92489 = CARTESIAN_POINT ( 'NONE',  ( -10.06780437910142645, 1410.639284901293877, 188.4524536534676429 ) ) ;
#92490 = CARTESIAN_POINT ( 'NONE',  ( -47.82285893009999711, 1379.680498130210026, 235.2466082674589813 ) ) ;
#92491 = CARTESIAN_POINT ( 'NONE',  ( -15.97096329820000093, 1473.842985808030107, 223.5132954784979802 ) ) ;
#92493 = LINE ( 'NONE', #57827, #90438 ) ;
#92492 = CARTESIAN_POINT ( 'NONE',  ( 15.26419385149999997, 1460.025905744229931, 232.1043486749979934 ) ) ;
#92494 = CARTESIAN_POINT ( 'NONE',  ( -4.802294408477028043, 1422.281227809200118, 184.7525987295207415 ) ) ;
#92495 = AXIS2_PLACEMENT_3D ( 'NONE', #67346, #93063, #25843 ) ;
#92496 = CARTESIAN_POINT ( 'NONE',  ( -3.260357166894999992, 1517.133889586189980, 216.8465783791270098 ) ) ;
#92497 = ORIENTED_EDGE ( 'NONE', *, *, #25421, .T. ) ;
#92498 = EDGE_CURVE ( 'NONE', #97770, #95189, #15042, .T. ) ;
#92499 = CARTESIAN_POINT ( 'NONE',  ( -22.62008889866104866, 1409.702957286100855, 209.3923290094326148 ) ) ;
#92500 = CARTESIAN_POINT ( 'NONE',  ( 0.000000000000000000, 1518.913060387330006, 209.1218459616979999 ) ) ;
#92501 = CARTESIAN_POINT ( 'NONE',  ( 1.323175339562953301, 1516.595782308469779, 216.8324875441551001 ) ) ;
#92502 = CARTESIAN_POINT ( 'NONE',  ( -2.480813923114999930, 1517.051603658920158, 214.1347848340070072 ) ) ;
#92503 = CARTESIAN_POINT ( 'NONE',  ( 2.329898844064780317, 1515.219291385429869, 213.4472495150509701 ) ) ;
#92504 = CARTESIAN_POINT ( 'NONE',  ( -11.60004869884644485, 1425.874190438160667, 138.5974276262502940 ) ) ;
#92506 = ORIENTED_EDGE ( 'NONE', *, *, #14782, .T. ) ;
#92505 = CARTESIAN_POINT ( 'NONE',  ( 4.833437557692500164, 1508.551704408439946, 213.0319999308929937 ) ) ;
#92507 = CARTESIAN_POINT ( 'NONE',  ( 0.5710642426230000401, 1435.008643400159826, 189.6733896163979978 ) ) ;
#92508 = CARTESIAN_POINT ( 'NONE',  ( -0.9525667512430020523, 1508.146044033290082, 220.9334930897990148 ) ) ;
#92509 = CARTESIAN_POINT ( 'NONE',  ( -11.68915241180000031, 1426.973230569230054, 148.0825247161979803 ) ) ;
#92510 = CARTESIAN_POINT ( 'NONE',  ( -2.103463323419999753, 1431.236868155990123, 214.4359102488789972 ) ) ;
#92511 = CARTESIAN_POINT ( 'NONE',  ( -109.9610541615100061, 1384.376359339889859, 311.4294103760240091 ) ) ;
#92512 = CARTESIAN_POINT ( 'NONE',  ( 11.86590152282269983, 1432.348277341620133, 151.0567667683120021 ) ) ;
#92513 = CARTESIAN_POINT ( 'NONE',  ( 8.104834441009998613, 1501.961773108790112, 207.6242399624189829 ) ) ;
#92514 = LINE ( 'NONE', #26416, #99819 ) ;
#92516 = CARTESIAN_POINT ( 'NONE',  ( -10.14004033922460124, 1481.416246290540130, 206.1146705078360242 ) ) ;
#92515 = CARTESIAN_POINT ( 'NONE',  ( -26.09377909390000028, 1495.363898751129909, 213.7758989565080014 ) ) ;
#92518 = FACE_OUTER_BOUND ( 'NONE', #63278, .T. ) ;
#92517 = CIRCLE ( 'NONE', #1353, 5.000000000000000888 ) ;
#92519 = EDGE_LOOP ( 'NONE', ( #2608, #5743, #98714, #79713 ) ) ;
#92520 = CARTESIAN_POINT ( 'NONE',  ( 3.253141137235000091, 1516.858171774179937, 205.8542424163969997 ) ) ;
#92521 = CARTESIAN_POINT ( 'NONE',  ( 4.933164704560000224, 1406.696844280630103, 269.4903318383980491 ) ) ;
#92522 = CARTESIAN_POINT ( 'NONE',  ( 0.1880691449870000032, 1408.919627906630012, 186.4705829950979989 ) ) ;
#92523 = CARTESIAN_POINT ( 'NONE',  ( 18.55657787220000188, 1449.736067588349897, 191.3116986559980148 ) ) ;
#92524 = CARTESIAN_POINT ( 'NONE',  ( 8.065173493921880876, 1506.579904882062237, 229.7035030383271419 ) ) ;
#92525 = EDGE_CURVE ( 'NONE', #48273, #109170, #36078, .T. ) ;
#92526 = CARTESIAN_POINT ( 'NONE',  ( 1.551945958219810073, 1454.746255304280112, 218.4022335687689917 ) ) ;
#92527 = CARTESIAN_POINT ( 'NONE',  ( 11.87275636863970085, 1432.783179063080070, 147.6501916617970096 ) ) ;
#92528 = CARTESIAN_POINT ( 'NONE',  ( -18.72407526530000155, 1458.246115540929850, 227.3156487912980026 ) ) ;
#92529 = CARTESIAN_POINT ( 'NONE',  ( -15.32028296150000024, 1415.735746099170001, 207.3531220195189917 ) ) ;
#92530 = CARTESIAN_POINT ( 'NONE',  ( -13.22933013659999979, 1444.724273266610226, 186.9257294308980022 ) ) ;
#92531 = CARTESIAN_POINT ( 'NONE',  ( -3.141117940442379908, 1485.405160230890033, 197.6410428545480045 ) ) ;
#92532 = CARTESIAN_POINT ( 'NONE',  ( -8.595910032225260622, 1436.830216193329989, 209.8479140031089969 ) ) ;
#92533 = CARTESIAN_POINT ( 'NONE',  ( 29.18127911709999722, 1415.346630214729885, 269.9487154676979799 ) ) ;
#92534 = CARTESIAN_POINT ( 'NONE',  ( 1.463768699429939923, 1492.321606822109970, 181.7584585652749922 ) ) ;
#92535 = CARTESIAN_POINT ( 'NONE',  ( -2.984513020910000147, 1427.913060387330006, 209.1218459616979999 ) ) ;
#92536 = CIRCLE ( 'NONE', #40682, 524.3013518614112627 ) ;
#92537 = ADVANCED_FACE ( 'NONE', ( #110193 ), #50318, .F. ) ;
#92538 = CARTESIAN_POINT ( 'NONE',  ( -11.15142467606159826, 1508.551704408290107, 209.1655305885859946 ) ) ;
#92539 = CARTESIAN_POINT ( 'NONE',  ( 30.51231035492521571, 1526.382868172863937, 218.1578534183718432 ) ) ;
#92540 = CARTESIAN_POINT ( 'NONE',  ( -2.111106103540000056, 1476.041150137029945, 267.5352996838980175 ) ) ;
#92541 = CARTESIAN_POINT ( 'NONE',  ( -6.754078978114156584, 1512.913060387330006, 184.4732361498326156 ) ) ;
#92542 = CARTESIAN_POINT ( 'NONE',  ( -14.77680793217355060, 1514.552080547093510, 192.8582046779301606 ) ) ;
#92543 = CARTESIAN_POINT ( 'NONE',  ( -5.050714599155177176, 1486.518763338962117, 182.0512026800892045 ) ) ;
#92544 = CARTESIAN_POINT ( 'NONE',  ( -45.47709076214669466, 1384.761897948679916, 252.4926689112959650 ) ) ;
#92545 = CARTESIAN_POINT ( 'NONE',  ( -106.4032899763519993, 1391.913060387289988, 304.0478018970730432 ) ) ;
#92546 = CARTESIAN_POINT ( 'NONE',  ( -6.558760908210000906, 1438.201672707379885, 154.7769642619979891 ) ) ;
#92547 = CARTESIAN_POINT ( 'NONE',  ( -107.2249090579999802, 1378.913060387289988, 300.8612202483589613 ) ) ;
#92548 = CARTESIAN_POINT ( 'NONE',  ( 4.226426730290000044, 1515.477082009390188, 208.7508285102820196 ) ) ;
#92549 = CARTESIAN_POINT ( 'NONE',  ( -13.95127756348659886, 1463.590397533409941, 223.6014887471609995 ) ) ;
#92550 = DIRECTION ( 'NONE',  ( -1.000000000000000000, 0.000000000000000000, 0.000000000000000000 ) ) ;
#92551 =( BOUNDED_CURVE ( )  B_SPLINE_CURVE ( 3, ( #16219, #65568, #67224, #40890 ),
 .UNSPECIFIED., .F., .T. ) 
 B_SPLINE_CURVE_WITH_KNOTS ( ( 4, 4 ),
 ( 1.005825317590492096, 2.135767310345805026 ),
 .UNSPECIFIED. ) 
 CURVE ( )  GEOMETRIC_REPRESENTATION_ITEM ( )  RATIONAL_B_SPLINE_CURVE ( ( 1.000000000000000000, 0.8964027527108247018, 0.8964027527108247018, 1.000000000000000000 ) ) 
 REPRESENTATION_ITEM ( '' )  );
#92552 = CARTESIAN_POINT ( 'NONE',  ( 0.000000000000000000, 1519.913060387329779, 209.1218459616979999 ) ) ;
#92553 = CARTESIAN_POINT ( 'NONE',  ( -15.04132722364800046, 1422.464884556249899, 228.7611645815219958 ) ) ;
#92554 = ADVANCED_FACE ( 'NONE', ( #76049 ), #13504, .T. ) ;
#92555 = CARTESIAN_POINT ( 'NONE',  ( -33.28034951413921760, 1522.382868172863937, 217.4407153818824838 ) ) ;
#92556 = ORIENTED_EDGE ( 'NONE', *, *, #28546, .F. ) ;
#92557 = CARTESIAN_POINT ( 'NONE',  ( -1.600048698852036821, 1401.254281879943164, 135.5999999980979851 ) ) ;
#92558 = CARTESIAN_POINT ( 'NONE',  ( 11.91319089239999940, 1436.492803299989873, 225.5464727294989871 ) ) ;
#92559 = CARTESIAN_POINT ( 'NONE',  ( -7.407689820122348223, 1511.025938507596948, 215.4649457401752102 ) ) ;
#92560 = CARTESIAN_POINT ( 'NONE',  ( 4.677562605192279399, 1434.889072343160024, 228.7640133632109780 ) ) ;
#92562 = CARTESIAN_POINT ( 'NONE',  ( 13.89869200000000049, 1452.835253893030085, 223.8385666725980059 ) ) ;
#92561 = CARTESIAN_POINT ( 'NONE',  ( -18.31941652021488665, 1522.051704408389924, 214.4156261991469421 ) ) ;
#92563 = B_SPLINE_CURVE_WITH_KNOTS ( 'NONE', 3,
 ( #89056, #12342, #46533, #29700, #4516, #30242, #63884, #55479, #12897, #38649, #21821, #90144, #81742, #57690, #76526, #108614, #51894, #26666, #66091, #26104, #74487, #77098, #17132, #31903, #9333, #100218, #86032, #40304, #51322, #407, #91805, #102272, #49277, #951, #23498, #83406, #110677, #85458, #8757, #35624, #15083, #25552, #8204 ),
 .UNSPECIFIED., .F., .F.,
 ( 4, 3, 3, 3, 3, 3, 3, 3, 3, 3, 3, 3, 3, 3, 4 ),
 ( -27.09462204860000156, -25.77410041705229915, -24.45357878550460029, -23.11321150369849775, -21.76171864759629671, -20.41647214834780044, -19.09105860935400045, -18.89473426365130138, -17.55491631884689951, -16.19268673722569929, -14.82069223479160058, -13.39723677660409962, -12.03725603264010147, -10.69631803245800228, -9.378668589109999232 ),
 .UNSPECIFIED. ) ;
#92564 = CARTESIAN_POINT ( 'NONE',  ( -121.5779650366699940, 1311.832804576489934, 299.7542032958689902 ) ) ;
#92565 = CARTESIAN_POINT ( 'NONE',  ( 8.446022254560531906, 1449.499043747640144, 203.1286689207940128 ) ) ;
#92566 = CARTESIAN_POINT ( 'NONE',  ( -0.07943192025475609430, 1419.763154935769990, 184.3780508227239920 ) ) ;
#92567 = CARTESIAN_POINT ( 'NONE',  ( -5.007588685045000432, 1516.804776704140068, 203.3466091393569855 ) ) ;
#92568 = DIRECTION ( 'NONE',  ( 5.980589973904019347E-17, -1.000000000000000000, 1.736889445713099699E-16 ) ) ;
#92570 = CARTESIAN_POINT ( 'NONE',  ( -13.45946769660000086, 1415.628674266529742, 221.4934452861980105 ) ) ;
#92569 = VECTOR ( 'NONE', #63608, 1000.000000000000114 ) ;
#92571 = CARTESIAN_POINT ( 'NONE',  ( 15.60002305023500035, 1512.080583811389943, 196.3149055962669820 ) ) ;
#92572 = FACE_BOUND ( 'NONE', #101935, .T. ) ;
#92573 = CARTESIAN_POINT ( 'NONE',  ( -43.51401419724399489, 1380.083813360000022, 232.6619762463070060 ) ) ;
#92574 = CARTESIAN_POINT ( 'NONE',  ( 21.53212336100769875, 1509.608430946529779, 228.7663254442010157 ) ) ;
#92576 = ORIENTED_EDGE ( 'NONE', *, *, #37851, .F. ) ;
#92575 = CARTESIAN_POINT ( 'NONE',  ( -36.30886271766330253, 1379.645996577580036, 223.9080834309320096 ) ) ;
#92577 = ORIENTED_EDGE ( 'NONE', *, *, #82353, .T. ) ;
#92578 = CARTESIAN_POINT ( 'NONE',  ( 11.79580364919999980, 1433.901673931670075, 150.9072373718979918 ) ) ;
#92579 = CARTESIAN_POINT ( 'NONE',  ( -2.678904600480000120, 1397.368089890330111, 222.0733538051979963 ) ) ;
#92580 = EDGE_LOOP ( 'NONE', ( #75139, #59800, #78453, #32857 ) ) ;
#92581 = CARTESIAN_POINT ( 'NONE',  ( -107.7196721970000084, 1378.913060387289988, 308.1225810710590167 ) ) ;
#92582 = EDGE_CURVE ( 'NONE', #35548, #94111, #53489, .T. ) ;
#92583 = CARTESIAN_POINT ( 'NONE',  ( -26.35475707739999862, 1507.985742211030129, 201.5462075370979846 ) ) ;
#92584 = CARTESIAN_POINT ( 'NONE',  ( 2.801043665294330243, 1515.551704203360032, 205.2926231557239873 ) ) ;
#92586 = CARTESIAN_POINT ( 'NONE',  ( -13.78816838342430096, 1508.464041683439973, 184.0619282346299883 ) ) ;
#92585 = CARTESIAN_POINT ( 'NONE',  ( -0.3050640126979990430, 1444.736015696789991, 199.0470353275990192 ) ) ;
#92587 = CARTESIAN_POINT ( 'NONE',  ( 8.417993523019999813, 1507.806286985430006, 234.9608247068980234 ) ) ;
#92588 = CARTESIAN_POINT ( 'NONE',  ( 4.283104481010000519, 1468.702552713330078, 183.4792885116980017 ) ) ;
#92589 = EDGE_CURVE ( 'NONE', #71163, #98390, #104421, .T. ) ;
#92590 = CARTESIAN_POINT ( 'NONE',  ( -9.257693745890000159, 1414.913060387329779, 195.2866393220980115 ) ) ;
#92591 = CARTESIAN_POINT ( 'NONE',  ( -22.12673812478050195, 1409.685743108969973, 209.8966867368829980 ) ) ;
#92592 = CARTESIAN_POINT ( 'NONE',  ( 10.52837420263239920, 1481.199010226290284, 208.2608686310830137 ) ) ;
#92593 = CARTESIAN_POINT ( 'NONE',  ( 2.500000000000000000, 1419.419920435030008, 142.4063544201979994 ) ) ;
#92594 = CARTESIAN_POINT ( 'NONE',  ( 11.57711677559999863, 1432.386434236500008, 151.1965308031980157 ) ) ;
#92595 = CARTESIAN_POINT ( 'NONE',  ( 7.881533592224999829, 1511.927085655870087, 202.8441633797569921 ) ) ;
#92596 = ORIENTED_EDGE ( 'NONE', *, *, #4413, .F. ) ;
#92597 = CARTESIAN_POINT ( 'NONE',  ( 13.17364486784780020, 1435.644391491809984, 150.5032994553720300 ) ) ;
#92598 = ORIENTED_EDGE ( 'NONE', *, *, #86562, .F. ) ;
#92599 = ORIENTED_EDGE ( 'NONE', *, *, #9971, .F. ) ;
#92600 = EDGE_CURVE ( 'NONE', #36027, #4206, #9217, .T. ) ;
#92601 = CARTESIAN_POINT ( 'NONE',  ( -19.29276911551260199, 1507.866073106370095, 229.6337110716330017 ) ) ;
#92602 = CARTESIAN_POINT ( 'NONE',  ( -9.181565401679998573, 1464.648192115530037, 232.7317226279979820 ) ) ;
#92603 = CIRCLE ( 'NONE', #46198, 33.13701971169416538 ) ;
#92604 = CARTESIAN_POINT ( 'NONE',  ( -108.0117080513960985, 1389.072098649294503, 309.9875421113430320 ) ) ;
#92605 = CARTESIAN_POINT ( 'NONE',  ( -7.328676208015000526, 1516.833844030519913, 216.0648195994369871 ) ) ;
#92606 = CARTESIAN_POINT ( 'NONE',  ( -7.976350790930257340, 1511.738149258256499, 212.4166275968371735 ) ) ;
#92607 = EDGE_CURVE ( 'NONE', #39656, #9799, #77741, .T. ) ;
#92608 = ORIENTED_EDGE ( 'NONE', *, *, #54852, .T. ) ;
#92609 = CARTESIAN_POINT ( 'NONE',  ( -11.92169980599999946, 1502.281710837490209, 208.9298105593169907 ) ) ;
#92610 = CARTESIAN_POINT ( 'NONE',  ( 2.500000000000000000, 1448.203471567069982, 169.7709218380130096 ) ) ;
#92611 = CARTESIAN_POINT ( 'NONE',  ( -3.771520291289999882, 1380.082072813469949, 207.5503167614189977 ) ) ;
#92612 = ORIENTED_EDGE ( 'NONE', *, *, #71307, .F. ) ;
#92613 = CARTESIAN_POINT ( 'NONE',  ( -7.724423432224999608, 1517.122088787240045, 205.6676733166769964 ) ) ;
#92614 = ORIENTED_EDGE ( 'NONE', *, *, #38357, .F. ) ;
#92615 = CARTESIAN_POINT ( 'NONE',  ( 5.786847739675000213, 1517.104497701820037, 209.8595134730280165 ) ) ;
#92616 = CARTESIAN_POINT ( 'NONE',  ( -19.21159046289999850, 1509.355098188429793, 230.6178137211979902 ) ) ;
#92617 = CARTESIAN_POINT ( 'NONE',  ( -12.40163225230000066, 1409.346134928529864, 191.0060158467980216 ) ) ;
#92618 = CARTESIAN_POINT ( 'NONE',  ( 7.521073031005000686, 1513.760531203580058, 215.9563302536469962 ) ) ;
#92620 = VERTEX_POINT ( 'NONE', #3095 ) ;
#92619 = CARTESIAN_POINT ( 'NONE',  ( -0.5081859946160119934, 1415.431750870129918, 226.9099371985450091 ) ) ;
#92621 = CARTESIAN_POINT ( 'NONE',  ( 22.84395564920000155, 1432.441498076889957, 216.6658011494079972 ) ) ;
#92622 = CARTESIAN_POINT ( 'NONE',  ( -32.97913964219445404, 1512.187213306747481, 197.9697544589750464 ) ) ;
#92623 = EDGE_CURVE ( 'NONE', #100575, #43125, #52378, .T. ) ;
#92625 = CARTESIAN_POINT ( 'NONE',  ( -102.7375125960000020, 1384.595838641269893, 311.2202755702589911 ) ) ;
#92624 = AXIS2_PLACEMENT_3D ( 'NONE', #22267, #89506, #65433 ) ;
#92626 = CARTESIAN_POINT ( 'NONE',  ( 8.503372964620000474, 1452.005661874290126, 212.9202014103589988 ) ) ;
#92627 = CIRCLE ( 'NONE', #49729, 1.999999999999999556 ) ;
#92628 = CARTESIAN_POINT ( 'NONE',  ( 8.283412044549999464, 1408.491064663830002, 270.2796699746979812 ) ) ;
#92629 = ADVANCED_FACE ( 'NONE', ( #11475 ), #30462, .F. ) ;
#92630 = CARTESIAN_POINT ( 'NONE',  ( 6.947377783174999877, 1517.009964551830080, 213.7374907746170152 ) ) ;
#92631 = AXIS2_PLACEMENT_3D ( 'NONE', #47804, #90336, #81939 ) ;
#92632 = CARTESIAN_POINT ( 'NONE',  ( 23.56944756660000095, 1409.993291288429873, 208.9546729833109850 ) ) ;
#92633 = LINE ( 'NONE', #9202, #35665 ) ;
#92634 = CARTESIAN_POINT ( 'NONE',  ( 17.49022258196330171, 1428.660011336650086, 204.2345431054930032 ) ) ;
#92635 = CIRCLE ( 'NONE', #97981, 2.500000000000002220 ) ;
#92636 = CARTESIAN_POINT ( 'NONE',  ( -31.81407709660760830, 1512.187213306747481, 221.9534378623334590 ) ) ;
#92637 = CARTESIAN_POINT ( 'NONE',  ( 4.044321679994999919, 1517.001127920769704, 211.4073335515969916 ) ) ;
#92638 = CARTESIAN_POINT ( 'NONE',  ( 9.327651199099038948, 1434.415569083649871, 206.2244204008570136 ) ) ;
#92639 = CARTESIAN_POINT ( 'NONE',  ( 17.27380198137656109, 1525.712835404586031, 181.5601764590613243 ) ) ;
#92640 = CARTESIAN_POINT ( 'NONE',  ( -15.90990259576500065, 1516.551704408390151, 220.0820010595669771 ) ) ;
#92642 = VERTEX_POINT ( 'NONE', #28263 ) ;
#92641 = CARTESIAN_POINT ( 'NONE',  ( -59.61585404930000465, 1389.535794964619981, 250.6150333764589675 ) ) ;
#92643 = CARTESIAN_POINT ( 'NONE',  ( -39.87565794312929768, 1385.182708064410235, 241.8885196562599731 ) ) ;
#92644 = CARTESIAN_POINT ( 'NONE',  ( 34.48978216789999607, 1443.099005942970052, 250.0021841735980388 ) ) ;
#92645 = CARTESIAN_POINT ( 'NONE',  ( 12.40160258794860049, 1420.584110727309962, 200.5244627772079866 ) ) ;
#92646 = CARTESIAN_POINT ( 'NONE',  ( -2.417252593174890940, 1495.142685870479681, 220.0295633172205214 ) ) ;
#92647 = CARTESIAN_POINT ( 'NONE',  ( -5.397648344820000332, 1433.838088735599968, 154.6405597680980009 ) ) ;
#92648 = FACE_OUTER_BOUND ( 'NONE', #31473, .T. ) ;
#92649 = DIRECTION ( 'NONE',  ( 0.9455185755993178454, 0.000000000000000000, -0.3255681544571537578 ) ) ;
#92651 = FACE_OUTER_BOUND ( 'NONE', #78665, .T. ) ;
#92650 = CARTESIAN_POINT ( 'NONE',  ( 2.872700517194999748, 1516.559109716219837, 216.8315272385270021 ) ) ;
#92652 = CARTESIAN_POINT ( 'NONE',  ( -20.71343476517491311, 1501.977400791986611, 238.3377464195766890 ) ) ;
#92653 = CARTESIAN_POINT ( 'NONE',  ( 10.32067503063590053, 1469.846144623479859, 207.1838946627530049 ) ) ;
#92654 = AXIS2_PLACEMENT_3D ( 'NONE', #5403, #11610, #106754 ) ;
#92655 = ORIENTED_EDGE ( 'NONE', *, *, #11965, .T. ) ;
#92656 = CARTESIAN_POINT ( 'NONE',  ( 7.714371502985000184, 1516.738222552470233, 203.3422428319769892 ) ) ;
#92657 = DIRECTION ( 'NONE',  ( 0.000000000000000000, 0.000000000000000000, 1.000000000000000000 ) ) ;
#92658 = CARTESIAN_POINT ( 'NONE',  ( 24.59498549419999947, 1440.913060393719888, 213.3385281389880106 ) ) ;
#92659 = CARTESIAN_POINT ( 'NONE',  ( -34.68852446352934749, 1522.382868172863709, 218.2490599186012048 ) ) ;
#92660 = DIRECTION ( 'NONE',  ( 0.000000000000000000, 0.000000000000000000, -1.000000000000000000 ) ) ;
#92661 = CARTESIAN_POINT ( 'NONE',  ( 4.509330006639999944, 1466.131481732889824, 218.7653230973990048 ) ) ;
#92662 = CARTESIAN_POINT ( 'NONE',  ( 12.09220637906934037, 1418.812808926449861, 229.3497755446491624 ) ) ;
#92663 = B_SPLINE_CURVE_WITH_KNOTS ( 'NONE', 3,
 ( #38939, #105627, #13728, #5355 ),
 .UNSPECIFIED., .F., .F.,
 ( 4, 4 ),
 ( 0.000000000000000000, 0.0002960034161023848394 ),
 .UNSPECIFIED. ) ;
#92664 = CARTESIAN_POINT ( 'NONE',  ( 28.38544967506950201, 1436.384351133610153, 136.6812180996950019 ) ) ;
#92665 = CARTESIAN_POINT ( 'NONE',  ( 37.86953476771359561, 1448.932043378939852, 136.3660121938399925 ) ) ;
#92666 = CARTESIAN_POINT ( 'NONE',  ( -23.64337581500000240, 1435.765689707139700, 212.0349968343079752 ) ) ;
#92667 = CARTESIAN_POINT ( 'NONE',  ( 19.05930086383897049, 1517.151704408390060, 195.1946787710221827 ) ) ;
#92668 = CARTESIAN_POINT ( 'NONE',  ( -109.7257039389999989, 1386.446923186560070, 297.1549502653589911 ) ) ;
#92669 = CARTESIAN_POINT ( 'NONE',  ( -17.37855975720000146, 1418.344423645829920, 226.3668775949979874 ) ) ;
#92670 = CARTESIAN_POINT ( 'NONE',  ( -20.85167060786264770, 1525.730671948511599, 184.1901411363043906 ) ) ;
#92671 = CARTESIAN_POINT ( 'NONE',  ( -37.69191876346824444, 1454.405435348816582, 269.5715054350180822 ) ) ;
#92672 = VERTEX_POINT ( 'NONE', #105535 ) ;
#92673 = CARTESIAN_POINT ( 'NONE',  ( -27.06019685167559885, 1499.595773131199849, 210.8334130608849932 ) ) ;
#92674 = CARTESIAN_POINT ( 'NONE',  ( -44.80680645038494703, 1434.320850119760053, 268.9981820606464566 ) ) ;
#92675 = EDGE_CURVE ( 'NONE', #73362, #77955, #64712, .T. ) ;
#92676 = AXIS2_PLACEMENT_3D ( 'NONE', #52401, #45109, #70876 ) ;
#92677 = CARTESIAN_POINT ( 'NONE',  ( 10.82822666301168546, 1452.534930380026481, 150.8032249175824973 ) ) ;
#92678 = CARTESIAN_POINT ( 'NONE',  ( 14.46096030374320129, 1429.566239157359860, 190.5376751034600034 ) ) ;
#92679 = CARTESIAN_POINT ( 'NONE',  ( 11.60004869885203327, 1427.311649295585767, 134.3124698398398493 ) ) ;
#92680 = B_SPLINE_CURVE_WITH_KNOTS ( 'NONE', 3,
 ( #24339, #42259, #15923, #58520, #76406, #70125, #35939, #95831, #19099, #83700 ),
 .UNSPECIFIED., .F., .F.,
 ( 4, 2, 2, 2, 4 ),
 ( 0.000000000000000000, 0.2500000000000384137, 0.3750000000000323075, 0.5000000000000262013, 1.000000000000000000 ),
 .UNSPECIFIED. ) ;
#92681 = CARTESIAN_POINT ( 'NONE',  ( -12.60265035039207504, 1445.042479274662128, 185.7580730998129184 ) ) ;
#92682 = CARTESIAN_POINT ( 'NONE',  ( -9.139549689176309499, 1438.859193681930265, 208.8000896448019716 ) ) ;
#92683 = CARTESIAN_POINT ( 'NONE',  ( -0.01912637926573700076, 1347.932035898419826, 206.1218459616989946 ) ) ;
#92684 = CARTESIAN_POINT ( 'NONE',  ( -7.687944582605556576, 1417.018756110837558, 231.0788709786680784 ) ) ;
#92685 = CARTESIAN_POINT ( 'NONE',  ( -1.816375554928643776, 1451.599121610970769, 154.0952112748995830 ) ) ;
#92686 = CARTESIAN_POINT ( 'NONE',  ( -17.85664671351639754, 1415.933499560010205, 209.2963377197989985 ) ) ;
#92687 = CARTESIAN_POINT ( 'NONE',  ( 25.18454231669999999, 1435.453564675389771, 136.2348277442980020 ) ) ;
#92688 = CARTESIAN_POINT ( 'NONE',  ( -12.95684771466127216, 1442.923466797464471, 169.4279956361965560 ) ) ;
#92690 = ORIENTED_EDGE ( 'NONE', *, *, #104758, .T. ) ;
#92689 = FACE_OUTER_BOUND ( 'NONE', #19811, .T. ) ;
#92691 = EDGE_CURVE ( 'NONE', #76035, #32612, #19852, .T. ) ;
#92692 = CARTESIAN_POINT ( 'NONE',  ( 0.1620860067197200105, 1416.842625005220043, 190.8755133330550109 ) ) ;
#92693 = CARTESIAN_POINT ( 'NONE',  ( -12.60774529335560779, 1379.062498616119001, 211.6870459221253498 ) ) ;
#92694 = EDGE_LOOP ( 'NONE', ( #73990, #30888, #83237, #7775 ) ) ;
#92695 = EDGE_LOOP ( 'NONE', ( #78195, #45827, #305, #103581 ) ) ;
#92696 = CARTESIAN_POINT ( 'NONE',  ( 17.55992563626299940, 1415.427621830080170, 209.2440911636060150 ) ) ;
#92698 = CARTESIAN_POINT ( 'NONE',  ( -25.06556152449999786, 1445.939394628079981, 220.8709965880979951 ) ) ;
#92697 = CARTESIAN_POINT ( 'NONE',  ( 42.06232341934592966, 1438.972018477124266, 269.6487565939506794 ) ) ;
#92699 = CARTESIAN_POINT ( 'NONE',  ( -1.073559339189999795, 1444.993510083389992, 218.0402162257890097 ) ) ;
#92700 = CARTESIAN_POINT ( 'NONE',  ( -11.71548584529999992, 1433.111737081540014, 150.8480738170979976 ) ) ;
#92701 = CARTESIAN_POINT ( 'NONE',  ( -12.29992035190429966, 1378.341876957339991, 209.9524196890029941 ) ) ;
#92702 = CARTESIAN_POINT ( 'NONE',  ( -2.720407840123674426, 1420.142528854944203, 186.0334220698562149 ) ) ;
#92703 = AXIS2_PLACEMENT_3D ( 'NONE', #20006, #63702, #36818 ) ;
#92704 = CARTESIAN_POINT ( 'NONE',  ( 7.664247930350000182, 1423.636725678029961, 212.7912655606789940 ) ) ;
#92705 = CARTESIAN_POINT ( 'NONE',  ( -13.97867491850210087, 1429.402194067919709, 222.2970902837259928 ) ) ;
#92706 = FACE_BOUND ( 'NONE', #61953, .T. ) ;
#92707 = CARTESIAN_POINT ( 'NONE',  ( 2.893622070869999785, 1451.002760034029734, 183.8359331502979614 ) ) ;
#92708 = CIRCLE ( 'NONE', #24748, 1.999999999999996669 ) ;
#92709 = CARTESIAN_POINT ( 'NONE',  ( 8.032334214226272806, 1363.687929514241205, 210.6218459617142003 ) ) ;
#92710 = CARTESIAN_POINT ( 'NONE',  ( -19.97979314536150142, 1483.906058459090218, 214.0067405813460084 ) ) ;
#92712 = VERTEX_POINT ( 'NONE', #90357 ) ;
#92711 = CYLINDRICAL_SURFACE ( 'NONE', #85466, 2.000000000000003553 ) ;
#92713 = VERTEX_POINT ( 'NONE', #22029 ) ;
#92714 = CARTESIAN_POINT ( 'NONE',  ( -11.84158678921130026, 1430.652403269130218, 149.7191781297279931 ) ) ;
#92715 = AXIS2_PLACEMENT_3D ( 'NONE', #102653, #7518, #85882 ) ;
#92716 = CARTESIAN_POINT ( 'NONE',  ( -0.06846930289512999368, 1501.841009900990002, 233.2444182323090160 ) ) ;
#92717 = CARTESIAN_POINT ( 'NONE',  ( -4.958608741100000827, 1473.061993129130087, 270.4263178540980448 ) ) ;
#92718 = CARTESIAN_POINT ( 'NONE',  ( -110.0630222465480017, 1384.919003957790210, 296.9512650941160246 ) ) ;
#92719 = CARTESIAN_POINT ( 'NONE',  ( -122.7580815721744614, 1314.643966242390661, 299.1095026942199411 ) ) ;
#92720 = CARTESIAN_POINT ( 'NONE',  ( -13.84676392108729992, 1425.218576473590019, 222.1679296936039805 ) ) ;
#92721 = EDGE_CURVE ( 'NONE', #21131, #84410, #105779, .T. ) ;
#92722 = CARTESIAN_POINT ( 'NONE',  ( -8.154761128900000600, 1384.841831967909911, 199.6474426925889816 ) ) ;
#92723 = DIRECTION ( 'NONE',  ( -1.755985294532469921E-16, 1.000000000000000000, -1.338183447452831989E-16 ) ) ;
#92724 = CARTESIAN_POINT ( 'NONE',  ( -18.02257621027557377, 1524.382868172863937, 235.3484976865589147 ) ) ;
#92725 = CARTESIAN_POINT ( 'NONE',  ( 11.39709565417286363, 1367.072585988989204, 209.6218459617033432 ) ) ;
#92726 = CARTESIAN_POINT ( 'NONE',  ( -10.31302053876249936, 1447.618248150379941, 210.0527956824380169 ) ) ;
#92727 = CARTESIAN_POINT ( 'NONE',  ( -10.57232560421230083, 1407.157108062349835, 269.2531376779569996 ) ) ;
#92728 = EDGE_CURVE ( 'NONE', #98935, #36118, #3880, .T. ) ;
#92729 = CARTESIAN_POINT ( 'NONE',  ( -13.69536319195090002, 1435.838696954500165, 150.2679701917390105 ) ) ;
#92730 = ORIENTED_EDGE ( 'NONE', *, *, #52310, .F. ) ;
#92731 = CARTESIAN_POINT ( 'NONE',  ( 2.493583506516910298, 1524.152349020271004, 242.7218833893027750 ) ) ;
#92732 = ORIENTED_EDGE ( 'NONE', *, *, #80244, .F. ) ;
#92733 = ORIENTED_EDGE ( 'NONE', *, *, #54473, .T. ) ;
#92734 = EDGE_CURVE ( 'NONE', #7082, #57816, #54012, .T. ) ;
#92735 = DIRECTION ( 'NONE',  ( 0.000000000000000000, -0.000000000000000000, 1.000000000000000000 ) ) ;
#92736 = CARTESIAN_POINT ( 'NONE',  ( 21.83550407203906119, 1523.678648413191468, 183.2743720722706655 ) ) ;
#92737 = AXIS2_PLACEMENT_3D ( 'NONE', #45399, #29664, #80074 ) ;
#92739 = CARTESIAN_POINT ( 'NONE',  ( 31.92108011125342770, 1512.187213306747481, 197.2845127572061301 ) ) ;
#92738 = CARTESIAN_POINT ( 'NONE',  ( 3.461047291624999911, 1516.858765657450249, 212.5691103191969944 ) ) ;
#92740 = CARTESIAN_POINT ( 'NONE',  ( 7.500396670941167798, 1516.934665496271919, 209.1219157010845322 ) ) ;
#92741 = EDGE_CURVE ( 'NONE', #7780, #32175, #37832, .T. ) ;
#92742 = CARTESIAN_POINT ( 'NONE',  ( 21.62164173326539895, 1517.151704408390060, 208.0273405521070060 ) ) ;
#92743 = VERTEX_POINT ( 'NONE', #20396 ) ;
#92744 = DIRECTION ( 'NONE',  ( 0.4090087482554252696, 0.000000000000000000, -0.9125304618753996566 ) ) ;
#92745 = CARTESIAN_POINT ( 'NONE',  ( -3.261635970955000019, 1516.613881697390070, 202.1867125516770045 ) ) ;
#92746 = CARTESIAN_POINT ( 'NONE',  ( 0.4151546846821903003, 1512.187213306747481, 242.9330574173806951 ) ) ;
#92747 = CARTESIAN_POINT ( 'NONE',  ( -35.55223107086649748, 1384.570145142690080, 209.1373044713860168 ) ) ;
#92748 = CARTESIAN_POINT ( 'NONE',  ( 3.375977085881459949, 1446.395221913229989, 199.5681764770490076 ) ) ;
#92749 = CARTESIAN_POINT ( 'NONE',  ( -7.042124254411990414, 1488.841176089370038, 189.4374097027819914 ) ) ;
#92751 = ORIENTED_EDGE ( 'NONE', *, *, #106537, .F. ) ;
#92750 = DIRECTION ( 'NONE',  ( 1.734723475976805517E-15, 0.000000000000000000, 1.000000000000000000 ) ) ;
#92752 = CARTESIAN_POINT ( 'NONE',  ( -25.74606116824569924, 1449.914928412390054, 208.7281950135569843 ) ) ;
#92753 = CARTESIAN_POINT ( 'NONE',  ( 27.46043822030000214, 1488.693027617030111, 209.1483437815799675 ) ) ;
#92754 = CARTESIAN_POINT ( 'NONE',  ( -28.27139721233027458, 1526.382868172864164, 219.5606225550389468 ) ) ;
#92755 = CARTESIAN_POINT ( 'NONE',  ( -9.263518881979999620, 1384.040644720069849, 200.0636813112390087 ) ) ;
#92756 = CARTESIAN_POINT ( 'NONE',  ( -23.99259057559999775, 1435.335336374720100, 136.7764849531980076 ) ) ;
#92757 = CARTESIAN_POINT ( 'NONE',  ( -24.91076472390000163, 1442.007094529510141, 210.4668357637779934 ) ) ;
#92758 = ADVANCED_FACE ( 'NONE', ( #46747 ), #65101, .T. ) ;
#92759 = CARTESIAN_POINT ( 'NONE',  ( 5.788436334164999586, 1517.116049120239950, 211.4102033778369787 ) ) ;
#92760 = CARTESIAN_POINT ( 'NONE',  ( -68.68265996670000106, 1379.747811297680300, 279.9579939446590515 ) ) ;
#92761 = CARTESIAN_POINT ( 'NONE',  ( 5.414082080120000917, 1435.477060051989838, 154.6761060569980089 ) ) ;
#92762 = CARTESIAN_POINT ( 'NONE',  ( 9.682534244272909874, 1436.279766483590038, 210.8540000661170097 ) ) ;
#92763 = B_SPLINE_CURVE_WITH_KNOTS ( 'NONE', 5,
 ( #90439, #80953, #29981, #54676, #38928, #81480, #98846, #28899, #22107, #73108, #105615, #5343 ),
 .UNSPECIFIED., .F., .F.,
 ( 6, 3, 3, 6 ),
 ( -8.927001670199999239, -7.815970586859999791, -6.076675143290000136, -3.686514310890000701 ),
 .UNSPECIFIED. ) ;
#92764 = DIRECTION ( 'NONE',  ( -0.4090087482554252696, 0.000000000000000000, 0.9125304618753996566 ) ) ;
#92765 = CARTESIAN_POINT ( 'NONE',  ( -2.882326017515000061, 1516.969638403840008, 207.4201161117570109 ) ) ;
#92766 = EDGE_CURVE ( 'NONE', #76507, #22264, #54600, .T. ) ;
#92767 = ORIENTED_EDGE ( 'NONE', *, *, #7158, .F. ) ;
#92768 = CARTESIAN_POINT ( 'NONE',  ( -33.91369120209999721, 1435.681798817159915, 134.0999984767980209 ) ) ;
#92769 = CARTESIAN_POINT ( 'NONE',  ( -11.40487640519999957, 1470.866518659589929, 208.6816973537609954 ) ) ;
#92770 = DIRECTION ( 'NONE',  ( -0.5877852522924762457, 0.000000000000000000, 0.8090169943749451198 ) ) ;
#92771 = ORIENTED_EDGE ( 'NONE', *, *, #70316, .F. ) ;
#92772 = CARTESIAN_POINT ( 'NONE',  ( -2.795964621609999590, 1422.864594294989956, 191.4386244948990168 ) ) ;
#92773 = CARTESIAN_POINT ( 'NONE',  ( 12.71462359147169963, 1434.614816316360020, 149.3386743435430049 ) ) ;
#92774 = B_SPLINE_SURFACE_WITH_KNOTS ( 'NONE', 5, 4, ( 
 ( #60943, #9956, #1033, #35156, #61491 ),
 ( #95072, #79933, #35711, #70453, #53085 ),
 ( #104574, #103449, #20545, #54204, #18338 ),
 ( #62622, #43570, #87793, #20011, #97270 ),
 ( #28423, #79382, #27868, #11076, #45244 ),
 ( #96739, #78263, #2697, #27310, #86115 ) ),
 .UNSPECIFIED., .F., .F., .F.,
 ( 6, 6 ),
 ( 5, 5 ),
 ( 0.000000000000000000, 111.1101480259999903 ),
 ( 25.81581217359999769, 39.03307591160000101 ),
 .UNSPECIFIED. ) ;
#92775 = CARTESIAN_POINT ( 'NONE',  ( 17.94638693882010116, 1459.309748162179858, 228.0675985784120314 ) ) ;
#92776 = FACE_OUTER_BOUND ( 'NONE', #38005, .T. ) ;
#92777 = CARTESIAN_POINT ( 'NONE',  ( 25.32264566339999945, 1452.028773922830169, 135.3109774066980151 ) ) ;
#92778 = CARTESIAN_POINT ( 'NONE',  ( 4.231776932839999894, 1487.020005215089896, 198.7423800976989980 ) ) ;
#92779 = CARTESIAN_POINT ( 'NONE',  ( -1.356522590139999984, 1410.335674019929911, 185.6037846922979782 ) ) ;
#92780 = PLANE ( 'NONE',  #471 ) ;
#92782 = CARTESIAN_POINT ( 'NONE',  ( -1.842963219480119985, 1515.064792700640055, 204.7923971808919816 ) ) ;
#92781 = CARTESIAN_POINT ( 'NONE',  ( -1.121383629864999953, 1517.104192383289956, 213.7476359466970166 ) ) ;
#92783 = CIRCLE ( 'NONE', #78497, 1.999999999999999556 ) ;
#92784 = CARTESIAN_POINT ( 'NONE',  ( -8.875811585187578956, 1385.236883567939913, 218.6688581284889779 ) ) ;
#92785 = CARTESIAN_POINT ( 'NONE',  ( 5.005700201405000271, 1516.732530461250008, 216.0598116305469887 ) ) ;
#92786 = VERTEX_POINT ( 'NONE', #88733 ) ;
#92787 = CARTESIAN_POINT ( 'NONE',  ( 7.721072739912949956, 1516.994132466350038, 209.3346182140349754 ) ) ;
#92788 = B_SPLINE_SURFACE_WITH_KNOTS ( 'NONE', 5, 5, ( 
 ( #43473, #110655, #93841, #77618, #51301, #60844 ),
 ( #42919, #75958, #69235, #103344, #26646, #18238 ),
 ( #28873, #54102, #38358, #88231, #46250, #19340 ),
 ( #3142, #87116, #54650, #89322, #70354, #97169 ),
 ( #70909, #29401, #96630, #28318, #64149, #19901 ),
 ( #10968, #44577, #10407, #37275, #45698, #53540 ),
 ( #72536, #78721, #61951, #2037, #36170, #105025 ),
 ( #106667, #20991, #11522, #62509, #36717, #63069 ),
 ( #79836, #104466, #71469, #105588, #27761, #96067 ),
 ( #29956, #87686, #20441, #88780, #18787, #12061 ),
 ( #80380, #3696, #37824, #72010, #45141, #79282 ),
 ( #2591, #106128, #63604, #97721, #55196, #12618 ),
 ( #46797, #80927, #52984, #4225, #73646, #15351 ),
 ( #73084, #108330, #22629, #6967, #56835, #14810 ),
 ( #49545, #82585, #55751, #23207, #57945, #38902 ),
 ( #92077, #39476, #108880, #65243, #107777, #32724 ),
 ( #14257, #90409, #13139, #89870, #5876, #48447 ),
 ( #83670, #41121, #47323, #30514, #81453, #4758 ) ),
 .UNSPECIFIED., .F., .F., .F.,
 ( 6, 3, 3, 3, 3, 6 ),
 ( 6, 6 ),
 ( 30.30137858949999696, 39.81263101060000054, 43.27628380800000230, 45.00811020669999607, 46.73993660539999695, 49.32388343160000233 ),
 ( 0.000000000000000000, 1.452596962060000108 ),
 .UNSPECIFIED. ) ;
#92789 = CARTESIAN_POINT ( 'NONE',  ( -32.85805783624314813, 1523.678648413191695, 201.0453875934059340 ) ) ;
#92790 = AXIS2_PLACEMENT_3D ( 'NONE', #40172, #31218, #56994 ) ;
#92791 = CARTESIAN_POINT ( 'NONE',  ( 1.611684368509999965, 1420.766153637229991, 184.2335115979979889 ) ) ;
#92792 = CONICAL_SURFACE ( 'NONE', #58841, 1.499999999999955369, 0.3430239404209998177 ) ;
#92793 = CARTESIAN_POINT ( 'NONE',  ( -3.657993755839999750, 1474.872004365689918, 218.7367895275489786 ) ) ;
#92794 = DIRECTION ( 'NONE',  ( 0.000000000000000000, 0.000000000000000000, 1.000000000000000000 ) ) ;
#92795 = UNCERTAINTY_MEASURE_WITH_UNIT (LENGTH_MEASURE( 1.000000000000000082E-05 ), #4196, 'distance_accuracy_value', 'NONE');
#92796 = CARTESIAN_POINT ( 'NONE',  ( -7.545023643077629849, 1384.923116630999857, 219.0875805831419996 ) ) ;
#92797 = CARTESIAN_POINT ( 'NONE',  ( 11.60004869885177925, 1426.116582408723389, 139.0978670934243553 ) ) ;
#92798 = CARTESIAN_POINT ( 'NONE',  ( -4.543595434040840431, 1508.194578301092406, 220.5427723295427143 ) ) ;
#92799 = CARTESIAN_POINT ( 'NONE',  ( 18.95816141779999953, 1416.822690122629865, 210.4639565196879971 ) ) ;
#92800 = CARTESIAN_POINT ( 'NONE',  ( 16.84932835999988754, 1507.643874508232784, 231.2344471367978826 ) ) ;
#92801 = CARTESIAN_POINT ( 'NONE',  ( 15.02262665340000147, 1434.992946305229907, 196.2760509299980072 ) ) ;
#92802 = CARTESIAN_POINT ( 'NONE',  ( 39.17967913610949893, 1440.913060373489770, 258.0998150948020111 ) ) ;
#92804 = LINE ( 'NONE', #16614, #108777 ) ;
#92803 = CARTESIAN_POINT ( 'NONE',  ( -10.94914411430109880, 1470.861661619450160, 209.5252488941420097 ) ) ;
#92805 = CARTESIAN_POINT ( 'NONE',  ( 12.97602761339999944, 1422.949401640830047, 222.4689737549979895 ) ) ;
#92806 = EDGE_LOOP ( 'NONE', ( #14307, #72208, #106463, #41293 ) ) ;
#92807 = VERTEX_POINT ( 'NONE', #12016 ) ;
#92808 = DIRECTION ( 'NONE',  ( 5.980589973904019347E-17, -1.000000000000000000, 1.736889445713099699E-16 ) ) ;
#92809 = CARTESIAN_POINT ( 'NONE',  ( -5.159279705950000405, 1438.838331987589982, 207.0068192150190214 ) ) ;
#92810 = CARTESIAN_POINT ( 'NONE',  ( -27.79064046509999741, 1508.605033444930086, 210.4916514804280041 ) ) ;
#92811 = CARTESIAN_POINT ( 'NONE',  ( 7.793708231120000107, 1423.746790494559946, 195.8019968817989991 ) ) ;
#92812 = VECTOR ( 'NONE', #45954, 1000.000000000000114 ) ;
#92813 = CARTESIAN_POINT ( 'NONE',  ( -13.82431552801049968, 1379.697172790399918, 208.1616873013680049 ) ) ;
#92814 = CARTESIAN_POINT ( 'NONE',  ( 9.753082900275339640, 1422.542729491349974, 212.4417178624250084 ) ) ;
#92815 = CARTESIAN_POINT ( 'NONE',  ( -1.514738108749209999, 1507.606285622480073, 232.0384771855580084 ) ) ;
#92816 = CARTESIAN_POINT ( 'NONE',  ( 18.19590854887482578, 1522.644714754858796, 180.0410247165244471 ) ) ;
#92817 = CARTESIAN_POINT ( 'NONE',  ( -74.68581025115760497, 1383.781068242549964, 299.5368704359049730 ) ) ;
#92818 = CARTESIAN_POINT ( 'NONE',  ( 23.58949756300000189, 1451.946940865630040, 139.7425502278979934 ) ) ;
#92819 = CARTESIAN_POINT ( 'NONE',  ( 10.94256459999999898, 1470.964391698490090, 209.6240817813279875 ) ) ;
#92820 = CARTESIAN_POINT ( 'NONE',  ( 11.01161918054969924, 1492.458987749750122, 212.4071534856509800 ) ) ;
#92822 = ORIENTED_EDGE ( 'NONE', *, *, #14485, .T. ) ;
#92821 = CARTESIAN_POINT ( 'NONE',  ( -2.909142857259999992, 1456.184073613490000, 218.1442093800189923 ) ) ;
#92823 = CARTESIAN_POINT ( 'NONE',  ( 34.61172972909617584, 1523.342713519622976, 218.2049768989050449 ) ) ;
#92824 = CARTESIAN_POINT ( 'NONE',  ( -49.82325338690000649, 1381.578505732160011, 226.8201688485589784 ) ) ;
#92825 = CARTESIAN_POINT ( 'NONE',  ( 19.81748036228530196, 1508.389368817880040, 229.3831171527509980 ) ) ;
#92826 = ORIENTED_EDGE ( 'NONE', *, *, #15213, .T. ) ;
#92827 = ORIENTED_EDGE ( 'NONE', *, *, #100468, .T. ) ;
#92828 = CARTESIAN_POINT ( 'NONE',  ( -7.846308076728210068, 1385.913410601039914, 218.8401308622059958 ) ) ;
#92829 = CARTESIAN_POINT ( 'NONE',  ( 37.16250662717590103, 1438.008325804049946, 136.5646560650300216 ) ) ;
#92831 = CARTESIAN_POINT ( 'NONE',  ( -22.59589169820000265, 1507.700907224229923, 208.9176257130850161 ) ) ;
#92830 = CARTESIAN_POINT ( 'NONE',  ( -3.269259737218870310, 1476.740802116999930, 199.2818558394819775 ) ) ;
#92832 = CARTESIAN_POINT ( 'NONE',  ( 11.68690449393020003, 1479.943320198230140, 210.6621425521760216 ) ) ;
#92833 = CARTESIAN_POINT ( 'NONE',  ( -106.2922410430000042, 1378.604080016899843, 300.8096223931590316 ) ) ;
#92834 = CARTESIAN_POINT ( 'NONE',  ( 1.956348389710000024, 1444.118055948189976, 203.1454441604489887 ) ) ;
#92835 = CARTESIAN_POINT ( 'NONE',  ( 41.66090683250000382, 1443.836063800979900, 135.6920700532980106 ) ) ;
#92836 = CARTESIAN_POINT ( 'NONE',  ( 14.38276615811350645, 1518.913060387330006, 235.4493228183861504 ) ) ;
#92837 = CARTESIAN_POINT ( 'NONE',  ( -3.494218103360000161, 1450.155609024890055, 190.3271737256989979 ) ) ;
#92838 = CARTESIAN_POINT ( 'NONE',  ( 1.236505811250000031, 1408.956240125730119, 186.2695617811980071 ) ) ;
#92839 = CARTESIAN_POINT ( 'NONE',  ( 4.585187189710000055, 1425.138335953130081, 185.5538527434979983 ) ) ;
#92840 = CARTESIAN_POINT ( 'NONE',  ( -11.54436755831595995, 1432.352357148824467, 151.3410661337507008 ) ) ;
#92841 = CARTESIAN_POINT ( 'NONE',  ( -2.705111913362410192, 1440.761320489169975, 170.5389615272939920 ) ) ;
#92842 = AXIS2_PLACEMENT_3D ( 'NONE', #858, #11861, #85373 ) ;
#92843 = CARTESIAN_POINT ( 'NONE',  ( 11.81707102253409936, 1430.266227662830033, 147.2485957573000235 ) ) ;
#92844 = VERTEX_POINT ( 'NONE', #3646 ) ;
#92845 = CARTESIAN_POINT ( 'NONE',  ( 3.813082683120000433E-15, 1426.500992774829911, 146.0666368882980066 ) ) ;
#92846 = CARTESIAN_POINT ( 'NONE',  ( 18.93827134509360022, 1456.920588905010163, 229.2656879365239888 ) ) ;
#92847 = CARTESIAN_POINT ( 'NONE',  ( 15.91888908530000180, 1468.833198747830011, 189.4696677705980221 ) ) ;
#92848 = AXIS2_PLACEMENT_3D ( 'NONE', #25896, #194, #102595 ) ;
#92849 = DIRECTION ( 'NONE',  ( 0.9149707217702669482, 0.000000000000000000, 0.4035202328300239172 ) ) ;
#92850 = EDGE_CURVE ( 'NONE', #72650, #66010, #72487, .T. ) ;
#92851 = CARTESIAN_POINT ( 'NONE',  ( 20.50381857201226765, 1436.445248144109883, 144.8890132701617404 ) ) ;
#92852 = CARTESIAN_POINT ( 'NONE',  ( -0.9044596846589999517, 1416.819756528429934, 228.0287516232980067 ) ) ;
#92853 = CARTESIAN_POINT ( 'NONE',  ( 1.002066158240000115, 1476.232001529690251, 198.0640689639990057 ) ) ;
#92854 = CARTESIAN_POINT ( 'NONE',  ( -105.5819434490000077, 1390.739035477769903, 306.4716207183589631 ) ) ;
#92855 = CARTESIAN_POINT ( 'NONE',  ( -7.533847566356209668, 1510.598356033829987, 215.0345739407800068 ) ) ;
#92856 = CARTESIAN_POINT ( 'NONE',  ( -9.178315062050000250, 1363.109187794150102, 207.6218459616989946 ) ) ;
#92857 = CARTESIAN_POINT ( 'NONE',  ( -45.97693700823750618, 1439.231401605989959, 268.4976759586160142 ) ) ;
#92858 = CARTESIAN_POINT ( 'NONE',  ( 0.7577247913304160365, 1429.693372890590126, 217.4019828439899698 ) ) ;
#92859 = CARTESIAN_POINT ( 'NONE',  ( -9.093965512229999604, 1423.880366148619942, 207.4491482849089721 ) ) ;
#92860 = CARTESIAN_POINT ( 'NONE',  ( 5.775625077365000415, 1516.745833913490060, 208.3665194962490261 ) ) ;
#92861 = CARTESIAN_POINT ( 'NONE',  ( -9.123030677640000974, 1385.451960981700040, 199.9749920654289781 ) ) ;
#92862 = CARTESIAN_POINT ( 'NONE',  ( -32.85805783624314813, 1523.678648413191695, 201.0453875934059340 ) ) ;
#92863 = CARTESIAN_POINT ( 'NONE',  ( 7.340346552482979625, 1426.363565825339947, 212.7077574225189949 ) ) ;
#92864 = AXIS2_PLACEMENT_3D ( 'NONE', #106181, #107277, #63656 ) ;
#92865 = CARTESIAN_POINT ( 'NONE',  ( -27.01904753585120034, 1451.963896065450172, 135.0863428763389891 ) ) ;
#92866 = VERTEX_POINT ( 'NONE', #71966 ) ;
#92867 = EDGE_CURVE ( 'NONE', #4207, #36154, #89755, .T. ) ;
#92868 = CARTESIAN_POINT ( 'NONE',  ( 9.325404832400000288, 1417.437270712429836, 238.2842636990980054 ) ) ;
#92870 = CARTESIAN_POINT ( 'NONE',  ( -15.19278571033129843, 1512.351864386150055, 222.0468280374129790 ) ) ;
#92869 = CARTESIAN_POINT ( 'NONE',  ( -11.43932180835810186, 1491.557538122099913, 206.8739097152079864 ) ) ;
#92871 =( BOUNDED_SURFACE ( )  B_SPLINE_SURFACE ( 3, 2, ( 
 ( #84930, #8777, #51344 ),
 ( #25019, #102289, #93338 ),
 ( #970, #17153, #58659 ),
 ( #84399, #110699, #25571 ),
 ( #59221, #85478, #58112 ),
 ( #7686, #68726, #92245 ),
 ( #15515, #7143, #42958 ),
 ( #77119, #94432, #17711 ),
 ( #76545, #50269, #16603 ),
 ( #50801, #41844, #33991 ),
 ( #109606, #425, #33421 ),
 ( #67070, #83844, #8224 ),
 ( #41299, #34542, #102830 ),
 ( #26125, #86054, #32880 ) ),
 .UNSPECIFIED., .F., .F., .F. ) 
 B_SPLINE_SURFACE_WITH_KNOTS ( ( 4, 2, 2, 2, 2, 2, 4 ),
 ( 3, 3 ),
 ( 0.000000000000000000, 0.0009440840677143950543, 0.001416126101571592473, 0.001888168135428790109, 0.002360210169285987744, 0.002832252203143184946, 0.003776336270857580217 ),
 ( 0.000000000000000000, 1.000000000000000000 ),
 .UNSPECIFIED. ) 
 GEOMETRIC_REPRESENTATION_ITEM ( )  RATIONAL_B_SPLINE_SURFACE ( (
 ( 1.000000000000000000, 0.8070209408750023128, 1.000000000000000000),
 ( 1.000000000000000000, 0.8215603905285601138, 1.000000000000000000),
 ( 1.000000000000000000, 0.8340988699059065370, 1.000000000000000000),
 ( 1.000000000000000000, 0.8516751610459424304, 1.000000000000000000),
 ( 1.000000000000000000, 0.8573697395158380585, 1.000000000000000000),
 ( 1.000000000000000000, 0.8683586635658061548, 1.000000000000000000),
 ( 1.000000000000000000, 0.8736518481709314443, 1.000000000000000000),
 ( 1.000000000000000000, 0.8840377753029409202, 1.000000000000000000),
 ( 1.000000000000000000, 0.8891294171307203564, 1.000000000000000000),
 ( 1.000000000000000000, 0.8992456600573149883, 1.000000000000000000),
 ( 1.000000000000000000, 0.9042785869252324416, 1.000000000000000000),
 ( 1.000000000000000000, 0.9189749222839583842, 1.000000000000000000),
 ( 1.000000000000000000, 0.9283978182347611963, 1.000000000000000000),
 ( 1.000000000000000000, 0.9376006582765945563, 1.000000000000000000) ) ) 
 REPRESENTATION_ITEM ( '' )  SURFACE ( )  );
#92872 = CARTESIAN_POINT ( 'NONE',  ( -0.5875326727945574534, 1487.946859735538737, 219.9643640775660458 ) ) ;
#92873 = CARTESIAN_POINT ( 'NONE',  ( -16.52604361424539903, 1508.522046710420000, 213.6181396652249873 ) ) ;
#92874 = CARTESIAN_POINT ( 'NONE',  ( 7.897123973650000295, 1424.702922360419961, 211.7415114879590021 ) ) ;
#92875 = EDGE_CURVE ( 'NONE', #98602, #36895, #92027, .T. ) ;
#92876 = CARTESIAN_POINT ( 'NONE',  ( -6.754078978114156584, 1519.913060387329779, 184.4732361498326156 ) ) ;
#92877 = CARTESIAN_POINT ( 'NONE',  ( 18.13864071049999893, 1429.364573343489837, 207.4452956957889853 ) ) ;
#92878 = ORIENTED_EDGE ( 'NONE', *, *, #49516, .F. ) ;
#92879 = CARTESIAN_POINT ( 'NONE',  ( -32.02808312589908013, 1512.187213306747481, 219.9649204700466782 ) ) ;
#92880 = CARTESIAN_POINT ( 'NONE',  ( 0.000000000000000000, 1515.551704408389924, 209.1218459616989946 ) ) ;
#92881 = CARTESIAN_POINT ( 'NONE',  ( 9.761911793579997720, 1462.730917074890158, 209.3821448747769978 ) ) ;
#92882 = ORIENTED_EDGE ( 'NONE', *, *, #72798, .T. ) ;
#92883 = ORIENTED_EDGE ( 'NONE', *, *, #56640, .F. ) ;
#92884 = CARTESIAN_POINT ( 'NONE',  ( -23.97223816435240096, 1410.985435140949903, 209.8860510689419812 ) ) ;
#92885 = ORIENTED_EDGE ( 'NONE', *, *, #30453, .F. ) ;
#92886 = CARTESIAN_POINT ( 'NONE',  ( -109.9857364230449974, 1384.899971927750130, 311.4562996732899478 ) ) ;
#92887 = AXIS2_PLACEMENT_3D ( 'NONE', #4902, #15488, #82159 ) ;
#92888 = CARTESIAN_POINT ( 'NONE',  ( -6.984406781949999754, 1427.831049039629988, 123.0297916884979941 ) ) ;
#92889 = B_SPLINE_SURFACE_WITH_KNOTS ( 'NONE', 5, 5, ( 
 ( #98970, #64306, #80542, #55903, #90573, #31224 ),
 ( #90021, #13298, #47491, #65406, #11675, #37434 ),
 ( #54796, #97328, #105752, #45852, #79984, #63221 ),
 ( #20597, #83282, #33408, #75459, #8210, #15501 ),
 ( #110683, #49699, #41829, #41285, #49150, #23904 ),
 ( #91130, #74360, #100620, #83829, #65958, #6025 ),
 ( #23367, #31771, #74903, #7130, #100083, #108488 ),
 ( #57557, #109594, #67056, #91680, #32865, #48600 ),
 ( #109052, #82734, #42376, #76531, #67603, #58099 ),
 ( #14955, #33974, #32337, #6580, #25005, #50785 ),
 ( #93326, #40729, #66517, #92230, #101162, #24456 ),
 ( #58644, #25558, #84385, #92778, #101713, #16053 ),
 ( #50257, #75984, #68170, #7672, #102277, #110135 ),
 ( #59207, #14407, #16588, #84918, #40179, #1498 ),
 ( #86039, #70379, #10434, #96090, #60299, #19367 ) ),
 .UNSPECIFIED., .F., .F., .F.,
 ( 6, 3, 3, 3, 6 ),
 ( 6, 6 ),
 ( 14.35637078220000085, 25.15719987230000143, 30.14272855600000156, 32.63549289790000074, 35.12825723969999814 ),
 ( 0.000000000000000000, 2.000000000000000000 ),
 .UNSPECIFIED. ) ;
#92890 = CARTESIAN_POINT ( 'NONE',  ( -12.15081611480000134, 1498.343186948530047, 232.9523657193980171 ) ) ;
#92891 = CARTESIAN_POINT ( 'NONE',  ( -19.73144153160000158, 1410.871738074529958, 221.4848234238980069 ) ) ;
#92892 = ORIENTED_EDGE ( 'NONE', *, *, #69299, .F. ) ;
#92893 = CARTESIAN_POINT ( 'NONE',  ( 45.44632409768470183, 1446.108118615839885, 266.4255912768500139 ) ) ;
#92894 = CARTESIAN_POINT ( 'NONE',  ( -0.7134561372089449627, 1424.170322885679980, 228.2193000291970293 ) ) ;
#92895 = PLANE ( 'NONE',  #100769 ) ;
#92896 = CARTESIAN_POINT ( 'NONE',  ( -0.7564342523539989704, 1516.783665406140017, 204.5091745923169810 ) ) ;
#92897 = EDGE_CURVE ( 'NONE', #26041, #86132, #95134, .T. ) ;
#92898 = ORIENTED_EDGE ( 'NONE', *, *, #60395, .F. ) ;
#92899 = CARTESIAN_POINT ( 'NONE',  ( -11.23615794200000018, 1433.983026149579928, 151.5834757130979824 ) ) ;
#92900 = CARTESIAN_POINT ( 'NONE',  ( 15.31201878717920017, 1512.804203059160045, 195.4761085552559905 ) ) ;
#92901 = CARTESIAN_POINT ( 'NONE',  ( 22.57319362359999815, 1409.701316935530031, 208.7927549349429910 ) ) ;
#92902 = ORIENTED_EDGE ( 'NONE', *, *, #5642, .T. ) ;
#92904 = VECTOR ( 'NONE', #92568, 1000.000000000000000 ) ;
#92903 = CARTESIAN_POINT ( 'NONE',  ( -10.78779494798200034, 1480.680906080729983, 211.1296427397590207 ) ) ;
#92905 = CARTESIAN_POINT ( 'NONE',  ( 26.73360441909009921, 1451.227420629079916, 136.2859150302269882 ) ) ;
#92906 = CARTESIAN_POINT ( 'NONE',  ( -3.545811734980049756, 1508.551704408389924, 213.8736419469829855 ) ) ;
#92907 = CARTESIAN_POINT ( 'NONE',  ( 5.220070305037049607, 1452.730771515490005, 152.0329402684909894 ) ) ;
#92908 = CARTESIAN_POINT ( 'NONE',  ( 7.823331862799999037, 1421.665691048000099, 195.8606073899989894 ) ) ;
#92910 = B_SPLINE_SURFACE_WITH_KNOTS ( 'NONE', 5, 5, ( 
 ( #97853, #89467, #62657, #3287, #22229, #39042 ),
 ( #72682, #46941, #45835, #55889, #96779, #13285 ),
 ( #73223, #106806, #107366, #21683, #88370, #38504 ),
 ( #37418, #64291, #97313, #4903, #11660, #12761 ),
 ( #105736, #71051, #20582, #48023, #29020, #30662 ),
 ( #47476, #81060, #29555, #98956, #81599, #30096 ),
 ( #4373, #90558, #98411, #54782, #3842, #63206 ),
 ( #105173, #20050, #88914, #12200, #46395, #80526 ),
 ( #37969, #72150, #63740, #73788, #33396, #57543 ) ),
 .UNSPECIFIED., .F., .F., .F.,
 ( 6, 3, 6 ),
 ( 6, 6 ),
 ( 0.7655572723410000169, 2.316155491860000026, 3.835724788439999866 ),
 ( 0.000000000000000000, 1.000000000000000000 ),
 .UNSPECIFIED. ) ;
#92909 = CARTESIAN_POINT ( 'NONE',  ( 17.72062905389999798, 1409.531878389729854, 220.9701597516980200 ) ) ;
#92911 = DIRECTION ( 'NONE',  ( -1.224646799147350002E-16, 1.836970198721029688E-16, 1.000000000000000000 ) ) ;
#92912 = CARTESIAN_POINT ( 'NONE',  ( 1.928639190254139990, 1408.980409951920137, 186.9081713113440060 ) ) ;
#92914 = DIRECTION ( 'NONE',  ( 0.000000000000000000, 0.000000000000000000, 1.000000000000000000 ) ) ;
#92913 = CARTESIAN_POINT ( 'NONE',  ( 2.041787225690000263, 1417.577345369830027, 234.8566030110980023 ) ) ;
#92915 = CARTESIAN_POINT ( 'NONE',  ( -16.62350534370865418, 1524.082740465118604, 180.5404690658195932 ) ) ;
#92916 = B_SPLINE_CURVE_WITH_KNOTS ( 'NONE', 3,
 ( #1978, #36113, #59664, #868, #52379, #51814, #87623, #27158, #53480, #77564, #33884, #94909, #76447, #10341, #104410, #18183, #17612, #26019, #60784, #103280, #93773, #85954, #9793, #44514, #43959, #17051, #60216, #1403, #51248, #35544, #85381, #95462, #69739, #61890, #19276, #42295, #110601, #8676, #77016, #322, #68623, #102725, #94334, #9255, #10910, #71408, #46734, #89260, #13078, #20386, #28253, #3635, #70853, #37212, #107160, #3085, #80867, #38843, #72477, #12555, #21475, #47265, #96569, #98205, #63547, #29347, #98757, #105522, #104963, #81388, #11465, #97662, #46187, #64085, #106067, #29891, #64636, #36657, #12006, #55685, #89808, #45084, #28811, #79226, #63010, #62444, #37763, #30452, #4166, #38296, #106607, #80318, #4701, #20934, #97117, #2535, #54589, #88173, #55140, #79778, #45640, #19841, #54046, #73021, #88724, #71956, #22018, #56215, #82522, #32660, #74682, #7455, #14749, #49477, #108262 ),
 .UNSPECIFIED., .F., .F.,
 ( 4, 3, 3, 3, 3, 3, 3, 3, 3, 3, 3, 3, 3, 3, 3, 3, 3, 3, 3, 3, 3, 3, 3, 3, 3, 3, 3, 3, 3, 3, 3, 3, 3, 3, 3, 3, 3, 3, 4 ),
 ( 12.74698783810000080, 13.96492021158590013, 15.19021758214300100, 16.42218468397550168, 17.66253057083640243, 18.90660447896850016, 20.15461610509670010, 20.77312021709999712, 22.02323751836510013, 23.27242081405690044, 24.51932165410020303, 25.76266663883209773, 26.99840962570149827, 28.22887374697500107, 29.44992649507029725, 30.29491413010000045, 31.53003531328260323, 32.76773977463359699, 34.00715209279349693, 35.24735736430879740, 36.48697184716329645, 37.72530858092299866, 38.96034359410540304, 39.81482060289999936, 41.03520056654750192, 42.26691267544130426, 43.50464977309270154, 44.74750943314289486, 45.99445407601399438, 47.24535532816859984, 48.49720425972940063, 49.74861903010859976, 50.51404411539999728, 51.76209235851399626, 53.00622896957969488, 54.24216509689028953, 55.47265940268459872, 56.69304412978929975, 57.85069212525870341 ),
 .UNSPECIFIED. ) ;
#92917 = CARTESIAN_POINT ( 'NONE',  ( -10.49741166160000105, 1379.367595482069873, 215.6674695879490002 ) ) ;
#92918 = DIRECTION ( 'NONE',  ( 1.755985294532464991E-16, -1.000000000000000000, 1.338183447452830017E-16 ) ) ;
#92919 = ORIENTED_EDGE ( 'NONE', *, *, #11025, .T. ) ;
#92920 = CARTESIAN_POINT ( 'NONE',  ( -32.85805783624317655, 1523.678648413191695, 201.0453875934059056 ) ) ;
#92921 = CYLINDRICAL_SURFACE ( 'NONE', #71358, 2.000000000000002220 ) ;
#92922 = CARTESIAN_POINT ( 'NONE',  ( -11.24957740497779923, 1482.901240094499826, 205.2054264539789870 ) ) ;
#92923 = B_SPLINE_SURFACE_WITH_KNOTS ( 'NONE', 5, 5, ( 
 ( #82855, #30240, #72822, #64975, #108051, #22929 ),
 ( #65531, #73922, #80665, #106955, #57133, #5047 ),
 ( #48173, #30797, #97462, #47615, #13425, #98550 ),
 ( #89054, #38646, #82311, #39192, #6144, #64434 ),
 ( #4514, #40302, #14540, #89602, #21819, #48729 ),
 ( #22369, #12895, #31347, #39762, #74485, #63882 ),
 ( #63342, #97997, #20731, #47072, #12340, #46531 ),
 ( #55477, #73369, #3979, #38103, #72281, #106413 ),
 ( #21267, #81196, #58771, #101283, #24026, #15081 ),
 ( #58226, #109182, #102407, #76119, #109718, #7799 ),
 ( #43075, #92350, #77235, #41421, #32466, #42506 ),
 ( #85597, #49275, #92908, #41965, #40855, #24578 ),
 ( #31901, #100742, #83404, #16182, #16721, #110815 ),
 ( #15622, #49828, #75586, #67735, #34108, #32993 ),
 ( #50383, #93450, #66641, #25137, #75030, #101844 ),
 ( #84511, #110259, #66088, #59340, #33535, #85052 ),
 ( #50921, #8342, #83958, #8897, #7258, #59884 ),
 ( #67182, #6700, #76666, #68299, #25689, #94009 ),
 ( #17274, #51465, #100215, #23496, #57688, #91803 ),
 ( #52033, #27364, #44744, #94555, #17828, #35772 ),
 ( #36314, #96229, #86169, #9462, #43627, #77775 ) ),
 .UNSPECIFIED., .F., .F., .F.,
 ( 6, 3, 3, 3, 3, 3, 6 ),
 ( 6, 6 ),
 ( 0.000000000000000000, 5.488753621229999879, 8.789679567349999445, 9.802594204569999192, 10.53188235890000080, 11.38341475070000008, 12.02704502919999996 ),
 ( 0.000000000000000000, 0.5000000000000000000 ),
 .UNSPECIFIED. ) ;
#92924 = CARTESIAN_POINT ( 'NONE',  ( -14.14948096550000045, 1390.186770710789915, 206.8378643784789972 ) ) ;
#92925 = CARTESIAN_POINT ( 'NONE',  ( 9.067461874531819177, 1422.840410830630162, 212.2224494962840140 ) ) ;
#92926 = CARTESIAN_POINT ( 'NONE',  ( 12.10217674255069831, 1421.433546240750047, 203.4323860903909917 ) ) ;
#92927 = CARTESIAN_POINT ( 'NONE',  ( -11.03055288841810011, 1462.470873763560121, 208.6170698419460052 ) ) ;
#92928 = CARTESIAN_POINT ( 'NONE',  ( -5.757839680740000077, 1468.063065667029832, 262.6648722463980334 ) ) ;
#92929 = CARTESIAN_POINT ( 'NONE',  ( -9.998385933616845023, 1478.713224390999585, 212.3145837183469666 ) ) ;
#92930 = CARTESIAN_POINT ( 'NONE',  ( 11.00807055750000174, 1433.414002013319987, 151.7532352853980058 ) ) ;
#92931 = CARTESIAN_POINT ( 'NONE',  ( 16.86383896579999941, 1465.456048507830019, 262.6648722511980054 ) ) ;
#92932 = B_SPLINE_SURFACE_WITH_KNOTS ( 'NONE', 5, 5, ( 
 ( #54279, #80004, #4410, #43244, #37452, #97889 ),
 ( #38539, #89502, #34824, #62128, #29055, #11163 ),
 ( #106839, #2773, #36893, #63241, #97347, #72185 ),
 ( #51639, #20618, #29588, #54821, #88945, #12238 ),
 ( #46427, #80560, #3875, #38003, #55369, #74381 ),
 ( #32356, #98987, #40748, #64880, #83303, #55920 ) ),
 .UNSPECIFIED., .F., .F., .F.,
 ( 6, 6 ),
 ( 6, 6 ),
 ( 9.225465320329998775, 10.07010781710000025 ),
 ( 0.000000000000000000, 2.000000000000000000 ),
 .UNSPECIFIED. ) ;
#92933 = CARTESIAN_POINT ( 'NONE',  ( -9.826755612460519984, 1461.294814416169856, 209.7781363122770131 ) ) ;
#92934 = CARTESIAN_POINT ( 'NONE',  ( -16.80096818656820190, 1420.465473985719882, 203.2469209014659839 ) ) ;
#92935 = AXIS2_PLACEMENT_3D ( 'NONE', #90083, #66586, #64920 ) ;
#92936 = CARTESIAN_POINT ( 'NONE',  ( 11.48582467623369929, 1425.717167183619949, 202.9080862240699901 ) ) ;
#92937 = FACE_OUTER_BOUND ( 'NONE', #45700, .T. ) ;
#92938 = CARTESIAN_POINT ( 'NONE',  ( 12.78776258891489981, 1416.851343896290018, 222.2791104166909975 ) ) ;
#92939 = CARTESIAN_POINT ( 'NONE',  ( -14.10814497719999849, 1418.505680634830014, 227.3595528058979767 ) ) ;
#92940 = CARTESIAN_POINT ( 'NONE',  ( -16.88043746970000214, 1409.502538253129842, 223.8714129622979954 ) ) ;
#92941 = VECTOR ( 'NONE', #67264, 1000.000000000000114 ) ;
#92942 = CARTESIAN_POINT ( 'NONE',  ( -8.118158757799047720, 1425.416527785969265, 208.7218458587759358 ) ) ;
#92943 = PLANE ( 'NONE',  #3827 ) ;
#92944 = CARTESIAN_POINT ( 'NONE',  ( -16.19056346127430146, 1409.478447324650006, 193.3259909677289841 ) ) ;
#92945 = CARTESIAN_POINT ( 'NONE',  ( -14.86200884888219953, 1383.858700832289969, 219.2304258842500246 ) ) ;
#92946 = CARTESIAN_POINT ( 'NONE',  ( 12.69240854808390040, 1426.852967891420121, 205.1934168669720009 ) ) ;
#92947 = CARTESIAN_POINT ( 'NONE',  ( -9.299436737415328835, 1446.922292678779968, 190.6945112243980134 ) ) ;
#92948 = CARTESIAN_POINT ( 'NONE',  ( -14.47400497512000150, 1421.606899549969967, 203.6042114461530161 ) ) ;
#92949 = CARTESIAN_POINT ( 'NONE',  ( 0.1721355080774560065, 1479.076444530880053, 182.1340621069099939 ) ) ;
#92951 = ORIENTED_EDGE ( 'NONE', *, *, #106730, .F. ) ;
#92950 = CARTESIAN_POINT ( 'NONE',  ( 0.06979892568819999477, 1408.910622955130066, 223.8076866983980153 ) ) ;
#92952 = CARTESIAN_POINT ( 'NONE',  ( -13.14421740897469704, 1444.740067931810472, 164.8757063741590230 ) ) ;
#92953 = DIRECTION ( 'NONE',  ( -0.000000000000000000, 1.000000000000000000, 0.000000000000000000 ) ) ;
#92954 = CARTESIAN_POINT ( 'NONE',  ( 13.80507509150000089, 1434.979586913100093, 149.8855771064980047 ) ) ;
#92955 = CARTESIAN_POINT ( 'NONE',  ( -41.40218316859470349, 1445.741963847249963, 134.0999999985380100 ) ) ;
#92956 = CARTESIAN_POINT ( 'NONE',  ( -109.3499934019999955, 1384.883594448820077, 297.1386964685590328 ) ) ;
#92957 = ORIENTED_EDGE ( 'NONE', *, *, #62066, .T. ) ;
#92958 = DIRECTION ( 'NONE',  ( 0.4999999999998399058, 0.7071067811867739472, -0.4999999999998399058 ) ) ;
#92959 = CARTESIAN_POINT ( 'NONE',  ( 2.470168521978401088, 1523.382868172864164, 175.3649660270905315 ) ) ;
#92960 = CARTESIAN_POINT ( 'NONE',  ( -105.2453956327515954, 1381.073543364039097, 308.6760955912837971 ) ) ;
#92961 = DIRECTION ( 'NONE',  ( 1.000000000000000000, 0.000000000000000000, 0.000000000000000000 ) ) ;
#92962 = CARTESIAN_POINT ( 'NONE',  ( -3.273107898713619957, 1432.100754207539921, 216.8813792401940077 ) ) ;
#92963 = CARTESIAN_POINT ( 'NONE',  ( -107.8212372937749421, 1380.513613017200441, 309.7939830466359581 ) ) ;
#92964 = VECTOR ( 'NONE', #58523, 1000.000000000000000 ) ;
#92965 = CARTESIAN_POINT ( 'NONE',  ( 22.09712912739999879, 1489.469559537729992, 210.0355320487269921 ) ) ;
#92966 = DIRECTION ( 'NONE',  ( -5.980589973904019347E-17, 1.000000000000000000, -1.736889445713099699E-16 ) ) ;
#92967 = CARTESIAN_POINT ( 'NONE',  ( 3.424114012090000436, 1431.484821031499905, 184.9008735491980246 ) ) ;
#92968 = CARTESIAN_POINT ( 'NONE',  ( -75.71336797908890048, 1385.139485295300119, 276.6772571808519956 ) ) ;
#92969 = CARTESIAN_POINT ( 'NONE',  ( -11.27004030100790111, 1391.913060387289988, 211.7974019302799888 ) ) ;
#92970 = CARTESIAN_POINT ( 'NONE',  ( 11.80015117941170111, 1427.466181701940059, 208.7971124954779896 ) ) ;
#92971 = CARTESIAN_POINT ( 'NONE',  ( -28.55009427459999927, 1451.055185256330105, 136.3289724744979878 ) ) ;
#92972 = CARTESIAN_POINT ( 'NONE',  ( 16.90776107416510143, 1442.831169986189479, 162.4346387413914385 ) ) ;
#92974 = ORIENTED_EDGE ( 'NONE', *, *, #27677, .T. ) ;
#92973 = CARTESIAN_POINT ( 'NONE',  ( -31.43069643840509642, 1526.748660780343471, 201.6857111062228967 ) ) ;
#92975 = CARTESIAN_POINT ( 'NONE',  ( 3.610101826099999744, 1473.850871782889953, 219.1404246027990155 ) ) ;
#92976 = B_SPLINE_CURVE_WITH_KNOTS ( 'NONE', 5,
 ( #89464, #39040, #22227, #28461, #46391, #63204, #81058, #107364, #30094 ),
 .UNSPECIFIED., .F., .F.,
 ( 6, 3, 6 ),
 ( -13.00939335640000039, -6.504696678220000194, 0.000000000000000000 ),
 .UNSPECIFIED. ) ;
#92977 = CARTESIAN_POINT ( 'NONE',  ( -9.638115897704999213, 1516.551704408390151, 203.7504991310570119 ) ) ;
#92978 = CARTESIAN_POINT ( 'NONE',  ( -9.178315062074918984, 1363.109187794137824, 210.6218459616987957 ) ) ;
#92979 = CARTESIAN_POINT ( 'NONE',  ( -11.77958525670000078, 1491.567240239189914, 205.4571824156389823 ) ) ;
#92980 = CARTESIAN_POINT ( 'NONE',  ( 39.14117453815377701, 1452.031574234373693, 269.5953450738427932 ) ) ;
#92981 = FACE_OUTER_BOUND ( 'NONE', #48723, .T. ) ;
#92982 = CARTESIAN_POINT ( 'NONE',  ( 14.97515213747811380, 1430.621276459560022, 220.1205205015936031 ) ) ;
#92983 = CARTESIAN_POINT ( 'NONE',  ( -5.513435588854999736, 1508.551704408389924, 216.1347675159770176 ) ) ;
#92984 = CARTESIAN_POINT ( 'NONE',  ( 9.279405576849999449, 1450.853110856889771, 207.7367179272790167 ) ) ;
#92985 = DIRECTION ( 'NONE',  ( -0.3390050494208924348, 0.7071067811868634312, -0.6205445805634688394 ) ) ;
#92986 = CARTESIAN_POINT ( 'NONE',  ( 24.16067383110895506, 1509.761787560979656, 192.2118785171494721 ) ) ;
#92987 = CARTESIAN_POINT ( 'NONE',  ( -2.880592967115000125, 1516.859514182039902, 206.2568738160869941 ) ) ;
#92988 = CARTESIAN_POINT ( 'NONE',  ( 2.500000010130000394, 1447.770735655929911, 162.7884763477979959 ) ) ;
#92989 = EDGE_LOOP ( 'NONE', ( #17445, #68996, #71995, #64882, #26407 ) ) ;
#92990 = CARTESIAN_POINT ( 'NONE',  ( -109.1111611177930030, 1384.583257041720117, 311.2497810013429671 ) ) ;
#92991 = CARTESIAN_POINT ( 'NONE',  ( -7.027906745119999823E-11, 1474.175172799329857, 270.1377427386980230 ) ) ;
#92993 = ORIENTED_EDGE ( 'NONE', *, *, #17104, .T. ) ;
#92992 = CARTESIAN_POINT ( 'NONE',  ( -68.58042545469770346, 1379.747469642939905, 280.1935340281700633 ) ) ;
#92994 = CARTESIAN_POINT ( 'NONE',  ( -8.233476245617373124, 1382.138012879694315, 218.4303649234365423 ) ) ;
#92995 = ORIENTED_EDGE ( 'NONE', *, *, #76825, .F. ) ;
#92996 = CARTESIAN_POINT ( 'NONE',  ( -16.61266726653357040, 1514.059034353336983, 223.2167079213704710 ) ) ;
#92997 = CARTESIAN_POINT ( 'NONE',  ( -23.86310425759999987, 1449.793994890560043, 202.1964979560380016 ) ) ;
#92999 = CARTESIAN_POINT ( 'NONE',  ( 16.07520829236349869, 1409.725530412830039, 192.1484554476330118 ) ) ;
#92998 = CARTESIAN_POINT ( 'NONE',  ( -10.84109190673120082, 1425.665916405870121, 103.8959551503590006 ) ) ;
#93000 = CARTESIAN_POINT ( 'NONE',  ( -4.995623491025000362, 1516.636036526019780, 210.8344906863870278 ) ) ;
#93001 = CARTESIAN_POINT ( 'NONE',  ( 34.99705909933560122, 1436.617605928890043, 136.4767353441200157 ) ) ;
#93002 = AXIS2_PLACEMENT_3D ( 'NONE', #99749, #57243, #74580 ) ;
#93003 = CARTESIAN_POINT ( 'NONE',  ( 2.477004153399889219, 1449.252234172512999, 182.3064460912110576 ) ) ;
#93004 = B_SPLINE_SURFACE_WITH_KNOTS ( 'NONE', 5, 5, ( 
 ( #5287, #92051, #73619, #65214, #30484, #24280, #14784, #58462, #22600 ),
 ( #92590, #15861, #6936, #50066, #100448, #7492, #31032, #90378, #48969 ),
 ( #22052, #40542, #83103, #56249, #108848, #107748, #90941, #57918, #14227 ),
 ( #82559, #42207, #86957, #9157, #27069, #24816, #84740, #9695, #68528 ),
 ( #86407, #52282, #93679, #76358, #8038, #77468, #101528, #85856, #43863 ),
 ( #110507, #60687, #61253, #43322, #34353, #75810, #76919, #102627, #42758 ) ),
 .UNSPECIFIED., .F., .F., .F.,
 ( 6, 6 ),
 ( 6, 3, 6 ),
 ( 25.26539769200000052, 42.22154018949999710 ),
 ( 0.000000000000000000, 1.000000000000000000, 2.000000000000000000 ),
 .UNSPECIFIED. ) ;
#93005 = CARTESIAN_POINT ( 'NONE',  ( -35.51625343300000281, 1423.702337785729924, 261.8360441569980139 ) ) ;
#93006 = DIRECTION ( 'NONE',  ( 2.479303797136877383E-05, 0.02617627755937491918, -0.9996573422320469415 ) ) ;
#93007 = CARTESIAN_POINT ( 'NONE',  ( 17.08853468078067550, 1460.333142299152769, 228.6834606794553792 ) ) ;
#93008 = CONTEXT_DEPENDENT_SHAPE_REPRESENTATION ( #37751, #99197 ) ;
#93009 = DIRECTION ( 'NONE',  ( -0.1070030146457386366, 0.000000000000000000, -0.9942586961433749204 ) ) ;
#93010 = CARTESIAN_POINT ( 'NONE',  ( -36.07989623025710557, 1437.464731524360104, 136.5385958873009997 ) ) ;
#93011 = ORIENTED_EDGE ( 'NONE', *, *, #15964, .T. ) ;
#93012 = CARTESIAN_POINT ( 'NONE',  ( 9.738311102098309746, 1493.400122879349965, 188.2659922716460130 ) ) ;
#93013 = CIRCLE ( 'NONE', #101956, 2.000000000000001776 ) ;
#93014 = CARTESIAN_POINT ( 'NONE',  ( -18.92249268369999982, 1456.941604937630018, 229.2980728310979828 ) ) ;
#93015 = ORIENTED_EDGE ( 'NONE', *, *, #46890, .F. ) ;
#93016 = ORIENTED_EDGE ( 'NONE', *, *, #61940, .T. ) ;
#93017 = CARTESIAN_POINT ( 'NONE',  ( 4.464391958920000292, 1426.554722128930052, 191.5974441596989948 ) ) ;
#93018 = CARTESIAN_POINT ( 'NONE',  ( 10.45954636811110028, 1453.050608579339951, 210.8472557228290043 ) ) ;
#93019 = CARTESIAN_POINT ( 'NONE',  ( -14.17425181905940157, 1380.106801343270035, 210.9147591587110071 ) ) ;
#93020 = CARTESIAN_POINT ( 'NONE',  ( -15.31153093854189962, 1508.451225488540103, 209.8004562725960227 ) ) ;
#93021 = CIRCLE ( 'NONE', #60932, 11.73460161499999899 ) ;
#93022 = CYLINDRICAL_SURFACE ( 'NONE', #4920, 1.000000000000000888 ) ;
#93023 = CARTESIAN_POINT ( 'NONE',  ( -5.529153398355120430, 1454.733540159410040, 201.5061756946240052 ) ) ;
#93024 = CARTESIAN_POINT ( 'NONE',  ( 38.81202645930000017, 1450.612734574179967, 134.0999998922980012 ) ) ;
#93025 = CARTESIAN_POINT ( 'NONE',  ( 0.2572000660973332575, 1516.857224341794563, 216.6260235208673635 ) ) ;
#93026 = CARTESIAN_POINT ( 'NONE',  ( -9.849896899200842881, 1512.913060387330006, 185.5490084180013923 ) ) ;
#93027 = CARTESIAN_POINT ( 'NONE',  ( 17.22592475669953416, 1443.913060387330688, 162.9227486557969655 ) ) ;
#93028 = B_SPLINE_CURVE_WITH_KNOTS ( 'NONE', 5,
 ( #78965, #3783, #8972, #52102, #44252, #95193 ),
 .UNSPECIFIED., .F., .F.,
 ( 6, 6 ),
 ( 239.4206172199999969, 244.3064142099999856 ),
 .UNSPECIFIED. ) ;
#93029 = CARTESIAN_POINT ( 'NONE',  ( -103.4471835965699995, 1384.884903909179911, 296.7663910193570587 ) ) ;
#93030 = ORIENTED_EDGE ( 'NONE', *, *, #61058, .T. ) ;
#93031 = CARTESIAN_POINT ( 'NONE',  ( 4.034908559714999399, 1517.068717944079935, 201.7859449365070077 ) ) ;
#93032 = CARTESIAN_POINT ( 'NONE',  ( 6.562094069294999166, 1517.122674412569950, 209.8604508749069737 ) ) ;
#93033 = EDGE_LOOP ( 'NONE', ( #8254, #41273, #6552, #5298 ) ) ;
#93034 = CARTESIAN_POINT ( 'NONE',  ( 10.79382126600000014, 1414.913060387329779, 222.1041115775979904 ) ) ;
#93035 = CARTESIAN_POINT ( 'NONE',  ( 3.547742475963274966, 1511.610050756757573, 217.1750692285095568 ) ) ;
#93036 = ORIENTED_EDGE ( 'NONE', *, *, #74475, .T. ) ;
#93037 = CARTESIAN_POINT ( 'NONE',  ( -13.47470376080000065, 1415.128105756529976, 220.8293656388979969 ) ) ;
#93038 = CARTESIAN_POINT ( 'NONE',  ( 5.610572505957840406, 1429.830968158320047, 216.7704346018900310 ) ) ;
#93039 = CARTESIAN_POINT ( 'NONE',  ( 20.70484064406403846, 1525.907212628473644, 233.2025904124105580 ) ) ;
#93040 = CARTESIAN_POINT ( 'NONE',  ( -9.833554420730120427, 1461.675800432549977, 208.3780452630800255 ) ) ;
#93041 = LINE ( 'NONE', #48317, #29680 ) ;
#93042 = CARTESIAN_POINT ( 'NONE',  ( 11.13973213087689906, 1470.272412021129867, 206.9146623043149873 ) ) ;
#93044 = B_SPLINE_CURVE_WITH_KNOTS ( 'NONE', 3,
 ( #73431, #5101, #20789, #55533, #47125, #81252, #21327, #7720, #56071, #54989 ),
 .UNSPECIFIED., .F., .F.,
 ( 4, 3, 3, 4 ),
 ( -157.4228417709999803, -134.4932994732330087, -78.88177757080619301, -29.50720979954130030 ),
 .UNSPECIFIED. ) ;
#93043 = LINE ( 'NONE', #32604, #60306 ) ;
#93045 = CARTESIAN_POINT ( 'NONE',  ( -14.97640067789438056, 1410.808495669646845, 190.7346035218114082 ) ) ;
#93046 = CARTESIAN_POINT ( 'NONE',  ( -54.25698729759999850, 1379.746222734200046, 249.0120014888590276 ) ) ;
#93047 = CARTESIAN_POINT ( 'NONE',  ( 24.49219634299049986, 1454.783420082590055, 206.2155678165669883 ) ) ;
#93049 = CARTESIAN_POINT ( 'NONE',  ( 7.978761767491338475, 1468.077760772049942, 201.2729507454290001 ) ) ;
#93048 = CARTESIAN_POINT ( 'NONE',  ( -20.69294079850000045, 1505.646924528690079, 209.1300474139309813 ) ) ;
#93050 = FACE_OUTER_BOUND ( 'NONE', #55270, .T. ) ;
#93051 = B_SPLINE_SURFACE_WITH_KNOTS ( 'NONE', 5, 1, ( 
 ( #4494, #83381 ),
 ( #6682, #38626 ),
 ( #13965, #40835 ),
 ( #75012, #64957 ),
 ( #5025, #98532 ),
 ( #63861, #97975 ) ),
 .UNSPECIFIED., .F., .F., .F.,
 ( 6, 6 ),
 ( 2, 2 ),
 ( 0.000000000000000000, 3.962517353580000012 ),
 ( 0.000000000000000000, 14.00000000000000000 ),
 .UNSPECIFIED. ) ;
#93052 = CARTESIAN_POINT ( 'NONE',  ( -0.7396922758749979732, 1517.135701590510052, 216.4591432822169850 ) ) ;
#93053 = ORIENTED_EDGE ( 'NONE', *, *, #64711, .T. ) ;
#93054 = CARTESIAN_POINT ( 'NONE',  ( 17.17241001986506888, 1512.187213306747481, 238.6251415217915337 ) ) ;
#93055 = CARTESIAN_POINT ( 'NONE',  ( -21.64969004980934741, 1524.547873515822630, 234.6921391611746230 ) ) ;
#93056 = CARTESIAN_POINT ( 'NONE',  ( 3.458526497885000328, 1516.742629295279812, 214.1194197574270106 ) ) ;
#93057 = CARTESIAN_POINT ( 'NONE',  ( 5.662343758720000508, 1504.894618425089902, 220.5557215505990314 ) ) ;
#93058 = CARTESIAN_POINT ( 'NONE',  ( -11.60004869885203682, 1425.894669204696356, 137.5118601392097730 ) ) ;
#93060 = ORIENTED_EDGE ( 'NONE', *, *, #82851, .F. ) ;
#93059 = CARTESIAN_POINT ( 'NONE',  ( -11.44574129031820142, 1500.980493451109851, 211.1514305463080063 ) ) ;
#93061 = CARTESIAN_POINT ( 'NONE',  ( -8.604576478229999381, 1384.925130841180135, 199.8686410051190023 ) ) ;
#93062 = AXIS2_PLACEMENT_3D ( 'NONE', #44772, #20621, #88948 ) ;
#93063 = DIRECTION ( 'NONE',  ( 5.980589973904019347E-17, -1.000000000000000000, 1.736889445713099699E-16 ) ) ;
#93064 = CARTESIAN_POINT ( 'NONE',  ( -11.73709484269999948, 1429.894488352029839, 150.3345969089980088 ) ) ;
#93065 = CARTESIAN_POINT ( 'NONE',  ( 19.15249185863720172, 1456.934575639789955, 224.9730113979510122 ) ) ;
#93066 = CARTESIAN_POINT ( 'NONE',  ( -11.00907965078549999, 1462.196140238690077, 209.7526447668389835 ) ) ;
#93067 = CARTESIAN_POINT ( 'NONE',  ( -2.298816259811510054, 1486.462377102800019, 220.8289805423670202 ) ) ;
#93068 = FACE_OUTER_BOUND ( 'NONE', #31246, .T. ) ;
#93069 = CARTESIAN_POINT ( 'NONE',  ( 0.2612772751870610088, 1416.851343895820037, 190.7759414009450154 ) ) ;
#93071 = CARTESIAN_POINT ( 'NONE',  ( -10.65742070623289983, 1481.357802822280064, 207.9456758233610287 ) ) ;
#93070 = CARTESIAN_POINT ( 'NONE',  ( -22.07223515240000111, 1495.368308318629943, 224.9714801519980085 ) ) ;
#93072 = CARTESIAN_POINT ( 'NONE',  ( -17.15288881900699991, 1460.895685894954113, 228.2717695460779908 ) ) ;
#93073 = ORIENTED_EDGE ( 'NONE', *, *, #62468, .T. ) ;
#93074 = CARTESIAN_POINT ( 'NONE',  ( 2.477986732234999767, 1516.922519270759949, 205.8529865360470126 ) ) ;
#93075 = CARTESIAN_POINT ( 'NONE',  ( 21.97873717970000129, 1409.919016783729830, 268.2775909820980473 ) ) ;
#93076 = CARTESIAN_POINT ( 'NONE',  ( -32.38114538885245253, 1523.604703353109699, 216.1203639561433363 ) ) ;
#93077 = CARTESIAN_POINT ( 'NONE',  ( 18.62522279299999894, 1430.306151902329930, 192.9288626887980058 ) ) ;
#93078 = ADVANCED_FACE ( 'NONE', ( #39967 ), #62172, .F. ) ;
#93079 = CARTESIAN_POINT ( 'NONE',  ( -0.3859486939953010176, 1508.980285656380147, 238.8607942401669959 ) ) ;
#93080 = ADVANCED_FACE ( 'NONE', ( #58435 ), #12642, .T. ) ;
#93081 = CARTESIAN_POINT ( 'NONE',  ( 4.319855718986739923, 1453.935607868970010, 217.4425725348959872 ) ) ;
#93082 = CARTESIAN_POINT ( 'NONE',  ( -1.695277381189999932, 1451.989423603729847, 184.1238975007979946 ) ) ;
#93083 = VECTOR ( 'NONE', #16723, 999.9999999999998863 ) ;
#93084 = CARTESIAN_POINT ( 'NONE',  ( -15.52522232080000109, 1416.123895944519973, 207.8294199178490089 ) ) ;
#93085 = CARTESIAN_POINT ( 'NONE',  ( -13.55686268810000072, 1443.939294377719989, 187.3937464511979840 ) ) ;
#93086 = ADVANCED_FACE ( 'NONE', ( #65737 ), #41629, .F. ) ;
#93087 = CARTESIAN_POINT ( 'NONE',  ( 18.89905511659999959, 1416.828040475729949, 210.6687957193779823 ) ) ;
#93088 = EDGE_CURVE ( 'NONE', #84204, #53816, #23707, .T. ) ;
#93089 = CARTESIAN_POINT ( 'NONE',  ( -5.215695451837711438, 1495.379824343749760, 198.7908095108026885 ) ) ;
#93090 = CARTESIAN_POINT ( 'NONE',  ( 43.83783108890263946, 1431.613812174279474, 269.7043230926977344 ) ) ;
#93091 = CARTESIAN_POINT ( 'NONE',  ( 1.465471608279500071, 1490.706886906569935, 181.8288697470349859 ) ) ;
#93092 = CARTESIAN_POINT ( 'NONE',  ( -18.67614678860000055, 1441.800567318090089, 210.9159933499589954 ) ) ;
#93093 = CARTESIAN_POINT ( 'NONE',  ( 10.50817522199910137, 1481.942267134329995, 210.4830409274069893 ) ) ;
#93094 = CARTESIAN_POINT ( 'NONE',  ( 32.66476241579317730, 1526.382868172863937, 219.1158660759119243 ) ) ;
#93095 = CARTESIAN_POINT ( 'NONE',  ( -9.814534880020000074, 1474.572486408329951, 269.4661027754979727 ) ) ;
#93096 = CARTESIAN_POINT ( 'NONE',  ( -30.38265071699166953, 1524.478200376968516, 196.4017061176955963 ) ) ;
#93097 = CARTESIAN_POINT ( 'NONE',  ( -12.27558643317981790, 1391.355947415424453, 211.6931146922721894 ) ) ;
#93098 = CARTESIAN_POINT ( 'NONE',  ( -24.15580053757905787, 1444.499259447567738, 211.6244612293730825 ) ) ;
#93099 = CARTESIAN_POINT ( 'NONE',  ( -56.29574522006849691, 1384.711066908519797, 274.2995360668660396 ) ) ;
#93100 = CARTESIAN_POINT ( 'NONE',  ( -9.457584820017499894, 1462.148799351590014, 206.2711904065230044 ) ) ;
#93101 = AXIS2_PLACEMENT_3D ( 'NONE', #1193, #1751, #26361 ) ;
#93102 = CARTESIAN_POINT ( 'NONE',  ( 11.66418951319000108, 1415.301705644340018, 222.9857275129059815 ) ) ;
#93103 = CYLINDRICAL_SURFACE ( 'NONE', #62474, 2.499999999999989786 ) ;
#93104 = CARTESIAN_POINT ( 'NONE',  ( -16.64685983873495445, 1523.847233649538339, 237.7436688609939779 ) ) ;
#93105 = DIRECTION ( 'NONE',  ( -5.168774739196950157E-16, 1.261506706387156225E-22, 1.000000000000000000 ) ) ;
#93106 = CARTESIAN_POINT ( 'NONE',  ( -22.20360156850000166, 1409.688427239630073, 206.9744876511380198 ) ) ;
#93107 = ADVANCED_FACE ( 'NONE', ( #104294 ), #9128, .F. ) ;
#93108 = CARTESIAN_POINT ( 'NONE',  ( -10.46358859826853838, 1379.681001781858413, 202.5371937123522912 ) ) ;
#93109 = CARTESIAN_POINT ( 'NONE',  ( 3.347839154809999940, 1485.651791778389907, 219.4796426812989978 ) ) ;
#93110 = CARTESIAN_POINT ( 'NONE',  ( 13.16517659032116860, 1522.051704408389924, 194.0489770726361485 ) ) ;
#93111 = CARTESIAN_POINT ( 'NONE',  ( 2.482344662330000062, 1440.444625599219989, 150.5580151863979950 ) ) ;
#93112 = CARTESIAN_POINT ( 'NONE',  ( -19.86670360899999821, 1443.974114956090034, 213.2631289620589712 ) ) ;
#93114 = EDGE_CURVE ( 'NONE', #53131, #77321, #86934, .T. ) ;
#93113 = CARTESIAN_POINT ( 'NONE',  ( -6.141397734697970456, 1509.034509440879901, 216.6345626749620124 ) ) ;
#93115 = CARTESIAN_POINT ( 'NONE',  ( -34.33069563939339730, 1442.322945709279793, 137.1732133424210360 ) ) ;
#93118 = CARTESIAN_POINT ( 'NONE',  ( -3.665756888430000249, 1509.038615934189920, 204.6345961887290059 ) ) ;
#93117 = AXIS2_PLACEMENT_3D ( 'NONE', #52354, #9766, #35521 ) ;
#93116 = CARTESIAN_POINT ( 'NONE',  ( -16.58369734668589501, 1417.133262957369880, 208.4557275984209923 ) ) ;
#93119 = CARTESIAN_POINT ( 'NONE',  ( -5.292247061280000331, 1391.913060387289988, 203.8075142969990168 ) ) ;
#93120 = CARTESIAN_POINT ( 'NONE',  ( 17.03783583027156823, 1524.776010967676029, 237.1517449984523864 ) ) ;
#93121 = CARTESIAN_POINT ( 'NONE',  ( 15.73570983720359884, 1409.462563483369877, 192.9527024472970140 ) ) ;
#93122 = EDGE_CURVE ( 'NONE', #37425, #90721, #60659, .T. ) ;
#93123 = CARTESIAN_POINT ( 'NONE',  ( 10.09177798305169915, 1451.176487112019913, 206.2838416248820010 ) ) ;
#93124 = CARTESIAN_POINT ( 'NONE',  ( 1.299941910205479889, 1406.964220106440052, 222.1218459604740190 ) ) ;
#93125 = AXIS2_PLACEMENT_3D ( 'NONE', #54270, #44199, #104641 ) ;
#93126 = CARTESIAN_POINT ( 'NONE',  ( 2.289624432225000117, 1517.154223579619838, 202.5582500624169882 ) ) ;
#93127 = DIRECTION ( 'NONE',  ( -0.6736849260863839728, 0.000000000000000000, 0.7390186874254150995 ) ) ;
#93128 = CARTESIAN_POINT ( 'NONE',  ( -11.17497852669747793, 1398.244341017566740, 202.4708927046083886 ) ) ;
#93129 = CARTESIAN_POINT ( 'NONE',  ( 16.01627747153500181, 1512.526319173689899, 195.5274977073669902 ) ) ;
#93130 = FACE_BOUND ( 'NONE', #34920, .T. ) ;
#93131 = CARTESIAN_POINT ( 'NONE',  ( 7.886150497493308481E-14, 1379.061224848670008, 211.6703178456000103 ) ) ;
#93132 = CARTESIAN_POINT ( 'NONE',  ( 20.77675428743160069, 1508.900241235260182, 228.2412293500289877 ) ) ;
#93134 = ORIENTED_EDGE ( 'NONE', *, *, #49297, .T. ) ;
#93133 = CARTESIAN_POINT ( 'NONE',  ( -48.10662876290690093, 1379.692216664059970, 241.4897638297360061 ) ) ;
#93135 = ORIENTED_EDGE ( 'NONE', *, *, #67838, .T. ) ;
#93136 = CARTESIAN_POINT ( 'NONE',  ( 11.33665491360190103, 1434.299677755099992, 151.5166025912550083 ) ) ;
#93137 = CARTESIAN_POINT ( 'NONE',  ( -10.98878578539999928, 1396.296797242730008, 211.1406780321979966 ) ) ;
#93138 = VERTEX_POINT ( 'NONE', #94783 ) ;
#93139 = CARTESIAN_POINT ( 'NONE',  ( -107.3950653609999932, 1379.272371631200031, 309.0941593425589531 ) ) ;
#93140 = CARTESIAN_POINT ( 'NONE',  ( -109.6575144470000112, 1384.919424601119999, 311.3230338722590318 ) ) ;
#93141 = CARTESIAN_POINT ( 'NONE',  ( 4.325403553351909736, 1515.219291385429869, 206.7919471176340096 ) ) ;
#93143 = CARTESIAN_POINT ( 'NONE',  ( -13.99352145463339880, 1509.057321564920130, 183.6517433629080074 ) ) ;
#93142 = CARTESIAN_POINT ( 'NONE',  ( 1.381522864419999941, 1444.570505314090042, 200.1133580050590126 ) ) ;
#93144 = CARTESIAN_POINT ( 'NONE',  ( 19.52954207340370019, 1507.817373360699776, 229.4580641922199788 ) ) ;
#93145 = AXIS2_PLACEMENT_3D ( 'NONE', #1956, #20366, #97644 ) ;
#93146 = CARTESIAN_POINT ( 'NONE',  ( 2.177068321099999704, 1449.238783986130102, 183.7865808134980057 ) ) ;
#93147 = CARTESIAN_POINT ( 'NONE',  ( 2.309941155180000205, 1466.993925648989944, 219.5497868284989806 ) ) ;
#93148 = LINE ( 'NONE', #74171, #98371 ) ;
#93149 = CARTESIAN_POINT ( 'NONE',  ( 10.93008446023089952, 1479.841554277730211, 208.5739487062600119 ) ) ;
#93150 = CARTESIAN_POINT ( 'NONE',  ( 1.455250893800000167, 1415.140114704729967, 191.2687284723980099 ) ) ;
#93151 = CARTESIAN_POINT ( 'NONE',  ( 11.30046002139999928, 1432.242744379899932, 151.5215588119980339 ) ) ;
#93152 = CARTESIAN_POINT ( 'NONE',  ( 6.402238466425000496, 1513.914017980340077, 201.5343560373169964 ) ) ;
#93153 = ORIENTED_EDGE ( 'NONE', *, *, #27349, .T. ) ;
#93154 = CARTESIAN_POINT ( 'NONE',  ( 13.27755285367060090, 1435.679892222259923, 150.4537440835390214 ) ) ;
#93155 = ORIENTED_EDGE ( 'NONE', *, *, #89048, .T. ) ;
#93156 = ORIENTED_EDGE ( 'NONE', *, *, #4212, .T. ) ;
#93157 = CARTESIAN_POINT ( 'NONE',  ( 13.50124191877204716, 1444.098444817566815, 169.3544818395477591 ) ) ;
#93158 = CARTESIAN_POINT ( 'NONE',  ( -5.054744702799999878, 1466.411211125930095, 234.4407030224980133 ) ) ;
#93159 = CARTESIAN_POINT ( 'NONE',  ( 6.942344691835000248, 1516.810037859429940, 216.8380980232070101 ) ) ;
#93160 = DIRECTION ( 'NONE',  ( 0.000000000000000000, 1.000000000000000000, 0.000000000000000000 ) ) ;
#93161 = PRODUCT_DEFINITION ( 'UNKNOWN', '', #51243, #51345 ) ;
#93162 = CARTESIAN_POINT ( 'NONE',  ( 11.19148376978288439, 1422.145534526647452, 210.4506217739875353 ) ) ;
#93163 = CARTESIAN_POINT ( 'NONE',  ( 2.500000000000000000, 1448.322079714279880, 163.7894488454339808 ) ) ;
#93164 = DIRECTION ( 'NONE',  ( 1.000000000000000000, 0.000000000000000000, 0.000000000000000000 ) ) ;
#93165 = ORIENTED_EDGE ( 'NONE', *, *, #45955, .F. ) ;
#93166 = CARTESIAN_POINT ( 'NONE',  ( -0.7576635715699989726, 1516.855632454399938, 206.2537338009369989 ) ) ;
#93167 = ORIENTED_EDGE ( 'NONE', *, *, #20027, .F. ) ;
#93168 = CARTESIAN_POINT ( 'NONE',  ( -104.4846036076890101, 1379.706327206979950, 304.5108243419020368 ) ) ;
#93169 = CARTESIAN_POINT ( 'NONE',  ( -18.84890028649999749, 1508.241238781830134, 229.7780645497980174 ) ) ;
#93170 = CARTESIAN_POINT ( 'NONE',  ( -12.98830284870000185, 1410.299474438730158, 189.7180828017980048 ) ) ;
#93171 = CARTESIAN_POINT ( 'NONE',  ( 8.041028920664999191, 1514.881364185380107, 215.2179418010969982 ) ) ;
#93173 = ORIENTED_EDGE ( 'NONE', *, *, #63454, .F. ) ;
#93172 = DIRECTION ( 'NONE',  ( -1.913759484722300243E-19, 1.000000000000000000, -1.836968204960139822E-16 ) ) ;
#93174 = CARTESIAN_POINT ( 'NONE',  ( 19.78185562140000187, 1426.701755847230061, 221.7132604633979724 ) ) ;
#93175 = CARTESIAN_POINT ( 'NONE',  ( 3.657829568870575976, 1442.827323799996748, 217.2295476630547171 ) ) ;
#93176 = CARTESIAN_POINT ( 'NONE',  ( -113.4000000000000057, 1383.754957750760013, 311.0314894602589675 ) ) ;
#93178 = EDGE_CURVE ( 'NONE', #58183, #88502, #26954, .T. ) ;
#93177 = CARTESIAN_POINT ( 'NONE',  ( 7.892605823620001182, 1452.443926081389918, 214.1248619204189936 ) ) ;
#93179 = CARTESIAN_POINT ( 'NONE',  ( 22.66254714602377973, 1523.342713519622293, 181.4291743802665735 ) ) ;
#93180 = EDGE_CURVE ( 'NONE', #44004, #18098, #33759, .T. ) ;
#93182 = CARTESIAN_POINT ( 'NONE',  ( 7.334957356574999920, 1517.030858226499959, 213.7381182667970165 ) ) ;
#93181 =( GEOMETRIC_REPRESENTATION_CONTEXT ( 3 ) GLOBAL_UNCERTAINTY_ASSIGNED_CONTEXT ( ( #84931 ) ) GLOBAL_UNIT_ASSIGNED_CONTEXT ( ( #81981, #13658, #108850 ) ) REPRESENTATION_CONTEXT ( 'NONE', 'WORKASPACE' ) );
#93183 = CARTESIAN_POINT ( 'NONE',  ( -3.132119737639480483, 1428.847266505159951, 200.2946123499760063 ) ) ;
#93184 = CARTESIAN_POINT ( 'NONE',  ( 23.54053215893118534, 1409.992431867414780, 209.4961292702789422 ) ) ;
#93185 = FACE_OUTER_BOUND ( 'NONE', #16078, .T. ) ;
#93186 = CARTESIAN_POINT ( 'NONE',  ( 6.950833530105000158, 1517.156142772249950, 211.6057959108269984 ) ) ;
#93187 = CARTESIAN_POINT ( 'NONE',  ( 39.47393889809999479, 1426.323565199129916, 271.1218459616979999 ) ) ;
#93188 = CARTESIAN_POINT ( 'NONE',  ( 13.79686514299999978, 1409.394857534729908, 192.7614752862980083 ) ) ;
#93189 = AXIS2_PLACEMENT_3D ( 'NONE', #18123, #52319, #86443 ) ;
#93190 = CARTESIAN_POINT ( 'NONE',  ( -11.14267526204083403, 1486.018413702905264, 184.3103354489751382 ) ) ;
#93192 = ORIENTED_EDGE ( 'NONE', *, *, #67340, .F. ) ;
#93191 = CARTESIAN_POINT ( 'NONE',  ( -53.47023167649999920, 1385.031515079650262, 230.7490043923590122 ) ) ;
#93193 = CARTESIAN_POINT ( 'NONE',  ( -63.30007382191959664, 1385.050657975149988, 286.2646782049000080 ) ) ;
#93194 = EDGE_CURVE ( 'NONE', #45310, #36236, #69755, .T. ) ;
#93195 = CARTESIAN_POINT ( 'NONE',  ( 15.89627787829999939, 1466.157227575730076, 250.4785789420980109 ) ) ;
#93196 = CARTESIAN_POINT ( 'NONE',  ( -32.02808312589930040, 1512.187213306747481, 198.2787714533499752 ) ) ;
#93197 = CARTESIAN_POINT ( 'NONE',  ( -16.68599179859999992, 1461.161699058329987, 228.2799821568980008 ) ) ;
#93198 = CARTESIAN_POINT ( 'NONE',  ( 11.27257476199999964, 1426.317358070279852, 206.4672093773990014 ) ) ;
#93199 = CARTESIAN_POINT ( 'NONE',  ( 1.354493917142649995, 1452.777995751539947, 183.4488450902570094 ) ) ;
#93200 = AXIS2_PLACEMENT_3D ( 'NONE', #85495, #7160, #8794 ) ;
#93202 = DIRECTION ( 'NONE',  ( -0.4978433412588781914, 0.000000000000000000, -0.8672669759446606230 ) ) ;
#93201 = DIRECTION ( 'NONE',  ( 0.000000000000000000, 0.000000000000000000, -1.000000000000000000 ) ) ;
#93203 = PLANE ( 'NONE',  #29961 ) ;
#93204 = CARTESIAN_POINT ( 'NONE',  ( -107.4633657559999875, 1380.084902923649906, 309.4123343822590186 ) ) ;
#93205 = ORIENTED_EDGE ( 'NONE', *, *, #73249, .F. ) ;
#93206 = CARTESIAN_POINT ( 'NONE',  ( 0.7386049046750020608, 1517.122674412569950, 202.5597518628069906 ) ) ;
#93207 = EDGE_CURVE ( 'NONE', #21199, #58053, #91539, .T. ) ;
#93208 = CARTESIAN_POINT ( 'NONE',  ( 14.13195592840999915, 1452.421092199690065, 222.7290593210850034 ) ) ;
#93209 = EDGE_CURVE ( 'NONE', #13899, #38713, #89526, .T. ) ;
#93210 = CARTESIAN_POINT ( 'NONE',  ( 13.06198372480000103, 1425.733590216230141, 223.1966135260979911 ) ) ;
#93211 = CARTESIAN_POINT ( 'NONE',  ( -33.72300830903702717, 1524.397344074318198, 219.5868698111212609 ) ) ;
#93212 = FACE_OUTER_BOUND ( 'NONE', #62167, .T. ) ;
#93213 =( BOUNDED_SURFACE ( )  B_SPLINE_SURFACE ( 3, 2, ( 
 ( #56082, #89126, #81261 ),
 ( #41347, #11876, #65036 ),
 ( #47682, #63954, #12413 ),
 ( #13491, #81810, #5112 ),
 ( #39268, #97529, #92285 ),
 ( #63414, #88593, #98068 ) ),
 .UNSPECIFIED., .F., .F., .F. ) 
 B_SPLINE_SURFACE_WITH_KNOTS ( ( 4, 2, 4 ),
 ( 3, 3 ),
 ( -5.139118297581291017E-17, 0.001312027981647291563, 0.002624055963294634301 ),
 ( 0.000000000000000000, 1.000000000000000000 ),
 .UNSPECIFIED. ) 
 GEOMETRIC_REPRESENTATION_ITEM ( )  RATIONAL_B_SPLINE_SURFACE ( (
 ( 1.000000000000000000, 0.9376006582765908925, 1.000000000000000000),
 ( 1.000000000000000000, 0.9569320108021285298, 1.000000000000000000),
 ( 1.000000000000000000, 0.9725743441620615659, 1.000000000000000000),
 ( 1.000000000000000000, 0.9942095667133905579, 1.000000000000000000),
 ( 1.000000000000000000, 1.000043666450838531, 1.000000000000000000),
 ( 1.000000000000000000, 1.000000000000000000, 1.000000000000000000) ) ) 
 REPRESENTATION_ITEM ( '' )  SURFACE ( )  );
#93214 = CARTESIAN_POINT ( 'NONE',  ( 27.01381218759999925, 1450.681579806120226, 136.4483250053980044 ) ) ;
#93215 = CARTESIAN_POINT ( 'NONE',  ( 4.276238399013360336, 1416.103362730192430, 231.6875764602628465 ) ) ;
#93216 = EDGE_CURVE ( 'NONE', #59183, #75973, #94890, .T. ) ;
#93217 = CIRCLE ( 'NONE', #34237, 7.300000000000009592 ) ;
#93218 = CARTESIAN_POINT ( 'NONE',  ( 30.86937158395179992, 1435.735953314200060, 136.0385399056279994 ) ) ;
#93219 = CARTESIAN_POINT ( 'NONE',  ( 39.15545969614949229, 1447.513155944669961, 136.5656658507510031 ) ) ;
#93220 = CARTESIAN_POINT ( 'NONE',  ( 2.531940903048510086E-08, 1457.850589566970029, 229.0733431205499926 ) ) ;
#93221 = CARTESIAN_POINT ( 'NONE',  ( -109.9909981520000031, 1385.946039747419945, 297.0141037326589526 ) ) ;
#93222 = CARTESIAN_POINT ( 'NONE',  ( 10.18862200870000123, 1507.986924515629880, 183.7493071292980176 ) ) ;
#93223 = CARTESIAN_POINT ( 'NONE',  ( 19.98413504154914122, 1526.143142182216479, 184.9530087056776040 ) ) ;
#93224 = AXIS2_PLACEMENT_3D ( 'NONE', #68597, #77540, #103256 ) ;
#93225 = LINE ( 'NONE', #42836, #77893 ) ;
#93226 = ORIENTED_EDGE ( 'NONE', *, *, #83473, .T. ) ;
#93227 = CARTESIAN_POINT ( 'NONE',  ( -9.096590249497090497, 1440.282600144749949, 206.1070276416620004 ) ) ;
#93228 = DIRECTION ( 'NONE',  ( -0.6736849260863839728, 0.000000000000000000, 0.7390186874254150995 ) ) ;
#93229 = EDGE_CURVE ( 'NONE', #92455, #3293, #64384, .T. ) ;
#93230 = FACE_OUTER_BOUND ( 'NONE', #105415, .T. ) ;
#93231 = FACE_OUTER_BOUND ( 'NONE', #56166, .T. ) ;
#93232 = CARTESIAN_POINT ( 'NONE',  ( 11.27587417618524057, 1425.429644209827529, 138.6751927835265121 ) ) ;
#93233 = CARTESIAN_POINT ( 'NONE',  ( 11.60235767850000066, 1501.497651028989821, 209.0874959428689976 ) ) ;
#93234 = CARTESIAN_POINT ( 'NONE',  ( -12.53380652166779896, 1445.052232296300190, 185.6742736269380032 ) ) ;
#93235 = CARTESIAN_POINT ( 'NONE',  ( -9.471890498288960458, 1438.598768578280215, 210.0041281920070162 ) ) ;
#93236 = CARTESIAN_POINT ( 'NONE',  ( 1.792279166353169861, 1494.398886770019999, 220.1169078828669967 ) ) ;
#93237 = AXIS2_PLACEMENT_3D ( 'NONE', #46171, #80300, #35527 ) ;
#93238 = ADVANCED_FACE ( 'NONE', ( #25903 ), #57584, .T. ) ;
#93239 = CARTESIAN_POINT ( 'NONE',  ( 44.70563250888439910, 1440.913044414219939, 269.9105896417649433 ) ) ;
#93240 = CARTESIAN_POINT ( 'NONE',  ( -20.21907573023804261, 1450.974930438806950, 145.3432850838296133 ) ) ;
#93241 = CARTESIAN_POINT ( 'NONE',  ( 25.85268144089999964, 1436.351425001499820, 136.9215235935979820 ) ) ;
#93242 = CARTESIAN_POINT ( 'NONE',  ( -13.10805326783636282, 1443.031241081782355, 169.4048015275553780 ) ) ;
#93243 = ORIENTED_EDGE ( 'NONE', *, *, #86399, .T. ) ;
#93244 = FACE_OUTER_BOUND ( 'NONE', #15729, .T. ) ;
#93245 = CARTESIAN_POINT ( 'NONE',  ( 21.44621485940070471, 1509.083181763402308, 226.4317593619785782 ) ) ;
#93246 = EDGE_LOOP ( 'NONE', ( #60955, #104857, #63999, #100627, #47165 ) ) ;
#93247 = ORIENTED_EDGE ( 'NONE', *, *, #75427, .F. ) ;
#93248 = CARTESIAN_POINT ( 'NONE',  ( -12.48995958879999968, 1501.883328876989935, 211.6213070136890053 ) ) ;
#93250 = EDGE_CURVE ( 'NONE', #22625, #93667, #61836, .T. ) ;
#93249 = CARTESIAN_POINT ( 'NONE',  ( 7.136265425265223783, 1516.548173715040548, 206.8118382600278267 ) ) ;
#93252 = CARTESIAN_POINT ( 'NONE',  ( -20.43149705680000139, 1451.305676987330116, 211.9821049860279913 ) ) ;
#93251 = CARTESIAN_POINT ( 'NONE',  ( 2.550590696230000010, 1455.409333296890054, 218.3516928308589797 ) ) ;
#93253 = CARTESIAN_POINT ( 'NONE',  ( -8.587559811879998506, 1448.168510073290008, 212.1995923204489998 ) ) ;
#93254 = EDGE_CURVE ( 'NONE', #32804, #1550, #18222, .T. ) ;
#93255 = CARTESIAN_POINT ( 'NONE',  ( -11.25211100100000117, 1433.083168801150123, 151.5369127784980208 ) ) ;
#93256 = CARTESIAN_POINT ( 'NONE',  ( -21.83550407203936672, 1523.678648413191695, 183.2743720722710634 ) ) ;
#93257 = CARTESIAN_POINT ( 'NONE',  ( -2.887076735410655015, 1419.617858305948175, 186.1929011117634900 ) ) ;
#93258 = CARTESIAN_POINT ( 'NONE',  ( -2.425477467416652377, 1523.390106123591067, 243.0915840373788228 ) ) ;
#93259 = CARTESIAN_POINT ( 'NONE',  ( -24.48419039099999850, 1440.340129069209979, 210.9825192850280189 ) ) ;
#93260 = FACE_BOUND ( 'NONE', #12830, .T. ) ;
#93261 = CARTESIAN_POINT ( 'NONE',  ( 2.874932676220000261, 1451.924210125230047, 183.8349795613980007 ) ) ;
#93262 = EDGE_CURVE ( 'NONE', #53103, #26024, #97547, .T. ) ;
#93263 = CARTESIAN_POINT ( 'NONE',  ( 8.035765206089191537, 1364.685966892704982, 208.3718459617061285 ) ) ;
#93264 = CARTESIAN_POINT ( 'NONE',  ( -29.03599522121404419, 1510.037923944993963, 216.6658193178216436 ) ) ;
#93266 = ORIENTED_EDGE ( 'NONE', *, *, #71459, .F. ) ;
#93265 = CARTESIAN_POINT ( 'NONE',  ( 4.709066435679999607, 1495.147136540189877, 220.5787752062990137 ) ) ;
#93267 = ORIENTED_EDGE ( 'NONE', *, *, #42522, .T. ) ;
#93268 = CARTESIAN_POINT ( 'NONE',  ( -2.178514691999632991, 1508.356099863727650, 220.7675093205359360 ) ) ;
#93269 = CARTESIAN_POINT ( 'NONE',  ( -19.88572122277579979, 1484.728771715989751, 191.0592865161910083 ) ) ;
#93270 = CARTESIAN_POINT ( 'NONE',  ( -4.854328638709999311, 1471.845299823429968, 270.0724596863979627 ) ) ;
#93271 = DIRECTION ( 'NONE',  ( -1.000000000000000000, 0.000000000000000000, 0.000000000000000000 ) ) ;
#93272 = CARTESIAN_POINT ( 'NONE',  ( -120.3440751137400895, 1358.631207110788864, 302.4487324766139409 ) ) ;
#93273 = CARTESIAN_POINT ( 'NONE',  ( 21.61512607259999896, 1497.713060387329961, 209.1218459615069776 ) ) ;
#93274 = CARTESIAN_POINT ( 'NONE',  ( -2.170920964160679922, 1475.243440997999869, 197.8895928898250247 ) ) ;
#93275 = CARTESIAN_POINT ( 'NONE',  ( -13.91344329550000047, 1453.313060387329870, 195.2084026667980083 ) ) ;
#93276 = CARTESIAN_POINT ( 'NONE',  ( 5.476632270752042508, 1369.746243050054318, 207.6218459616987673 ) ) ;
#93277 = CARTESIAN_POINT ( 'NONE',  ( -8.953512711461160123, 1447.964222359199994, 211.4838949693660197 ) ) ;
#93278 = CARTESIAN_POINT ( 'NONE',  ( -15.29008408311359979, 1408.674945077619896, 269.5757537869589555 ) ) ;
#93279 = CARTESIAN_POINT ( 'NONE',  ( -13.72009304850000078, 1435.216353071280082, 149.6398781814980055 ) ) ;
#93280 = ORIENTED_EDGE ( 'NONE', *, *, #75537, .T. ) ;
#93281 = CARTESIAN_POINT ( 'NONE',  ( -4.326992699989999913, 1515.158586642790169, 209.1218459619010162 ) ) ;
#93282 = CARTESIAN_POINT ( 'NONE',  ( 13.69653208179999915, 1445.056976842780159, 189.0353891572979990 ) ) ;
#93283 = EDGE_LOOP ( 'NONE', ( #98530, #19762, #14005, #78103 ) ) ;
#93284 = ORIENTED_EDGE ( 'NONE', *, *, #77689, .T. ) ;
#93285 = TOROIDAL_SURFACE ( 'NONE', #71849, 2.000000000000000000, 1.000000000000000000 ) ;
#93286 = CARTESIAN_POINT ( 'NONE',  ( 5.023595874863397093, 1422.819015197833551, 184.4347302699305260 ) ) ;
#93287 = CARTESIAN_POINT ( 'NONE',  ( 21.96543842109161204, 1523.313115944345327, 182.9844783913649451 ) ) ;
#93288 = CARTESIAN_POINT ( 'NONE',  ( 2.296124850935000072, 1516.677239312369920, 213.7299927514870319 ) ) ;
#93289 = CARTESIAN_POINT ( 'NONE',  ( -14.88092153600000067, 1470.466294572129755, 187.7539579896979944 ) ) ;
#93291 = EDGE_CURVE ( 'NONE', #80871, #2901, #38728, .T. ) ;
#93290 = CARTESIAN_POINT ( 'NONE',  ( -9.699660872752350116, 1472.030908259890111, 212.1562907213800031 ) ) ;
#93292 = ORIENTED_EDGE ( 'NONE', *, *, #61773, .F. ) ;
#93293 = CARTESIAN_POINT ( 'NONE',  ( -113.4000000000000057, 1379.413060387289988, 303.4364477938589744 ) ) ;
#93294 = CARTESIAN_POINT ( 'NONE',  ( -2.873958889724999910, 1516.588006113850042, 202.1873174023370154 ) ) ;
#93295 = AXIS2_PLACEMENT_3D ( 'NONE', #83979, #40324, #23518 ) ;
#93296 = CARTESIAN_POINT ( 'NONE',  ( -28.13569435490000004, 1509.875538910929890, 202.7428287808179732 ) ) ;
#93297 = CARTESIAN_POINT ( 'NONE',  ( 4.026786250540000722, 1408.413060387330006, 137.0999999980979851 ) ) ;
#93298 = CARTESIAN_POINT ( 'NONE',  ( -32.52026698425390094, 1384.562322830350013, 207.0570309995399896 ) ) ;
#93299 = CARTESIAN_POINT ( 'NONE',  ( -5.451927469500000178, 1408.921438759329931, 196.0890200002980066 ) ) ;
#93300 = CARTESIAN_POINT ( 'NONE',  ( -105.5485668489999966, 1388.544618357170066, 309.1779867852590655 ) ) ;
#93302 = ORIENTED_EDGE ( 'NONE', *, *, #98759, .F. ) ;
#93301 = CARTESIAN_POINT ( 'NONE',  ( 15.58634593796259082, 1506.535970899979247, 193.4985844669198514 ) ) ;
#93303 = CARTESIAN_POINT ( 'NONE',  ( -26.02644626588410048, 1469.349415895499760, 210.5465789334240299 ) ) ;
#93304 = CARTESIAN_POINT ( 'NONE',  ( 22.23102602810000405, 1508.124938944730047, 224.5788317314980134 ) ) ;
#93305 = CARTESIAN_POINT ( 'NONE',  ( -49.40611499322205447, 1379.690198512848838, 244.6122530584670187 ) ) ;
#93306 = CARTESIAN_POINT ( 'NONE',  ( 10.48725263721749990, 1460.097526990779897, 206.1395495003129952 ) ) ;
#93307 = ADVANCED_FACE ( 'NONE', ( #70733 ), #47152, .T. ) ;
#93308 = CARTESIAN_POINT ( 'NONE',  ( -4.987078454554999318, 1508.551704408389924, 205.6342535004969818 ) ) ;
#93309 = CARTESIAN_POINT ( 'NONE',  ( -3.445201526505000000, 1516.743010792419909, 210.8372070624770060 ) ) ;
#93310 = VECTOR ( 'NONE', #101466, 1000.000000000000227 ) ;
#93311 = CARTESIAN_POINT ( 'NONE',  ( -68.59203063350000207, 1379.747524784999996, 279.7276289599590200 ) ) ;
#93312 = DIRECTION ( 'NONE',  ( -1.699538841806929935E-33, 1.000000000000000000, -1.698192320643030073E-16 ) ) ;
#93313 = CARTESIAN_POINT ( 'NONE',  ( -20.71343476517490956, 1524.726013923371283, 238.3377464195766038 ) ) ;
#93314 = CARTESIAN_POINT ( 'NONE',  ( 2.865636809105000182, 1516.815173273089840, 207.9858416580370033 ) ) ;
#93315 = VERTEX_POINT ( 'NONE', #10794 ) ;
#93316 = CARTESIAN_POINT ( 'NONE',  ( -10.10810022239999917, 1473.154118535690031, 207.6476596274190172 ) ) ;
#93317 = CARTESIAN_POINT ( 'NONE',  ( -19.96907025085698351, 1456.518973795319653, 225.2441494129984676 ) ) ;
#93318 = ORIENTED_EDGE ( 'NONE', *, *, #19919, .T. ) ;
#93319 = DIRECTION ( 'NONE',  ( -3.828568698926946970E-16, 0.000000000000000000, 1.000000000000000000 ) ) ;
#93320 = EDGE_CURVE ( 'NONE', #36772, #39681, #46644, .T. ) ;
#93321 = CARTESIAN_POINT ( 'NONE',  ( -22.98628035409431192, 1509.732561025907899, 227.7597765635970859 ) ) ;
#93322 = CARTESIAN_POINT ( 'NONE',  ( -4.070572111042093155, 1440.961967058545042, 184.9442369547908243 ) ) ;
#93323 = CARTESIAN_POINT ( 'NONE',  ( -9.678642251699999477, 1414.581381510680103, 208.2850554633440083 ) ) ;
#93324 = CARTESIAN_POINT ( 'NONE',  ( 2.482344662330000062, 1440.444625599219989, 150.5580151863979950 ) ) ;
#93325 = ADVANCED_FACE ( 'NONE', ( #53929 ), #92218, .T. ) ;
#93326 = CARTESIAN_POINT ( 'NONE',  ( 4.907342515529999893, 1485.995388969990245, 199.5215206418690173 ) ) ;
#93327 = CARTESIAN_POINT ( 'NONE',  ( 1.338019250827790163, 1431.361302059610125, 218.5179660117710227 ) ) ;
#93328 = FACE_OUTER_BOUND ( 'NONE', #110670, .T. ) ;
#93330 = CARTESIAN_POINT ( 'NONE',  ( 35.14729775950531376, 1435.724875876663646, 135.0317234473804433 ) ) ;
#93329 = CARTESIAN_POINT ( 'NONE',  ( 1.132949076425000090, 1516.693851263360102, 214.1195642086070166 ) ) ;
#93331 = CARTESIAN_POINT ( 'NONE',  ( 20.25110058739999985, 1509.046039775230156, 188.8042360712979928 ) ) ;
#93332 = CARTESIAN_POINT ( 'NONE',  ( -6.942354311545000378, 1516.905946377369901, 216.8406094761369900 ) ) ;
#93333 = ORIENTED_EDGE ( 'NONE', *, *, #80813, .F. ) ;
#93334 = CARTESIAN_POINT ( 'NONE',  ( -17.14943674877569890, 1460.897686246159992, 228.2718295297070199 ) ) ;
#93335 = CARTESIAN_POINT ( 'NONE',  ( -11.60004869885204215, 1426.273944179774844, 138.2686100621498326 ) ) ;
#93336 = VERTEX_POINT ( 'NONE', #59969 ) ;
#93337 = CARTESIAN_POINT ( 'NONE',  ( 1.654267213550000060, 1420.334206264930117, 184.6982689316979815 ) ) ;
#93338 = CARTESIAN_POINT ( 'NONE',  ( 2.487422374635116284, 1523.954924407802764, 175.4471440611261244 ) ) ;
#93339 = CARTESIAN_POINT ( 'NONE',  ( -21.39706014069999895, 1505.152228921489950, 211.4762334770289840 ) ) ;
#93340 = DIRECTION ( 'NONE',  ( -1.755985294532469921E-16, 1.000000000000000000, -1.338183447452831989E-16 ) ) ;
#93341 = CARTESIAN_POINT ( 'NONE',  ( -4.376990639194925592, 1508.181752870080800, 220.5833432285685944 ) ) ;
#93342 = CARTESIAN_POINT ( 'NONE',  ( 17.57597226803159529, 1423.079937563883959, 226.3733900275827580 ) ) ;
#93344 = EDGE_CURVE ( 'NONE', #102960, #7082, #16799, .T. ) ;
#93343 = DIRECTION ( 'NONE',  ( 0.9774101051267758411, 0.000000000000000000, -0.2113515706023144369 ) ) ;
#93345 = SPHERICAL_SURFACE ( 'NONE', #103859, 2.000000000510000042 ) ;
#93346 = CARTESIAN_POINT ( 'NONE',  ( -9.709302419510001059, 1435.943783413959864, 148.7752736812980174 ) ) ;
#93347 = CARTESIAN_POINT ( 'NONE',  ( 42.05112052806060063, 1440.913060353040009, 262.0200795381490479 ) ) ;
#93349 = DIRECTION ( 'NONE',  ( 0.000000000000000000, -1.000000000000000000, 0.000000000000000000 ) ) ;
#93348 = CARTESIAN_POINT ( 'NONE',  ( -10.27997055782769920, 1471.607896215150049, 209.6291398427710249 ) ) ;
#93350 = DIRECTION ( 'NONE',  ( 0.9455185755993178454, 0.000000000000000000, -0.3255681544571537578 ) ) ;
#93351 = VERTEX_POINT ( 'NONE', #26326 ) ;
#93352 = EDGE_CURVE ( 'NONE', #8198, #61380, #57267, .T. ) ;
#93353 = ORIENTED_EDGE ( 'NONE', *, *, #73400, .T. ) ;
#93354 = CARTESIAN_POINT ( 'NONE',  ( 1.548840712014900145, 1416.196255291370107, 190.3585702930099899 ) ) ;
#93355 = EDGE_CURVE ( 'NONE', #101350, #29004, #14963, .T. ) ;
#93356 = CARTESIAN_POINT ( 'NONE',  ( -20.20959865099451847, 1512.187213306747481, 236.2316688286741453 ) ) ;
#93357 = CARTESIAN_POINT ( 'NONE',  ( -2.157496122451409537, 1526.189892541618974, 177.9627121745355396 ) ) ;
#93358 = CARTESIAN_POINT ( 'NONE',  ( 3.920879176457659820, 1439.701872010520219, 184.6839060028229937 ) ) ;
#93359 = CARTESIAN_POINT ( 'NONE',  ( 2.500000000000000000, 1448.894380913990062, 168.9807461826979704 ) ) ;
#93360 = EDGE_CURVE ( 'NONE', #6969, #101078, #77242, .T. ) ;
#93361 = CARTESIAN_POINT ( 'NONE',  ( 2.448877809997429988, 1508.551704408389924, 219.5616561886379827 ) ) ;
#93362 = CARTESIAN_POINT ( 'NONE',  ( 5.140094423509999011, 1436.845494339190054, 228.7442485628990028 ) ) ;
#93363 = CARTESIAN_POINT ( 'NONE',  ( -64.14920489430819828, 1383.791463424650146, 287.2113058269809471 ) ) ;
#93364 = CARTESIAN_POINT ( 'NONE',  ( 22.54437430309999968, 1451.697077564529991, 142.2380798234979977 ) ) ;
#93365 = CARTESIAN_POINT ( 'NONE',  ( -5.254554520956747687, 1391.913060387289988, 214.4737135289948071 ) ) ;
#93366 = CARTESIAN_POINT ( 'NONE',  ( 12.32717396260830078, 1492.190839752460079, 209.5895836007599939 ) ) ;
#93368 = EDGE_LOOP ( 'NONE', ( #62214, #12655, #62058, #101959, #64197 ) ) ;
#93367 = CARTESIAN_POINT ( 'NONE',  ( -1.880000144899999892, 1457.107126484389937, 218.8420116927090078 ) ) ;
#93369 = CARTESIAN_POINT ( 'NONE',  ( -1.359627476360000031, 1451.982671778829854, 183.7885425899980305 ) ) ;
#93370 = CARTESIAN_POINT ( 'NONE',  ( -44.90575339929999643, 1380.945526020650050, 246.6134158280590043 ) ) ;
#93371 = CARTESIAN_POINT ( 'NONE',  ( 8.274166279097638466, 1436.481534978870059, 206.7313558027209695 ) ) ;
#93372 = VERTEX_POINT ( 'NONE', #58853 ) ;
#93373 = ORIENTED_EDGE ( 'NONE', *, *, #44989, .F. ) ;
#93374 = DIRECTION ( 'NONE',  ( 0.000000000000000000, 1.000000000000000000, 0.000000000000000000 ) ) ;
#93375 = CARTESIAN_POINT ( 'NONE',  ( -9.252619606462529234, 1386.194650040039960, 218.4639876966940051 ) ) ;
#93376 = CARTESIAN_POINT ( 'NONE',  ( 39.78919856916219544, 1441.136557108880197, 136.8413242771979981 ) ) ;
#93378 = CARTESIAN_POINT ( 'NONE',  ( 18.34590456075850184, 1416.851343895820037, 209.3831232368769975 ) ) ;
#93377 = DIRECTION ( 'NONE',  ( -0.8775825618903712044, -0.000000000000000000, -0.4794255386042061140 ) ) ;
#93379 = EDGE_CURVE ( 'NONE', #46101, #37972, #94084, .T. ) ;
#93380 = CARTESIAN_POINT ( 'NONE',  ( -6.816032832730000379, 1464.119504676089946, 200.4313534491789994 ) ) ;
#93381 = CARTESIAN_POINT ( 'NONE',  ( -109.0917520289999914, 1383.655254917920047, 297.2994177358589809 ) ) ;
#93382 = FACE_OUTER_BOUND ( 'NONE', #48086, .T. ) ;
#93383 = CARTESIAN_POINT ( 'NONE',  ( -0.3594932246804328768, 1451.468209969438931, 182.7573421932325459 ) ) ;
#93384 = CARTESIAN_POINT ( 'NONE',  ( -15.31939472967450122, 1508.551704408389924, 214.5736414636859877 ) ) ;
#93385 = CARTESIAN_POINT ( 'NONE',  ( 4.243919250670000309, 1409.061261313129990, 187.1626498370980016 ) ) ;
#93386 = CARTESIAN_POINT ( 'NONE',  ( 4.187037607680000662, 1423.917686004630013, 184.1424184849980179 ) ) ;
#93387 = EDGE_CURVE ( 'NONE', #30117, #75707, #21567, .T. ) ;
#93388 = CARTESIAN_POINT ( 'NONE',  ( 5.538490023541649876, 1434.582427083100129, 202.4776097773300023 ) ) ;
#93389 = CARTESIAN_POINT ( 'NONE',  ( -4.277751951706020073, 1441.052902712039895, 157.0207293387669836 ) ) ;
#93390 = AXIS2_PLACEMENT_3D ( 'NONE', #46410, #29037, #71633 ) ;
#93391 = CARTESIAN_POINT ( 'NONE',  ( 11.78818133093700027, 1426.417832666100139, 148.5075478569980021 ) ) ;
#93392 = CARTESIAN_POINT ( 'NONE',  ( 0.7979415355729999604, 1465.377788775429963, 236.2027333408979928 ) ) ;
#93393 = ORIENTED_EDGE ( 'NONE', *, *, #74040, .F. ) ;
#93394 = CARTESIAN_POINT ( 'NONE',  ( 4.912821653402110300, 1470.978916084819957, 187.7503311908630224 ) ) ;
#93395 = CARTESIAN_POINT ( 'NONE',  ( -9.828024340748898524, 1446.801136768030119, 212.2328356403849909 ) ) ;
#93396 = CARTESIAN_POINT ( 'NONE',  ( -26.04901691849709877, 1446.564900598870054, 138.1454006445720211 ) ) ;
#93397 = CARTESIAN_POINT ( 'NONE',  ( -14.48519483975229960, 1416.181292564900104, 203.8595933512790168 ) ) ;
#93398 = CARTESIAN_POINT ( 'NONE',  ( 18.18137294690000161, 1507.608465325429734, 188.5297611294979845 ) ) ;
#93399 = B_SPLINE_CURVE_WITH_KNOTS ( 'NONE', 3,
 ( #13023, #21417, #66235, #98701, #39900, #55629, #47210, #47755, #21960, #15223, #99786, #23077, #90289, #5759, #81890, #91950, #49416, #30944, #6297, #83540, #90845, #48320, #106556, #5193, #73524, #107657, #99230, #22508, #14130 ),
 .UNSPECIFIED., .F., .F.,
 ( 4, 2, 2, 1, 1, 2, 2, 2, 2, 2, 2, 2, 1, 2, 2, 4 ),
 ( 0.000000000000000000, 0.1250000000022731261, 0.1875000000034070802, 0.2187500000039730719, 0.2343750000041630310, 0.2421875000041678883, 0.2500000000041727732, 0.3750000000024993341, 0.4375000000016680546, 0.5000000000008367751, 0.6249999999991767696, 0.6874999999983395504, 0.7187499999981038501, 0.7343749999981645793, 0.7499999999982251975, 1.000000000000000000 ),
 .UNSPECIFIED. ) ;
#93400 = CARTESIAN_POINT ( 'NONE',  ( -2.040094528446590223E-09, 1471.382348965860047, 257.5322757312809472 ) ) ;
#93401 = CARTESIAN_POINT ( 'NONE',  ( 14.59277107062129986, 1436.244837967300100, 149.8707660814949918 ) ) ;
#93402 = CARTESIAN_POINT ( 'NONE',  ( -0.7890062529830000893, 1416.021639796329964, 227.7424621462980099 ) ) ;
#93403 = CARTESIAN_POINT ( 'NONE',  ( -23.80546598920000179, 1430.806027415329936, 211.0847187605880038 ) ) ;
#93404 = CARTESIAN_POINT ( 'NONE',  ( -1.804012654820000172, 1476.275330878590012, 198.7886378605990103 ) ) ;
#93405 = CARTESIAN_POINT ( 'NONE',  ( -107.0970161019999978, 1387.848630225089892, 309.9720921612589564 ) ) ;
#93406 = CARTESIAN_POINT ( 'NONE',  ( -7.554100975061009748, 1510.639750819960000, 214.6448992246709793 ) ) ;
#93407 = CARTESIAN_POINT ( 'NONE',  ( 1.826803300828446330, 1359.441796170313637, 207.6218459616987673 ) ) ;
#93408 = CARTESIAN_POINT ( 'NONE',  ( -46.25879973035969783, 1439.825279062879872, 267.5901298074010128 ) ) ;
#93409 = CARTESIAN_POINT ( 'NONE',  ( 2.151199513684490139, 1429.150501611710069, 217.1299383594469816 ) ) ;
#93410 = CARTESIAN_POINT ( 'NONE',  ( -7.824467775549998727, 1425.791227067999898, 206.8230464701690039 ) ) ;
#93411 = EDGE_LOOP ( 'NONE', ( #59573, #84489, #10805, #103649 ) ) ;
#93412 = CARTESIAN_POINT ( 'NONE',  ( -4.042388539304999640, 1517.045004075700035, 208.3857484934819979 ) ) ;
#93413 = CARTESIAN_POINT ( 'NONE',  ( -19.63722818134010240, 1521.951704408389787, 200.0074286634620364 ) ) ;
#93414 = CARTESIAN_POINT ( 'NONE',  ( 19.26228722078564459, 1456.171679175456120, 225.0188521063314511 ) ) ;
#93415 = CARTESIAN_POINT ( 'NONE',  ( 7.225592507856469560, 1426.518265663189823, 212.9482508202709994 ) ) ;
#93416 = CARTESIAN_POINT ( 'NONE',  ( -26.58673239743909633, 1451.978834094609965, 135.0959505759149977 ) ) ;
#93417 = VERTEX_POINT ( 'NONE', #26899 ) ;
#93418 = CARTESIAN_POINT ( 'NONE',  ( -2.138097991060000180E-08, 1420.509147084929964, 221.4103263195979707 ) ) ;
#93420 = CARTESIAN_POINT ( 'NONE',  ( 15.24905281719999905, 1488.805759879029893, 194.1126383535979869 ) ) ;
#93419 = CARTESIAN_POINT ( 'NONE',  ( -10.94209231895430179, 1492.979988125699947, 207.3926202358989883 ) ) ;
#93421 = CARTESIAN_POINT ( 'NONE',  ( -2.374774714134009646, 1419.515052570159924, 186.0454628696550117 ) ) ;
#93422 = CARTESIAN_POINT ( 'NONE',  ( -4.261736552472808803, 1515.372048948340080, 207.2788837468951613 ) ) ;
#93423 = CARTESIAN_POINT ( 'NONE',  ( 10.54065430160000005, 1425.980116282510153, 194.3020730708990129 ) ) ;
#93424 = LINE ( 'NONE', #50357, #20306 ) ;
#93425 = EDGE_LOOP ( 'NONE', ( #65847, #57664, #1373, #18513 ) ) ;
#93426 = CARTESIAN_POINT ( 'NONE',  ( -4.976825802775040053, 1408.127936775080116, 270.2880426513530097 ) ) ;
#93427 = CARTESIAN_POINT ( 'NONE',  ( 6.488431865357080497, 1418.472541117210085, 233.3050633955320166 ) ) ;
#93428 = CARTESIAN_POINT ( 'NONE',  ( 4.939530087350459949E-13, 1547.051704408389924, 209.1218459616989946 ) ) ;
#93429 = ORIENTED_EDGE ( 'NONE', *, *, #13099, .T. ) ;
#93430 = ORIENTED_EDGE ( 'NONE', *, *, #77426, .T. ) ;
#93431 = CARTESIAN_POINT ( 'NONE',  ( -23.26431872588840122, 1410.005238423490027, 210.0136070511539970 ) ) ;
#93432 = CARTESIAN_POINT ( 'NONE',  ( -1.356543646279819937, 1410.335726175669834, 185.6038078910299873 ) ) ;
#93433 = CARTESIAN_POINT ( 'NONE',  ( -3.955028505459999653E-16, 1420.349145488430167, 170.8340916043979973 ) ) ;
#93434 = CARTESIAN_POINT ( 'NONE',  ( -2.286265947080000416, 1427.727383903629971, 112.4493539157979995 ) ) ;
#93435 = CARTESIAN_POINT ( 'NONE',  ( -19.84697927394439887, 1469.911627675270211, 193.3779138725080031 ) ) ;
#93436 = CARTESIAN_POINT ( 'NONE',  ( 4.246473540454690720, 1508.879013859839915, 212.8696703459879984 ) ) ;
#93437 = CARTESIAN_POINT ( 'NONE',  ( 36.83564954605069630, 1461.809058848290078, 268.7794616686949780 ) ) ;
#93438 = CARTESIAN_POINT ( 'NONE',  ( -11.00165343754819958, 1391.913060387039877, 206.0010710664089970 ) ) ;
#93439 = CARTESIAN_POINT ( 'NONE',  ( -5.706316465129999571, 1427.594387386090148, 202.5140759953890210 ) ) ;
#93440 = CARTESIAN_POINT ( 'NONE',  ( -1.135460355084999762, 1516.790374942449944, 205.8685445508469911 ) ) ;
#93441 = ORIENTED_EDGE ( 'NONE', *, *, #29677, .T. ) ;
#93442 = CARTESIAN_POINT ( 'NONE',  ( 18.80856254815538975, 1458.020595720538040, 227.1643417640127041 ) ) ;
#93443 = CARTESIAN_POINT ( 'NONE',  ( 0.3220128118225270009, 1444.991323582689802, 199.0632997620110132 ) ) ;
#93444 = CARTESIAN_POINT ( 'NONE',  ( -21.38516915558007270, 1501.977400791986611, 180.3939891059723664 ) ) ;
#93445 = EDGE_LOOP ( 'NONE', ( #6265, #82525, #7411, #81550 ) ) ;
#93446 = CARTESIAN_POINT ( 'NONE',  ( -10.88526200584609960, 1480.877704328530172, 210.6248047774270162 ) ) ;
#93447 = CARTESIAN_POINT ( 'NONE',  ( 5.382848799108077564, 1434.543798359927450, 202.5092580921534307 ) ) ;
#93448 = CARTESIAN_POINT ( 'NONE',  ( -4.604592056941269718, 1508.551704408389924, 212.9405302482509796 ) ) ;
#93449 = CARTESIAN_POINT ( 'NONE',  ( -9.853078183510000088, 1384.932634673870098, 199.8720430995890069 ) ) ;
#93450 = CARTESIAN_POINT ( 'NONE',  ( 7.496491729189999731, 1422.157925818930153, 195.6730238920989962 ) ) ;
#93451 = CARTESIAN_POINT ( 'NONE',  ( -2.012497635052489908, 1432.674193821990002, 218.4327187538029875 ) ) ;
#93452 = CARTESIAN_POINT ( 'NONE',  ( -4.474843316269999427, 1495.214972003490175, 197.6335801705990036 ) ) ;
#93453 = CARTESIAN_POINT ( 'NONE',  ( 1.909580902767660016, 1408.979744421860232, 186.9029660347310084 ) ) ;
#93455 = DIRECTION ( 'NONE',  ( 0.9824080081115887930, -2.243614313870717968E-31, 0.1867471702549210744 ) ) ;
#93454 = CARTESIAN_POINT ( 'NONE',  ( 1.492583962270000120, 1417.432316503030052, 234.4047366681980122 ) ) ;
#93456 = CARTESIAN_POINT ( 'NONE',  ( -16.49514911236800785, 1525.343710797494396, 181.2134097543055020 ) ) ;
#93457 = CARTESIAN_POINT ( 'NONE',  ( -11.62355165729999840, 1378.295668984849954, 213.2764633795689804 ) ) ;
#93458 = FACE_OUTER_BOUND ( 'NONE', #62154, .T. ) ;
#93459 = EDGE_LOOP ( 'NONE', ( #63084, #35465, #90793 ) ) ;
#93460 = CARTESIAN_POINT ( 'NONE',  ( 11.69495607182030028, 1415.089948427370018, 221.9856941327800257 ) ) ;
#93461 = CYLINDRICAL_SURFACE ( 'NONE', #5204, 2.000000000000003109 ) ;
#93462 = CARTESIAN_POINT ( 'NONE',  ( 20.28288303839970297, 1497.593166955129846, 226.9817472065090271 ) ) ;
#93463 = CARTESIAN_POINT ( 'NONE',  ( -11.91005457920000055, 1391.448248967449899, 205.5251632796090178 ) ) ;
#93464 = CARTESIAN_POINT ( 'NONE',  ( -113.4589914632272212, 1390.913060387289988, 306.7211498618009387 ) ) ;
#93465 = CARTESIAN_POINT ( 'NONE',  ( -35.74233958356999352, 1450.108979485610007, 136.2379703606449937 ) ) ;
#93466 = CARTESIAN_POINT ( 'NONE',  ( 13.29158107345610063, 1425.436905002130061, 221.8979834808779970 ) ) ;
#93467 = ADVANCED_FACE ( 'NONE', ( #8983 ), #48445, .T. ) ;
#93468 = CARTESIAN_POINT ( 'NONE',  ( -11.47403709369999980, 1467.186912539730201, 262.6648722463980334 ) ) ;
#93469 = CARTESIAN_POINT ( 'NONE',  ( -16.87240959569610155, 1409.502257913620042, 196.1298155364530089 ) ) ;
#93471 = EDGE_CURVE ( 'NONE', #63441, #13894, #60948, .T. ) ;
#93470 = CARTESIAN_POINT ( 'NONE',  ( 11.92576087849999844, 1433.460360144529886, 150.1385202855979912 ) ) ;
#93472 = CARTESIAN_POINT ( 'NONE',  ( 17.26713005559999914, 1453.798585003029984, 234.3916895593979746 ) ) ;
#93473 = B_SPLINE_CURVE_WITH_KNOTS ( 'NONE', 3,
 ( #29441, #3731, #107257, #5352, #12654, #91001, #22671, #106164, #81490, #56872, #89360, #30552, #4791, #65281, #80961, #80417 ),
 .UNSPECIFIED., .F., .F.,
 ( 4, 3, 3, 3, 3, 4 ),
 ( -7.430926500750000052, -7.205864747455129837, -6.166310293502959894, -5.126937956299970622, -4.087228192414619876, -3.046684027040000409 ),
 .UNSPECIFIED. ) ;
#93474 = CARTESIAN_POINT ( 'NONE',  ( -10.99082249780570031, 1462.122377081429931, 210.0450475653020135 ) ) ;
#93475 = CARTESIAN_POINT ( 'NONE',  ( -16.76078030769999927, 1420.494757909599912, 203.1294657649889928 ) ) ;
#93476 = CARTESIAN_POINT ( 'NONE',  ( 12.80027819501479946, 1420.728244072559846, 201.6266405663580201 ) ) ;
#93477 = CARTESIAN_POINT ( 'NONE',  ( 6.653879410529840221, 1466.704669164200141, 216.5527109682910236 ) ) ;
#93478 = CARTESIAN_POINT ( 'NONE',  ( -19.52953025160000067, 1486.085187770929906, 189.9534856570979855 ) ) ;
#93479 = APPLICATION_CONTEXT ( 'automotive_design' ) ;
#93480 = CARTESIAN_POINT ( 'NONE',  ( 12.92120458945395178, 1398.295995395735417, 207.6489814522168160 ) ) ;
#93481 = CARTESIAN_POINT ( 'NONE',  ( 2.902343810100000088, 1466.632250239430050, 234.1422825223980340 ) ) ;
#93482 = B_SPLINE_CURVE_WITH_KNOTS ( 'NONE', 3,
 ( #23266, #108392, #80987, #65854, #47393, #31123, #55811, #6480, #73141, #4818, #40080, #4293, #90477, #106725, #38963, #99973, #5934, #73710, #31673, #74260, #89928, #48504, #74803, #23812, #57463, #38420, #30578, #83191, #98328, #107284, #46858, #72596, #32235, #13203, #99417, #91589, #14864, #56345, #107835, #49055, #40632, #30015, #108946, #21606, #82643, #66415, #100532, #64769, #65305, #98879, #13753, #22145, #82073, #47938, #22696, #58003, #64205, #12678, #5378, #81514, #39536, #56895, #91026, #14313, #7030, #68070, #110044, #77008, #102182, #85946, #314, #66960, #41188, #109500, #51805, #24902, #7579, #75360, #84286, #32776, #42846, #8121, #92681, #93234 ),
 .UNSPECIFIED., .F., .F.,
 ( 4, 2, 2, 2, 2, 2, 1, 1, 2, 2, 2, 1, 2, 2, 2, 1, 2, 2, 2, 2, 2, 2, 2, 2, 2, 1, 2, 2, 2, 2, 1, 2, 2, 2, 1, 1, 2, 2, 2, 2, 2, 2, 2, 2, 2, 4 ),
 ( 0.000000000000000000, 0.03125000000032555209, 0.04687500000049735216, 0.06250000000066914529, 0.09375000000098251962, 0.1093750000011391998, 0.1171875000012245205, 0.1210937500012671947, 0.1230468750012885248, 0.1250000000013098411, 0.1562500000012651546, 0.1718750000012148615, 0.1796875000011508294, 0.1875000000010867973, 0.2187500000008300860, 0.2343750000007013834, 0.2421875000006821210, 0.2500000000006628031, 0.3125000000008504308, 0.3437500000008782974, 0.3750000000009061085, 0.4375000000009540146, 0.5000000000010018653, 0.5625000000010497159, 0.5937500000010736967, 0.6093750000010144108, 0.6171875000009849899, 0.6250000000009555690, 0.6875000000012977397, 0.7187500000014160895, 0.7343750000015131230, 0.7421875000015614177, 0.7500000000016097124, 0.7812500000016466828, 0.7968750000016586732, 0.8046875000017007507, 0.8085937500016995294, 0.8125000000016981971, 0.8437500000015355495, 0.8593750000014233059, 0.8671875000013464785, 0.8750000000012696511, 0.9062500000009766632, 0.9218750000008136825, 0.9375000000006507017, 1.000000000000000000 ),
 .UNSPECIFIED. ) ;
#93483 = CARTESIAN_POINT ( 'NONE',  ( 22.14280420710000286, 1430.347761818229856, 217.9176945388080071 ) ) ;
#93484 = EDGE_CURVE ( 'NONE', #60257, #105885, #3718, .T. ) ;
#93485 = CARTESIAN_POINT ( 'NONE',  ( 3.727343958979999705, 1478.549430577389785, 229.1364021244989715 ) ) ;
#93486 = CARTESIAN_POINT ( 'NONE',  ( -33.42844755917176514, 1501.977400791986611, 222.1271778627171045 ) ) ;
#93487 = CARTESIAN_POINT ( 'NONE',  ( -10.24703385824910029, 1383.862840724990065, 218.6056771012169975 ) ) ;
#93488 = CARTESIAN_POINT ( 'NONE',  ( -5.292247061280000331, 1391.913060387289988, 203.8075142969990168 ) ) ;
#93489 = CARTESIAN_POINT ( 'NONE',  ( 20.56230379148770027, 1477.111289846620139, 217.7195331044080149 ) ) ;
#93490 = CARTESIAN_POINT ( 'NONE',  ( 7.335900995594999863, 1517.068717944079935, 213.1567545299469657 ) ) ;
#93491 = CARTESIAN_POINT ( 'NONE',  ( -13.58779897810510029, 1422.057029525010194, 203.7652383086400221 ) ) ;
#93492 = CARTESIAN_POINT ( 'NONE',  ( 0.1688278169330330314, 1481.018758052769954, 182.0506284089370013 ) ) ;
#93494 = EDGE_LOOP ( 'NONE', ( #27615, #99183, #41745, #2450 ) ) ;
#93493 = CYLINDRICAL_SURFACE ( 'NONE', #33571, 1.999999999999999556 ) ;
#93495 = CARTESIAN_POINT ( 'NONE',  ( 2.157482617120738855, 1526.189899547014647, 177.9627270532062937 ) ) ;
#93496 = CARTESIAN_POINT ( 'NONE',  ( -17.11714618744286653, 1444.740067931808881, 162.7561046190442369 ) ) ;
#93497 = CARTESIAN_POINT ( 'NONE',  ( 13.50074992389999906, 1434.968959668390198, 149.7892634259980298 ) ) ;
#93498 = CARTESIAN_POINT ( 'NONE',  ( -39.62133910739139964, 1449.056109088350013, 134.0999999980940061 ) ) ;
#93499 = CARTESIAN_POINT ( 'NONE',  ( -110.0634901189999937, 1384.899971912280080, 296.9512051102590249 ) ) ;
#93500 = VERTEX_POINT ( 'NONE', #54331 ) ;
#93501 = CARTESIAN_POINT ( 'NONE',  ( -38.62063634653199529, 1443.662372644130073, 137.1803698382369987 ) ) ;
#93502 = CARTESIAN_POINT ( 'NONE',  ( 2.620401159595450391, 1523.462669333491931, 176.0805060895404495 ) ) ;
#93503 = CARTESIAN_POINT ( 'NONE',  ( 7.273621552740451968, 1447.419844749426829, 203.6721120216986662 ) ) ;
#93504 = FACE_OUTER_BOUND ( 'NONE', #26631, .T. ) ;
#93505 = CARTESIAN_POINT ( 'NONE',  ( -7.878925220306069122, 1435.199465323840059, 212.6510895369020204 ) ) ;
#93506 = CARTESIAN_POINT ( 'NONE',  ( -107.4791259594196617, 1380.106263187048626, 309.4148095461648609 ) ) ;
#93507 = CARTESIAN_POINT ( 'NONE',  ( -17.80192030199999920, 1421.535218730880160, 207.7056227470090164 ) ) ;
#93508 = DIRECTION ( 'NONE',  ( -4.857225732735055447E-14, 0.000000000000000000, 1.000000000000000000 ) ) ;
#93509 = CARTESIAN_POINT ( 'NONE',  ( -11.42604309490000070, 1391.913060387289988, 207.1941759383389865 ) ) ;
#93510 = CARTESIAN_POINT ( 'NONE',  ( -84.10063176446999478, 1385.173004153059992, 287.8709662445750155 ) ) ;
#93511 = EDGE_CURVE ( 'NONE', #97416, #39586, #1961, .T. ) ;
#93512 = CARTESIAN_POINT ( 'NONE',  ( -11.62628111383389928, 1391.913060387289988, 210.2022570141400024 ) ) ;
#93513 = CARTESIAN_POINT ( 'NONE',  ( 12.25515206146219960, 1421.728505657969890, 208.1409196252290030 ) ) ;
#93514 = ORIENTED_EDGE ( 'NONE', *, *, #6278, .F. ) ;
#93515 = CARTESIAN_POINT ( 'NONE',  ( -33.31574679630000446, 1451.295103689730240, 135.9631183953979985 ) ) ;
#93516 = CARTESIAN_POINT ( 'NONE',  ( 17.22654844235838567, 1443.913060387328869, 162.9224179604370590 ) ) ;
#93518 = VERTEX_POINT ( 'NONE', #46477 ) ;
#93517 = CARTESIAN_POINT ( 'NONE',  ( -1.800936940629448868, 1526.306647125542440, 239.8931631715260835 ) ) ;
#93519 = CARTESIAN_POINT ( 'NONE',  ( 2.771411902819999717, 1474.602400374589934, 220.2115235061990006 ) ) ;
#93520 =( BOUNDED_CURVE ( )  B_SPLINE_CURVE ( 3, ( #25192, #17892, #67789, #34 ),
 .UNSPECIFIED., .F., .T. ) 
 B_SPLINE_CURVE_WITH_KNOTS ( ( 4, 4 ),
 ( 0.9324631327127209657, 1.578300326584209934 ),
 .UNSPECIFIED. ) 
 CURVE ( )  GEOMETRIC_REPRESENTATION_ITEM ( )  RATIONAL_B_SPLINE_CURVE ( ( 1.000000000000000000, 0.9655421889976167904, 0.9655421889976167904, 1.000000000000000000 ) ) 
 REPRESENTATION_ITEM ( '' )  );
#93521 = EDGE_CURVE ( 'NONE', #109101, #13629, #56319, .T. ) ;
#93522 = CARTESIAN_POINT ( 'NONE',  ( 19.13035349170000288, 1454.816283974190128, 206.3418420143889875 ) ) ;
#93523 = CARTESIAN_POINT ( 'NONE',  ( -7.826634146540749626, 1363.535366961594946, 210.6218459617142003 ) ) ;
#93524 = CARTESIAN_POINT ( 'NONE',  ( -7.515867157249999764, 1494.783219423989976, 200.6183447482190161 ) ) ;
#93525 = DIRECTION ( 'NONE',  ( 0.9999982561604894293, 0.0004617740651251722099, 0.001809541569896410676 ) ) ;
#93526 = CARTESIAN_POINT ( 'NONE',  ( 14.72576938353500076, 1512.123542805230272, 196.9321265835669976 ) ) ;
#93527 = CARTESIAN_POINT ( 'NONE',  ( 19.05403812430366628, 1437.962009608390417, 213.1328251454357314 ) ) ;
#93528 = CARTESIAN_POINT ( 'NONE',  ( 9079.130222195200986, 5181.793945261120825, 1985.491949542980137 ) ) ;
#93529 = CARTESIAN_POINT ( 'NONE',  ( -2.344512155952720001, 1516.526058380829909, 201.4130301786289863 ) ) ;
#93530 = DIRECTION ( 'NONE',  ( 0.000000000000000000, -1.000000000000000000, 0.000000000000000000 ) ) ;
#93531 = CARTESIAN_POINT ( 'NONE',  ( 12.45610846519999981, 1519.913060387329779, 228.8821925242980058 ) ) ;
#93532 = CARTESIAN_POINT ( 'NONE',  ( -29.00779973304124582, 1526.382868172864164, 217.2942086403127178 ) ) ;
#93533 = CARTESIAN_POINT ( 'NONE',  ( -4.624736897314999595, 1516.994127245590107, 206.2540423059970180 ) ) ;
#93534 = CARTESIAN_POINT ( 'NONE',  ( 3.667960006519999983, 1446.440575811169992, 162.7182762402979961 ) ) ;
#93535 = CARTESIAN_POINT ( 'NONE',  ( -2.500000000000000000, 1433.766566658040119, 157.5373253330980106 ) ) ;
#93536 = CARTESIAN_POINT ( 'NONE',  ( -2.443866463060000438, 1496.089559380390028, 197.4171228521990145 ) ) ;
#93538 = VERTEX_POINT ( 'NONE', #28551 ) ;
#93537 = CARTESIAN_POINT ( 'NONE',  ( -68.43502141645350889, 1379.747127445309843, 280.0327720878970013 ) ) ;
#93539 = DIRECTION ( 'NONE',  ( 0.9942586961433749204, 0.000000000000000000, -0.1070030146457375819 ) ) ;
#93540 = ORIENTED_EDGE ( 'NONE', *, *, #29533, .T. ) ;
#93541 = DIRECTION ( 'NONE',  ( 0.9455185755993178454, 0.000000000000000000, -0.3255681544571537578 ) ) ;
#93542 = CARTESIAN_POINT ( 'NONE',  ( -22.97761739119999902, 1449.791915370539982, 200.0590113766180025 ) ) ;
#93544 = CARTESIAN_POINT ( 'NONE',  ( 17.36313619760800009, 1410.599962583540218, 192.4802441439230165 ) ) ;
#93543 = CARTESIAN_POINT ( 'NONE',  ( -11.24352777690759808, 1426.459969836569826, 108.4497583346609986 ) ) ;
#93545 = CARTESIAN_POINT ( 'NONE',  ( 3.462620818104999998, 1516.938330505699923, 211.6001527901769919 ) ) ;
#93546 = CARTESIAN_POINT ( 'NONE',  ( 29.52087390520885890, 1510.054509514609435, 214.7123836248202338 ) ) ;
#93547 = CARTESIAN_POINT ( 'NONE',  ( 1.228114002177200126, 1450.757138880049979, 181.5372592238319953 ) ) ;
#93548 =( NAMED_UNIT ( * ) SI_UNIT ( $, .STERADIAN. ) SOLID_ANGLE_UNIT ( ) );
#93549 = CARTESIAN_POINT ( 'NONE',  ( -12.32917350377740107, 1378.362683362840016, 209.4170945134390251 ) ) ;
#93550 = CARTESIAN_POINT ( 'NONE',  ( 12.57213386914980013, 1501.053060317580048, 211.0179505362860084 ) ) ;
#93551 = ITEM_DEFINED_TRANSFORMATION ( 'NONE', 'NONE', #3932,  #21632 ) ;
#93552 = CARTESIAN_POINT ( 'NONE',  ( 3.586875048626919860, 1508.551704408389924, 213.8556843534749987 ) ) ;
#93553 = CARTESIAN_POINT ( 'NONE',  ( -37.59663830446049815, 1438.304367445970001, 136.5843146558879937 ) ) ;
#93554 = EDGE_LOOP ( 'NONE', ( #24707, #50358, #84336, #86290, #46158 ) ) ;
#93555 = CARTESIAN_POINT ( 'NONE',  ( 10.63633553050959968, 1397.322975409730134, 200.4736743436469908 ) ) ;
#93556 = CARTESIAN_POINT ( 'NONE',  ( 9.249044665192510450, 1461.483507358830138, 206.1780078038019894 ) ) ;
#93557 = CARTESIAN_POINT ( 'NONE',  ( -18.44235347220000065, 1458.914805433830225, 227.7103923031980059 ) ) ;
#93558 = EDGE_LOOP ( 'NONE', ( #57947, #65786, #63641, #57935 ) ) ;
#93559 = ORIENTED_EDGE ( 'NONE', *, *, #10545, .T. ) ;
#93560 = DIRECTION ( 'NONE',  ( 0.7074300732568278294, -0.02470400251969398497, 0.7063514732138287400 ) ) ;
#93561 = CARTESIAN_POINT ( 'NONE',  ( -6.446325850290750559, 1432.345402019870107, 154.6647260408460056 ) ) ;
#93562 = CARTESIAN_POINT ( 'NONE',  ( -14.27857828532780182, 1380.308034680090032, 210.1943914574769963 ) ) ;
#93563 = CARTESIAN_POINT ( 'NONE',  ( -14.16968073959050045, 1507.983981868130059, 209.4049785662649867 ) ) ;
#93564 = CARTESIAN_POINT ( 'NONE',  ( 4.015749066599999750, 1515.588778490289997, 209.8749815410619988 ) ) ;
#93565 = CARTESIAN_POINT ( 'NONE',  ( 0.000000000000000000, 1512.187213306747481, 209.1218459616979999 ) ) ;
#93566 = CARTESIAN_POINT ( 'NONE',  ( -3.218186458279999940, 1461.193909496529841, 234.7217908393980110 ) ) ;
#93567 = PLANE ( 'NONE',  #9960 ) ;
#93568 = CARTESIAN_POINT ( 'NONE',  ( 9.657865277128729886, 1451.546502117730142, 208.2092904370149995 ) ) ;
#93569 = CARTESIAN_POINT ( 'NONE',  ( 16.90742456144603523, 1442.831169986190389, 162.4348202098863396 ) ) ;
#93570 = CARTESIAN_POINT ( 'NONE',  ( -103.8531838164470003, 1384.886124027839969, 296.8068726812870182 ) ) ;
#93571 = ORIENTED_EDGE ( 'NONE', *, *, #23472, .T. ) ;
#93572 = CARTESIAN_POINT ( 'NONE',  ( -7.329925260535000042, 1516.833976295079992, 201.4049670291269933 ) ) ;
#93573 = CARTESIAN_POINT ( 'NONE',  ( -6.944466780504999548, 1516.939530130779985, 209.1331108864249870 ) ) ;
#93574 = ORIENTED_EDGE ( 'NONE', *, *, #100590, .F. ) ;
#93575 = DIRECTION ( 'NONE',  ( 0.000000000000000000, -1.000000000000000000, -0.000000000000000000 ) ) ;
#93576 = CARTESIAN_POINT ( 'NONE',  ( 4.982648642978618980, 1511.399506464539627, 217.6390045414088092 ) ) ;
#93577 = ORIENTED_EDGE ( 'NONE', *, *, #44085, .F. ) ;
#93578 = CARTESIAN_POINT ( 'NONE',  ( -14.44947381900000138, 1416.568813549730066, 221.3833631277979919 ) ) ;
#93579 = CARTESIAN_POINT ( 'NONE',  ( 5.215161240205300253, 1429.990180876930253, 217.0496817771059739 ) ) ;
#93580 = CARTESIAN_POINT ( 'NONE',  ( 21.92333112166549469, 1524.538969332612623, 233.6740449069407077 ) ) ;
#93581 = CARTESIAN_POINT ( 'NONE',  ( -7.675557469593909943, 1490.010120624091769, 216.9302191894742293 ) ) ;
#93582 = CARTESIAN_POINT ( 'NONE',  ( -4.629727834550000587, 1424.354173624029954, 185.7675860119980200 ) ) ;
#93583 = CARTESIAN_POINT ( 'NONE',  ( -7.667845439150741349, 1446.704503592666470, 154.1274023243013005 ) ) ;
#93584 = CARTESIAN_POINT ( 'NONE',  ( -1.317811661047103788, 1517.151704408390060, 194.7136484256038500 ) ) ;
#93585 = CARTESIAN_POINT ( 'NONE',  ( 5.755589866880000294, 1494.343251907090007, 219.1208360334990175 ) ) ;
#93586 = CARTESIAN_POINT ( 'NONE',  ( -58.13411997410000254, 1379.718485381059963, 257.1571189129589925 ) ) ;
#93587 = CIRCLE ( 'NONE', #59651, 2.000000000000001776 ) ;
#93588 = CARTESIAN_POINT ( 'NONE',  ( -17.27619074209999894, 1507.625766698130064, 224.2558816620979769 ) ) ;
#93590 = CARTESIAN_POINT ( 'NONE',  ( 6.502040414733439633, 1467.454815019450052, 200.0748247799739943 ) ) ;
#93589 = CARTESIAN_POINT ( 'NONE',  ( 17.96268052179999941, 1457.880256331229930, 230.1796192676980013 ) ) ;
#93591 = CARTESIAN_POINT ( 'NONE',  ( -4.863986520837263683, 1423.459995654392742, 184.6347918575768858 ) ) ;
#93592 = CARTESIAN_POINT ( 'NONE',  ( -2.499957339907119991, 1419.383080839190143, 144.1003724646560045 ) ) ;
#93593 = ORIENTED_EDGE ( 'NONE', *, *, #100899, .F. ) ;
#93594 = CARTESIAN_POINT ( 'NONE',  ( 18.19680845026800142, 1424.503018947390046, 223.8103149804830139 ) ) ;
#93595 = CARTESIAN_POINT ( 'NONE',  ( -21.35000886514797003, 1525.163527997505071, 234.4063825837820048 ) ) ;
#93596 = CARTESIAN_POINT ( 'NONE',  ( -2.901263397339155503, 1484.476379004488081, 183.2956404250009541 ) ) ;
#93597 = CARTESIAN_POINT ( 'NONE',  ( -14.15287909329999927, 1415.677402202029953, 214.2967794726189936 ) ) ;
#93599 = VERTEX_POINT ( 'NONE', #63828 ) ;
#93598 = CARTESIAN_POINT ( 'NONE',  ( -11.26962181946710118, 1500.379234792439775, 210.9259952136519871 ) ) ;
#93600 = CARTESIAN_POINT ( 'NONE',  ( 1.116994350369999944, 1471.309462467129833, 187.7634697624980049 ) ) ;
#93601 = CARTESIAN_POINT ( 'NONE',  ( -2.152267782280000041, 1508.551704408389924, 220.2796779675990138 ) ) ;
#93602 = CARTESIAN_POINT ( 'NONE',  ( -11.78791146169999848, 1427.317704561630080, 147.8403236071979734 ) ) ;
#93603 = CARTESIAN_POINT ( 'NONE',  ( -22.75273496409560181, 1523.382868172864164, 234.5707981297189519 ) ) ;
#93604 = CARTESIAN_POINT ( 'NONE',  ( 3.150079082345019987, 1446.276749673359973, 199.4986788256669854 ) ) ;
#93605 = CARTESIAN_POINT ( 'NONE',  ( 14.44412038922260066, 1509.548839689010038, 235.4430145295710020 ) ) ;
#93606 = DIRECTION ( 'NONE',  ( -9.341989762165448955E-47, 1.000000000000000000, -1.836970198721029688E-16 ) ) ;
#93607 = CARTESIAN_POINT ( 'NONE',  ( -2.482344662330000062, 1440.444625599219989, 150.5580151863979950 ) ) ;
#93609 = CARTESIAN_POINT ( 'NONE',  ( -11.82004774745709952, 1482.260572698100077, 207.7363177859789971 ) ) ;
#93608 = CARTESIAN_POINT ( 'NONE',  ( -21.80579869879999677, 1495.368972219230045, 225.4358925196980010 ) ) ;
#93610 = CARTESIAN_POINT ( 'NONE',  ( -18.18664760840000127, 1466.015845117190111, 218.0276224371390015 ) ) ;
#93611 = EDGE_LOOP ( 'NONE', ( #17424, #81862, #58147, #84373, #39150, #1730, #39363, #62082, #61650, #90536 ) ) ;
#93612 = CARTESIAN_POINT ( 'NONE',  ( -6.949265684145000677, 1517.089216728169959, 205.6689289091970068 ) ) ;
#93613 = CARTESIAN_POINT ( 'NONE',  ( 23.55040952570000101, 1411.064796383629982, 269.0842170185980535 ) ) ;
#93614 = CARTESIAN_POINT ( 'NONE',  ( 0.8662106067031465351, 1465.087948376955410, 238.0466371020243059 ) ) ;
#93615 = CARTESIAN_POINT ( 'NONE',  ( 24.17852980030000154, 1469.149352981230095, 201.1913038658580035 ) ) ;
#93616 = ADVANCED_FACE ( 'NONE', ( #2281 ), #104649, .T. ) ;
#93617 = CARTESIAN_POINT ( 'NONE',  ( 0.05134268663526449922, 1508.133705146910188, 237.5625132777319948 ) ) ;
#93618 = DIRECTION ( 'NONE',  ( 0.000000000000000000, 0.000000000000000000, 1.000000000000000000 ) ) ;
#93619 = CARTESIAN_POINT ( 'NONE',  ( -1.370024040769999951, 1450.924184932629942, 183.2893338627980029 ) ) ;
#93620 = CARTESIAN_POINT ( 'NONE',  ( 17.41280537782821369, 1458.364529780870271, 230.6041477805117665 ) ) ;
#93621 = CARTESIAN_POINT ( 'NONE',  ( -15.00614681839999953, 1416.220781585230043, 205.5855558466790001 ) ) ;
#93622 = CARTESIAN_POINT ( 'NONE',  ( -13.74969930740000024, 1443.369189997270041, 188.1932585784979892 ) ) ;
#93623 = EDGE_CURVE ( 'NONE', #41956, #44860, #46881, .T. ) ;
#93624 = CARTESIAN_POINT ( 'NONE',  ( -21.61512607259999896, 1497.713060387329961, 209.1218459618889938 ) ) ;
#93625 = CARTESIAN_POINT ( 'NONE',  ( -16.41393203050009220, 1419.676706660666696, 209.5083631726842839 ) ) ;
#93626 = CARTESIAN_POINT ( 'NONE',  ( 1.861700016370000164E-09, 1407.650947845630071, 270.1377426662980383 ) ) ;
#93627 = ORIENTED_EDGE ( 'NONE', *, *, #2824, .F. ) ;
#93628 = CARTESIAN_POINT ( 'NONE',  ( 1.466447836938430171, 1489.784574236090066, 181.8690865221339834 ) ) ;
#93629 = CARTESIAN_POINT ( 'NONE',  ( -12.69333308194260113, 1409.356321345949937, 201.2342037859239952 ) ) ;
#93630 = FACE_OUTER_BOUND ( 'NONE', #72796, .T. ) ;
#93631 = CARTESIAN_POINT ( 'NONE',  ( -12.02612939183720009, 1377.659857216290220, 211.7505375168460091 ) ) ;
#93632 = CARTESIAN_POINT ( 'NONE',  ( -18.25597770279999921, 1472.821217557230057, 269.1701651182979731 ) ) ;
#93633 = CARTESIAN_POINT ( 'NONE',  ( 30.24842679174819082, 1524.082582765195411, 195.7700791222141845 ) ) ;
#93634 = CARTESIAN_POINT ( 'NONE',  ( -14.39972043569755655, 1514.266809408770769, 192.6372960624397308 ) ) ;
#93635 = CARTESIAN_POINT ( 'NONE',  ( 18.15041076583969826, 1424.504405689699979, 223.8575062216150116 ) ) ;
#93636 = CARTESIAN_POINT ( 'NONE',  ( -67.43312117150000518, 1384.669984925169956, 291.9984064737109861 ) ) ;
#93637 = CARTESIAN_POINT ( 'NONE',  ( -24.94794202207559763, 1384.959512558119968, 203.2447943497110145 ) ) ;
#93638 = CARTESIAN_POINT ( 'NONE',  ( 11.44693299035330192, 1415.124054205850143, 222.7699361616149929 ) ) ;
#93639 = CARTESIAN_POINT ( 'NONE',  ( 3.439855069772169809E-11, 1452.913060387330006, 150.8032249182200246 ) ) ;
#93640 = DIRECTION ( 'NONE',  ( 0.001027118858036968341, 0.9999913661844073154, 0.004026485253184815781 ) ) ;
#93641 = CARTESIAN_POINT ( 'NONE',  ( -14.35058941781813324, 1519.551704408389924, 193.9977807835901729 ) ) ;
#93642 = CARTESIAN_POINT ( 'NONE',  ( -22.04343844010000097, 1409.682834220629957, 204.9962922481880128 ) ) ;
#93643 = CARTESIAN_POINT ( 'NONE',  ( -10.84436532123444508, 1379.243588034859386, 203.2049456427220946 ) ) ;
#93644 = CARTESIAN_POINT ( 'NONE',  ( 3.848901911860000080, 1484.746040934790017, 219.9081948904990043 ) ) ;
#93645 = CARTESIAN_POINT ( 'NONE',  ( 4.009460067780000081, 1422.110854443290009, 194.2227175196989890 ) ) ;
#93646 = CARTESIAN_POINT ( 'NONE',  ( 2.927701378049999713E-15, 1442.756953654919926, 150.7628527808980152 ) ) ;
#93647 = CARTESIAN_POINT ( 'NONE',  ( -8.468273497790530513, 1438.274789257269958, 228.4488543761889900 ) ) ;
#93648 = CARTESIAN_POINT ( 'NONE',  ( 16.51370628721609179, 1525.137881624894590, 181.0453264504938602 ) ) ;
#93649 = CARTESIAN_POINT ( 'NONE',  ( -21.26810766748090131, 1485.919195119950018, 201.7808564924430073 ) ) ;
#93650 =( BOUNDED_SURFACE ( )  B_SPLINE_SURFACE ( 4, 2, ( 
 ( #25810, #74602, #33667 ),
 ( #93569, #16844, #33123 ),
 ( #107, #51596, #94129 ),
 ( #59459, #42638, #75699 ),
 ( #93027, #40426, #49942 ) ),
 .UNSPECIFIED., .F., .F., .F. ) 
 B_SPLINE_SURFACE_WITH_KNOTS ( ( 5, 5 ),
 ( 3, 3 ),
 ( 1.967616199060000071, 3.613988937050000239 ),
 ( 5.300753508050029872, 6.148936695274129782 ),
 .UNSPECIFIED. ) 
 GEOMETRIC_REPRESENTATION_ITEM ( )  RATIONAL_B_SPLINE_SURFACE ( (
 ( 0.8627701935039280290, 0.8230940375028089617, 0.9542143464239759565),
 ( 0.8627701935039280290, 0.8230940375028089617, 0.9542143464239759565),
 ( 0.8627701935039280290, 0.8230940375028089617, 0.9542143464239759565),
 ( 0.8627701935039280290, 0.8230940375028089617, 0.9542143464239759565),
 ( 0.8627701935039280290, 0.8230940375028089617, 0.9542143464239759565) ) ) 
 REPRESENTATION_ITEM ( '' )  SURFACE ( )  );
#93652 = CARTESIAN_POINT ( 'NONE',  ( -12.47607414476330057, 1379.154200148260088, 210.8826634821560049 ) ) ;
#93651 = DIRECTION ( 'NONE',  ( 0.000000000000000000, 0.000000000000000000, -1.000000000000000000 ) ) ;
#93653 = CARTESIAN_POINT ( 'NONE',  ( 11.71967320325980211, 1426.707059066819966, 142.9268082951259942 ) ) ;
#93654 = CARTESIAN_POINT ( 'NONE',  ( -3.171072485709999889, 1451.871858332230204, 182.7750508701979868 ) ) ;
#93655 = CARTESIAN_POINT ( 'NONE',  ( -6.754078978114156584, 1512.913060387330006, 184.4732361498326156 ) ) ;
#93656 = CARTESIAN_POINT ( 'NONE',  ( 7.801285059986189374, 1449.017548237110077, 202.3630618800679883 ) ) ;
#93657 = AXIS2_PLACEMENT_3D ( 'NONE', #69368, #96761, #88898 ) ;
#93658 = CARTESIAN_POINT ( 'NONE',  ( -17.01536243937009729, 1507.593738226439882, 224.5318899074820251 ) ) ;
#93659 = CARTESIAN_POINT ( 'NONE',  ( 0.7376675027960020170, 1517.104497701820037, 203.3349981924270082 ) ) ;
#93660 = CARTESIAN_POINT ( 'NONE',  ( -8.492040095572983560, 1398.165184799730923, 218.9680983094823148 ) ) ;
#93661 = CARTESIAN_POINT ( 'NONE',  ( -3.406513463655362894, 1440.721058893708914, 156.8280215876527848 ) ) ;
#93662 = DIRECTION ( 'NONE',  ( -0.9455185755993178454, 0.000000000000000000, 0.3255681544571539243 ) ) ;
#93663 = FACE_OUTER_BOUND ( 'NONE', #28209, .T. ) ;
#93664 = CARTESIAN_POINT ( 'NONE',  ( 10.16310853745439857, 1503.066809769739848, 217.0134810410080206 ) ) ;
#93665 = AXIS2_PLACEMENT_3D ( 'NONE', #63215, #37979, #1633 ) ;
#93667 = VERTEX_POINT ( 'NONE', #30744 ) ;
#93666 = CARTESIAN_POINT ( 'NONE',  ( -56.90245408136139815, 1379.713870185199994, 259.4980311760010068 ) ) ;
#93668 = EDGE_LOOP ( 'NONE', ( #20848, #42603, #27595, #52142, #20162 ) ) ;
#93669 = CARTESIAN_POINT ( 'NONE',  ( 11.97438681890969825, 1433.814205175160168, 150.4339170446530147 ) ) ;
#93670 = CARTESIAN_POINT ( 'NONE',  ( -12.55642688110000016, 1397.977875496030038, 212.9353772083979948 ) ) ;
#93671 = VERTEX_POINT ( 'NONE', #73870 ) ;
#93672 = CARTESIAN_POINT ( 'NONE',  ( -12.71559489689999900, 1467.455103516190093, 192.9444858715990279 ) ) ;
#93673 = CARTESIAN_POINT ( 'NONE',  ( -109.3075263750000090, 1384.927480430210153, 311.2646524412589315 ) ) ;
#93674 = CARTESIAN_POINT ( 'NONE',  ( 4.077241479695380200, 1515.224507089990084, 205.5390440451549807 ) ) ;
#93676 = CARTESIAN_POINT ( 'NONE',  ( -13.85731421134180152, 1508.722096842320070, 183.9202016419540087 ) ) ;
#93675 = CARTESIAN_POINT ( 'NONE',  ( -7.848979634317430509, 1517.151704408390060, 202.2988320601959913 ) ) ;
#93677 = DIRECTION ( 'NONE',  ( -0.000000000000000000, -1.000000000000000000, -0.000000000000000000 ) ) ;
#93678 = CARTESIAN_POINT ( 'NONE',  ( 9.322640526599998978, 1468.697217342230033, 185.3328853447980009 ) ) ;
#93679 = CARTESIAN_POINT ( 'NONE',  ( -2.628012640819999746, 1414.971287085330005, 192.6484313466980041 ) ) ;
#93680 = CARTESIAN_POINT ( 'NONE',  ( -3.968827103576990201, 1519.551704408389924, 229.5396913781519856 ) ) ;
#93681 = B_SPLINE_CURVE_WITH_KNOTS ( 'NONE', 3,
 ( #28202, #3035, #2486, #70802, #97072, #54543, #11954, #80269, #3584, #71909 ),
 .UNSPECIFIED., .F., .F.,
 ( 4, 2, 2, 2, 4 ),
 ( 3.122502256758252770E-17, 0.0007406479101619058971, 0.001481295820323780569, 0.002221943730485655133, 0.002962591640647529913 ),
 .UNSPECIFIED. ) ;
#93682 = B_SPLINE_SURFACE_WITH_KNOTS ( 'NONE', 5, 1, ( 
 ( #24090, #58278 ),
 ( #84012, #41478 ),
 ( #109776, #58824 ),
 ( #33593, #79496 ),
 ( #54311, #96850 ),
 ( #43679, #63268 ),
 ( #88438, #103573 ),
 ( #62728, #87335 ),
 ( #77830, #104129 ) ),
 .UNSPECIFIED., .F., .F., .F.,
 ( 6, 3, 6 ),
 ( 2, 2 ),
 ( -8.704553073772529568E-10, 8.290775826610000010, 16.58943550237049891 ),
 ( 0.000000000000000000, 14.00000211182629961 ),
 .UNSPECIFIED. ) ;
#93683 = CARTESIAN_POINT ( 'NONE',  ( 5.579983761340000292, 1439.143574310590111, 210.6739328916289935 ) ) ;
#93684 = CARTESIAN_POINT ( 'NONE',  ( 14.30082345506829888, 1416.007771869970156, 197.0130041503479958 ) ) ;
#93685 = CARTESIAN_POINT ( 'NONE',  ( 11.86332839419999985, 1432.142273804659908, 149.9796868945980179 ) ) ;
#93686 = FACE_OUTER_BOUND ( 'NONE', #68647, .T. ) ;
#93687 = VERTEX_POINT ( 'NONE', #48678 ) ;
#93688 = CARTESIAN_POINT ( 'NONE',  ( 13.42930060380339974, 1434.933243636549832, 148.8496443608690072 ) ) ;
#93689 = ORIENTED_EDGE ( 'NONE', *, *, #308, .F. ) ;
#93690 = ORIENTED_EDGE ( 'NONE', *, *, #71836, .T. ) ;
#93691 = CARTESIAN_POINT ( 'NONE',  ( 13.51303151820626169, 1443.998943487957831, 169.3513894483426157 ) ) ;
#93692 = CARTESIAN_POINT ( 'NONE',  ( -4.353746609069999884, 1464.535296998829836, 236.7958744120979873 ) ) ;
#93693 = CARTESIAN_POINT ( 'NONE',  ( -7.030811903863808610, 1475.320784634834354, 201.5754146800807689 ) ) ;
#93694 = CARTESIAN_POINT ( 'NONE',  ( 2.485217193935000068, 1516.534320418310244, 216.8308781079170160 ) ) ;
#93695 = CARTESIAN_POINT ( 'NONE',  ( -8.335875861980486690, 1511.410071747324082, 213.5558459922955308 ) ) ;
#93696 = B_SPLINE_SURFACE_WITH_KNOTS ( 'NONE', 5, 5, ( 
 ( #32681, #24799, #5838, #82544, #83086, #65748 ),
 ( #99865, #66860, #23163, #67413, #100970, #109405 ),
 ( #14769, #24266, #75794, #49500, #39978, #33771 ),
 ( #6379, #109946, #83625, #57902, #58446, #92036 ),
 ( #84179, #74154, #6922, #108284, #33225, #67968 ),
 ( #41079, #92574, #50051, #101513, #42191, #14214 ),
 ( #31571, #66316, #59005, #93132, #57364, #16400 ),
 ( #50594, #84725, #76342, #102076, #25359, #32131 ),
 ( #100434, #90927, #48955, #40525, #74703, #108834 ) ),
 .UNSPECIFIED., .F., .F., .F.,
 ( 6, 3, 6 ),
 ( 6, 6 ),
 ( 1.126366143519770047, 3.287928953729999826, 6.228946179000230288 ),
 ( 0.000000000000000000, 2.000010957310230264 ),
 .UNSPECIFIED. ) ;
#93697 =( GEOMETRIC_REPRESENTATION_CONTEXT ( 3 ) GLOBAL_UNCERTAINTY_ASSIGNED_CONTEXT ( ( #95011 ) ) GLOBAL_UNIT_ASSIGNED_CONTEXT ( ( #5435, #16014, #35464 ) ) REPRESENTATION_CONTEXT ( 'NONE', 'WORKASPACE' ) );
#93698 = CARTESIAN_POINT ( 'NONE',  ( -19.07453550630248174, 1442.252090472558848, 210.5365316514335916 ) ) ;
#93699 = CARTESIAN_POINT ( 'NONE',  ( 2.500000000000000000, 1448.365115610690054, 162.8856519708890005 ) ) ;
#93700 = CARTESIAN_POINT ( 'NONE',  ( -11.54050778900000118, 1375.649725832029844, 207.7392432702390295 ) ) ;
#93701 = ADVANCED_FACE ( 'NONE', ( #57637 ), #52794, .T. ) ;
#93702 = ORIENTED_EDGE ( 'NONE', *, *, #104085, .T. ) ;
#93703 = CARTESIAN_POINT ( 'NONE',  ( 4.608417506514999928, 1516.691389976299888, 206.6316000176769876 ) ) ;
#93704 = ORIENTED_EDGE ( 'NONE', *, *, #84481, .F. ) ;
#93705 = DIRECTION ( 'NONE',  ( -1.000000000000000000, 0.000000000000000000, 0.000000000000000000 ) ) ;
#93706 = CARTESIAN_POINT ( 'NONE',  ( 19.53786426059039982, 1512.187213306747481, 236.7197124308265188 ) ) ;
#93708 = EDGE_CURVE ( 'NONE', #80584, #86711, #51979, .T. ) ;
#93707 = CARTESIAN_POINT ( 'NONE',  ( 5.451195050909999503E-14, 1410.389826760030019, 269.3346704430979912 ) ) ;
#93709 = CARTESIAN_POINT ( 'NONE',  ( 7.770779652545000360, 1514.639648807489948, 215.0467008345069928 ) ) ;
#93711 = ORIENTED_EDGE ( 'NONE', *, *, #24808, .T. ) ;
#93710 = CARTESIAN_POINT ( 'NONE',  ( -0.2892576526283990312, 1415.943166310999914, 227.2001892735609943 ) ) ;
#93712 = CARTESIAN_POINT ( 'NONE',  ( 19.54815321029999708, 1426.815511739029944, 223.9912215281979968 ) ) ;
#93713 = CARTESIAN_POINT ( 'NONE',  ( -14.60203837859040021, 1508.551704408389924, 210.3568941631429823 ) ) ;
#93714 = CARTESIAN_POINT ( 'NONE',  ( -11.60004869885203860, 1428.965959225140750, 137.0999999980979851 ) ) ;
#93715 = CARTESIAN_POINT ( 'NONE',  ( 8.723134474349999223, 1451.781317889190177, 212.2855316608589931 ) ) ;
#93716 = CARTESIAN_POINT ( 'NONE',  ( 21.61625474793712343, 1526.178928173327904, 183.7635344381618268 ) ) ;
#93717 = B_SPLINE_SURFACE_WITH_KNOTS ( 'NONE', 5, 1, ( 
 ( #6365, #7463 ),
 ( #5825, #67399 ),
 ( #83610, #108271 ),
 ( #24252, #90915 ),
 ( #107722, #14199 ),
 ( #23704, #58432 ),
 ( #108822, #47820 ),
 ( #32668, #75241 ),
 ( #65734, #41625 ),
 ( #92560, #15830 ),
 ( #100421, #66846 ),
 ( #22025, #56777 ),
 ( #39415, #31557 ),
 ( #39964, #66303 ),
 ( #50034, #41064 ),
 ( #100956, #48942 ),
 ( #5262, #40512 ),
 ( #56223, #99299 ),
 ( #109391, #74140 ),
 ( #48386, #81955 ),
 ( #57888, #84162 ),
 ( #82528, #23148 ),
 ( #22573, #65187 ),
 ( #75779, #109932 ),
 ( #92024, #90354 ),
 ( #33210, #49487 ),
 ( #83073, #73592 ),
 ( #99853, #31007 ),
 ( #57351, #91476 ),
 ( #32118, #15295 ),
 ( #43290, #10221 ),
 ( #86377, #1855 ),
 ( #16932, #86930 ),
 ( #26460, #738 ),
 ( #34321, #27035 ),
 ( #85825, #94213 ),
 ( #35990, #25899 ),
 ( #84710, #94779 ),
 ( #93649, #77980 ),
 ( #43835, #8557 ),
 ( #44399, #77438 ),
 ( #9663, #1288 ),
 ( #101497, #9123 ),
 ( #78541, #34870 ),
 ( #35427, #17488 ),
 ( #58987, #103159 ),
 ( #69058, #51686 ),
 ( #103736, #24785 ),
 ( #51134, #60655 ),
 ( #18056, #197 ),
 ( #69614, #59537 ) ),
 .UNSPECIFIED., .F., .F., .F.,
 ( 6, 3, 3, 3, 3, 3, 3, 3, 3, 3, 3, 3, 3, 3, 3, 3, 6 ),
 ( 2, 2 ),
 ( 0.000000000000000000, 28.69702819429999963, 61.04778752440000034, 93.62768910810000023, 123.7336603250000024, 156.1762685979999787, 187.3272846180000215, 220.4669312460000015, 237.3878297990000021, 254.2938300590000154, 289.2398204710000300, 325.3030936050000150, 360.8626869010000178, 395.8828220460000011, 432.6128460950000090, 468.8934854820000169, 502.1482307969999965 ),
 ( -1.158612088544819935E-09, 2.001768489946770035 ),
 .UNSPECIFIED. ) ;
#93718 = CARTESIAN_POINT ( 'NONE',  ( 3.457266605394999637, 1516.691414181030041, 214.8945738789770132 ) ) ;
#93719 = CARTESIAN_POINT ( 'NONE',  ( -2.800144927338689804, 1429.031935871130145, 200.1802602962729907 ) ) ;
#93720 = CARTESIAN_POINT ( 'NONE',  ( -20.58397420629999885, 1508.353852242129960, 189.9891704665979830 ) ) ;
#93721 = CARTESIAN_POINT ( 'NONE',  ( 6.141399090249540116, 1509.034509426269778, 216.6345626869079979 ) ) ;
#93722 = CARTESIAN_POINT ( 'NONE',  ( 4.043990307595000111, 1516.983612918759945, 211.6010928179370012 ) ) ;
#93723 = CARTESIAN_POINT ( 'NONE',  ( -11.87328627558470018, 1482.014094172719979, 208.6022272904490080 ) ) ;
#93724 = CARTESIAN_POINT ( 'NONE',  ( -18.09477754449768838, 1486.177057533957395, 188.5520870720846176 ) ) ;
#93726 = ORIENTED_EDGE ( 'NONE', *, *, #46392, .F. ) ;
#93725 = CARTESIAN_POINT ( 'NONE',  ( -67.09670646059998944, 1386.610685867510028, 292.1437283079590088 ) ) ;
#93727 = CARTESIAN_POINT ( 'NONE',  ( -60.62638870901079713, 1385.063061064700150, 282.0167569604489586 ) ) ;
#93728 = CARTESIAN_POINT ( 'NONE',  ( 31.20802388370000102, 1451.456139920330088, 248.1710554673980198 ) ) ;
#93729 = CARTESIAN_POINT ( 'NONE',  ( 10.92886027419739925, 1490.469936390880093, 210.0530976118369892 ) ) ;
#93730 = CARTESIAN_POINT ( 'NONE',  ( 9.638115859575000499, 1516.551704408390151, 214.4931927712770232 ) ) ;
#93731 = CARTESIAN_POINT ( 'NONE',  ( -7.140946062075090417, 1508.970007424190044, 236.7165944161500022 ) ) ;
#93732 = CARTESIAN_POINT ( 'NONE',  ( -23.29298009400000069, 1448.643654431140021, 216.8814030764980032 ) ) ;
#93733 = CARTESIAN_POINT ( 'NONE',  ( 12.18971934853500194, 1512.123542805230272, 223.8476153537669973 ) ) ;
#93734 = AXIS2_PLACEMENT_3D ( 'NONE', #10441, #25564, #1505 ) ;
#93736 = CARTESIAN_POINT ( 'NONE',  ( 19.47214361940000060, 1455.728784677129852, 226.5116728881979782 ) ) ;
#93735 = CARTESIAN_POINT ( 'NONE',  ( -4.035536263215000474, 1517.086065052259983, 216.8453260496270047 ) ) ;
#93737 = DIRECTION ( 'NONE',  ( -0.02616798426500960631, -0.9993150019883682011, -0.02616798426500960631 ) ) ;
#93738 = CARTESIAN_POINT ( 'NONE',  ( -109.0056894283609950, 1382.294289550630083, 310.8401910643229940 ) ) ;
#93739 = ORIENTED_EDGE ( 'NONE', *, *, #74320, .F. ) ;
#93740 = CARTESIAN_POINT ( 'NONE',  ( -4.037378294184999383, 1516.688761843659904, 202.5730239910470232 ) ) ;
#93741 = CARTESIAN_POINT ( 'NONE',  ( 2.779481089730000180E-10, 1406.506670174130022, 269.4986873273979882 ) ) ;
#93742 = CARTESIAN_POINT ( 'NONE',  ( 27.77037800339999762, 1508.603156330129877, 207.7292936111279857 ) ) ;
#93743 = AXIS2_PLACEMENT_3D ( 'NONE', #90227, #20272, #14070 ) ;
#93744 = CARTESIAN_POINT ( 'NONE',  ( 24.61702284729999946, 1442.198266432479841, 213.4925807370779864 ) ) ;
#93745 = CARTESIAN_POINT ( 'NONE',  ( -34.61172972909704981, 1523.342713519622976, 218.2049768989091376 ) ) ;
#93746 = LINE ( 'NONE', #75341, #10896 ) ;
#93747 = CARTESIAN_POINT ( 'NONE',  ( 26.35137190500821092, 1450.746515883685333, 136.5686529940089713 ) ) ;
#93748 = DIRECTION ( 'NONE',  ( 0.8775825618903732028, -4.965288137873349002E-32, 0.4794255386042021172 ) ) ;
#93749 = CARTESIAN_POINT ( 'NONE',  ( 26.81567905896629966, 1435.593051660359833, 136.1631590423840237 ) ) ;
#93750 = CARTESIAN_POINT ( 'NONE',  ( 40.16194930853830414, 1445.050329818410091, 136.9555904954470122 ) ) ;
#93751 = DIRECTION ( 'NONE',  ( 0.7067700363771036720, 0.03085824620770448445, 0.7067700363771035610 ) ) ;
#93752 = CARTESIAN_POINT ( 'NONE',  ( -109.1450416020000063, 1385.242479493820156, 297.1468691531589457 ) ) ;
#93753 = CARTESIAN_POINT ( 'NONE',  ( -17.38342248510000232, 1410.833857452530083, 225.7816926272979856 ) ) ;
#93754 = CARTESIAN_POINT ( 'NONE',  ( 5.544571539851137487, 1465.562015094885737, 218.7011515308894047 ) ) ;
#93755 = CARTESIAN_POINT ( 'NONE',  ( -21.59934095315038860, 1525.137881624895044, 184.7402563171935128 ) ) ;
#93756 = CARTESIAN_POINT ( 'NONE',  ( 2.923521462801879967, 1410.394928839790055, 231.6309329194170061 ) ) ;
#93757 = VERTEX_POINT ( 'NONE', #110212 ) ;
#93758 = DIRECTION ( 'NONE',  ( 0.000000000000000000, -1.000000000000000000, 0.000000000000000000 ) ) ;
#93759 = CARTESIAN_POINT ( 'NONE',  ( 2.660639375520162719, 1425.975332079923646, 184.4015672484581785 ) ) ;
#93760 = CARTESIAN_POINT ( 'NONE',  ( -3.822989278826689930, 1508.729442775010057, 213.6787569762799990 ) ) ;
#93761 = CARTESIAN_POINT ( 'NONE',  ( 0.000000000000000000, 1515.551704408389924, 209.1218459616989946 ) ) ;
#93762 = CARTESIAN_POINT ( 'NONE',  ( 10.85919384568302526, 1424.796381347971874, 138.1955824056398399 ) ) ;
#93764 = DIRECTION ( 'NONE',  ( 1.836970198721029688E-16, 1.000000000000000000, 0.000000000000000000 ) ) ;
#93763 = CARTESIAN_POINT ( 'NONE',  ( 12.02501080200000061, 1501.456225530590018, 211.6043546659689980 ) ) ;
#93765 = CARTESIAN_POINT ( 'NONE',  ( -28.30178298279999893, 1508.659383665829864, 209.2808554955639977 ) ) ;
#93766 = CARTESIAN_POINT ( 'NONE',  ( 7.465427998170000023, 1423.561403314650079, 212.9273434364789921 ) ) ;
#93767 = CARTESIAN_POINT ( 'NONE',  ( 1.569161254424999985, 1517.051704408389924, 201.3992656178269840 ) ) ;
#93768 = CARTESIAN_POINT ( 'NONE',  ( -11.51163193560000053, 1413.913060387330006, 206.7812028963490150 ) ) ;
#93769 = CARTESIAN_POINT ( 'NONE',  ( -38.60438541162910298, 1444.259423794019995, 137.1474472167009822 ) ) ;
#93770 = CARTESIAN_POINT ( 'NONE',  ( -18.10358820054819873, 1416.830086716310007, 209.2067746984330086 ) ) ;
#93771 = CARTESIAN_POINT ( 'NONE',  ( 25.87716807187569756, 1435.480308988900106, 135.9284055610729922 ) ) ;
#93772 = B_SPLINE_CURVE_WITH_KNOTS ( 'NONE', 3,
 ( #24632, #76175, #84016, #50442, #7857, #33597, #25194, #34168, #68354, #62162, #79499, #11733, #63272, #54314, #46460, #36376, #96288, #2806, #28533, #18443, #27977, #10634, #19565, #44802, #87907, #78955, #105242, #97382, #70018, #37485, #53771, #61601, #29087, #105807, #11196, #36924, #71121, #86779, #20121, #71689, #12268, #80593, #3359, #104132, #44242, #35835, #88980, #45360, #3907, #70565, #88442, #62732, #20654, #87338, #38036, #96853, #106338, #29624, #72216, #10068, #78386, #45902, #27418, #1694, #63808, #53198, #52642, #54856, #95734, #18998, #80038, #2262, #104683, #31280, #39116, #64358, #40787, #65464, #99022, #73856, #6632, #4444, #31832, #49208, #81666, #21748, #47003, #107983, #108542, #39688, #74963, #82786, #23427, #73296, #109113, #82236, #83336, #22298, #99571, #32393, #57620, #66018, #97925, #4972, #55950, #81126, #22857, #100141, #57063, #21192, #6081, #91736, #107431, #55402, #5537, #89534, #12823, #30726, #91188, #64911, #56500, #14469, #30168, #15010 ),
 .UNSPECIFIED., .F., .F.,
 ( 4, 3, 3, 3, 3, 3, 3, 3, 3, 3, 3, 3, 3, 3, 3, 3, 3, 3, 3, 3, 3, 3, 3, 3, 3, 3, 3, 3, 3, 3, 3, 3, 3, 3, 3, 3, 3, 3, 3, 3, 3, 4 ),
 ( -74.85727727459999414, -74.48123371302079931, -73.19548303872750239, -71.89858627928869339, -70.59406779746200300, -69.27706090161748875, -67.95207998846730391, -66.61972111345330916, -65.28071632980000061, -65.07820501495520205, -63.73244012951310111, -62.38233361708310554, -61.03011531218779595, -59.61324830631710370, -58.26014992637010437, -56.90891767115380162, -55.56075881110690062, -54.17219345129359453, -52.83759983287470163, -51.51014382337439201, -50.19057675987170342, -48.87949243769620011, -47.57733876788930161, -46.28443321930000565, -45.15800308885260250, -43.85412093733170025, -42.53885251026929382, -41.21701627981990157, -39.88454573359799582, -38.54622334132480432, -37.20301750951840347, -35.85601880476590253, -34.50543421572560732, -33.15433547973400863, -31.80422057938690017, -30.45655169721700872, -29.11270829773580004, -27.77394855399130336, -26.44138195807519764, -25.11595400857649452, -23.80322223705459805, -22.49960185790659750 ),
 .UNSPECIFIED. ) ;
#93773 = CARTESIAN_POINT ( 'NONE',  ( -9.075617034181210130, 1396.229987919329915, 202.8041746642439875 ) ) ;
#93774 = ORIENTED_EDGE ( 'NONE', *, *, #29645, .T. ) ;
#93775 = VECTOR ( 'NONE', #67740, 1000.000000000000000 ) ;
#93776 = CARTESIAN_POINT ( 'NONE',  ( -24.02854066789229748, 1507.902906607559999, 222.3115874531950169 ) ) ;
#93777 = CARTESIAN_POINT ( 'NONE',  ( 21.87285660853828162, 1509.490619970689522, 226.7826239887661757 ) ) ;
#93778 = ORIENTED_EDGE ( 'NONE', *, *, #29046, .T. ) ;
#93779 = ORIENTED_EDGE ( 'NONE', *, *, #24912, .F. ) ;
#93780 = CARTESIAN_POINT ( 'NONE',  ( 3.044773427654349440, 1435.191935258749936, 227.3099679716739843 ) ) ;
#93781 = CARTESIAN_POINT ( 'NONE',  ( 7.142873439723720352, 1516.547309683342064, 206.8320615317442162 ) ) ;
#93783 = CARTESIAN_POINT ( 'NONE',  ( -11.10358245799999999, 1458.675538803330028, 216.3235414262480276 ) ) ;
#93782 = CARTESIAN_POINT ( 'NONE',  ( 10.04590426459999897, 1425.199081096129930, 97.30533624469789800 ) ) ;
#93784 = B_SPLINE_CURVE_WITH_KNOTS ( 'NONE', 3,
 ( #74690, #13632, #14755, #6908 ),
 .UNSPECIFIED., .F., .F.,
 ( 4, 4 ),
 ( 0.000000000000000000, 1.000000000000000000 ),
 .UNSPECIFIED. ) ;
#93785 = CARTESIAN_POINT ( 'NONE',  ( -20.55914306749999909, 1506.541454689430111, 190.4276830417979909 ) ) ;
#93786 = CARTESIAN_POINT ( 'NONE',  ( 4.259251705083289430, 1425.302291051229759, 185.3604417148609969 ) ) ;
#93787 = EDGE_CURVE ( 'NONE', #61056, #43369, #25673, .T. ) ;
#93788 = CARTESIAN_POINT ( 'NONE',  ( -25.65041448810000091, 1380.250345454750004, 213.2122020707489867 ) ) ;
#93789 = CARTESIAN_POINT ( 'NONE',  ( -2.559527845430900950, 1420.757063664457291, 185.5806755108912967 ) ) ;
#93790 = CARTESIAN_POINT ( 'NONE',  ( 7.717520428720000325, 1424.057070268800089, 212.3256381827789880 ) ) ;
#93791 = CARTESIAN_POINT ( 'NONE',  ( -17.11733429290000075, 1420.830776148560062, 201.6585816624789800 ) ) ;
#93792 = LINE ( 'NONE', #87075, #74860 ) ;
#93793 = CARTESIAN_POINT ( 'NONE',  ( 2.500000780830000213, 1448.894380426520001, 182.3534016871979873 ) ) ;
#93794 = B_SPLINE_SURFACE_WITH_KNOTS ( 'NONE', 5, 5, ( 
 ( #74769, #32201, #100502, #23781, #57969, #15381 ),
 ( #49570, #83698, #6994, #24337, #15921, #81852 ),
 ( #12458, #14092, #107067, #5155, #46640, #72389 ),
 ( #38206, #89167, #21924, #48281, #47721, #64543 ),
 ( #20844, #12991, #20295, #37663, #47174, #30352 ),
 ( #3540, #21380, #106518, #13535, #80774, #55589 ),
 ( #29261, #80222, #63995, #97572, #39864, #30902 ),
 ( #29807, #73483, #56119, #98661, #11914, #81302 ),
 ( #90253, #39312, #107619, #89713, #65080, #99195 ) ),
 .UNSPECIFIED., .F., .F., .F.,
 ( 6, 3, 6 ),
 ( 6, 6 ),
 ( -0.0001215403142825610000, 11.59601121190000050, 17.59296286301430001 ),
 ( -0.0001215403143104999955, 2.000000000000000000 ),
 .UNSPECIFIED. ) ;
#93795 = CARTESIAN_POINT ( 'NONE',  ( 7.877099145841899741, 1362.118768394163908, 210.6218459616987957 ) ) ;
#93796 = CARTESIAN_POINT ( 'NONE',  ( -28.29825159847881011, 1510.012726057827649, 199.1527708751072794 ) ) ;
#93798 = ORIENTED_EDGE ( 'NONE', *, *, #11217, .F. ) ;
#93797 = CARTESIAN_POINT ( 'NONE',  ( -1.719768424131510052E-09, 1416.259762861719992, 239.8605997301720265 ) ) ;
#93799 = ORIENTED_EDGE ( 'NONE', *, *, #96517, .T. ) ;
#93800 = CARTESIAN_POINT ( 'NONE',  ( -11.84918753543019854, 1431.164029985320212, 149.8564009815129907 ) ) ;
#93801 = CARTESIAN_POINT ( 'NONE',  ( 7.428892750695719194, 1510.947106981214347, 202.8329269027580324 ) ) ;
#93802 = CARTESIAN_POINT ( 'NONE',  ( -1.423698823499999877, 1472.030635481829904, 270.0714644396979907 ) ) ;
#93803 = CARTESIAN_POINT ( 'NONE',  ( 12.11072210459613885, 1433.924378751797121, 147.5235493649816192 ) ) ;
#93804 = CARTESIAN_POINT ( 'NONE',  ( -124.1837824924000557, 1366.350733876289723, 315.0056284496589001 ) ) ;
#93805 = CARTESIAN_POINT ( 'NONE',  ( 2.390047989666873818, 1526.069472839378705, 240.5369618407319763 ) ) ;
#93806 = CARTESIAN_POINT ( 'NONE',  ( -3.021909043552730267, 1474.995172108610177, 198.0928472765529875 ) ) ;
#93807 =( LENGTH_UNIT ( ) NAMED_UNIT ( * ) SI_UNIT ( .MILLI., .METRE. ) );
#93808 = LINE ( 'NONE', #15453, #100483 ) ;
#93809 = CARTESIAN_POINT ( 'NONE',  ( 8.251048879697160388, 1367.474174444406117, 210.6218459616991936 ) ) ;
#93810 = CARTESIAN_POINT ( 'NONE',  ( -8.587344795677900322, 1448.168822778199910, 212.1998721081249926 ) ) ;
#93811 = CARTESIAN_POINT ( 'NONE',  ( -18.81371465716550162, 1408.757176060300026, 267.3868151054060149 ) ) ;
#93812 = CARTESIAN_POINT ( 'NONE',  ( -14.42244451974389996, 1436.256339167430042, 149.9811569559620068 ) ) ;
#93813 = VERTEX_POINT ( 'NONE', #88333 ) ;
#93814 = CARTESIAN_POINT ( 'NONE',  ( -12.50888813809999967, 1391.368279522899911, 208.1679514191799854 ) ) ;
#93815 = CARTESIAN_POINT ( 'NONE',  ( 14.11808846290000119, 1443.215913278590051, 189.5356027256979985 ) ) ;
#93816 = B_SPLINE_SURFACE_WITH_KNOTS ( 'NONE', 5, 5, ( 
 ( #80852, #10895, #28797, #68200, #102303, #85494 ),
 ( #8793, #37198, #104394, #27690, #71393, #105507 ),
 ( #20370, #74666, #108800, #57327, #106594, #22552 ),
 ( #21459, #73568, #23681, #98741, #49461, #99276 ),
 ( #81934, #83583, #81374, #38828, #39392, #5237 ),
 ( #38281, #48361, #91993, #72464, #47248, #56755 ) ),
 .UNSPECIFIED., .F., .F., .F.,
 ( 6, 6 ),
 ( 6, 6 ),
 ( 4.991132198159999867, 7.657648704650000582 ),
 ( 0.000000000000000000, 0.5000000000000000000 ),
 .UNSPECIFIED. ) ;
#93817 = AXIS2_PLACEMENT_3D ( 'NONE', #96082, #45714, #88246 ) ;
#93818 = EDGE_LOOP ( 'NONE', ( #29463, #30930, #81491, #48290 ) ) ;
#93819 = ORIENTED_EDGE ( 'NONE', *, *, #74658, .F. ) ;
#93820 = CARTESIAN_POINT ( 'NONE',  ( -5.013435694540000043, 1375.426148861440197, 203.5256706139790310 ) ) ;
#93821 = CARTESIAN_POINT ( 'NONE',  ( 17.84338787571943641, 1523.382868172864164, 237.8836641337660467 ) ) ;
#93822 = CIRCLE ( 'NONE', #33004, 1.999999592264639414 ) ;
#93823 = CARTESIAN_POINT ( 'NONE',  ( 1.133516965105000107, 1516.713079096360161, 213.7319258036569920 ) ) ;
#93824 = CARTESIAN_POINT ( 'NONE',  ( -15.32559775480000042, 1485.482973650830218, 187.2514416256980212 ) ) ;
#93825 = CARTESIAN_POINT ( 'NONE',  ( -17.61615199279099997, 1498.327676081939899, 229.4274054627400119 ) ) ;
#93826 = B_SPLINE_SURFACE_WITH_KNOTS ( 'NONE', 5, 1, ( 
 ( #59409, #94633 ),
 ( #17907, #34180 ),
 ( #26890, #1155 ),
 ( #69470, #93522 ),
 ( #86790, #77303 ),
 ( #78397, #51541 ) ),
 .UNSPECIFIED., .F., .F., .F.,
 ( 6, 6 ),
 ( 2, 2 ),
 ( 0.000000000000000000, 3.563599656280000083 ),
 ( 0.000000000000000000, 14.00000000000000000 ),
 .UNSPECIFIED. ) ;
#93827 = ORIENTED_EDGE ( 'NONE', *, *, #101266, .F. ) ;
#93828 = CARTESIAN_POINT ( 'NONE',  ( -109.5441724430000079, 1379.437034645699896, 303.4364478832590066 ) ) ;
#93829 = ADVANCED_FACE ( 'NONE', ( #78267 ), #37912, .T. ) ;
#93830 = ADVANCED_FACE ( 'NONE', ( #20548 ), #80558, .T. ) ;
#93831 = EDGE_CURVE ( 'NONE', #61245, #11716, #30921, .T. ) ;
#93832 = CARTESIAN_POINT ( 'NONE',  ( -0.01244697378919850002, 1516.939646076049939, 203.3402601539570185 ) ) ;
#93833 = B_SPLINE_CURVE_WITH_KNOTS ( 'NONE', 5,
 ( #14018, #67633, #90738, #76559, #48208, #101189, #51358, #82347, #50815 ),
 .UNSPECIFIED., .F., .F.,
 ( 6, 3, 6 ),
 ( 0.000000000000000000, 0.2400526034259363450, 1.000000000000000000 ),
 .UNSPECIFIED. ) ;
#93834 = CARTESIAN_POINT ( 'NONE',  ( -26.94883404700000185, 1508.590872208830206, 203.1439566689379888 ) ) ;
#93835 = EDGE_CURVE ( 'NONE', #36566, #67278, #32279, .T. ) ;
#93836 = B_SPLINE_SURFACE_WITH_KNOTS ( 'NONE', 5, 5, ( 
 ( #58894, #67857, #48301, #66217, #84624, #100864 ),
 ( #23623, #101969, #65651, #109844, #57807, #23057 ),
 ( #67309, #91931, #109302, #58345, #101406, #14671 ),
 ( #7377, #99767, #57266, #108179, #24155, #7921 ),
 ( #91393, #42091, #39883, #15205, #49394, #92469 ),
 ( #6816, #33122, #48859, #24697, #25255, #75155 ) ),
 .UNSPECIFIED., .F., .F., .F.,
 ( 6, 6 ),
 ( 6, 6 ),
 ( 7.312299096829999456, 16.26600630569999950 ),
 ( -3.330669073880000148E-16, 2.000000000000000000 ),
 .UNSPECIFIED. ) ;
#93837 = CARTESIAN_POINT ( 'NONE',  ( -0.9123187539339999708, 1477.817894300629860, 230.7076694989980012 ) ) ;
#93838 = ADVANCED_FACE ( 'NONE', ( #72645 ), #63602, .T. ) ;
#93839 = CARTESIAN_POINT ( 'NONE',  ( -38.89130781446370122, 1384.579501196720003, 211.8816752983790082 ) ) ;
#93840 = CARTESIAN_POINT ( 'NONE',  ( -6.224176958410000182, 1407.473636847229955, 197.7087082664980073 ) ) ;
#93841 = CARTESIAN_POINT ( 'NONE',  ( -13.55936951270000002, 1409.552479637329952, 226.6517338397979984 ) ) ;
#93843 = ORIENTED_EDGE ( 'NONE', *, *, #99050, .T. ) ;
#93842 = CARTESIAN_POINT ( 'NONE',  ( -11.40944913868885280, 1511.843510977571214, 193.5978051729433957 ) ) ;
#93844 = CARTESIAN_POINT ( 'NONE',  ( -15.90990515426090113, 1514.921193439799936, 224.3246443988719818 ) ) ;
#93845 = CARTESIAN_POINT ( 'NONE',  ( 24.64286055050000002, 1488.680273900929933, 218.7263997298479694 ) ) ;
#93846 = CARTESIAN_POINT ( 'NONE',  ( -47.29346754776256034, 1379.682659667603048, 240.6734148706816825 ) ) ;
#93847 = EDGE_CURVE ( 'NONE', #63792, #107214, #93808, .T. ) ;
#93848 = CARTESIAN_POINT ( 'NONE',  ( -10.78800202809769893, 1480.681112002840109, 211.1294777255430120 ) ) ;
#93849 = CARTESIAN_POINT ( 'NONE',  ( -23.69915799640000031, 1435.325095724740095, 137.0907082570979867 ) ) ;
#93850 = CARTESIAN_POINT ( 'NONE',  ( -2.476733514145000203, 1516.858326417339867, 211.6155457388669845 ) ) ;
#93851 = CARTESIAN_POINT ( 'NONE',  ( -68.70392287810000198, 1379.747767561100090, 279.9836365250589552 ) ) ;
#93852 = CARTESIAN_POINT ( 'NONE',  ( -14.29797315729999951, 1418.019966737229879, 227.1912819175979905 ) ) ;
#93853 = CARTESIAN_POINT ( 'NONE',  ( -29.79244380916537338, 1525.556090473913855, 221.4001982487179419 ) ) ;
#93854 = CIRCLE ( 'NONE', #79592, 2.000000000000068390 ) ;
#93855 = CARTESIAN_POINT ( 'NONE',  ( 4.031168767865001001, 1516.805675336850072, 208.3649472324300120 ) ) ;
#93856 = VERTEX_POINT ( 'NONE', #17087 ) ;
#93857 = CARTESIAN_POINT ( 'NONE',  ( -7.965680540240001051, 1384.926148861439970, 199.4891222871690104 ) ) ;
#93859 = EDGE_CURVE ( 'NONE', #94676, #54104, #97874, .T. ) ;
#93858 = CARTESIAN_POINT ( 'NONE',  ( 2.470955845399089856, 1523.580203803270933, 242.8749759691355621 ) ) ;
#93860 =( BOUNDED_CURVE ( )  B_SPLINE_CURVE ( 3, ( #59188, #101691, #25539, #32844 ),
 .UNSPECIFIED., .F., .T. ) 
 B_SPLINE_CURVE_WITH_KNOTS ( ( 4, 4 ),
 ( 1.570952388538209288, 3.141745507188739239 ),
 .UNSPECIFIED. ) 
 CURVE ( )  GEOMETRIC_REPRESENTATION_ITEM ( )  RATIONAL_B_SPLINE_CURVE ( ( 1.000000000000000000, 0.8047386102906373129, 0.8047386102906373129, 1.000000000000000000 ) ) 
 REPRESENTATION_ITEM ( '' )  );
#93861 = CARTESIAN_POINT ( 'NONE',  ( -2.142567804705589641E-15, 1385.055606633620073, 218.6218459572590120 ) ) ;
#93862 = ORIENTED_EDGE ( 'NONE', *, *, #87166, .F. ) ;
#93863 = CARTESIAN_POINT ( 'NONE',  ( -105.2660175659031125, 1379.052920223518413, 304.0369892317328890 ) ) ;
#93864 = CARTESIAN_POINT ( 'NONE',  ( -3.899052081260000246, 1430.170681384590125, 201.7535711888990022 ) ) ;
#93865 = CARTESIAN_POINT ( 'NONE',  ( 11.97008865472790085, 1434.984363622560068, 151.1079544380379787 ) ) ;
#93866 = CARTESIAN_POINT ( 'NONE',  ( -4.078748368091082988, 1441.172350307923807, 184.7183383138763588 ) ) ;
#93867 = EDGE_CURVE ( 'NONE', #10690, #96166, #109451, .T. ) ;
#93868 = CIRCLE ( 'NONE', #33050, 1.999999999999997780 ) ;
#93869 = CARTESIAN_POINT ( 'NONE',  ( -0.8378199854720000950, 1507.147729960229753, 180.8463070743979983 ) ) ;
#93870 = DIRECTION ( 'NONE',  ( -0.02616798426500965835, -0.9993150019883683122, 0.02616798426500970692 ) ) ;
#93871 = CARTESIAN_POINT ( 'NONE',  ( -1.137524366430000100, 1408.952783613529846, 187.3908199154979854 ) ) ;
#93872 = EDGE_CURVE ( 'NONE', #67049, #105289, #11031, .T. ) ;
#93873 = CARTESIAN_POINT ( 'NONE',  ( 2.764297497180530083, 1430.881855750599925, 218.1996282248960028 ) ) ;
#93874 = CARTESIAN_POINT ( 'NONE',  ( -33.93019615848938741, 1512.187213306747481, 220.5829544587966211 ) ) ;
#93876 = CARTESIAN_POINT ( 'NONE',  ( 13.58268853708210067, 1416.851343896850040, 196.3340833727469885 ) ) ;
#93875 = CARTESIAN_POINT ( 'NONE',  ( 7.720650135305000994, 1516.977993847330026, 214.9014730243169993 ) ) ;
#93877 = CARTESIAN_POINT ( 'NONE',  ( 19.97699626480000035, 1508.102459361230103, 189.1029257653979982 ) ) ;
#93878 = CARTESIAN_POINT ( 'NONE',  ( 5.779603100124999671, 1516.738222552470233, 216.8362174732170047 ) ) ;
#93879 = ORIENTED_EDGE ( 'NONE', *, *, #59650, .T. ) ;
#93880 = CARTESIAN_POINT ( 'NONE',  ( -12.27023112300000030, 1416.839692131129823, 194.6640134917980163 ) ) ;
#93881 = CARTESIAN_POINT ( 'NONE',  ( -16.83891731359999966, 1420.416781728159776, 203.6059137768390030 ) ) ;
#93882 = ORIENTED_EDGE ( 'NONE', *, *, #86258, .T. ) ;
#93883 = ADVANCED_FACE ( 'NONE', ( #23854 ), #58046, .F. ) ;
#93884 = CARTESIAN_POINT ( 'NONE',  ( 0.1674543970350000077, 1419.793577484730122, 184.3767484295979955 ) ) ;
#93885 = CARTESIAN_POINT ( 'NONE',  ( 1.859895826240000050, 1474.627878585689814, 219.9708148048989926 ) ) ;
#93886 = CARTESIAN_POINT ( 'NONE',  ( 0.000000000000000000, 1515.551704408389924, 209.1218459616989946 ) ) ;
#93887 = UNCERTAINTY_MEASURE_WITH_UNIT (LENGTH_MEASURE( 1.000000000000000082E-05 ), #41656, 'distance_accuracy_value', 'NONE');
#93888 = CARTESIAN_POINT ( 'NONE',  ( -7.545176580024880231, 1384.913154240279937, 219.0875923063640016 ) ) ;
#93889 = DIRECTION ( 'NONE',  ( 1.000000000000000000, 0.000000000000000000, 0.000000000000000000 ) ) ;
#93890 = CARTESIAN_POINT ( 'NONE',  ( -6.649360560760902317, 1508.353256394122127, 219.8944077188511130 ) ) ;
#93891 = CARTESIAN_POINT ( 'NONE',  ( 18.64588652299999794, 1416.828040475229955, 209.6843149956849857 ) ) ;
#93892 = CARTESIAN_POINT ( 'NONE',  ( 18.69800617379813801, 1425.875008635436643, 224.9978991839990954 ) ) ;
#93893 = DIRECTION ( 'NONE',  ( 0.000000000000000000, 1.000000000000000000, 0.000000000000000000 ) ) ;
#93894 = CARTESIAN_POINT ( 'NONE',  ( 14.38014760757803145, 1522.051704408389924, 208.3596762285818045 ) ) ;
#93895 = CARTESIAN_POINT ( 'NONE',  ( -2.265645423020000049, 1414.246892558129957, 164.3383647881979925 ) ) ;
#93897 = CARTESIAN_POINT ( 'NONE',  ( 4.326992699990039881, 1515.158586642889986, 209.0578234245899978 ) ) ;
#93896 = CARTESIAN_POINT ( 'NONE',  ( -8.459381271141269920, 1419.310188839569946, 195.9551710783830174 ) ) ;
#93898 = CARTESIAN_POINT ( 'NONE',  ( 2.580915939757335131, 1524.130440953581001, 242.3512492075526836 ) ) ;
#93899 = ORIENTED_EDGE ( 'NONE', *, *, #95927, .T. ) ;
#93900 = VERTEX_POINT ( 'NONE', #109543 ) ;
#93901 = CARTESIAN_POINT ( 'NONE',  ( 21.62164173114529930, 1521.951704408389787, 208.0273405545509888 ) ) ;
#93902 = CARTESIAN_POINT ( 'NONE',  ( -24.41204057910000103, 1440.938895779720042, 212.0297384891179888 ) ) ;
#93903 = CARTESIAN_POINT ( 'NONE',  ( 8.883832781222039898, 1425.079104944299843, 195.6883722520829849 ) ) ;
#93904 = CARTESIAN_POINT ( 'NONE',  ( -10.38946316992339902, 1479.436785722010200, 210.5481016495319864 ) ) ;
#93905 = CARTESIAN_POINT ( 'NONE',  ( 28.27139721233034209, 1526.382868172864164, 219.5606225550385204 ) ) ;
#93906 = EDGE_CURVE ( 'NONE', #48999, #101369, #61201, .T. ) ;
#93907 = CARTESIAN_POINT ( 'NONE',  ( -4.642542606699569419, 1378.262313272806523, 203.6938890911571320 ) ) ;
#93908 = CARTESIAN_POINT ( 'NONE',  ( 13.20846944180000015, 1414.988015876730060, 197.7899243527979820 ) ) ;
#93909 = CARTESIAN_POINT ( 'NONE',  ( -58.10467463043680425, 1383.799326198670087, 277.2797696228070095 ) ) ;
#93910 = CARTESIAN_POINT ( 'NONE',  ( 23.90214117500000057, 1451.650320089529941, 139.9216469008979971 ) ) ;
#93911 = EDGE_CURVE ( 'NONE', #18098, #39550, #55830, .T. ) ;
#93912 = CARTESIAN_POINT ( 'NONE',  ( -29.75012120250000081, 1509.993914124430148, 208.5595671623779879 ) ) ;
#93913 = CARTESIAN_POINT ( 'NONE',  ( -1.212902923111830011, 1516.615653621559886, 201.4106840095360269 ) ) ;
#93915 = VERTEX_POINT ( 'NONE', #103890 ) ;
#93914 = CARTESIAN_POINT ( 'NONE',  ( 10.49159676556239873, 1452.005212983920046, 208.0898620772609888 ) ) ;
#93916 = CARTESIAN_POINT ( 'NONE',  ( -17.62491468606772926, 1460.289161246174444, 228.1912235019598540 ) ) ;
#93917 = CARTESIAN_POINT ( 'NONE',  ( -58.29236204880000116, 1384.661700128139955, 240.0739325125589971 ) ) ;
#93918 = CARTESIAN_POINT ( 'NONE',  ( 8.535515121215828671, 1436.958083742609915, 207.8253345400139835 ) ) ;
#93919 = EDGE_LOOP ( 'NONE', ( #97967, #36293, #29606 ) ) ;
#93920 = EDGE_LOOP ( 'NONE', ( #81621, #17405, #66864, #80764 ) ) ;
#93921 = CARTESIAN_POINT ( 'NONE',  ( 17.33159214698790151, 1507.668127079400165, 230.9408589578669933 ) ) ;
#93922 = CARTESIAN_POINT ( 'NONE',  ( 30.90487439922556945, 1525.907212628473644, 201.8101144455177689 ) ) ;
#93923 = CARTESIAN_POINT ( 'NONE',  ( 37.05187274396420349, 1437.940711956549876, 136.5605698765780005 ) ) ;
#93925 = DIRECTION ( 'NONE',  ( 0.000000000000000000, 1.000000000000000000, 0.000000000000000000 ) ) ;
#93924 = CARTESIAN_POINT ( 'NONE',  ( 20.71063674850000069, 1470.804162803530062, 209.3922244785459839 ) ) ;
#93926 = CARTESIAN_POINT ( 'NONE',  ( 11.77725420934070044, 1479.493139331419798, 209.1772973198850138 ) ) ;
#93927 = CARTESIAN_POINT ( 'NONE',  ( -107.9739803319999965, 1382.432766417899984, 297.9312510628590189 ) ) ;
#93928 = EDGE_CURVE ( 'NONE', #28739, #52504, #96604, .T. ) ;
#93929 = LINE ( 'NONE', #19285, #17769 ) ;
#93930 = CARTESIAN_POINT ( 'NONE',  ( -12.83448315710464094, 1435.932405785817082, 150.8148811484861085 ) ) ;
#93931 = DIRECTION ( 'NONE',  ( -1.755985294532469921E-16, 1.000000000000000000, -1.338183447452831989E-16 ) ) ;
#93932 = CARTESIAN_POINT ( 'NONE',  ( 1.843841672930000009, 1409.915254994430143, 185.4154735675980135 ) ) ;
#93933 = CARTESIAN_POINT ( 'NONE',  ( 0.8856752070958160417, 1486.352519237200113, 197.2385176272069884 ) ) ;
#93934 = CARTESIAN_POINT ( 'NONE',  ( 40.27308693906149273, 1443.611999474700042, 137.1163322506119755 ) ) ;
#93935 = CARTESIAN_POINT ( 'NONE',  ( 10.83341016640000021, 1434.513252767399763, 151.9041015218980135 ) ) ;
#93936 = CARTESIAN_POINT ( 'NONE',  ( -3.117233513421850066, 1441.234898769120036, 170.5448813734479927 ) ) ;
#93937 = CARTESIAN_POINT ( 'NONE',  ( 11.76196284288320015, 1425.587143582329873, 146.3421855601949915 ) ) ;
#93938 = CARTESIAN_POINT ( 'NONE',  ( 1.430284437999999936, 1465.025931307530072, 237.8691342077979982 ) ) ;
#93939 = VERTEX_POINT ( 'NONE', #104999 ) ;
#93940 = CIRCLE ( 'NONE', #79678, 23.69926344187880929 ) ;
#93941 = CARTESIAN_POINT ( 'NONE',  ( 20.60747693140000081, 1477.505856213189873, 217.6602180427189808 ) ) ;
#93942 = CARTESIAN_POINT ( 'NONE',  ( -42.15579669299999921, 1443.896589930619939, 269.8789809301979403 ) ) ;
#93943 = CARTESIAN_POINT ( 'NONE',  ( -23.72545963659144874, 1436.118670184939447, 211.8535580904316191 ) ) ;
#93944 = FACE_OUTER_BOUND ( 'NONE', #93920, .T. ) ;
#93945 = CARTESIAN_POINT ( 'NONE',  ( 14.54088607839999980, 1410.754219483329962, 191.4792867801979810 ) ) ;
#93946 = EDGE_CURVE ( 'NONE', #98935, #77078, #1723, .T. ) ;
#93947 = CARTESIAN_POINT ( 'NONE',  ( 2.330134126090000368, 1515.551704408389924, 212.9514660752490158 ) ) ;
#93948 = CARTESIAN_POINT ( 'NONE',  ( 9.990309780743139356, 1460.215770112410155, 206.0069743695009947 ) ) ;
#93949 = CARTESIAN_POINT ( 'NONE',  ( -1.986418230135969853, 1420.852199177890043, 193.8262422174969970 ) ) ;
#93950 = CARTESIAN_POINT ( 'NONE',  ( -8.352280533070000956, 1418.964256225429835, 232.1493934695980101 ) ) ;
#93951 = CARTESIAN_POINT ( 'NONE',  ( -2.234267340169999727, 1476.147103045889935, 198.8785287704990026 ) ) ;
#93952 = CARTESIAN_POINT ( 'NONE',  ( -107.7913657269999987, 1387.087163723699859, 310.5801087772589995 ) ) ;
#93953 = VECTOR ( 'NONE', #97591, 1000.000000000000114 ) ;
#93954 = CARTESIAN_POINT ( 'NONE',  ( 0.01072155311641910871, 1486.299748484872907, 181.8129703845364133 ) ) ;
#93955 = B_SPLINE_CURVE_WITH_KNOTS ( 'NONE', 3,
 ( #68561, #102660, #85890, #85319, #8614, #49549, #93713, #101015, #32728, #75844, #25960, #42791, #9192, #94276, #24314, #58496, #51754, #33270, #103219, #51190, #43354, #77502, #16990, #60155, #260, #802, #34931, #59597, #69118, #76951, #26527 ),
 .UNSPECIFIED., .F., .F.,
 ( 4, 3, 3, 3, 3, 3, 3, 3, 3, 3, 4 ),
 ( -117.7436746770000013, -117.2149955653400042, -116.2593090969979954, -115.4891864406449997, -114.8126480616819975, -114.1739245078169915, -113.5701753798730067, -112.8587766767369942, -112.0199461915819938, -111.3181123378909945, -110.7231579952140095 ),
 .UNSPECIFIED. ) ;
#93956 = CARTESIAN_POINT ( 'NONE',  ( 5.944559947674049383, 1359.984290312718713, 210.6218459617030021 ) ) ;
#93957 = CARTESIAN_POINT ( 'NONE',  ( -45.75507445926909611, 1438.283494741970117, 266.4162312795270395 ) ) ;
#93958 = CARTESIAN_POINT ( 'NONE',  ( 13.58148582911039881, 1508.837191255689959, 233.6100809729150001 ) ) ;
#93959 = ADVANCED_FACE ( 'NONE', ( #61372 ), #12616, .T. ) ;
#93960 = CARTESIAN_POINT ( 'NONE',  ( -12.98226713004480004, 1414.913060387349788, 219.9156686614909972 ) ) ;
#93961 = ORIENTED_EDGE ( 'NONE', *, *, #53441, .T. ) ;
#93962 = CARTESIAN_POINT ( 'NONE',  ( 5.000329995535000016, 1516.770163853809890, 208.3657552043160024 ) ) ;
#93963 = CARTESIAN_POINT ( 'NONE',  ( -2.478930769269999779, 1432.582979956780036, 157.5229504622980130 ) ) ;
#93964 = B_SPLINE_SURFACE_WITH_KNOTS ( 'NONE', 5, 1, ( 
 ( #58983, #50579 ),
 ( #9120, #85256 ),
 ( #84707, #25340 ),
 ( #60094, #17485 ),
 ( #51683, #45515 ),
 ( #97541, #27575 ) ),
 .UNSPECIFIED., .F., .F., .F.,
 ( 6, 6 ),
 ( 2, 2 ),
 ( -2.269822869709659820E-05, 16.31242598182869941 ),
 ( 0.000000000000000000, 14.00002269822869927 ),
 .UNSPECIFIED. ) ;
#93965 = CARTESIAN_POINT ( 'NONE',  ( -26.31343033946440002, 1441.279830965969950, 137.8584457592320121 ) ) ;
#93966 = CARTESIAN_POINT ( 'NONE',  ( 7.533869295375639652, 1425.775636318390070, 212.2138369296450264 ) ) ;
#93967 = CARTESIAN_POINT ( 'NONE',  ( -26.37095841104669702, 1451.986996602540103, 135.1286765312639773 ) ) ;
#93968 = ORIENTED_EDGE ( 'NONE', *, *, #106382, .F. ) ;
#93969 = CARTESIAN_POINT ( 'NONE',  ( 22.58796458730000012, 1427.336410677830145, 231.9597913024979903 ) ) ;
#93971 = CARTESIAN_POINT ( 'NONE',  ( 13.85241133699999949, 1452.817890303829927, 195.1465048085980243 ) ) ;
#93970 = CARTESIAN_POINT ( 'NONE',  ( -10.99258910100319930, 1492.354469455359776, 207.1887574598779906 ) ) ;
#93972 = EDGE_CURVE ( 'NONE', #100188, #55613, #338, .T. ) ;
#93973 = CARTESIAN_POINT ( 'NONE',  ( 1.801533744329999909, 1412.572206465630188, 232.2925451922980074 ) ) ;
#93974 = CARTESIAN_POINT ( 'NONE',  ( -16.59142030353789821, 1508.492718974290028, 213.6717301258460111 ) ) ;
#93975 = DIRECTION ( 'NONE',  ( -1.000000000000000000, 0.000000000000000000, 0.000000000000000000 ) ) ;
#93976 = EDGE_CURVE ( 'NONE', #37540, #61158, #23037, .T. ) ;
#93977 = CARTESIAN_POINT ( 'NONE',  ( 4.559613763440699685, 1467.726731048589954, 217.9977195186110066 ) ) ;
#93978 = DIRECTION ( 'NONE',  ( -1.755985294532469921E-16, 1.000000000000000000, -1.338183447452831989E-16 ) ) ;
#93979 = EDGE_LOOP ( 'NONE', ( #70023, #19878, #55995, #78001 ) ) ;
#93980 = CARTESIAN_POINT ( 'NONE',  ( -6.563901503888989630, 1410.596044972080108, 269.6193547258999956 ) ) ;
#93981 = CARTESIAN_POINT ( 'NONE',  ( 4.104804799730410458, 1416.793721508729732, 231.8084991735399853 ) ) ;
#93982 = CARTESIAN_POINT ( 'NONE',  ( -113.4000000000000057, 1310.214785017039958, 304.2218459572619622 ) ) ;
#93984 = ORIENTED_EDGE ( 'NONE', *, *, #61862, .T. ) ;
#93983 = CARTESIAN_POINT ( 'NONE',  ( -2.500000000000000000, 1439.509563876250013, 163.9071501952790300 ) ) ;
#93985 = VERTEX_POINT ( 'NONE', #94103 ) ;
#93986 = DIRECTION ( 'NONE',  ( -0.9455185755993178454, 0.000000000000000000, 0.3255681544571537578 ) ) ;
#93987 = EDGE_CURVE ( 'NONE', #32165, #44736, #76465, .T. ) ;
#93988 = CARTESIAN_POINT ( 'NONE',  ( -0.08584137263299880527, 1408.916058034080152, 186.4688618524710080 ) ) ;
#93989 = CARTESIAN_POINT ( 'NONE',  ( -18.22824482168599758, 1443.229620491730202, 204.5519806992609801 ) ) ;
#93990 = CARTESIAN_POINT ( 'NONE',  ( -39.51550670970809165, 1423.010682514669952, 266.3652739410081836 ) ) ;
#93991 = EDGE_CURVE ( 'NONE', #9014, #17632, #96492, .T. ) ;
#93992 = CARTESIAN_POINT ( 'NONE',  ( -20.83970284856240340, 1501.660516804690133, 192.3719794906700145 ) ) ;
#93993 = EDGE_CURVE ( 'NONE', #14138, #72956, #84415, .T. ) ;
#93994 = CARTESIAN_POINT ( 'NONE',  ( -17.72560687289999848, 1420.841998356029990, 226.0101997189979954 ) ) ;
#93995 = CARTESIAN_POINT ( 'NONE',  ( 35.78853434691840363, 1463.243804785920020, 267.3096158296730209 ) ) ;
#93996 = AXIS2_PLACEMENT_3D ( 'NONE', #5569, #23457, #31308 ) ;
#93997 = CARTESIAN_POINT ( 'NONE',  ( -3.481252530716044458, 1466.728071799404233, 234.8984253771955935 ) ) ;
#93998 = CARTESIAN_POINT ( 'NONE',  ( -17.33992335449591238, 1422.584892946659920, 226.5971582259074637 ) ) ;
#93999 = CARTESIAN_POINT ( 'NONE',  ( -0.7574260232259989456, 1516.837969789639828, 205.8660360680970030 ) ) ;
#94000 = VERTEX_POINT ( 'NONE', #83862 ) ;
#94001 = CARTESIAN_POINT ( 'NONE',  ( -11.94180849701186631, 1433.516162581537174, 150.0911432144437470 ) ) ;
#94002 = CARTESIAN_POINT ( 'NONE',  ( -1.278600148798100022, 1444.381613973289859, 199.1499497165799824 ) ) ;
#94003 = CARTESIAN_POINT ( 'NONE',  ( -109.1324239101479918, 1384.847617670179943, 313.2643838898119952 ) ) ;
#94004 = ORIENTED_EDGE ( 'NONE', *, *, #84469, .T. ) ;
#94005 = CARTESIAN_POINT ( 'NONE',  ( -1.123912433469769878, 1458.003495002930094, 229.8665499421440188 ) ) ;
#94006 = CARTESIAN_POINT ( 'NONE',  ( 26.70809291654819972, 1451.980330768489921, 135.0059442101320144 ) ) ;
#94007 = CARTESIAN_POINT ( 'NONE',  ( -14.92122233627069861, 1514.080593477140155, 194.3039127111239850 ) ) ;
#94008 = CARTESIAN_POINT ( 'NONE',  ( -1.543833121739990100, 1424.175334750540060, 228.3471663839470125 ) ) ;
#94009 = CARTESIAN_POINT ( 'NONE',  ( 7.348570800660000124, 1422.803073198840139, 195.5677875354990078 ) ) ;
#94010 = EDGE_CURVE ( 'NONE', #56530, #11508, #23936, .T. ) ;
#94011 = CARTESIAN_POINT ( 'NONE',  ( 18.50818375480000100, 1409.559380405929915, 219.7813082434980174 ) ) ;
#94012 = CARTESIAN_POINT ( 'NONE',  ( -3.938370151530000474, 1495.868122056089987, 198.2201402197989921 ) ) ;
#94013 = CARTESIAN_POINT ( 'NONE',  ( 8.043739714546198627, 1409.193953967760081, 189.2334580016899963 ) ) ;
#94015 = CARTESIAN_POINT ( 'NONE',  ( -18.07895559939639796, 1423.750420671800157, 225.6737883517463672 ) ) ;
#94014 = CARTESIAN_POINT ( 'NONE',  ( 1.379877562750000175, 1416.709753722929918, 233.1857291387979956 ) ) ;
#94016 = CARTESIAN_POINT ( 'NONE',  ( 10.56558922819999857, 1409.282018893330132, 228.0601045111980056 ) ) ;
#94017 = CARTESIAN_POINT ( 'NONE',  ( -12.02613236540000052, 1377.659859441090020, 211.7505269062990010 ) ) ;
#94018 = EDGE_CURVE ( 'NONE', #98127, #73912, #34134, .T. ) ;
#94019 = CARTESIAN_POINT ( 'NONE',  ( 3.145310910306181373, 1370.220870732725871, 208.0282141261312461 ) ) ;
#94020 = EDGE_LOOP ( 'NONE', ( #65549, #49795, #95928, #95467 ) ) ;
#94021 = CARTESIAN_POINT ( 'NONE',  ( -0.8350686643532192477, 1524.382868172863937, 177.3106345060153046 ) ) ;
#94022 = CARTESIAN_POINT ( 'NONE',  ( 11.74913122504709939, 1432.337153681070049, 150.6947002683050130 ) ) ;
#94023 = DIRECTION ( 'NONE',  ( 1.025155669219414347E-18, -1.000000000000000000, 0.000000000000000000 ) ) ;
#94024 = VECTOR ( 'NONE', #62463, 1000.000000000000114 ) ;
#94025 = CARTESIAN_POINT ( 'NONE',  ( -12.43556348120000088, 1391.700544350710061, 208.3488348747239911 ) ) ;
#94026 = CARTESIAN_POINT ( 'NONE',  ( 8.561386400597299939, 1423.835855477939958, 211.2535102716829840 ) ) ;
#94027 = CARTESIAN_POINT ( 'NONE',  ( 3.975726521872664510, 1422.097627045033278, 194.1803425279607040 ) ) ;
#94028 = CARTESIAN_POINT ( 'NONE',  ( -10.91387039267799963, 1462.739297843610075, 207.3784283796969987 ) ) ;
#94029 = CARTESIAN_POINT ( 'NONE',  ( -13.66603629819999810, 1471.441739209529942, 271.1218459616979999 ) ) ;
#94030 = CARTESIAN_POINT ( 'NONE',  ( -21.91509347160294396, 1509.516311833964437, 191.4267936841458493 ) ) ;
#94031 = CARTESIAN_POINT ( 'NONE',  ( 11.89524296629999967, 1433.269816950409904, 149.9550912523980060 ) ) ;
#94032 = CARTESIAN_POINT ( 'NONE',  ( 19.47651264659999626, 1455.559577376729976, 243.9198229517980110 ) ) ;
#94033 = CARTESIAN_POINT ( 'NONE',  ( 12.50317167496160131, 1415.933499560010205, 196.3719056758750128 ) ) ;
#94034 = VECTOR ( 'NONE', #72828, 1000.000000000000000 ) ;
#94035 = CARTESIAN_POINT ( 'NONE',  ( -9.104779855139769396, 1421.478964305890031, 192.1853055963059660 ) ) ;
#94036 = CARTESIAN_POINT ( 'NONE',  ( 12.49065589463330106, 1426.226283141350223, 200.9747314135889837 ) ) ;
#94037 = DIRECTION ( 'NONE',  ( 0.000000000000000000, 1.000000000000000000, 0.000000000000000000 ) ) ;
#94038 = CARTESIAN_POINT ( 'NONE',  ( -17.59109303050000150, 1486.013267125129914, 188.2745623029979924 ) ) ;
#94039 = CARTESIAN_POINT ( 'NONE',  ( 11.80540162446047603, 1398.263086677583033, 214.5664719749284473 ) ) ;
#94040 = CARTESIAN_POINT ( 'NONE',  ( 2.385953148540000068, 1466.626847306429909, 234.2518259445980107 ) ) ;
#94041 = CARTESIAN_POINT ( 'NONE',  ( 23.75028666869999938, 1410.916158841730066, 210.9577920301479992 ) ) ;
#94042 = CARTESIAN_POINT ( 'NONE',  ( 12.26979804483799974, 1416.828039243390094, 223.5793509210460002 ) ) ;
#94043 = CARTESIAN_POINT ( 'NONE',  ( 26.51057051087156680, 1436.730213643903198, 136.8073690796935011 ) ) ;
#94044 = CARTESIAN_POINT ( 'NONE',  ( 3.155009993958097336, 1508.551704391360545, 219.5005843085808692 ) ) ;
#94045 = CARTESIAN_POINT ( 'NONE',  ( 11.40809304261581403, 1434.668754042350429, 151.4869022581049194 ) ) ;
#94046 = CARTESIAN_POINT ( 'NONE',  ( 10.75631870973100135, 1451.138109356459836, 190.3409054002840151 ) ) ;
#94047 = CARTESIAN_POINT ( 'NONE',  ( 1.714334247185000049, 1516.699825673279975, 213.1484604498870112 ) ) ;
#94048 = CARTESIAN_POINT ( 'NONE',  ( -15.77321957905520122, 1420.788161934480058, 204.8879566011889892 ) ) ;
#94049 = CARTESIAN_POINT ( 'NONE',  ( 0.2057925133900349868, 1459.718704435009840, 182.9651470494519856 ) ) ;
#94051 = EDGE_LOOP ( 'NONE', ( #69358, #12482, #97906, #44877 ) ) ;
#94050 = CARTESIAN_POINT ( 'NONE',  ( 5.170971366870000807, 1436.537220372990078, 207.3761814019889869 ) ) ;
#94052 = CARTESIAN_POINT ( 'NONE',  ( 1.191524307911311586, 1526.382868172863937, 179.0083900503167911 ) ) ;
#94053 = CARTESIAN_POINT ( 'NONE',  ( 5.371346801045000063, 1517.051704408389924, 199.4837300725270097 ) ) ;
#94054 = CARTESIAN_POINT ( 'NONE',  ( 12.06086588840000040, 1433.903735958359903, 149.7888706136980090 ) ) ;
#94055 = CARTESIAN_POINT ( 'NONE',  ( -41.50828902776399332, 1442.131284357510140, 134.0999999980909934 ) ) ;
#94056 = CARTESIAN_POINT ( 'NONE',  ( -7.470275378713659542, 1508.551704408439946, 219.0703384621789951 ) ) ;
#94057 = ORIENTED_EDGE ( 'NONE', *, *, #17863, .T. ) ;
#94058 = CARTESIAN_POINT ( 'NONE',  ( -10.19384471300000072, 1472.681895133989883, 209.3325899942670105 ) ) ;
#94059 = CARTESIAN_POINT ( 'NONE',  ( -13.33377604244770076, 1390.546217195540066, 210.7350625626099827 ) ) ;
#94060 = CARTESIAN_POINT ( 'NONE',  ( -14.39499459219999977, 1414.971339025629959, 218.6292155375679727 ) ) ;
#94061 = CARTESIAN_POINT ( 'NONE',  ( -16.62993785878394348, 1526.306647125543122, 183.1687632256341658 ) ) ;
#94062 = CARTESIAN_POINT ( 'NONE',  ( 2.484221813290000025, 1505.974367507990110, 221.6747987149990138 ) ) ;
#94063 = FACE_OUTER_BOUND ( 'NONE', #12255, .T. ) ;
#94064 = LINE ( 'NONE', #35834, #78168 ) ;
#94065 = B_SPLINE_CURVE_WITH_KNOTS ( 'NONE', 5,
 ( #43766, #1224, #35359, #61693, #44329, #61155, #95271, #78472, #1784, #35922, #104218, #19082, #42114, #54933, #20738, #89062, #11813, #80672, #12347, #44892, #79042, #29163, #63351, #2343, #55484, #96371, #28055, #36456, #98004, #105321, #2889, #28614, #72288, #45441, #106420, #37565, #81204, #88528, #38110, #72830, #45983, #10721, #79584, #54396, #70654, #19650, #12901, #97469 ),
 .UNSPECIFIED., .F., .F.,
 ( 6, 3, 3, 3, 3, 3, 3, 3, 3, 3, 3, 3, 3, 3, 3, 6 ),
 ( 0.000000000000000000, 0.001696444935363111695, 0.002566884068491868606, 0.004136085766892796077, 0.005705287465293942123, 0.008843690869748293756, 0.01637566666253125955, 0.02390764245531465729, 0.03884334483964269058, 0.08207802453382453955, 0.1535160673748799665, 0.2249756095436203363, 0.4745335301881646317, 0.7379578698543362014, 0.8518335909529411998, 1.000000000000000000 ),
 .UNSPECIFIED. ) ;
#94066 = CARTESIAN_POINT ( 'NONE',  ( -13.50145109259999998, 1379.789977162729883, 211.3496610090389822 ) ) ;
#94067 = CARTESIAN_POINT ( 'NONE',  ( -11.66658561999999932, 1391.913060387289988, 209.7120187064359982 ) ) ;
#94068 = CARTESIAN_POINT ( 'NONE',  ( -85.93020247385199184, 1385.179414779810031, 289.5851895153920168 ) ) ;
#94069 = CARTESIAN_POINT ( 'NONE',  ( -11.59266921033580111, 1391.913060387289988, 210.4631112540610047 ) ) ;
#94070 = CARTESIAN_POINT ( 'NONE',  ( 10.41307521078920040, 1422.727929710979879, 209.2808407624430060 ) ) ;
#94071 = EDGE_LOOP ( 'NONE', ( #63243, #49909, #99177, #64129, #20568, #107865, #76453 ) ) ;
#94072 = CARTESIAN_POINT ( 'NONE',  ( -33.31575678469999247, 1451.596268149030038, 135.6057732153979885 ) ) ;
#94074 = EDGE_LOOP ( 'NONE', ( #91797, #110712, #38229, #61377 ) ) ;
#94073 = CARTESIAN_POINT ( 'NONE',  ( 11.60004869885203682, 1428.983126981193436, 134.0999999980966777 ) ) ;
#94075 = DIRECTION ( 'NONE',  ( 0.000000000000000000, 1.000000000000000000, 0.000000000000000000 ) ) ;
#94076 = CARTESIAN_POINT ( 'NONE',  ( -18.35817859039589806, 1441.385501788960028, 212.7641934202129903 ) ) ;
#94077 = CARTESIAN_POINT ( 'NONE',  ( -8.698548410450724688, 1364.095994859965231, 207.6218459616988241 ) ) ;
#94078 = FACE_OUTER_BOUND ( 'NONE', #80683, .T. ) ;
#94079 = EDGE_CURVE ( 'NONE', #75001, #44739, #105700, .T. ) ;
#94080 = FACE_OUTER_BOUND ( 'NONE', #46988, .T. ) ;
#94081 = CARTESIAN_POINT ( 'NONE',  ( 16.33922116421775428, 1432.268274340457310, 218.1941633188057779 ) ) ;
#94082 = CARTESIAN_POINT ( 'NONE',  ( 1.808028501710000180, 1417.177841219630182, 232.8705156747979856 ) ) ;
#94083 = CARTESIAN_POINT ( 'NONE',  ( 5.235182724180000413, 1445.859873156990034, 201.6914249771490120 ) ) ;
#94084 = LINE ( 'NONE', #68373, #64546 ) ;
#94085 = CARTESIAN_POINT ( 'NONE',  ( -5.236338392959879684, 1368.774323667059889, 210.6218459616991936 ) ) ;
#94086 = CARTESIAN_POINT ( 'NONE',  ( -2.436662679049999891, 1455.201177966789828, 199.6236828809589952 ) ) ;
#94087 = B_SPLINE_CURVE_WITH_KNOTS ( 'NONE', 5,
 ( #66400, #16486, #58539, #25446, #109486, #100519 ),
 .UNSPECIFIED., .F., .F.,
 ( 6, 6 ),
 ( 0.000000000000000000, 1.000000000000000000 ),
 .UNSPECIFIED. ) ;
#94088 = CARTESIAN_POINT ( 'NONE',  ( 7.321455873725000174, 1516.545806094630279, 206.6359999332069890 ) ) ;
#94089 = CARTESIAN_POINT ( 'NONE',  ( 2.499999999749999979, 1448.248598671410036, 156.2048689938979749 ) ) ;
#94090 = DIRECTION ( 'NONE',  ( 0.9352732527595466472, 0.3048504653312879564, 0.1798058298828889567 ) ) ;
#94091 = CARTESIAN_POINT ( 'NONE',  ( 40.34922463040000196, 1457.054874283830031, 269.7804020139980139 ) ) ;
#94093 = VERTEX_POINT ( 'NONE', #49731 ) ;
#94092 = CARTESIAN_POINT ( 'NONE',  ( 1.901527550710000014, 1494.834316974189960, 220.2474433046989759 ) ) ;
#94094 = PRESENTATION_LAYER_ASSIGNMENT (  '', '', ( #60162 ) ) ;
#94095 = CARTESIAN_POINT ( 'NONE',  ( 1.804213551060599885, 1410.351307734219972, 232.1928989352460064 ) ) ;
#94097 = VERTEX_POINT ( 'NONE', #110169 ) ;
#94096 = TOROIDAL_SURFACE ( 'NONE', #88774, 2.000000000000000000, 1.000000000000000000 ) ;
#94098 = CARTESIAN_POINT ( 'NONE',  ( -16.44706025664929783, 1514.320576835004431, 223.5963406863797047 ) ) ;
#94099 = CARTESIAN_POINT ( 'NONE',  ( -21.05081438890000101, 1449.791259199039814, 196.5491838007980050 ) ) ;
#94101 = CARTESIAN_POINT ( 'NONE',  ( 17.14529549334500302, 1410.143790924649920, 192.4629487703649886 ) ) ;
#94100 = CARTESIAN_POINT ( 'NONE',  ( -11.12709171348789994, 1426.472547912719847, 99.91404471913999430 ) ) ;
#94102 = CARTESIAN_POINT ( 'NONE',  ( -2.476450702264999748, 1516.843453247299749, 211.4215022863270121 ) ) ;
#94103 = CARTESIAN_POINT ( 'NONE',  ( -8.337034337958552754, 1374.913060387289988, 204.5673033449591003 ) ) ;
#94104 = CARTESIAN_POINT ( 'NONE',  ( 1.758988666023477698, 1450.448601557000757, 181.8112131745612885 ) ) ;
#94105 = CARTESIAN_POINT ( 'NONE',  ( -37.17587469459999738, 1423.049458637629868, 264.1764750911980286 ) ) ;
#94106 = CARTESIAN_POINT ( 'NONE',  ( -13.65428303350900130, 1379.630667800430047, 208.3402418708319885 ) ) ;
#94108 = EDGE_CURVE ( 'NONE', #36324, #73043, #24491, .T. ) ;
#94107 = CARTESIAN_POINT ( 'NONE',  ( 28.66375039995369889, 1509.283859617730059, 209.4897258303710146 ) ) ;
#94109 = CARTESIAN_POINT ( 'NONE',  ( 4.038129178976070044, 1508.551704408389924, 213.5713170429240222 ) ) ;
#94110 = CARTESIAN_POINT ( 'NONE',  ( -39.25138508177120400, 1440.085603367899921, 136.7362581835410253 ) ) ;
#94111 = VERTEX_POINT ( 'NONE', #22831 ) ;
#94112 = CARTESIAN_POINT ( 'NONE',  ( 8.792868328939640321, 1397.264807581909963, 218.9196783556029970 ) ) ;
#94113 = CARTESIAN_POINT ( 'NONE',  ( 9.990133414916458676, 1460.215732121300107, 206.0067476231430135 ) ) ;
#94114 = EDGE_CURVE ( 'NONE', #18354, #79507, #8243, .T. ) ;
#94115 = CARTESIAN_POINT ( 'NONE',  ( -17.79268936480000107, 1459.536118998330039, 228.1430453449980007 ) ) ;
#94116 = VERTEX_POINT ( 'NONE', #7163 ) ;
#94117 = ORIENTED_EDGE ( 'NONE', *, *, #89772, .F. ) ;
#94118 = CARTESIAN_POINT ( 'NONE',  ( -3.200208338885655479, 1370.366479271463049, 211.5769014320682970 ) ) ;
#94119 = CARTESIAN_POINT ( 'NONE',  ( -3.165116544085609718, 1422.680544489370277, 151.1405016111839927 ) ) ;
#94120 = EDGE_CURVE ( 'NONE', #2979, #22353, #16139, .T. ) ;
#94121 = CARTESIAN_POINT ( 'NONE',  ( -7.274316450086129926, 1508.306618212879812, 219.8289394896960118 ) ) ;
#94122 = CARTESIAN_POINT ( 'NONE',  ( -11.07029335559397509, 1417.884409290571966, 198.4126321785992388 ) ) ;
#94123 = CARTESIAN_POINT ( 'NONE',  ( -0.4967073565345429542, 1415.438070636819930, 233.3911243540180180 ) ) ;
#94124 = CARTESIAN_POINT ( 'NONE',  ( 13.69373227756942057, 1507.296992741110671, 227.3135802372769092 ) ) ;
#94125 = EDGE_CURVE ( 'NONE', #37122, #66446, #103974, .T. ) ;
#94126 = CARTESIAN_POINT ( 'NONE',  ( -2.573686490390000081, 1461.195040433729901, 234.8853213935979909 ) ) ;
#94127 = CARTESIAN_POINT ( 'NONE',  ( 2.161235707085400026, 1421.184930282719961, 183.1997352710330063 ) ) ;
#94128 = CARTESIAN_POINT ( 'NONE',  ( 9.407380373042538935, 1451.375700834039890, 208.8070606591070089 ) ) ;
#94129 = CARTESIAN_POINT ( 'NONE',  ( 38.50397186617925627, 1443.086052842850904, 136.9545993544632552 ) ) ;
#94130 = CARTESIAN_POINT ( 'NONE',  ( -105.1378806791870062, 1384.889948924000009, 296.9208209011409849 ) ) ;
#94131 = ORIENTED_EDGE ( 'NONE', *, *, #49160, .F. ) ;
#94132 = CARTESIAN_POINT ( 'NONE',  ( 2.288357407604999949, 1517.116049120239950, 203.3334095979369920 ) ) ;
#94133 = CARTESIAN_POINT ( 'NONE',  ( 4.037050997585000189, 1516.939819969850078, 209.1086255745840106 ) ) ;
#94134 = VERTEX_POINT ( 'NONE', #44083 ) ;
#94135 = CARTESIAN_POINT ( 'NONE',  ( 11.79631778455750002, 1428.064473684170025, 147.9895841176879685 ) ) ;
#94136 = CARTESIAN_POINT ( 'NONE',  ( 2.941308709124147658, 1512.218044539111133, 217.0079618907426493 ) ) ;
#94137 = ORIENTED_EDGE ( 'NONE', *, *, #54235, .T. ) ;
#94138 = CARTESIAN_POINT ( 'NONE',  ( -13.73564804769999981, 1415.163755998629995, 220.6561513494980034 ) ) ;
#94139 = CARTESIAN_POINT ( 'NONE',  ( -11.58617079055879806, 1432.339219433009930, 151.0669314679269917 ) ) ;
#94140 = CARTESIAN_POINT ( 'NONE',  ( 4.966585816180000279, 1508.577461573030178, 236.2865006180979890 ) ) ;
#94141 = LINE ( 'NONE', #68983, #40060 ) ;
#94142 = CARTESIAN_POINT ( 'NONE',  ( -4.895323701719999754, 1423.483672866529787, 184.9472429021979849 ) ) ;
#94143 = CARTESIAN_POINT ( 'NONE',  ( -0.4403324739431219714, 1517.051704035390003, 216.6089087266339845 ) ) ;
#94144 = CARTESIAN_POINT ( 'NONE',  ( -10.13245345400000019, 1472.295918207390059, 207.1576006814689777 ) ) ;
#94145 = CARTESIAN_POINT ( 'NONE',  ( -9.840626851222889826, 1410.631480589668854, 188.3682688390927638 ) ) ;
#94146 = CARTESIAN_POINT ( 'NONE',  ( -21.21955013839999893, 1379.607182551329970, 209.4272815681599980 ) ) ;
#94147 = CARTESIAN_POINT ( 'NONE',  ( 23.05067725217429953, 1422.501892093690003, 206.2034611426070114 ) ) ;
#94149 = CARTESIAN_POINT ( 'NONE',  ( 8.721463030380689929, 1468.435740110270217, 202.0638425475829933 ) ) ;
#94148 = FACE_OUTER_BOUND ( 'NONE', #56355, .T. ) ;
#94150 = CARTESIAN_POINT ( 'NONE',  ( -5.007627065198849259, 1423.109407737726542, 184.7889011730115669 ) ) ;
#94151 = ADVANCED_FACE ( 'NONE', ( #988 ), #107915, .F. ) ;
#94152 = CARTESIAN_POINT ( 'NONE',  ( -8.123539286424179551, 1500.423757730580064, 210.2681710058099895 ) ) ;
#94153 = VERTEX_POINT ( 'NONE', #86073 ) ;
#94154 = CARTESIAN_POINT ( 'NONE',  ( 5.360207926212690488, 1422.242713656610022, 144.1549664376839814 ) ) ;
#94155 = PRODUCT_DEFINITION_FORMATION_WITH_SPECIFIED_SOURCE ( 'ANY', '', #31272, .NOT_KNOWN. ) ;
#94156 = CARTESIAN_POINT ( 'NONE',  ( -17.07724394729179096, 1524.330813522192102, 181.0533268958121766 ) ) ;
#94157 = CARTESIAN_POINT ( 'NONE',  ( -2.899874285569436161, 1484.420918474829932, 183.3032565327546592 ) ) ;
#94158 = EDGE_CURVE ( 'NONE', #73768, #26502, #80662, .T. ) ;
#94159 = CARTESIAN_POINT ( 'NONE',  ( -14.20591846559999993, 1415.677402202029953, 213.6695356306190092 ) ) ;
#94161 = ORIENTED_EDGE ( 'NONE', *, *, #109775, .F. ) ;
#94160 = CARTESIAN_POINT ( 'NONE',  ( 0.3770322116046740391, 1515.150283736280016, 204.7946358424930224 ) ) ;
#94162 = CARTESIAN_POINT ( 'NONE',  ( 1.514732344039999790, 1507.625766668030110, 186.2043550924979911 ) ) ;
#94163 = CARTESIAN_POINT ( 'NONE',  ( -12.78690713350000152, 1416.828040475229955, 195.5394874918979724 ) ) ;
#94164 = CARTESIAN_POINT ( 'NONE',  ( -11.24637745149999901, 1428.358274944230061, 150.3272095878980110 ) ) ;
#94165 = DIRECTION ( 'NONE',  ( 0.000000000000000000, -1.000000000000000000, 0.000000000000000000 ) ) ;
#94166 = CARTESIAN_POINT ( 'NONE',  ( -4.219439073160000220, 1441.595895977600094, 183.5288107362979702 ) ) ;
#94167 = CARTESIAN_POINT ( 'NONE',  ( -12.98386957539999997, 1379.322232868390074, 207.9132533945689829 ) ) ;
#94168 = CARTESIAN_POINT ( 'NONE',  ( -4.868096759910030435, 1427.828191610080012, 201.1376980637430165 ) ) ;
#94169 = CARTESIAN_POINT ( 'NONE',  ( -16.10875979846499817, 1511.961073825299991, 221.2567963359670102 ) ) ;
#94170 = CARTESIAN_POINT ( 'NONE',  ( -2.461716435160000049, 1435.943783413959864, 150.4083956814980070 ) ) ;
#94172 = CARTESIAN_POINT ( 'NONE',  ( -11.87328667094049983, 1482.014090395339963, 208.6022402748390050 ) ) ;
#94171 = FACE_OUTER_BOUND ( 'NONE', #10487, .T. ) ;
#94173 = LINE ( 'NONE', #109350, #74668 ) ;
#94174 = VERTEX_POINT ( 'NONE', #87181 ) ;
#94175 = CARTESIAN_POINT ( 'NONE',  ( -4.625359562974999506, 1517.025470194390209, 206.6416589153869836 ) ) ;
#94176 = CARTESIAN_POINT ( 'NONE',  ( 26.99677755089999920, 1412.522578206929893, 268.7553209094979820 ) ) ;
#94177 = CARTESIAN_POINT ( 'NONE',  ( -113.4000000000000057, 1379.913060387289988, 304.2218459572590064 ) ) ;
#94178 = CARTESIAN_POINT ( 'NONE',  ( 22.65318487140000059, 1449.722345962300096, 199.2838700365680040 ) ) ;
#94179 = B_SPLINE_CURVE_WITH_KNOTS ( 'NONE', 5,
 ( #61753, #105950, #10780, #21342, #55005, #89131 ),
 .UNSPECIFIED., .F., .F.,
 ( 6, 6 ),
 ( -74.90934616261959889, -17.77505807049999476 ),
 .UNSPECIFIED. ) ;
#94180 = CARTESIAN_POINT ( 'NONE',  ( -0.2086532769659229791, 1507.120225578089958, 237.3378754264870167 ) ) ;
#94181 = CARTESIAN_POINT ( 'NONE',  ( 32.23107245336971260, 1523.542365884047740, 216.8383915158461548 ) ) ;
#94182 =( BOUNDED_CURVE ( )  B_SPLINE_CURVE ( 3, ( #64616, #63529, #107137, #20913 ),
 .UNSPECIFIED., .F., .F. ) 
 B_SPLINE_CURVE_WITH_KNOTS ( ( 4, 4 ),
 ( 1.965701907008354667E-12, 0.4510268114855934263 ),
 .UNSPECIFIED. ) 
 CURVE ( )  GEOMETRIC_REPRESENTATION_ITEM ( )  RATIONAL_B_SPLINE_CURVE ( ( 1.000000000000000000, 0.9831196230105666567, 0.9831196230105666567, 1.000000000000000000 ) ) 
 REPRESENTATION_ITEM ( '' )  );
#94183 = CARTESIAN_POINT ( 'NONE',  ( -1.271867598320000292, 1450.975052773130074, 183.1634528037979806 ) ) ;
#94184 = CARTESIAN_POINT ( 'NONE',  ( 14.92875414504869980, 1473.796938403280137, 194.5760049489949779 ) ) ;
#94185 = CARTESIAN_POINT ( 'NONE',  ( -14.24607136059999846, 1416.872397861769969, 203.2551075799290174 ) ) ;
#94186 = CARTESIAN_POINT ( 'NONE',  ( -14.12261623989999926, 1444.009911080699794, 188.5535776405979789 ) ) ;
#94187 = CARTESIAN_POINT ( 'NONE',  ( -4.664452821781310377, 1485.067080777090041, 198.1685467601409982 ) ) ;
#94188 = CARTESIAN_POINT ( 'NONE',  ( 17.68711869539999881, 1428.828027849089949, 204.9896315466789929 ) ) ;
#94189 = CARTESIAN_POINT ( 'NONE',  ( -1.530900592538410043, 1457.980095062469900, 229.8454460011110143 ) ) ;
#94190 = VERTEX_POINT ( 'NONE', #61453 ) ;
#94191 = CARTESIAN_POINT ( 'NONE',  ( -1.805659813559999938, 1477.256586422089867, 201.7144240183190220 ) ) ;
#94192 = CARTESIAN_POINT ( 'NONE',  ( -13.46159057049859875, 1409.383149488619893, 202.6401911298929974 ) ) ;
#94193 = CARTESIAN_POINT ( 'NONE',  ( -12.38301933211369921, 1507.638490190219954, 208.9814132950569956 ) ) ;
#94194 = CARTESIAN_POINT ( 'NONE',  ( -15.23237985030026564, 1418.498831278173157, 202.0311994841594867 ) ) ;
#94195 = CARTESIAN_POINT ( 'NONE',  ( -14.64149520810000027, 1474.304963572530141, 268.3932719582979871 ) ) ;
#94196 = CARTESIAN_POINT ( 'NONE',  ( 3.148391675384991206, 1370.270822080606422, 210.8418201729652992 ) ) ;
#94197 = CARTESIAN_POINT ( 'NONE',  ( -14.28806610630405238, 1514.188942798055677, 192.5865514699557082 ) ) ;
#94198 = CARTESIAN_POINT ( 'NONE',  ( -24.06860914254439621, 1444.374860723432676, 212.0637649108989251 ) ) ;
#94199 = CARTESIAN_POINT ( 'NONE',  ( -81.63561843131769535, 1384.635211739379884, 304.8817802514000164 ) ) ;
#94200 = CARTESIAN_POINT ( 'NONE',  ( -14.30187964350709962, 1384.940608584799975, 200.5040086548420106 ) ) ;
#94201 = CARTESIAN_POINT ( 'NONE',  ( 11.82816149694599872, 1415.492117401570113, 223.1475517754469990 ) ) ;
#94202 = CARTESIAN_POINT ( 'NONE',  ( 3.448830483803561719, 1523.382868172864164, 243.0842028158767789 ) ) ;
#94203 = LINE ( 'NONE', #67389, #1898 ) ;
#94204 = CARTESIAN_POINT ( 'NONE',  ( -46.05259875475182696, 1440.913026109461498, 266.6770514725025691 ) ) ;
#94205 = CARTESIAN_POINT ( 'NONE',  ( -22.53916331800000350, 1409.864589572430077, 205.1045926694380057 ) ) ;
#94206 = CARTESIAN_POINT ( 'NONE',  ( 15.72677903779999831, 1414.913060387329779, 204.2094322949480159 ) ) ;
#94207 = DIRECTION ( 'NONE',  ( 0.5877852522924853496, 0.000000000000000000, 0.8090169943749385695 ) ) ;
#94208 = DIRECTION ( 'NONE',  ( 0.08077839049150441209, -0.9967320861844480850, 0.000000000000000000 ) ) ;
#94209 = CARTESIAN_POINT ( 'NONE',  ( 24.18363701780000241, 1464.258769156330118, 206.0765659417580196 ) ) ;
#94210 = VECTOR ( 'NONE', #57561, 1000.000000000000114 ) ;
#94211 = CARTESIAN_POINT ( 'NONE',  ( 11.35868560929959870, 1433.949220014620096, 225.7806587185430089 ) ) ;
#94212 = CARTESIAN_POINT ( 'NONE',  ( 16.57702445344274977, 1524.523992613119390, 180.6870595316466677 ) ) ;
#94213 = CARTESIAN_POINT ( 'NONE',  ( -4.354845126375000319, 1481.954762872750052, 231.1149980757659819 ) ) ;
#94215 = CARTESIAN_POINT ( 'NONE',  ( -9.007783669269999294, 1383.959994898070136, 200.0643063390290024 ) ) ;
#94214 = CARTESIAN_POINT ( 'NONE',  ( -22.77127499929999743, 1411.073674604029975, 211.3149786677880115 ) ) ;
#94216 = CARTESIAN_POINT ( 'NONE',  ( 11.72356565703490006, 1426.704528874140124, 143.2054359492850040 ) ) ;
#94217 = CARTESIAN_POINT ( 'NONE',  ( 9.811585304708989597, 1435.742264125679867, 209.6664975758049820 ) ) ;
#94218 = CARTESIAN_POINT ( 'NONE',  ( -11.04520924769999901, 1490.920650304590026, 210.5690864859589908 ) ) ;
#94219 = B_SPLINE_CURVE_WITH_KNOTS ( 'NONE', 3,
 ( #44396, #46612, #95885, #97002 ),
 .UNSPECIFIED., .F., .F.,
 ( 4, 4 ),
 ( 123.8981301339999987, 143.2822930380000059 ),
 .UNSPECIFIED. ) ;
#94220 = CARTESIAN_POINT ( 'NONE',  ( 6.177122345705179818, 1447.962585782399856, 200.9448045309679856 ) ) ;
#94221 = CARTESIAN_POINT ( 'NONE',  ( -17.27558692971449972, 1507.606285623229951, 224.2552697136770234 ) ) ;
#94222 = CARTESIAN_POINT ( 'NONE',  ( 3.257220602695000355, 1517.040132827679827, 203.3350082531769942 ) ) ;
#94223 = CARTESIAN_POINT ( 'NONE',  ( -8.039183776086851196, 1398.151822053308933, 219.3381333954307593 ) ) ;
#94224 = CARTESIAN_POINT ( 'NONE',  ( -113.4000000000000057, 1378.528619065190014, 304.2218459572590064 ) ) ;
#94225 = CYLINDRICAL_SURFACE ( 'NONE', #66253, 0.9999999999999988898 ) ;
#94226 = CARTESIAN_POINT ( 'NONE',  ( -7.889195814119081440, 1372.293237941190000, 204.8119586455805177 ) ) ;
#94227 = CARTESIAN_POINT ( 'NONE',  ( 6.347281094337080098, 1505.438767865790169, 219.0712605421129808 ) ) ;
#94228 = CARTESIAN_POINT ( 'NONE',  ( -14.35646903299999799, 1420.584115152450067, 213.7701001417389932 ) ) ;
#94231 = EDGE_LOOP ( 'NONE', ( #92892, #87516, #105797, #108869, #79488, #67545, #29945, #103588, #98417, #98975, #72048, #85401, #6929, #55803 ) ) ;
#94230 = CARTESIAN_POINT ( 'NONE',  ( -63.22294501475990103, 1379.735052518850125, 271.8309557046729878 ) ) ;
#94229 = AXIS2_PLACEMENT_3D ( 'NONE', #89783, #21994, #99823 ) ;
#94232 = ORIENTED_EDGE ( 'NONE', *, *, #28441, .T. ) ;
#94233 = CARTESIAN_POINT ( 'NONE',  ( 11.90939254660839985, 1433.635556608139950, 150.4772598317650250 ) ) ;
#94234 = CARTESIAN_POINT ( 'NONE',  ( 21.11882185302462389, 1525.651285554131618, 184.9294391855967490 ) ) ;
#94235 = ORIENTED_EDGE ( 'NONE', *, *, #87682, .F. ) ;
#94236 = CARTESIAN_POINT ( 'NONE',  ( -0.0003153230261271207065, 1396.811848177620050, 221.8113320389208809 ) ) ;
#94237 = CARTESIAN_POINT ( 'NONE',  ( -23.61138782050000273, 1508.482532590330038, 195.6450445675980063 ) ) ;
#94238 = CARTESIAN_POINT ( 'NONE',  ( -8.888756782119999755, 1385.314821197049923, 218.6605176087589939 ) ) ;
#94240 = FACE_OUTER_BOUND ( 'NONE', #49085, .T. ) ;
#94239 = DIRECTION ( 'NONE',  ( -0.000000000000000000, -1.000000000000000000, -0.000000000000000000 ) ) ;
#94241 = CARTESIAN_POINT ( 'NONE',  ( 19.49173981795879840, 1498.116573650230066, 228.9790417235219877 ) ) ;
#94242 = CARTESIAN_POINT ( 'NONE',  ( 1.210143529950000074, 1488.175041650030153, 181.8896941532979952 ) ) ;
#94243 = CARTESIAN_POINT ( 'NONE',  ( 5.826428076080000906, 1473.811884028689974, 218.9454251420289950 ) ) ;
#94244 = CARTESIAN_POINT ( 'NONE',  ( -7.878537825433329367, 1522.051704408389924, 218.1850669711710111 ) ) ;
#94245 = EDGE_CURVE ( 'NONE', #41855, #10827, #103010, .T. ) ;
#94246 = CARTESIAN_POINT ( 'NONE',  ( -0.7351098092479989576, 1516.977504706749869, 211.6135016956469883 ) ) ;
#94247 = CARTESIAN_POINT ( 'NONE',  ( 5.532282644110000369, 1438.101548174390018, 209.4569669639380152 ) ) ;
#94248 = CARTESIAN_POINT ( 'NONE',  ( 34.92262156983900212, 1435.778361306969828, 134.0999999978019730 ) ) ;
#94249 = CARTESIAN_POINT ( 'NONE',  ( 11.86558108900000086, 1432.299711256910086, 149.9824918235980249 ) ) ;
#94250 = CARTESIAN_POINT ( 'NONE',  ( 6.534620444044999310, 1514.642928591849795, 201.0029630038770279 ) ) ;
#94251 = VERTEX_POINT ( 'NONE', #1533 ) ;
#94252 = CARTESIAN_POINT ( 'NONE',  ( 13.74692504272130122, 1435.515273018320158, 150.0128078956250306 ) ) ;
#94253 = EDGE_LOOP ( 'NONE', ( #101120, #103791, #86089, #55860, #68383 ) ) ;
#94254 = ORIENTED_EDGE ( 'NONE', *, *, #27940, .T. ) ;
#94255 = CARTESIAN_POINT ( 'NONE',  ( 13.14995078890901681, 1444.757455661086169, 169.3984255879898626 ) ) ;
#94256 = CARTESIAN_POINT ( 'NONE',  ( -0.7477858788270000945, 1465.398313615129837, 236.2223280954979998 ) ) ;
#94257 = CARTESIAN_POINT ( 'NONE',  ( -4.958564224928870168, 1476.141795758730041, 200.0452580833139962 ) ) ;
#94258 = VECTOR ( 'NONE', #17415, 1000.000000000000000 ) ;
#94259 = CARTESIAN_POINT ( 'NONE',  ( 1.129386202275000084, 1516.613712827999962, 216.4452363774470030 ) ) ;
#94260 = CARTESIAN_POINT ( 'NONE',  ( -19.84400731930000106, 1467.319027288089956, 208.1478232803480068 ) ) ;
#94261 = CARTESIAN_POINT ( 'NONE',  ( 11.89841253197050008, 1421.888142385570063, 209.0481693330570181 ) ) ;
#94262 = CARTESIAN_POINT ( 'NONE',  ( -58.97309372111901382, 1379.721245612332950, 259.0595248300897993 ) ) ;
#94263 = CARTESIAN_POINT ( 'NONE',  ( -7.592224575779999540, 1380.058622747559866, 207.5503173039890044 ) ) ;
#94264 = EDGE_CURVE ( 'NONE', #22920, #25299, #19943, .T. ) ;
#94265 = CARTESIAN_POINT ( 'NONE',  ( -0.01327257453019850021, 1516.940252185109784, 206.2479269295770052 ) ) ;
#94266 = ORIENTED_EDGE ( 'NONE', *, *, #69240, .F. ) ;
#94267 = CARTESIAN_POINT ( 'NONE',  ( -105.4978708633500162, 1378.553056725880197, 304.5324165031829580 ) ) ;
#94268 = CARTESIAN_POINT ( 'NONE',  ( 16.66966702893499885, 1516.995662938509895, 223.5648772753669959 ) ) ;
#94269 = VERTEX_POINT ( 'NONE', #96129 ) ;
#94270 = ADVANCED_FACE ( 'NONE', ( #26143 ), #103404, .T. ) ;
#94271 = CARTESIAN_POINT ( 'NONE',  ( -13.15560506839999988, 1409.874636222130221, 190.0057851175980090 ) ) ;
#94272 = CARTESIAN_POINT ( 'NONE',  ( 7.743766081754999142, 1514.370494773850169, 215.3809789565369783 ) ) ;
#94274 = VERTEX_POINT ( 'NONE', #26708 ) ;
#94273 = CARTESIAN_POINT ( 'NONE',  ( -3.732259305638550018, 1433.538075186169863, 217.9425128220690056 ) ) ;
#94275 = CARTESIAN_POINT ( 'NONE',  ( 24.22543016360000223, 1436.719751587260134, 213.3442258677480083 ) ) ;
#94276 = CARTESIAN_POINT ( 'NONE',  ( -15.74454477997780089, 1508.551704408389924, 210.3741846618140130 ) ) ;
#94277 = CARTESIAN_POINT ( 'NONE',  ( 5.662343758720000508, 1504.894618425089902, 220.5557215505990314 ) ) ;
#94278 = CARTESIAN_POINT ( 'NONE',  ( 0.003825492543937429601, 1466.393772595959945, 235.6965109011690060 ) ) ;
#94279 = LINE ( 'NONE', #17556, #39599 ) ;
#94280 = AXIS2_PLACEMENT_3D ( 'NONE', #91128, #14405, #11962 ) ;
#94281 = CARTESIAN_POINT ( 'NONE',  ( 5.006329581384999727, 1516.755758396839838, 215.6722354023569892 ) ) ;
#94282 = CARTESIAN_POINT ( 'NONE',  ( -3.241666583938100032, 1428.785741415590110, 200.3354813264270149 ) ) ;
#94283 = CARTESIAN_POINT ( 'NONE',  ( -21.06166912470000341, 1509.324064458830208, 189.5257785579979952 ) ) ;
#94284 = CARTESIAN_POINT ( 'NONE',  ( 21.95372433850586802, 1524.425415513990629, 184.5473008717370931 ) ) ;
#94285 = CARTESIAN_POINT ( 'NONE',  ( -4.995726007844999650, 1516.651306816259876, 211.4173314712770093 ) ) ;
#94286 = CARTESIAN_POINT ( 'NONE',  ( 13.85929690100000045, 1410.325638471030061, 191.1496520999980078 ) ) ;
#94287 = EDGE_CURVE ( 'NONE', #63901, #31779, #87797, .T. ) ;
#94288 = CARTESIAN_POINT ( 'NONE',  ( 30.83402112501738657, 1524.872178180564561, 221.7254380314573723 ) ) ;
#94290 = EDGE_LOOP ( 'NONE', ( #27318, #105286, #70857, #21637 ) ) ;
#94289 = CARTESIAN_POINT ( 'NONE',  ( -103.5315408879999950, 1389.439030332400080, 299.8536342697589703 ) ) ;
#94291 = CARTESIAN_POINT ( 'NONE',  ( -68.14386999458439220, 1385.030899397170060, 292.8874234360349647 ) ) ;
#94292 = CARTESIAN_POINT ( 'NONE',  ( 26.19684153890000289, 1465.282679496030141, 259.6167425913980082 ) ) ;
#94293 = CARTESIAN_POINT ( 'NONE',  ( 2.479191938638227732, 1452.138930638437387, 183.7341620333366166 ) ) ;
#94294 = CARTESIAN_POINT ( 'NONE',  ( -11.86716023049999968, 1432.353341358199941, 147.6509521729980179 ) ) ;
#94295 = CARTESIAN_POINT ( 'NONE',  ( -7.652862273441430219, 1508.994713535709934, 236.5479620134960044 ) ) ;
#94296 = CARTESIAN_POINT ( 'NONE',  ( -31.34137657934027388, 1523.382868172864164, 196.3411265156551906 ) ) ;
#94297 = VECTOR ( 'NONE', #92109, 1000.000000000000000 ) ;
#94299 = CARTESIAN_POINT ( 'NONE',  ( 19.47028325960000217, 1455.696635970729858, 226.3889713599980098 ) ) ;
#94298 = CARTESIAN_POINT ( 'NONE',  ( 5.004442038985000174, 1516.690345681169902, 216.8349637732169697 ) ) ;
#94300 = DIRECTION ( 'NONE',  ( 0.000000000000000000, 1.000000000000000000, 0.000000000000000000 ) ) ;
#94301 = CARTESIAN_POINT ( 'NONE',  ( -107.9316645854389947, 1381.454286385220257, 310.0668126409769911 ) ) ;
#94302 = EDGE_LOOP ( 'NONE', ( #98344, #11643 ) ) ;
#94303 = CARTESIAN_POINT ( 'NONE',  ( -1.712644754285000070, 1516.636036526019780, 204.1262224792070015 ) ) ;
#94304 = CARTESIAN_POINT ( 'NONE',  ( 0.3396529269219999980, 1405.776763257430048, 268.4837298631979934 ) ) ;
#94305 = CARTESIAN_POINT ( 'NONE',  ( 28.17856933310000045, 1509.667335739130067, 207.1106752990980056 ) ) ;
#94306 = CIRCLE ( 'NONE', #42441, 2.000000000000002220 ) ;
#94307 = CARTESIAN_POINT ( 'NONE',  ( 24.50134868650000186, 1443.648489106190027, 213.6791898706979964 ) ) ;
#94308 = DIRECTION ( 'NONE',  ( 0.9824080081115912355, 0.000000000000000000, 0.1867471702549089174 ) ) ;
#94309 = CARTESIAN_POINT ( 'NONE',  ( 3.554051323329999956, 1466.352086058089981, 219.5854740514990056 ) ) ;
#94310 = CARTESIAN_POINT ( 'NONE',  ( 2.167844020415154560, 1468.694760366214268, 218.9020797896687327 ) ) ;
#94311 = CARTESIAN_POINT ( 'NONE',  ( 28.37195397669790253, 1435.488266588540000, 135.2384698397310103 ) ) ;
#94312 = CARTESIAN_POINT ( 'NONE',  ( 35.84500107954239922, 1450.075251917649894, 136.2401620429770048 ) ) ;
#94313 = CARTESIAN_POINT ( 'NONE',  ( 3.360259919131120113E-15, 1458.663800951910162, 232.7180369472359871 ) ) ;
#94314 = CARTESIAN_POINT ( 'NONE',  ( -1.848575068539999977, 1431.426229023689984, 200.9261770996690188 ) ) ;
#94315 = CARTESIAN_POINT ( 'NONE',  ( 10.52417073115330126, 1481.313718111980052, 210.1442249564590270 ) ) ;
#94316 = CARTESIAN_POINT ( 'NONE',  ( -21.51513853577911917, 1524.871836253796118, 183.6915109491697535 ) ) ;
#94317 =( BOUNDED_CURVE ( )  B_SPLINE_CURVE ( 3, ( #34164, #102456, #68904, #6747 ),
 .UNSPECIFIED., .F., .F. ) 
 B_SPLINE_CURVE_WITH_KNOTS ( ( 4, 4 ),
 ( 0.000000000000000000, 0.7048113239778065475 ),
 .UNSPECIFIED. ) 
 CURVE ( )  GEOMETRIC_REPRESENTATION_ITEM ( )  RATIONAL_B_SPLINE_CURVE ( ( 1.000000000000000000, 0.9590300661663091475, 0.9590300661663091475, 1.000000000000000000 ) ) 
 REPRESENTATION_ITEM ( '' )  );
#94318 = CARTESIAN_POINT ( 'NONE',  ( -2.086548178679999754, 1515.551704408389924, 212.9514660752490158 ) ) ;
#94319 = ORIENTED_EDGE ( 'NONE', *, *, #54820, .T. ) ;
#94320 = CARTESIAN_POINT ( 'NONE',  ( 0.2331202188386839735, 1408.921201124740037, 186.4825399812679905 ) ) ;
#94321 = CARTESIAN_POINT ( 'NONE',  ( 12.40450132490000179, 1434.419879851630185, 146.7589221149980006 ) ) ;
#94322 = CARTESIAN_POINT ( 'NONE',  ( 11.39903530061180170, 1471.112746094619979, 209.6182361319149834 ) ) ;
#94323 = CARTESIAN_POINT ( 'NONE',  ( 15.25323211731929973, 1454.458797326860122, 189.7583580193819728 ) ) ;
#94324 = CARTESIAN_POINT ( 'NONE',  ( -0.7333927689999999444, 1417.382029894330117, 235.1308572242979835 ) ) ;
#94326 = CARTESIAN_POINT ( 'NONE',  ( -6.919353105000337401, 1470.289799349278837, 190.2359701780528383 ) ) ;
#94325 = CARTESIAN_POINT ( 'NONE',  ( 12.17208542549999883, 1501.180003388690011, 210.7301006051390004 ) ) ;
#94327 = CARTESIAN_POINT ( 'NONE',  ( -29.77420895410000057, 1509.998730836529830, 208.8314797160269904 ) ) ;
#94328 = CARTESIAN_POINT ( 'NONE',  ( 8.625843005480000159, 1428.332922249990133, 213.2805166664589933 ) ) ;
#94329 = CARTESIAN_POINT ( 'NONE',  ( -13.52759590285629976, 1384.881001315799949, 219.1662475987569962 ) ) ;
#94330 = CARTESIAN_POINT ( 'NONE',  ( -9.338711182531437061, 1417.673218423038179, 230.3173475666119998 ) ) ;
#94331 = CARTESIAN_POINT ( 'NONE',  ( -21.03297590181131582, 1450.947314460161351, 144.4212294945661768 ) ) ;
#94332 = CARTESIAN_POINT ( 'NONE',  ( -7.288035249400000026, 1483.352442713390019, 201.0303113485389872 ) ) ;
#94333 = CARTESIAN_POINT ( 'NONE',  ( 23.99831809630000024, 1435.341613007889919, 136.9207814653979938 ) ) ;
#94334 = CARTESIAN_POINT ( 'NONE',  ( -11.02512559413370141, 1396.298066256809761, 208.1314111368130000 ) ) ;
#94335 = VERTEX_POINT ( 'NONE', #95029 ) ;
#94336 = CARTESIAN_POINT ( 'NONE',  ( -17.36307779888920066, 1410.600141639559979, 225.7635892599339797 ) ) ;
#94337 = CARTESIAN_POINT ( 'NONE',  ( 7.346057189749999772, 1434.541746329560056, 149.5958201245979922 ) ) ;
#94338 = VERTEX_POINT ( 'NONE', #104532 ) ;
#94339 = ORIENTED_EDGE ( 'NONE', *, *, #91348, .T. ) ;
#94340 = CARTESIAN_POINT ( 'NONE',  ( 0.2132038637309990048, 1494.307031516189909, 217.5014853844989773 ) ) ;
#94341 = CARTESIAN_POINT ( 'NONE',  ( 7.217397777882030852, 1516.541660446024480, 207.0726429044282781 ) ) ;
#94343 = CARTESIAN_POINT ( 'NONE',  ( -1.171005540028109859, 1457.331745760810236, 219.6985076373949823 ) ) ;
#94342 = CARTESIAN_POINT ( 'NONE',  ( 34.68852446352940433, 1501.977400791986611, 199.9946320047950223 ) ) ;
#94344 = CARTESIAN_POINT ( 'NONE',  ( 4.383945358651920365, 1425.749019032469960, 185.4609551595589778 ) ) ;
#94345 = AXIS2_PLACEMENT_3D ( 'NONE', #23260, #75356, #93228 ) ;
#94346 = CARTESIAN_POINT ( 'NONE',  ( -2.571138338408573532, 1420.704546681525699, 185.6354774934253840 ) ) ;
#94347 = CARTESIAN_POINT ( 'NONE',  ( -2.456601303385831159, 1523.611961620354123, 242.9433449337721243 ) ) ;
#94348 = CARTESIAN_POINT ( 'NONE',  ( 18.99431323780000014, 1459.501207708489801, 220.3864241394989847 ) ) ;
#94349 = FACE_BOUND ( 'NONE', #52556, .T. ) ;
#94350 = CARTESIAN_POINT ( 'NONE',  ( 2.864767215090000096, 1448.949360505710047, 183.5737851087979777 ) ) ;
#94351 = CARTESIAN_POINT ( 'NONE',  ( 10.02176186330000007, 1364.879735892739973, 207.6218459616989946 ) ) ;
#94353 = ORIENTED_EDGE ( 'NONE', *, *, #70326, .F. ) ;
#94352 = CARTESIAN_POINT ( 'NONE',  ( 3.076465250140000052, 1495.499561967389809, 221.1031209306989638 ) ) ;
#94354 = ORIENTED_EDGE ( 'NONE', *, *, #48204, .F. ) ;
#94355 = CARTESIAN_POINT ( 'NONE',  ( -41.14440994790000161, 1444.077640937079877, 136.9184649836980157 ) ) ;
#94356 = B_SPLINE_CURVE_WITH_KNOTS ( 'NONE', 5,
 ( #87259, #44725, #96212, #19487, #106799, #31199 ),
 .UNSPECIFIED., .F., .F.,
 ( 6, 6 ),
 ( 363.0445097500000315, 368.0632323040000529 ),
 .UNSPECIFIED. ) ;
#94357 = CARTESIAN_POINT ( 'NONE',  ( -21.62191568639999772, 1508.114882721290087, 209.5578768717909668 ) ) ;
#94358 = CARTESIAN_POINT ( 'NONE',  ( -7.875528793950000407E-10, 1472.619496933430128, 270.3713665234980112 ) ) ;
#94359 = CARTESIAN_POINT ( 'NONE',  ( 9.088475950640962253, 1500.760587046248929, 202.1887800772891808 ) ) ;
#94360 = CARTESIAN_POINT ( 'NONE',  ( 0.1141191476639999841, 1485.968486491729891, 182.2121106956980157 ) ) ;
#94361 = CARTESIAN_POINT ( 'NONE',  ( -32.79520279071641653, 1523.954914175594695, 201.0814687157684091 ) ) ;
#94362 = CARTESIAN_POINT ( 'NONE',  ( 0.3658621740327940297, 1475.868828734210183, 197.6638016826259729 ) ) ;
#94363 = CARTESIAN_POINT ( 'NONE',  ( -33.91368313123930278, 1450.440614192689964, 136.2454513106639808 ) ) ;
#94364 = DIRECTION ( 'NONE',  ( 0.000000000000000000, 0.000000000000000000, 1.000000000000000000 ) ) ;
#94365 = CARTESIAN_POINT ( 'NONE',  ( -13.22806383200000013, 1431.113060387329824, 195.8937821299979873 ) ) ;
#94366 = CARTESIAN_POINT ( 'NONE',  ( 9.803099786913902491, 1368.651548183235036, 208.3718459617010978 ) ) ;
#94367 = CARTESIAN_POINT ( 'NONE',  ( 9.106334930605640920, 1408.186707947460036, 198.7849738689709795 ) ) ;
#94368 = CARTESIAN_POINT ( 'NONE',  ( -18.83033903852280133, 1408.714486736299932, 267.7018036114649817 ) ) ;
#94369 = B_SPLINE_CURVE_WITH_KNOTS ( 'NONE', 3,
 ( #61788, #95910, #44421, #53377, #68524, #8033, #10245, #43858, #78005, #76914, #69639, #60681, #25924, #76353, #60121, #77463, #27063, #110502, #765, #61249, #69082, #103183, #29256, #44982, #79131, #62341, #38200, #12449, #38744, #98651, #98100, #2439, #105418, #47168, #96466, #2985, #10813, #36554, #107061, #81296, #106512, #20287, #71304, #21372, #64536, #4610, #55581, #4075, #3532, #54493, #46633, #72922, #30345, #37105, #63447 ),
 .UNSPECIFIED., .F., .F.,
 ( 4, 3, 3, 3, 3, 3, 3, 3, 3, 3, 3, 3, 3, 3, 3, 3, 3, 3, 4 ),
 ( -169.6276195580000206, -126.5933223886119947, -88.68156620233840215, -52.61810133791399835, -51.73140211568609459, -50.56540007835791073, -49.37793206528289147, -48.17557270853839668, -46.94365568215079065, -45.68967734683630511, -44.41100891884349267, -43.10437972021219366, -41.74527663196900562, -40.34034550197179669, -38.87942175190678995, -37.34527141349130375, -35.70714590379060382, -33.89535962364968213, -31.55396706740000923 ),
 .UNSPECIFIED. ) ;
#94370 = DIRECTION ( 'NONE',  ( -0.6736849260863841948, 0.000000000000000000, 0.7390186874254148774 ) ) ;
#94371 = VERTEX_POINT ( 'NONE', #9913 ) ;
#94372 = CARTESIAN_POINT ( 'NONE',  ( -11.86538722380000088, 1432.286166193919826, 149.9824190662980072 ) ) ;
#94373 = CARTESIAN_POINT ( 'NONE',  ( 13.47846152179999990, 1444.303430095470048, 188.1230873751979686 ) ) ;
#94374 = ORIENTED_EDGE ( 'NONE', *, *, #92623, .F. ) ;
#94375 = AXIS2_PLACEMENT_3D ( 'NONE', #3333, #98452, #4416 ) ;
#94376 = ORIENTED_EDGE ( 'NONE', *, *, #87716, .F. ) ;
#94377 = CARTESIAN_POINT ( 'NONE',  ( 4.939111363942668476, 1423.323286052371714, 184.2638540454798886 ) ) ;
#94378 = CARTESIAN_POINT ( 'NONE',  ( 8.486023334060124768, 1522.051704408389924, 207.2139745301958271 ) ) ;
#94379 = CARTESIAN_POINT ( 'NONE',  ( 4.621267883935000320, 1516.830644417779922, 214.1213023606370029 ) ) ;
#94380 = CARTESIAN_POINT ( 'NONE',  ( -18.39416877649999904, 1470.473699348829996, 189.9134802429980198 ) ) ;
#94381 = AXIS2_PLACEMENT_3D ( 'NONE', #51687, #101499, #93651 ) ;
#94382 = EDGE_LOOP ( 'NONE', ( #4325, #74384, #99085, #92073 ) ) ;
#94383 = CARTESIAN_POINT ( 'NONE',  ( -105.7140364779999970, 1379.461008902830145, 303.4364470169589936 ) ) ;
#94384 = CIRCLE ( 'NONE', #55113, 0.4999999999999449329 ) ;
#94385 = FACE_OUTER_BOUND ( 'NONE', #73325, .T. ) ;
#94386 = CARTESIAN_POINT ( 'NONE',  ( -6.946748557085000719, 1516.983995446890049, 204.1186252050270014 ) ) ;
#94387 = CARTESIAN_POINT ( 'NONE',  ( -28.44576460359999714, 1509.873577826230076, 203.8870703132379845 ) ) ;
#94388 = DIRECTION ( 'NONE',  ( -0.000000000000000000, -0.000000000000000000, 1.000000000000000000 ) ) ;
#94389 = CARTESIAN_POINT ( 'NONE',  ( -68.70547844060000386, 1384.729371863979850, 263.4329467144589785 ) ) ;
#94390 = CARTESIAN_POINT ( 'NONE',  ( -43.64178920747140467, 1384.594654343729871, 216.7300204284549920 ) ) ;
#94391 = CARTESIAN_POINT ( 'NONE',  ( -1.288987972930000003, 1407.277489897129954, 196.1207496164979887 ) ) ;
#94392 = CARTESIAN_POINT ( 'NONE',  ( -104.4869036590000064, 1389.270867165570053, 307.8650956148590012 ) ) ;
#94394 = ORIENTED_EDGE ( 'NONE', *, *, #91873, .F. ) ;
#94393 = CARTESIAN_POINT ( 'NONE',  ( -5.705323726350000513, 1447.426426495140049, 185.3480178495979658 ) ) ;
#94395 = CARTESIAN_POINT ( 'NONE',  ( -24.65352725776519804, 1430.511890270439835, 210.2240530382869963 ) ) ;
#94396 = CARTESIAN_POINT ( 'NONE',  ( 25.47381561340000289, 1508.124471600029892, 219.0002699717279881 ) ) ;
#94397 = CARTESIAN_POINT ( 'NONE',  ( -10.37617513879240150, 1479.403831811299824, 210.6295454707710064 ) ) ;
#94398 = CARTESIAN_POINT ( 'NONE',  ( -25.10800663690000079, 1436.295742790639906, 137.5680277278979986 ) ) ;
#94399 = B_SPLINE_CURVE_WITH_KNOTS ( 'NONE', 3,
 ( #73914, #20329, #108042, #57125, #88667, #46126, #80256, #71900, #48721, #82846, #31894, #6136, #40293, #66079, #100204, #53412, #87563, #79169, #45024, #8886, #25129, #50376, #85045, #51458, #57681, #23489, #76112, #91795, #110252, #83395, #32986, #33526, #92900, #84502, #15072, #109172, #50914, #83950, #109711, #42499, #15614, #49268, #49821, #85590, #6693, #40849, #67728, #75022, #101835, #32459, #67175, #59332, #16173, #7792, #66634 ),
 .UNSPECIFIED., .F., .F.,
 ( 4, 3, 3, 3, 3, 3, 3, 3, 3, 3, 3, 3, 3, 3, 3, 3, 3, 3, 4 ),
 ( 9.902195898180000455, 10.17210527305349999, 10.45530577770620084, 10.70141353110000004, 11.00396970308270106, 11.32322756685590015, 11.52456852350000105, 11.84989040654489934, 12.16242387770419953, 12.38020728900000123, 12.74551463658920092, 13.12275145097810025, 13.53252099856839941, 13.95359103769039955, 14.40783883234119855, 14.91487510225679891, 15.44821056775730028, 15.94145638524550179, 16.40090783169999966 ),
 .UNSPECIFIED. ) ;
#94400 = AXIS2_PLACEMENT_3D ( 'NONE', #76158, #7841, #84000 ) ;
#94401 = CARTESIAN_POINT ( 'NONE',  ( -2.477373643995000485, 1516.891731298979948, 212.0030687278169808 ) ) ;
#94402 = CARTESIAN_POINT ( 'NONE',  ( -68.62999220760001151, 1379.747924320049833, 279.8460896497590511 ) ) ;
#94403 = CARTESIAN_POINT ( 'NONE',  ( -14.60531145299999878, 1420.435034123629976, 227.1460274248979943 ) ) ;
#94404 = DIRECTION ( 'NONE',  ( 0.000000000000000000, 0.000000000000000000, 1.000000000000000000 ) ) ;
#94405 = CARTESIAN_POINT ( 'NONE',  ( 1.119592181715000079, 1516.958737650239982, 207.9859471464170326 ) ) ;
#94406 = ORIENTED_EDGE ( 'NONE', *, *, #69502, .T. ) ;
#94407 = CARTESIAN_POINT ( 'NONE',  ( 2.500000000000000000, 1435.404599731399912, 157.5892871108979989 ) ) ;
#94408 = CARTESIAN_POINT ( 'NONE',  ( -2.365925665009999790, 1412.840979806830092, 232.8160838550979861 ) ) ;
#94409 = CARTESIAN_POINT ( 'NONE',  ( -59.22805538469999931, 1384.945537078079951, 279.9292060866590077 ) ) ;
#94410 = EDGE_LOOP ( 'NONE', ( #56663, #39108, #6743, #47163 ) ) ;
#94411 = CARTESIAN_POINT ( 'NONE',  ( -15.37547630988030001, 1385.293449114180021, 219.4910068333289814 ) ) ;
#94412 = CARTESIAN_POINT ( 'NONE',  ( -3.802211600920000212, 1430.235143476489839, 201.6995583931590090 ) ) ;
#94413 = CARTESIAN_POINT ( 'NONE',  ( 12.23060000949119974, 1434.169197542179973, 149.9832296201709880 ) ) ;
#94414 = CARTESIAN_POINT ( 'NONE',  ( 16.77391199951920342, 1459.306422992139915, 228.8325835937480122 ) ) ;
#94415 = CARTESIAN_POINT ( 'NONE',  ( -21.33188221090540182, 1507.840646589619837, 227.2305681273250002 ) ) ;
#94416 = B_SPLINE_CURVE_WITH_KNOTS ( 'NONE', 3,
 ( #54830, #30139, #11171, #46978, #38011, #81102, #45331, #79470, #72192, #106311, #54288, #88411, #57033, #40757, #99544, #14985, #82201, #41318, #32364, #108514, #92261, #4945, #101192, #73831, #6607, #83311, #49181, #91160, #13881, #15532, #39663, #14435, #40207, #58128 ),
 .UNSPECIFIED., .F., .F.,
 ( 4, 3, 3, 3, 3, 3, 3, 3, 3, 3, 3, 4 ),
 ( -1.999999997816839903, -1.865374217096350096, -1.681834405945489941, -1.496047443713429903, -1.309079570038079954, -1.120656966309940161, -0.9318186706558500010, -0.7430292649658170046, -0.5547479918945381616, -0.3681582181805309606, -0.1831547726995599312, 0.000000000000000000 ),
 .UNSPECIFIED. ) ;
#94417 = CARTESIAN_POINT ( 'NONE',  ( -2.760778490449999900, 1409.009468896630096, 188.0459414135980012 ) ) ;
#94418 = B_SPLINE_CURVE_WITH_KNOTS ( 'NONE', 5,
 ( #6807, #51035, #109834, #49933, #58885, #24146 ),
 .UNSPECIFIED., .F., .F.,
 ( 6, 6 ),
 ( -93.91916526269999110, -17.09700588378190389 ),
 .UNSPECIFIED. ) ;
#94419 = CARTESIAN_POINT ( 'NONE',  ( 3.427508779931670357, 1430.651858238479917, 217.9719317096229929 ) ) ;
#94420 = LINE ( 'NONE', #17140, #16477 ) ;
#94421 = EDGE_CURVE ( 'NONE', #62944, #41530, #61514, .T. ) ;
#94423 = CARTESIAN_POINT ( 'NONE',  ( -3.909710721586120208, 1517.051704408389924, 197.7672215555029993 ) ) ;
#94422 = CARTESIAN_POINT ( 'NONE',  ( 0.7560907277860019482, 1516.770163853809890, 214.1221759657669850 ) ) ;
#94424 = CARTESIAN_POINT ( 'NONE',  ( -8.864690188119949354, 1385.133112985140087, 218.6772544400749894 ) ) ;
#94425 = CARTESIAN_POINT ( 'NONE',  ( -2.500000000000000000, 1419.383100980419840, 144.1003751433630100 ) ) ;
#94426 = ORIENTED_EDGE ( 'NONE', *, *, #68016, .F. ) ;
#94427 = CARTESIAN_POINT ( 'NONE',  ( -12.26979143229999991, 1416.828042640230024, 194.6643372026980217 ) ) ;
#94428 = CARTESIAN_POINT ( 'NONE',  ( -11.60004869885203682, 1426.043662085331562, 137.7527993286476544 ) ) ;
#94429 = ORIENTED_EDGE ( 'NONE', *, *, #62348, .F. ) ;
#94430 = CARTESIAN_POINT ( 'NONE',  ( 3.571721340409999890, 1420.465157505230081, 185.4391698450980073 ) ) ;
#94431 = CARTESIAN_POINT ( 'NONE',  ( -12.61766350599999953, 1502.778797914289953, 208.5850585992880042 ) ) ;
#94432 = CARTESIAN_POINT ( 'NONE',  ( 2.664527636416277989, 1524.964230758899930, 176.5361228849588997 ) ) ;
#94433 = CARTESIAN_POINT ( 'NONE',  ( 2.901791247649999850, 1441.419505434789926, 218.6084270491589905 ) ) ;
#94434 = CARTESIAN_POINT ( 'NONE',  ( -26.35977987659270028, 1508.073080378489749, 201.5431538711860071 ) ) ;
#94435 = CARTESIAN_POINT ( 'NONE',  ( -16.38947255413719617, 1409.756821326547652, 192.2387554727406496 ) ) ;
#94436 = CARTESIAN_POINT ( 'NONE',  ( 18.46483594369999892, 1415.628674276829770, 210.6745050120780149 ) ) ;
#94437 = DIRECTION ( 'NONE',  ( 1.755985294532469921E-16, -1.000000000000000000, 1.338183447452831989E-16 ) ) ;
#94438 = CARTESIAN_POINT ( 'NONE',  ( 8.787489738345170665, 1459.851268306849988, 204.0738034033330166 ) ) ;
#94439 = DIRECTION ( 'NONE',  ( 0.4090087482554383702, 0.000000000000000000, 0.9125304618753937724 ) ) ;
#94440 = CARTESIAN_POINT ( 'NONE',  ( 26.92291421019269748, 1446.493256787829978, 137.3410761307699772 ) ) ;
#94442 = CARTESIAN_POINT ( 'NONE',  ( -2.506807337198010188, 1509.132703289729989, 179.1218463405919863 ) ) ;
#94441 = CARTESIAN_POINT ( 'NONE',  ( -8.867713673612659164, 1420.193669887999931, 195.6881175697860158 ) ) ;
#94443 = DIRECTION ( 'NONE',  ( 0.000000000000000000, 1.000000000000000000, 0.000000000000000000 ) ) ;
#94444 = VERTEX_POINT ( 'NONE', #78785 ) ;
#94445 = CARTESIAN_POINT ( 'NONE',  ( 1.550759356559749946, 1415.890045858090161, 190.5138187982429940 ) ) ;
#94446 = CARTESIAN_POINT ( 'NONE',  ( 26.22432434920000333, 1488.572867069630092, 206.9931121771180074 ) ) ;
#94447 = CARTESIAN_POINT ( 'NONE',  ( -4.329448776040000446, 1515.064792882589927, 207.2788837304390199 ) ) ;
#94448 = CARTESIAN_POINT ( 'NONE',  ( 5.066731847092691865, 1410.465363966433870, 186.3980185437680177 ) ) ;
#94449 = AXIS2_PLACEMENT_3D ( 'NONE', #99967, #109494, #58547 ) ;
#94450 = CARTESIAN_POINT ( 'NONE',  ( -10.50924080488429979, 1480.092739868610124, 208.7673280485799978 ) ) ;
#94451 = CARTESIAN_POINT ( 'NONE',  ( 12.15678282470000049, 1407.401676941830146, 215.7644370117779999 ) ) ;
#94452 = CARTESIAN_POINT ( 'NONE',  ( -18.49885826511389908, 1509.559054752839984, 185.8253364393310108 ) ) ;
#94453 = AXIS2_PLACEMENT_3D ( 'NONE', #24060, #94037, #43102 ) ;
#94454 = CARTESIAN_POINT ( 'NONE',  ( -1.520740653450000091, 1487.755788924029957, 231.1622291657979815 ) ) ;
#94455 = FACE_OUTER_BOUND ( 'NONE', #38602, .T. ) ;
#94456 = CARTESIAN_POINT ( 'NONE',  ( -66.89731259161800381, 1383.788378096659926, 291.0260303366639505 ) ) ;
#94457 = VECTOR ( 'NONE', #32987, 1000.000000000000000 ) ;
#94458 = EDGE_CURVE ( 'NONE', #11723, #79464, #37592, .T. ) ;
#94459 = EDGE_CURVE ( 'NONE', #27091, #20305, #52298, .T. ) ;
#94460 = CARTESIAN_POINT ( 'NONE',  ( 22.25038035520000079, 1451.993487009829778, 142.0274306324980103 ) ) ;
#94461 = CARTESIAN_POINT ( 'NONE',  ( -8.590718235127866365, 1437.541524225612193, 210.2462751636549569 ) ) ;
#94462 = CARTESIAN_POINT ( 'NONE',  ( -23.52438668707183211, 1410.744642857871213, 210.4400693876917217 ) ) ;
#94463 = EDGE_CURVE ( 'NONE', #77650, #66906, #65562, .T. ) ;
#94465 = ORIENTED_EDGE ( 'NONE', *, *, #41858, .T. ) ;
#94464 = CARTESIAN_POINT ( 'NONE',  ( 23.97351809889999785, 1509.497062395329976, 194.1275154229979876 ) ) ;
#94466 = AXIS2_PLACEMENT_3D ( 'NONE', #40259, #107458, #108008 ) ;
#94467 = CARTESIAN_POINT ( 'NONE',  ( -18.29272317556928940, 1459.191059311327763, 227.8243320175402573 ) ) ;
#94468 = CARTESIAN_POINT ( 'NONE',  ( -94.50912602849999189, 1384.855827234549906, 294.8620370673590401 ) ) ;
#94469 = ADVANCED_FACE ( 'NONE', ( #45758 ), #99353, .F. ) ;
#94470 = CARTESIAN_POINT ( 'NONE',  ( -0.5929201156298425923, 1417.119756057481027, 234.4154478403977180 ) ) ;
#94471 = VERTEX_POINT ( 'NONE', #81515 ) ;
#94472 = EDGE_LOOP ( 'NONE', ( #7864, #19577, #59515, #84182 ) ) ;
#94473 = CARTESIAN_POINT ( 'NONE',  ( 18.66884402514269681, 1509.506581848020005, 231.4335292741830017 ) ) ;
#94474 = DIRECTION ( 'NONE',  ( -0.3081687959821756695, 0.7660444431188054848, -0.5640991972602826809 ) ) ;
#94475 = CARTESIAN_POINT ( 'NONE',  ( 40.20118103687880051, 1442.631303985449904, 137.0031652087610041 ) ) ;
#94477 = CARTESIAN_POINT ( 'NONE',  ( -8.081131085970000546E-10, 1475.995192538530091, 267.2558860777979817 ) ) ;
#94476 = CARTESIAN_POINT ( 'NONE',  ( 5.510800338187703318, 1410.588349387585595, 269.3375996105341983 ) ) ;
#94478 = CARTESIAN_POINT ( 'NONE',  ( 8.663291285446870660, 1437.708809294000048, 209.4154668070010246 ) ) ;
#94479 = CARTESIAN_POINT ( 'NONE',  ( -109.2455494860000016, 1384.077694082239987, 297.1940690992589680 ) ) ;
#94480 = CARTESIAN_POINT ( 'NONE',  ( -11.87299952773408762, 1435.287980174489348, 151.2457144668333910 ) ) ;
#94481 = CARTESIAN_POINT ( 'NONE',  ( -20.02256639929999693, 1485.317074534930043, 191.1140876134980147 ) ) ;
#94482 = CIRCLE ( 'NONE', #103431, 1.999999999999998668 ) ;
#94483 = CARTESIAN_POINT ( 'NONE',  ( 2.894471309390000080, 1409.014137552730062, 187.1861089909980080 ) ) ;
#94484 = CARTESIAN_POINT ( 'NONE',  ( 0.1984908215090459838, 1486.169885337769983, 197.2145582505330026 ) ) ;
#94485 = CARTESIAN_POINT ( 'NONE',  ( -12.15187876699999947, 1435.108173511759787, 151.0159321440980023 ) ) ;
#94486 = CARTESIAN_POINT ( 'NONE',  ( -9.163589329508671000, 1449.727551480139937, 209.8107205256980023 ) ) ;
#94487 = DIRECTION ( 'NONE',  ( 1.755985294532469921E-16, -1.000000000000000000, 1.338183447452831989E-16 ) ) ;
#94488 = LINE ( 'NONE', #32932, #105265 ) ;
#94489 = CARTESIAN_POINT ( 'NONE',  ( 0.2811493428090000024, 1466.033507498329982, 235.8442874365980231 ) ) ;
#94490 = VERTEX_POINT ( 'NONE', #4819 ) ;
#94491 = CARTESIAN_POINT ( 'NONE',  ( -4.410745166166390341, 1508.610338516509955, 212.9873992348109937 ) ) ;
#94492 = CARTESIAN_POINT ( 'NONE',  ( 11.06889095329999861, 1479.888754528190020, 229.8106084604989974 ) ) ;
#94494 = EDGE_CURVE ( 'NONE', #65542, #93856, #83009, .T. ) ;
#94493 = CARTESIAN_POINT ( 'NONE',  ( -37.00343483889999874, 1455.724349294930107, 269.5585655813979997 ) ) ;
#94495 = PLANE ( 'NONE',  #12288 ) ;
#94496 = CARTESIAN_POINT ( 'NONE',  ( 17.41346973679999977, 1410.020394403929913, 224.1775087769979962 ) ) ;
#94497 = CARTESIAN_POINT ( 'NONE',  ( -16.86523139679999872, 1468.641458686789974, 198.2210143100990081 ) ) ;
#94498 = CARTESIAN_POINT ( 'NONE',  ( -1.076288783000059918E-08, 1474.539729485439921, 264.4539261149100184 ) ) ;
#94499 = CARTESIAN_POINT ( 'NONE',  ( -4.115882898156034919, 1509.032014410906640, 213.4860376516270719 ) ) ;
#94500 = CARTESIAN_POINT ( 'NONE',  ( -1.061258286910000015, 1415.553739807329976, 227.5328994501979878 ) ) ;
#94501 = CARTESIAN_POINT ( 'NONE',  ( -6.733539913119999554, 1418.366792801529982, 233.9669031324980040 ) ) ;
#94502 = CARTESIAN_POINT ( 'NONE',  ( -108.7149811449999959, 1387.932087793509936, 310.6222449872589664 ) ) ;
#94503 = EDGE_CURVE ( 'NONE', #76626, #32282, #28377, .T. ) ;
#94504 = CARTESIAN_POINT ( 'NONE',  ( -7.867033286719529173, 1511.220110216749845, 214.5458993444780162 ) ) ;
#94505 = CARTESIAN_POINT ( 'NONE',  ( 1.895014057282678577, 1358.567760096916572, 208.3718459617010978 ) ) ;
#94506 = CARTESIAN_POINT ( 'NONE',  ( -45.98858655093319925, 1439.424532750870185, 268.4973034418130169 ) ) ;
#94507 = CARTESIAN_POINT ( 'NONE',  ( -2.694622903610000009, 1431.454301131900138, 185.0137053526979969 ) ) ;
#94508 = CARTESIAN_POINT ( 'NONE',  ( -8.097513007330000789, 1424.669315053030004, 209.4052413237879762 ) ) ;
#94509 = EDGE_CURVE ( 'NONE', #105177, #55324, #66381, .T. ) ;
#94510 = ORIENTED_EDGE ( 'NONE', *, *, #8261, .T. ) ;
#94511 = CARTESIAN_POINT ( 'NONE',  ( 7.726684687535000151, 1517.208444099459939, 210.2479840788170122 ) ) ;
#94512 = CARTESIAN_POINT ( 'NONE',  ( -5.455807433810000440, 1438.116814840910138, 154.7280903985979990 ) ) ;
#94513 = CARTESIAN_POINT ( 'NONE',  ( -9.385572798718857968, 1471.838051314206268, 213.1320772043752072 ) ) ;
#94514 = CARTESIAN_POINT ( 'NONE',  ( 7.510429961322310888, 1425.933150149150151, 212.2881029679170126 ) ) ;
#94515 = CARTESIAN_POINT ( 'NONE',  ( -26.88702675072890003, 1451.212428032629987, 136.2751528734569888 ) ) ;
#94516 = ORIENTED_EDGE ( 'NONE', *, *, #50285, .T. ) ;
#94517 = CARTESIAN_POINT ( 'NONE',  ( 10.80267214090000039, 1423.683922205029830, 212.9172522967979830 ) ) ;
#94519 = CARTESIAN_POINT ( 'NONE',  ( -15.26795443890799930, 1513.114148094120083, 223.1466213588239782 ) ) ;
#94518 = FACE_OUTER_BOUND ( 'NONE', #20686, .T. ) ;
#94520 =( BOUNDED_CURVE ( )  B_SPLINE_CURVE ( 3, ( #66116, #107531, #74507, #90726 ),
 .UNSPECIFIED., .F., .T. ) 
 B_SPLINE_CURVE_WITH_KNOTS ( ( 4, 4 ),
 ( 4.409610424194855050, 5.070003779556289558 ),
 .UNSPECIFIED. ) 
 CURVE ( )  GEOMETRIC_REPRESENTATION_ITEM ( )  RATIONAL_B_SPLINE_CURVE ( ( 1.000000000000000000, 0.9639857288000422963, 0.9639857288000422963, 1.000000000000000000 ) ) 
 REPRESENTATION_ITEM ( '' )  );
#94521 = CARTESIAN_POINT ( 'NONE',  ( 11.60004869885203682, 1425.691286098748606, 137.2109839355661904 ) ) ;
#94522 = CARTESIAN_POINT ( 'NONE',  ( 13.43167025587599817, 1509.382104656720003, 235.1752264429409820 ) ) ;
#94523 = CARTESIAN_POINT ( 'NONE',  ( -4.772433264290000032, 1461.586210710390105, 228.1254610687989839 ) ) ;
#94524 = LINE ( 'NONE', #507, #16747 ) ;
#94525 = ORIENTED_EDGE ( 'NONE', *, *, #102669, .F. ) ;
#94526 = CARTESIAN_POINT ( 'NONE',  ( -1.249564655339530095, 1407.936288853909900, 270.2925089982160216 ) ) ;
#94527 = CARTESIAN_POINT ( 'NONE',  ( 2.865636809105000182, 1516.815173273089840, 207.9858416580370033 ) ) ;
#94528 = CARTESIAN_POINT ( 'NONE',  ( 10.72383926760000072, 1418.448279815129808, 229.9424527573980015 ) ) ;
#94529 = CARTESIAN_POINT ( 'NONE',  ( -2.500000000000000000, 1448.894380913990062, 183.1110264324979937 ) ) ;
#94531 = ORIENTED_EDGE ( 'NONE', *, *, #45442, .T. ) ;
#94530 = CARTESIAN_POINT ( 'NONE',  ( -2.500000000000000000, 1439.390253060799978, 161.6061717842659959 ) ) ;
#94532 = ORIENTED_EDGE ( 'NONE', *, *, #52210, .F. ) ;
#94533 = CARTESIAN_POINT ( 'NONE',  ( -22.76136400371149904, 1409.717529452729877, 209.5657493702119893 ) ) ;
#94534 = CARTESIAN_POINT ( 'NONE',  ( -4.249337494120000613, 1423.895439858529926, 184.8620138466980052 ) ) ;
#94535 = CARTESIAN_POINT ( 'NONE',  ( -12.13574144734536375, 1436.932434855902784, 151.4274810089637526 ) ) ;
#94536 = CARTESIAN_POINT ( 'NONE',  ( -4.579624579470000789, 1427.832655172230034, 112.4493539157979995 ) ) ;
#94537 = AXIS2_PLACEMENT_3D ( 'NONE', #76605, #95068, #43567 ) ;
#94538 = AXIS2_PLACEMENT_3D ( 'NONE', #58162, #101222, #76054 ) ;
#94539 = CARTESIAN_POINT ( 'NONE',  ( -20.57759663809800088, 1493.275265424210147, 192.6373786097109928 ) ) ;
#94540 = CARTESIAN_POINT ( 'NONE',  ( -17.98568901069999981, 1415.860170671229980, 225.2002861224979995 ) ) ;
#94541 = VECTOR ( 'NONE', #110271, 1000.000000000000114 ) ;
#94542 = CARTESIAN_POINT ( 'NONE',  ( 39.10679733682070491, 1459.373169423960007, 268.7147505820800006 ) ) ;
#94543 = CARTESIAN_POINT ( 'NONE',  ( -2.201151872242963492, 1466.932782758140092, 235.2250472885538670 ) ) ;
#94544 = CARTESIAN_POINT ( 'NONE',  ( -16.94111210471653450, 1421.944315043240977, 226.8380784755184152 ) ) ;
#94545 = CARTESIAN_POINT ( 'NONE',  ( -3.461360131404999763, 1516.874084700499907, 205.8683838714370040 ) ) ;
#94546 = ORIENTED_EDGE ( 'NONE', *, *, #42536, .F. ) ;
#94547 = CARTESIAN_POINT ( 'NONE',  ( 18.89223017036711738, 1457.760250004050249, 226.9657477437493185 ) ) ;
#94548 = CARTESIAN_POINT ( 'NONE',  ( 1.523969922190620219, 1455.113528485800089, 183.3838728237819851 ) ) ;
#94549 = CARTESIAN_POINT ( 'NONE',  ( 22.65292971370000075, 1409.704085498430004, 208.9051947466459751 ) ) ;
#94550 = VERTEX_POINT ( 'NONE', #97230 ) ;
#94551 = DIRECTION ( 'NONE',  ( 0.000000000000000000, 0.000000000000000000, 1.000000000000000000 ) ) ;
#94552 = CARTESIAN_POINT ( 'NONE',  ( 24.77492596718960272, 1452.047903808549790, 135.6621443109009988 ) ) ;
#94553 = CARTESIAN_POINT ( 'NONE',  ( -4.948068031382700127, 1508.551704408389924, 212.0494981076920169 ) ) ;
#94554 = CARTESIAN_POINT ( 'NONE',  ( -6.331822530929999360, 1388.284444344999883, 200.8293682005390224 ) ) ;
#94555 = CARTESIAN_POINT ( 'NONE',  ( 7.463794710130000176, 1422.976950754710060, 195.6323374253989869 ) ) ;
#94556 = CARTESIAN_POINT ( 'NONE',  ( 17.69145655820000229, 1410.027806010230051, 193.3443910425980050 ) ) ;
#94557 = CARTESIAN_POINT ( 'NONE',  ( 20.75326766870000128, 1444.324653571829913, 176.0807405191980024 ) ) ;
#94558 = CARTESIAN_POINT ( 'NONE',  ( 3.400285785609643785, 1439.690925502392702, 184.4405085457196662 ) ) ;
#94560 = CARTESIAN_POINT ( 'NONE',  ( -22.76204189940434830, 1432.230029621326366, 215.7233072855924831 ) ) ;
#94559 = CARTESIAN_POINT ( 'NONE',  ( 30.00400320040656510, 1524.843178112495480, 195.9692341599732686 ) ) ;
#94561 = CARTESIAN_POINT ( 'NONE',  ( 1.131322572361280088, 1452.208024494899746, 183.3657943293449932 ) ) ;
#94562 = EDGE_CURVE ( 'NONE', #4626, #30502, #37747, .T. ) ;
#94563 = CARTESIAN_POINT ( 'NONE',  ( -0.01940215194334939802, 1508.902653225929953, 179.5976350532890251 ) ) ;
#94564 = VECTOR ( 'NONE', #107349, 1000.000000000000000 ) ;
#94565 = CARTESIAN_POINT ( 'NONE',  ( 1.363639811660000145, 1415.765555525229956, 232.8698637559979829 ) ) ;
#94566 = ADVANCED_FACE ( 'NONE', ( #20502 ), #63663, .T. ) ;
#94567 = CARTESIAN_POINT ( 'NONE',  ( 17.22592475670000312, 1443.913060387330006, 162.9227486557980171 ) ) ;
#94568 = ORIENTED_EDGE ( 'NONE', *, *, #44686, .T. ) ;
#94569 = CARTESIAN_POINT ( 'NONE',  ( 11.40293847519150106, 1414.971993471370070, 221.9446473240219859 ) ) ;
#94570 = DIRECTION ( 'NONE',  ( -0.6736849260863841948, 0.000000000000000000, 0.7390186874254148774 ) ) ;
#94571 = CARTESIAN_POINT ( 'NONE',  ( -0.3563141984344909696, 1409.037191904199972, 232.3070811437949885 ) ) ;
#94572 = CARTESIAN_POINT ( 'NONE',  ( -12.43426257129999968, 1391.244016237139931, 206.9658053057590053 ) ) ;
#94573 = CARTESIAN_POINT ( 'NONE',  ( -0.1602782174031799067, 1421.018467852183903, 193.7178847131137047 ) ) ;
#94574 = CARTESIAN_POINT ( 'NONE',  ( 0.2545641544693758029, 1506.446781329472969, 231.1141566264156779 ) ) ;
#94575 = CARTESIAN_POINT ( 'NONE',  ( -19.62446893450000118, 1443.054186837209954, 214.3676144197979738 ) ) ;
#94576 = ADVANCED_FACE ( 'NONE', ( #12123 ), #12723, .F. ) ;
#94577 = CARTESIAN_POINT ( 'NONE',  ( -21.41430812654454385, 1509.039033548261386, 191.8384994702369966 ) ) ;
#94578 = CARTESIAN_POINT ( 'NONE',  ( 11.62685186760000100, 1433.421535312869764, 151.0711183502979793 ) ) ;
#94579 = CARTESIAN_POINT ( 'NONE',  ( 21.37693748330000076, 1443.303628179369980, 224.8635562210979799 ) ) ;
#94580 = CARTESIAN_POINT ( 'NONE',  ( 12.71641934408430075, 1415.429375168349907, 196.8674432429739909 ) ) ;
#94581 = CARTESIAN_POINT ( 'NONE',  ( -16.89200104021849924, 1419.273703591249841, 201.3369295748360059 ) ) ;
#94582 = CARTESIAN_POINT ( 'NONE',  ( 22.91663120903140083, 1507.606285602550088, 210.6365840681099826 ) ) ;
#94583 = CARTESIAN_POINT ( 'NONE',  ( 24.86520269990570142, 1436.144666160072575, 137.8610266872903196 ) ) ;
#94584 = CARTESIAN_POINT ( 'NONE',  ( 22.58840255639999839, 1409.701846760530088, 208.8102578915460015 ) ) ;
#94585 = CARTESIAN_POINT ( 'NONE',  ( 10.57127173870284054, 1398.226368140626164, 201.5218381721108756 ) ) ;
#94586 = CARTESIAN_POINT ( 'NONE',  ( -21.61785201490240027, 1509.681104934679979, 231.5207931856990058 ) ) ;
#94587 = AXIS2_PLACEMENT_3D ( 'NONE', #17604, #51804, #103270 ) ;
#94588 = CARTESIAN_POINT ( 'NONE',  ( -8.040086649609909486, 1425.809972356560820, 207.7969723859449687 ) ) ;
#94589 = B_SPLINE_CURVE_WITH_KNOTS ( 'NONE', 3,
 ( #36094, #70280, #45619, #62991, #18706, #70834, #28235, #96548, #79759, #104389, #37740, #27686, #62422, #87604, #61870, #105501, #46170, #95988, #88156, #71389, #53459, #10892, #45065 ),
 .UNSPECIFIED., .F., .F.,
 ( 4, 2, 2, 1, 2, 2, 2, 2, 2, 2, 2, 4 ),
 ( 0.000000000000000000, 0.1249999999998680222, 0.1874999999999092115, 0.2187499999998207545, 0.2343749999997765676, 0.2499999999997324085, 0.3749999999997780109, 0.4999999999998235856, 0.6249999999998692157, 0.6874999999998908651, 0.7499999999999124034, 1.000000000000000000 ),
 .UNSPECIFIED. ) ;
#94590 = CARTESIAN_POINT ( 'NONE',  ( -0.6463351481710662982, 1477.515498289491234, 198.7392143834898661 ) ) ;
#94591 = CARTESIAN_POINT ( 'NONE',  ( -8.664500300950001233, 1509.043687291729839, 236.1803262411980029 ) ) ;
#94592 = CARTESIAN_POINT ( 'NONE',  ( 3.406450987864870328, 1507.508084575899829, 220.3277226881679951 ) ) ;
#94593 = ADVANCED_FACE ( 'NONE', ( #35095 ), #59766, .T. ) ;
#94594 = CARTESIAN_POINT ( 'NONE',  ( -4.705736713569160123, 1479.984769566100113, 230.9466532730550057 ) ) ;
#94595 = CARTESIAN_POINT ( 'NONE',  ( 2.491188358395000080, 1516.733363207009916, 213.1488973760370129 ) ) ;
#94596 = CARTESIAN_POINT ( 'NONE',  ( -10.59625218578830008, 1423.662071466640100, 204.3772360533070014 ) ) ;
#94597 = CARTESIAN_POINT ( 'NONE',  ( 0.1603187917380029803, 1486.074899099739923, 181.8333893279200026 ) ) ;
#94598 = ADVANCED_FACE ( 'NONE', ( #101732 ), #92871, .F. ) ;
#94600 = VERTEX_POINT ( 'NONE', #51912 ) ;
#94599 = CARTESIAN_POINT ( 'NONE',  ( 5.365832140090000202, 1437.051389308390071, 208.1168906416689879 ) ) ;
#94601 = CARTESIAN_POINT ( 'NONE',  ( -0.9044596104409999837, 1416.819760301830001, 228.0287517993979804 ) ) ;
#94602 = AXIS2_PLACEMENT_3D ( 'NONE', #23011, #99164, #82933 ) ;
#94603 = PRESENTATION_LAYER_ASSIGNMENT (  '', '', ( #60686 ) ) ;
#94604 = FACE_OUTER_BOUND ( 'NONE', #61466, .T. ) ;
#94605 = CARTESIAN_POINT ( 'NONE',  ( 13.50077136620000040, 1434.968960439809962, 149.6996353846979844 ) ) ;
#94606 = CARTESIAN_POINT ( 'NONE',  ( -32.28351601132079196, 1524.972613296805093, 217.0406166517271060 ) ) ;
#94607 = CARTESIAN_POINT ( 'NONE',  ( 4.677526816337639559, 1434.888920963079954, 228.7640148925319750 ) ) ;
#94608 = ORIENTED_EDGE ( 'NONE', *, *, #27920, .T. ) ;
#94609 = B_SPLINE_SURFACE_WITH_KNOTS ( 'NONE', 5, 1, ( 
 ( #31956, #73430 ),
 ( #106467, #90197 ),
 ( #66149, #91864 ),
 ( #38700, #23552 ),
 ( #31403, #89657 ),
 ( #57743, #15137 ),
 ( #107564, #12943 ),
 ( #80721, #4029 ),
 ( #99144, #98053 ) ),
 .UNSPECIFIED., .F., .F., .F.,
 ( 6, 3, 6 ),
 ( 2, 2 ),
 ( 0.000000000000000000, 3.695647608739999868, 7.374251186729999574 ),
 ( 0.000000000000000000, 14.00000000000000000 ),
 .UNSPECIFIED. ) ;
#94610 = DIRECTION ( 'NONE',  ( 0.000000000000000000, 2.960594732333748082E-13, -1.000000000000000000 ) ) ;
#94611 = CARTESIAN_POINT ( 'NONE',  ( -14.43963703662210030, 1380.159948612549897, 209.0189137943660000 ) ) ;
#94612 = CARTESIAN_POINT ( 'NONE',  ( 9.046284717930422659, 1449.608882353234549, 207.3630802585645938 ) ) ;
#94613 = CARTESIAN_POINT ( 'NONE',  ( -3.313501335607589748, 1397.551704408390151, 203.0565224509919915 ) ) ;
#94615 = EDGE_CURVE ( 'NONE', #29914, #99683, #1508, .T. ) ;
#94614 = CARTESIAN_POINT ( 'NONE',  ( -4.881632653818110512, 1434.082703436370139, 217.0349096382250025 ) ) ;
#94616 = CARTESIAN_POINT ( 'NONE',  ( -108.6923101465634716, 1381.634892108574377, 310.5848204547120304 ) ) ;
#94617 = B_SPLINE_CURVE_WITH_KNOTS ( 'NONE', 3,
 ( #63211, #14398, #48592, #48028, #38509, #89472, #82726, #72688, #81065, #73228, #5465, #31216, #20588, #73794, #82166, #63745, #88919, #30102, #12205, #65398, #39048, #6016, #64852, #30667, #39626, #107921, #90013, #81605, #98962, #97318, #12768, #54787, #90564, #3847, #64297, #13290, #46400, #80532, #37974, #72156, #106274, #23358, #101155, #16046, #49142, #109586, #108479, #8201, #23896, #31762, #102269, #25548, #93317, #83821, #100612, #59740, #7121, #49692, #41820, #84909, #110673, #42368, #50776, #109043, #57549, #41276, #91672, #33966, #84377, #32856, #74352, #24449, #67048, #75451, #40170, #50247, #58091, #24996 ),
 .UNSPECIFIED., .F., .F.,
 ( 4, 2, 2, 1, 1, 1, 1, 2, 2, 2, 1, 1, 1, 1, 1, 2, 2, 2, 2, 1, 1, 1, 2, 2, 2, 1, 1, 1, 1, 1, 2, 2, 2, 2, 2, 1, 1, 1, 1, 2, 2, 2, 2, 1, 1, 1, 2, 2, 2, 2, 4 ),
 ( 0.000000000000000000, 0.06249999999905236914, 0.09374999999857999700, 0.1093749999983438387, 0.1171874999982358140, 0.1210937499981719484, 0.1230468749981302318, 0.1240234374981080828, 0.1249999999980859339, 0.1874999999981248888, 0.2187499999981443732, 0.2343749999981540599, 0.2421874999981687426, 0.2460937499981760701, 0.2480468749981797338, 0.2490234374981733778, 0.2499999999981670773, 0.3749999999993307576, 0.4374999999999126810, 0.4687500000002036704, 0.4843750000003492207, 0.4921875000004325429, 0.4960937500004755085, 0.5000000000005184742, 0.6250000000021559421, 0.6875000000029746205, 0.7187500000033728575, 0.7343750000035703662, 0.7421875000036677328, 0.7460937500037260195, 0.7480468750037470027, 0.7500000000037678749, 0.8125000000041449066, 0.8437500000043415271, 0.8593750000044494408, 0.8671875000045020654, 0.8710937500045184967, 0.8730468750045379256, 0.8740234375045391468, 0.8745117187545383697, 0.8750000000045374815, 0.8906250000045405901, 0.8984375000045421444, 0.9023437500045430326, 0.9042968750045285997, 0.9052734375045072834, 0.9057617187544817483, 0.9062500000044562132, 0.9218750000037139181, 0.9375000000029716229, 1.000000000000000000 ),
 .UNSPECIFIED. ) ;
#94618 = CARTESIAN_POINT ( 'NONE',  ( -16.26800630319999641, 1422.453322322420036, 210.2998271891489992 ) ) ;
#94619 = CARTESIAN_POINT ( 'NONE',  ( 0.000000000000000000, 1511.187213306747708, 209.1218459616979999 ) ) ;
#94620 = CARTESIAN_POINT ( 'NONE',  ( -12.54019733330000008, 1391.397793261360221, 209.7548870936209937 ) ) ;
#94621 = B_SPLINE_SURFACE_WITH_KNOTS ( 'NONE', 5, 5, ( 
 ( #44149, #34626, #68810, #41931, #102912, #26211 ),
 ( #67700, #93420, #17794, #76087, #42471, #1053 ),
 ( #35178, #18909, #76629, #27328, #78284, #1597 ),
 ( #59847, #51994, #9428, #93971, #43592, #35734 ),
 ( #77740, #69922, #61513, #89857, #70474, #99340 ),
 ( #45264, #107211, #87814, #44707, #47311, #13127 ) ),
 .UNSPECIFIED., .F., .F., .F.,
 ( 6, 6 ),
 ( 6, 6 ),
 ( 30.40177460640000007, 157.7844419379999863 ),
 ( -6.938893903909999252E-17, 1.000000000000000000 ),
 .UNSPECIFIED. ) ;
#94622 = CARTESIAN_POINT ( 'NONE',  ( -71.90449437803688681, 1385.121734512539888, 269.7491603056169538 ) ) ;
#94623 = CARTESIAN_POINT ( 'NONE',  ( -17.53497677579999703, 1411.915013305630055, 192.5944228452979985 ) ) ;
#94624 = CARTESIAN_POINT ( 'NONE',  ( 10.62762824711120224, 1422.391620394080064, 210.1053338132739725 ) ) ;
#94625 = VERTEX_POINT ( 'NONE', #67618 ) ;
#94626 = EDGE_CURVE ( 'NONE', #57348, #94097, #100319, .T. ) ;
#94627 = CARTESIAN_POINT ( 'NONE',  ( 12.93811130839999812, 1442.831169986189934, 169.4238961894979809 ) ) ;
#94629 = ORIENTED_EDGE ( 'NONE', *, *, #24066, .T. ) ;
#94628 = DIRECTION ( 'NONE',  ( -0.05876148091703057436, 0.002052003564324334384, 0.9982699422710319404 ) ) ;
#94630 = CARTESIAN_POINT ( 'NONE',  ( 6.970868710793260092, 1466.504179844829878, 216.1871911102630008 ) ) ;
#94631 = AXIS2_PLACEMENT_3D ( 'NONE', #38987, #22169, #107854 ) ;
#94632 = EDGE_LOOP ( 'NONE', ( #106547, #100909, #3973, #89853 ) ) ;
#94633 = CARTESIAN_POINT ( 'NONE',  ( 19.32263322520000060, 1455.378559704889767, 209.1218459616989946 ) ) ;
#94634 = CARTESIAN_POINT ( 'NONE',  ( -8.318057838368259738, 1363.950293616733916, 210.6218459617142003 ) ) ;
#94635 = CARTESIAN_POINT ( 'NONE',  ( -11.37447413379999972, 1491.756880625089934, 205.6190363507990071 ) ) ;
#94636 = CARTESIAN_POINT ( 'NONE',  ( 1.114882633370010031E-09, 1467.056812769279986, 237.6398032221420067 ) ) ;
#94637 = DIRECTION ( 'NONE',  ( 0.000000000000000000, -1.000000000000000000, 0.000000000000000000 ) ) ;
#94638 = CARTESIAN_POINT ( 'NONE',  ( 19.02416918379194044, 1437.840865032662805, 213.1984861927293480 ) ) ;
#94639 = CARTESIAN_POINT ( 'NONE',  ( -9108.204429824800172, -2340.220200558880151, -1569.808522337019895 ) ) ;
#94640 = CARTESIAN_POINT ( 'NONE',  ( -5.189380558823482481, 1516.874058588360640, 214.5460175109637362 ) ) ;
#94641 = CARTESIAN_POINT ( 'NONE',  ( -4.155669664704369382, 1439.704322410719897, 185.4969487652249995 ) ) ;
#94642 = CARTESIAN_POINT ( 'NONE',  ( -7.052101012867634466, 1370.311329506408583, 209.6218459617033432 ) ) ;
#94643 = B_SPLINE_CURVE_WITH_KNOTS ( 'NONE', 5,
 ( #11870, #46042, #63409, #97524, #16239, #91322 ),
 .UNSPECIFIED., .F., .F.,
 ( 6, 6 ),
 ( 0.000000000000000000, 1.000000000000000000 ),
 .UNSPECIFIED. ) ;
#94644 = EDGE_CURVE ( 'NONE', #76907, #51033, #25161, .T. ) ;
#94645 = CARTESIAN_POINT ( 'NONE',  ( 1.779428958460000265, 1456.357349049189907, 198.6855221643990035 ) ) ;
#94646 = CARTESIAN_POINT ( 'NONE',  ( 1.700706776364999895, 1516.923170579120097, 206.8211163054370161 ) ) ;
#94647 = AXIS2_PLACEMENT_3D ( 'NONE', #77629, #59193, #26656 ) ;
#94648 = CARTESIAN_POINT ( 'NONE',  ( 2.500000005440000006, 1448.104721459739949, 157.8850530793979772 ) ) ;
#94649 = EDGE_CURVE ( 'NONE', #22078, #12048, #76518, .T. ) ;
#94650 = B_SPLINE_SURFACE_WITH_KNOTS ( 'NONE', 5, 1, ( 
 ( #34603, #58167 ),
 ( #41907, #77719 ),
 ( #68789, #102350 ),
 ( #16664, #94497 ),
 ( #76607, #50861 ),
 ( #32937, #26186 ),
 ( #60376, #17768 ),
 ( #51972, #9407 ),
 ( #37374, #45243 ) ),
 .UNSPECIFIED., .F., .F., .F.,
 ( 6, 3, 6 ),
 ( 2, 2 ),
 ( 0.000000000000000000, 8.334083717689999560, 16.69887895509999964 ),
 ( 0.000000000000000000, 14.00000000000000000 ),
 .UNSPECIFIED. ) ;
#94651 = LINE ( 'NONE', #70048, #28312 ) ;
#94652 = CARTESIAN_POINT ( 'NONE',  ( -3.370189795129999943, 1496.076862149890076, 198.0269955820990049 ) ) ;
#94654 = ORIENTED_EDGE ( 'NONE', *, *, #73891, .T. ) ;
#94653 = CARTESIAN_POINT ( 'NONE',  ( -2.231199251659999661, 1495.993596543689819, 220.2514328137989992 ) ) ;
#94655 = CARTESIAN_POINT ( 'NONE',  ( 21.01415622463857247, 1517.151704408390060, 200.8719909741391803 ) ) ;
#94656 = ORIENTED_EDGE ( 'NONE', *, *, #34393, .T. ) ;
#94657 = CARTESIAN_POINT ( 'NONE',  ( -16.58691043322057368, 1514.105081324218872, 223.2867520483846420 ) ) ;
#94658 = CARTESIAN_POINT ( 'NONE',  ( -23.88743783630000195, 1410.917949452529911, 207.8246455712279896 ) ) ;
#94660 = CARTESIAN_POINT ( 'NONE',  ( 16.21964127711080295, 1409.479387927570087, 193.0992798958739911 ) ) ;
#94659 = CARTESIAN_POINT ( 'NONE',  ( -10.35833152844089966, 1425.137813717620020, 115.9780672966650030 ) ) ;
#94661 = CARTESIAN_POINT ( 'NONE',  ( -7.708745685915000756, 1516.523379810429788, 210.8299382363969983 ) ) ;
#94662 = CARTESIAN_POINT ( 'NONE',  ( 28.80933051664284861, 1510.030156971867427, 200.7517252896445257 ) ) ;
#94663 = DIRECTION ( 'NONE',  ( 0.9510565162951561957, 0.000000000000000000, 0.3090169943749392911 ) ) ;
#94664 = AXIS2_PLACEMENT_3D ( 'NONE', #68776, #1017, #109653 ) ;
#94665 = CARTESIAN_POINT ( 'NONE',  ( -30.10636673460000168, 1413.645518868930139, 266.8104471709979748 ) ) ;
#94666 = CARTESIAN_POINT ( 'NONE',  ( -12.84384240866459947, 1379.221145577220113, 208.6845722232019966 ) ) ;
#94667 = CARTESIAN_POINT ( 'NONE',  ( 17.47747713618334942, 1459.994120045239242, 228.4137988842376217 ) ) ;
#94668 = ITEM_DEFINED_TRANSFORMATION ( 'NONE', 'NONE', #59323,  #21632 ) ;
#94669 = CARTESIAN_POINT ( 'NONE',  ( -5.076113882490000506, 1391.871667423589997, 214.6636951175890147 ) ) ;
#94670 = CARTESIAN_POINT ( 'NONE',  ( -35.83369766294850223, 1437.372084409380022, 136.5363233108159875 ) ) ;
#94671 = VERTEX_POINT ( 'NONE', #103955 ) ;
#94672 = CARTESIAN_POINT ( 'NONE',  ( 6.700735663969999756, 1396.147055234629988, 199.0043882911979836 ) ) ;
#94673 = CARTESIAN_POINT ( 'NONE',  ( -19.52647806210000070, 1464.795176723290069, 212.0690861509589809 ) ) ;
#94674 = CARTESIAN_POINT ( 'NONE',  ( -17.12355492049999839, 1460.407125116229736, 228.2713570448979965 ) ) ;
#94675 = VERTEX_POINT ( 'NONE', #9893 ) ;
#94676 = VERTEX_POINT ( 'NONE', #54689 ) ;
#94677 = CARTESIAN_POINT ( 'NONE',  ( -2.431412526649999961, 1428.647745098929818, 149.4227846719979880 ) ) ;
#94678 = CARTESIAN_POINT ( 'NONE',  ( -11.76196305498579875, 1425.587148902949821, 146.3422030814200241 ) ) ;
#94679 = ORIENTED_EDGE ( 'NONE', *, *, #37851, .T. ) ;
#94680 = CARTESIAN_POINT ( 'NONE',  ( -12.39098292546499991, 1517.051704408389924, 199.8633830690170043 ) ) ;
#94681 = CARTESIAN_POINT ( 'NONE',  ( -9.765242783855931918, 1418.346146421839194, 197.2107663835972176 ) ) ;
#94682 = CARTESIAN_POINT ( 'NONE',  ( -11.87239127897699831, 1432.808531436009844, 149.9811485733590075 ) ) ;
#94683 = CIRCLE ( 'NONE', #101778, 10.00000000000000000 ) ;
#94684 = DIRECTION ( 'NONE',  ( 0.9824080081115912355, 0.000000000000000000, 0.1867471702549089174 ) ) ;
#94685 = CARTESIAN_POINT ( 'NONE',  ( 7.512750234439120156, 1509.038617475950105, 203.6086461444880058 ) ) ;
#94686 = CARTESIAN_POINT ( 'NONE',  ( 9.194133702223101778, 1450.204357222580029, 208.5217520979160213 ) ) ;
#94687 = FACE_OUTER_BOUND ( 'NONE', #84393, .T. ) ;
#94688 = CARTESIAN_POINT ( 'NONE',  ( -92.29727215281390329, 1384.847535221339967, 293.8106274702879546 ) ) ;
#94689 = VERTEX_POINT ( 'NONE', #60884 ) ;
#94690 = CARTESIAN_POINT ( 'NONE',  ( -1.709358701255000001, 1516.542957540330008, 202.1882582765869927 ) ) ;
#94691 = CARTESIAN_POINT ( 'NONE',  ( -5.781585816274999345, 1516.939646076049939, 209.1342929058909874 ) ) ;
#94692 = ORIENTED_EDGE ( 'NONE', *, *, #5258, .T. ) ;
#94693 = CARTESIAN_POINT ( 'NONE',  ( 11.80334487768269902, 1428.396969778590119, 148.3489976931730041 ) ) ;
#94694 = CARTESIAN_POINT ( 'NONE',  ( 4.583898368691166070, 1511.400233449630605, 217.5067962340223744 ) ) ;
#94695 = ORIENTED_EDGE ( 'NONE', *, *, #78879, .F. ) ;
#94696 = CARTESIAN_POINT ( 'NONE',  ( 29.00779973304130266, 1526.382868172863937, 200.9494832830834810 ) ) ;
#94697 = CARTESIAN_POINT ( 'NONE',  ( -13.31869796660000027, 1443.086052842849995, 169.3753098992980028 ) ) ;
#94698 = CARTESIAN_POINT ( 'NONE',  ( 11.34707687579999913, 1509.309309043230087, 235.7409118476979870 ) ) ;
#94699 = CARTESIAN_POINT ( 'NONE',  ( -9.816650044347928983, 1461.735905517830133, 208.1390970106120051 ) ) ;
#94700 = CARTESIAN_POINT ( 'NONE',  ( -6.205088089679999364, 1421.916341492230003, 186.7344349734979971 ) ) ;
#94701 = CIRCLE ( 'NONE', #78648, 1.000000000000000888 ) ;
#94702 = CARTESIAN_POINT ( 'NONE',  ( 4.235651746019999386, 1408.707576597030084, 270.4270856384979993 ) ) ;
#94703 = CARTESIAN_POINT ( 'NONE',  ( 4.487357219410602838, 1509.034509700537683, 206.0057024814164777 ) ) ;
#94704 = CARTESIAN_POINT ( 'NONE',  ( -6.479645409570000680, 1473.991665852890037, 200.1438768917790014 ) ) ;
#94705 = CARTESIAN_POINT ( 'NONE',  ( -16.50765472400000178, 1379.592255418909872, 208.3681221328770050 ) ) ;
#94706 = CARTESIAN_POINT ( 'NONE',  ( 24.33627900605520011, 1451.288492182929986, 206.2143456058219897 ) ) ;
#94708 = DIRECTION ( 'NONE',  ( -1.755985294532469921E-16, 1.000000000000000000, -1.338183447452831989E-16 ) ) ;
#94707 = CARTESIAN_POINT ( 'NONE',  ( -4.503834590931400150, 1496.999185789959938, 198.8010291948349959 ) ) ;
#94709 = CARTESIAN_POINT ( 'NONE',  ( -4.636078765298575100, 1423.706159026812657, 184.4443473542607990 ) ) ;
#94710 = EDGE_CURVE ( 'NONE', #47910, #35107, #57430, .T. ) ;
#94711 = CARTESIAN_POINT ( 'NONE',  ( -17.68237282055029880, 1517.151704408390060, 205.6847408665509818 ) ) ;
#94712 = CARTESIAN_POINT ( 'NONE',  ( -2.152516339165368109, 1506.379860764218165, 187.2722548778648104 ) ) ;
#94713 = EDGE_LOOP ( 'NONE', ( #42859, #72106, #63335, #72028 ) ) ;
#94714 = AXIS2_PLACEMENT_3D ( 'NONE', #13306, #81625, #91140 ) ;
#94715 = CARTESIAN_POINT ( 'NONE',  ( 29.35072644275232179, 1526.211528530236592, 197.7230832643897713 ) ) ;
#94716 = DIRECTION ( 'NONE',  ( -1.000000000000000000, 0.000000000000000000, 0.000000000000000000 ) ) ;
#94717 = CARTESIAN_POINT ( 'NONE',  ( -2.913081468028484000, 1484.790404518151718, 183.2223388818480316 ) ) ;
#94718 = CARTESIAN_POINT ( 'NONE',  ( -17.60616670766113856, 1410.892144164382898, 193.1022257080302893 ) ) ;
#94720 = ORIENTED_EDGE ( 'NONE', *, *, #23393, .T. ) ;
#94719 = CARTESIAN_POINT ( 'NONE',  ( 0.5750010241369649666, 1515.139742041519867, 204.7943597985580197 ) ) ;
#94721 = CARTESIAN_POINT ( 'NONE',  ( 0.5928098971900001013, 1489.480617679929765, 187.2733462026980078 ) ) ;
#94722 = CARTESIAN_POINT ( 'NONE',  ( -2.163895355619999794, 1508.493132411889974, 220.4958316090989854 ) ) ;
#94723 = EDGE_CURVE ( 'NONE', #54088, #23279, #52058, .T. ) ;
#94724 = CARTESIAN_POINT ( 'NONE',  ( -11.82919182880000086, 1429.685437959029969, 149.7801030883980218 ) ) ;
#94725 = CARTESIAN_POINT ( 'NONE',  ( -10.83059686145892186, 1424.984354290685587, 145.3974420532384499 ) ) ;
#94726 = CARTESIAN_POINT ( 'NONE',  ( -10.76971639860709828, 1461.755917255409940, 211.3234507930380062 ) ) ;
#94727 = CARTESIAN_POINT ( 'NONE',  ( -4.993214560040000194, 1391.653934889589891, 203.5347113830289913 ) ) ;
#94728 = EDGE_CURVE ( 'NONE', #24039, #9564, #19945, .T. ) ;
#94729 = CARTESIAN_POINT ( 'NONE',  ( -2.038646110889678287, 1525.960063244516959, 241.1857569150893994 ) ) ;
#94730 = CARTESIAN_POINT ( 'NONE',  ( -16.44381314316499854, 1512.620989416249813, 222.6384675079670217 ) ) ;
#94731 = CARTESIAN_POINT ( 'NONE',  ( 1.285879139104720042E-15, 1391.913060387289988, 209.1218459572589836 ) ) ;
#94732 = CARTESIAN_POINT ( 'NONE',  ( -11.31630330039999954, 1480.636685083989732, 212.6825498069390221 ) ) ;
#94733 = CARTESIAN_POINT ( 'NONE',  ( -15.80613827389999670, 1459.265199882230036, 230.3675922840980093 ) ) ;
#94734 = AXIS2_PLACEMENT_3D ( 'NONE', #66437, #64792, #100553 ) ;
#94735 = CARTESIAN_POINT ( 'NONE',  ( -7.337793750624999944, 1517.145312756229941, 206.2496372219370073 ) ) ;
#94736 = CARTESIAN_POINT ( 'NONE',  ( 18.38362700379999737, 1408.577091670229947, 267.3950545271980559 ) ) ;
#94737 = CARTESIAN_POINT ( 'NONE',  ( 2.219943740554563227, 1464.863888248525654, 237.3912208037882294 ) ) ;
#94738 = CARTESIAN_POINT ( 'NONE',  ( 20.68393032789999708, 1449.727573619960140, 194.8750444304980078 ) ) ;
#94739 = CARTESIAN_POINT ( 'NONE',  ( -23.01365769190000066, 1432.948698623059954, 214.9133548742180153 ) ) ;
#94740 = CARTESIAN_POINT ( 'NONE',  ( -0.09392903680032700653, 1507.117918406099989, 237.3493018655460105 ) ) ;
#94741 = FACE_OUTER_BOUND ( 'NONE', #8968, .T. ) ;
#94742 = CARTESIAN_POINT ( 'NONE',  ( 20.59269117493390056, 1507.766073655780019, 227.7908423917359926 ) ) ;
#94743 = CARTESIAN_POINT ( 'NONE',  ( -6.294750357631860638, 1408.079328830519898, 197.5408074016749822 ) ) ;
#94744 = CARTESIAN_POINT ( 'NONE',  ( -18.88659680459999990, 1416.522662136229883, 207.5785872533780037 ) ) ;
#94745 = CIRCLE ( 'NONE', #16070, 1.000002395586160775 ) ;
#94746 = CARTESIAN_POINT ( 'NONE',  ( -12.54789821530000005, 1442.763165783939940, 186.3817407933979950 ) ) ;
#94747 = ADVANCED_FACE ( 'NONE', ( #79874 ), #5494, .T. ) ;
#94748 = CARTESIAN_POINT ( 'NONE',  ( -3.703568358935259930, 1497.311626042180023, 220.9591690318370070 ) ) ;
#94749 = CARTESIAN_POINT ( 'NONE',  ( 18.20044471017449794, 1429.674601861270048, 208.8920640582719841 ) ) ;
#94750 = CARTESIAN_POINT ( 'NONE',  ( 26.02835829290000191, 1413.547636220630011, 269.9886483863980402 ) ) ;
#94751 = VERTEX_POINT ( 'NONE', #107264 ) ;
#94752 = EDGE_CURVE ( 'NONE', #106368, #27485, #17534, .T. ) ;
#94753 = CARTESIAN_POINT ( 'NONE',  ( -5.513435705061030312, 1509.038615938849944, 201.6090957135359929 ) ) ;
#94754 = CARTESIAN_POINT ( 'NONE',  ( -10.61798429165910029, 1409.283848569250040, 198.5915965930109905 ) ) ;
#94755 = B_SPLINE_SURFACE_WITH_KNOTS ( 'NONE', 5, 5, ( 
 ( #32029, #34230, #83523, #17400, #76240, #110387 ),
 ( #6277, #66218, #23625, #100337, #85179, #6817 ),
 ( #57808, #91932, #92470, #109303, #15206, #7922 ),
 ( #100865, #16299, #49396, #68416, #40976, #109846 ),
 ( #75156, #32589, #66765, #24156, #15741, #84080 ),
 ( #51046, #7378, #76791, #67310, #101407, #24698 ),
 ( #50503, #84625, #42092, #69524, #26942, #68970 ),
 ( #18508, #87967, #2321, #104745, #36431, #61131 ),
 ( #95245, #43198, #96905, #28033, #87403, #60567 ) ),
 .UNSPECIFIED., .F., .F., .F.,
 ( 6, 3, 6 ),
 ( 6, 6 ),
 ( 0.000000000000000000, 5.089590486009999637, 11.22315645349999969 ),
 ( 0.000000000000000000, 1.000000000000000000 ),
 .UNSPECIFIED. ) ;
#94757 = EDGE_CURVE ( 'NONE', #43960, #73303, #199, .T. ) ;
#94756 = CARTESIAN_POINT ( 'NONE',  ( -11.62069880129860167, 1507.830664569160263, 207.5518378911060040 ) ) ;
#94758 = CARTESIAN_POINT ( 'NONE',  ( 20.49599333844873783, 1525.960063244516959, 233.8638087104922931 ) ) ;
#94759 = CARTESIAN_POINT ( 'NONE',  ( -7.085472565520000821, 1475.647693041629964, 268.4624854401979519 ) ) ;
#94760 = CARTESIAN_POINT ( 'NONE',  ( 29.85692247043846237, 1525.159196711359755, 196.1177113527152187 ) ) ;
#94761 = CARTESIAN_POINT ( 'NONE',  ( 0.3192358074811350033, 1419.260587148479772, 184.5597205914540098 ) ) ;
#94762 = CARTESIAN_POINT ( 'NONE',  ( 18.02577102991580205, 1424.483463156160042, 224.6203623841139745 ) ) ;
#94763 = CARTESIAN_POINT ( 'NONE',  ( -60.62730084387049345, 1384.693337083439928, 282.0175979611260004 ) ) ;
#94764 = CARTESIAN_POINT ( 'NONE',  ( -5.511153256349440532, 1374.913063729909936, 214.9361186106310129 ) ) ;
#94765 = CARTESIAN_POINT ( 'NONE',  ( 11.74953517310929918, 1415.393085341090000, 223.0700735755810058 ) ) ;
#94766 = EDGE_CURVE ( 'NONE', #41878, #42556, #10835, .T. ) ;
#94767 = DIRECTION ( 'NONE',  ( 1.755985294532464991E-16, -1.000000000000000000, 1.338183447452830017E-16 ) ) ;
#94768 = CARTESIAN_POINT ( 'NONE',  ( -18.98249322452759813, 1526.382868172864164, 185.2725498412215188 ) ) ;
#94769 = CARTESIAN_POINT ( 'NONE',  ( -9.094910833689999308, 1384.931037369060050, 199.9427862008689942 ) ) ;
#94770 = CARTESIAN_POINT ( 'NONE',  ( -22.93992789289999834, 1409.878607768230040, 206.3744506774879994 ) ) ;
#94771 = CARTESIAN_POINT ( 'NONE',  ( 17.76192431929999671, 1416.216739748630062, 206.2762435944279957 ) ) ;
#94772 = CARTESIAN_POINT ( 'NONE',  ( 3.645289263010000003, 1485.122998769089918, 219.6252413598990074 ) ) ;
#94773 = CIRCLE ( 'NONE', #100127, 2.000000000000003553 ) ;
#94774 = CARTESIAN_POINT ( 'NONE',  ( 10.63291962098290000, 1480.187357847879866, 208.2421106722409831 ) ) ;
#94775 = B_SPLINE_SURFACE_WITH_KNOTS ( 'NONE', 5, 5, ( 
 ( #107454, #93810, #81690, #106901, #7620, #59697 ),
 ( #98502, #33363, #13378, #30187, #30749, #42331 ),
 ( #41778, #84330, #48122, #4997, #16002, #73317 ),
 ( #17089, #55971, #93277, #82261, #64930, #50731 ),
 ( #73876, #67004, #21770, #110635, #51281, #99043 ),
 ( #67556, #64380, #32817, #90095, #22321, #76483 ),
 ( #56523, #39712, #90650, #101114, #5561, #84864 ),
 ( #108004, #24410, #101659, #50205, #58595, #92726 ),
 ( #75933, #8162, #33920, #68115, #4465, #102228 ) ),
 .UNSPECIFIED., .F., .F., .F.,
 ( 6, 3, 6 ),
 ( 6, 6 ),
 ( 2.932875705070239647, 5.043863234400000728, 7.154850763719760032 ),
 ( -0.0004325517097626320083, 2.000000000000000000 ),
 .UNSPECIFIED. ) ;
#94776 = CARTESIAN_POINT ( 'NONE',  ( 1.650293394300000216, 1438.194204504490017, 150.5634062101979964 ) ) ;
#94777 = CARTESIAN_POINT ( 'NONE',  ( -3.250062279909999852, 1451.275148989389891, 188.5377248918989892 ) ) ;
#94778 = CARTESIAN_POINT ( 'NONE',  ( -4.019735481675231092, 1515.589562461625064, 209.7439076584321356 ) ) ;
#94779 = CARTESIAN_POINT ( 'NONE',  ( -22.15968219182800070, 1485.573411980050196, 217.2083784210080069 ) ) ;
#94781 = CARTESIAN_POINT ( 'NONE',  ( -7.989567385690000023, 1384.306347471770096, 199.5291465469090042 ) ) ;
#94780 = CARTESIAN_POINT ( 'NONE',  ( -23.10442739089999975, 1411.095127590530183, 210.9251608893080174 ) ) ;
#94782 = CARTESIAN_POINT ( 'NONE',  ( 11.71397520463430020, 1426.710800257239953, 142.5191138725960229 ) ) ;
#94783 = CARTESIAN_POINT ( 'NONE',  ( 21.63849897547177292, 1517.051704408389924, 202.6852139837136804 ) ) ;
#94784 = CIRCLE ( 'NONE', #109107, 2.000000000000001776 ) ;
#94785 = CARTESIAN_POINT ( 'NONE',  ( -10.81369826949999968, 1491.706306174490010, 211.2949660241190202 ) ) ;
#94786 = ADVANCED_FACE ( 'NONE', ( #32759 ), #76420, .T. ) ;
#94787 = CARTESIAN_POINT ( 'NONE',  ( -30.60907494343237190, 1526.073429442291854, 201.6841126651373770 ) ) ;
#94788 = CARTESIAN_POINT ( 'NONE',  ( -16.49511036701739997, 1507.275788732180217, 224.7012778065829934 ) ) ;
#94789 = CARTESIAN_POINT ( 'NONE',  ( -1.130607502004999931, 1516.632821972880038, 202.5736453444569918 ) ) ;
#94790 = CARTESIAN_POINT ( 'NONE',  ( -4.672678730482617837, 1398.052343473715382, 221.2534302702293019 ) ) ;
#94791 = DIRECTION ( 'NONE',  ( 0.4794255386042040601, 0.000000000000000000, 0.8775825618903722036 ) ) ;
#94792 = CARTESIAN_POINT ( 'NONE',  ( 16.68551868298740004, 1431.393131126370008, 216.7641592467800251 ) ) ;
#94793 = CARTESIAN_POINT ( 'NONE',  ( -19.21352096260000053, 1449.658915334390258, 194.0202163047979980 ) ) ;
#94794 = EDGE_CURVE ( 'NONE', #108598, #62493, #93746, .T. ) ;
#94795 = AXIS2_PLACEMENT_3D ( 'NONE', #12265, #31827, #98476 ) ;
#94796 = FILL_AREA_STYLE ('',( #60668 ) ) ;
#94797 = CARTESIAN_POINT ( 'NONE',  ( -11.36959371680000075, 1503.847165134090119, 207.0750569533189775 ) ) ;
#94799 = EDGE_LOOP ( 'NONE', ( #2848, #44232, #7908, #51659 ) ) ;
#94798 = CARTESIAN_POINT ( 'NONE',  ( -62.68882714082580065, 1379.739779185960060, 270.6182910835300390 ) ) ;
#94800 = ORIENTED_EDGE ( 'NONE', *, *, #14548, .T. ) ;
#94801 = CARTESIAN_POINT ( 'NONE',  ( 11.25336247954099989, 1434.059297280159853, 151.5716172890120106 ) ) ;
#94802 = CARTESIAN_POINT ( 'NONE',  ( 28.65660564130000054, 1509.914370929529923, 215.8254011786380033 ) ) ;
#94803 = ORIENTED_EDGE ( 'NONE', *, *, #81678, .F. ) ;
#94804 = CARTESIAN_POINT ( 'NONE',  ( -107.3880028199999970, 1378.913060387289988, 307.7170154214589388 ) ) ;
#94805 = CARTESIAN_POINT ( 'NONE',  ( -10.36148874078660143, 1447.909434907649938, 209.3402815508519836 ) ) ;
#94806 = CARTESIAN_POINT ( 'NONE',  ( 4.138326087764579775, 1515.492270357739926, 206.7919250688289878 ) ) ;
#94808 = EDGE_CURVE ( 'NONE', #54763, #2539, #91571, .T. ) ;
#94807 = CARTESIAN_POINT ( 'NONE',  ( -0.6816155568609990612, 1444.074492657990049, 199.8235773416689938 ) ) ;
#94809 = CARTESIAN_POINT ( 'NONE',  ( 4.677877709162899578, 1498.105331289570131, 235.3354212934999907 ) ) ;
#94810 = CARTESIAN_POINT ( 'NONE',  ( -0.1852737114690000131, 1488.178506539929913, 181.6492668772979755 ) ) ;
#94811 = CARTESIAN_POINT ( 'NONE',  ( 2.035491882000000086, 1468.277065364090276, 218.9268452469790134 ) ) ;
#94812 = CARTESIAN_POINT ( 'NONE',  ( 16.05825058989999832, 1409.640465031130134, 226.2302501376979933 ) ) ;
#94813 = CARTESIAN_POINT ( 'NONE',  ( 5.788097227154999302, 1517.099836525840146, 211.6039138304569747 ) ) ;
#94814 = CARTESIAN_POINT ( 'NONE',  ( 14.13596061226570022, 1415.658863692649902, 197.1814981948540151 ) ) ;
#94815 = CARTESIAN_POINT ( 'NONE',  ( -7.469914488626709925, 1425.609915395969892, 205.2032434723799952 ) ) ;
#94816 = CARTESIAN_POINT ( 'NONE',  ( 6.865869608695000181, 1512.784460098850104, 201.9080085634870159 ) ) ;
#94817 = VERTEX_POINT ( 'NONE', #7561 ) ;
#94818 = CARTESIAN_POINT ( 'NONE',  ( 14.36046478289659944, 1436.108318026239886, 149.9810154171919976 ) ) ;
#94819 = CARTESIAN_POINT ( 'NONE',  ( -5.013337946330830519, 1375.421898367659878, 203.5257142815540305 ) ) ;
#94820 = EDGE_LOOP ( 'NONE', ( #6428, #13419, #47705, #91979 ) ) ;
#94821 = VERTEX_POINT ( 'NONE', #42270 ) ;
#94822 = CARTESIAN_POINT ( 'NONE',  ( -7.300067000364999892, 1513.142795523620180, 216.3167343031170162 ) ) ;
#94823 = CARTESIAN_POINT ( 'NONE',  ( 16.53955848059638356, 1513.001574290601184, 197.2393618145187020 ) ) ;
#94824 = AXIS2_PLACEMENT_3D ( 'NONE', #109491, #42835, #26000 ) ;
#94825 = CARTESIAN_POINT ( 'NONE',  ( -8.332436002999379809, 1474.689645896253978, 203.1022837292814245 ) ) ;
#94826 = CARTESIAN_POINT ( 'NONE',  ( -1.709384611084999950, 1517.224900789629828, 216.4615953054470197 ) ) ;
#94827 = CARTESIAN_POINT ( 'NONE',  ( 1.483134297318269956, 1465.770756053359946, 198.2023842196989847 ) ) ;
#94829 = CARTESIAN_POINT ( 'NONE',  ( 12.06000798031920063, 1421.818391337039884, 208.6542734367120033 ) ) ;
#94828 = B_SPLINE_CURVE_WITH_KNOTS ( 'NONE', 3,
 ( #30564, #73127, #30000, #21592, #56882, #14302, #91013, #64191, #32221, #38406, #98313, #31661, #65841, #90461, #108379, #31112, #100521, #66402, #72582, #40069, #22683, #74790, #15401 ),
 .UNSPECIFIED., .F., .F.,
 ( 4, 2, 2, 2, 1, 1, 1, 1, 1, 2, 2, 2, 2, 4 ),
 ( 0.000000000000000000, 0.2499999999977853271, 0.3749999999966871500, 0.4374999999961360908, 0.4687499999958624763, 0.4843749999957339125, 0.4921874999956594166, 0.4960937499956221131, 0.4980468749956012409, 0.4990234374955930807, 0.4999999999955848651, 0.7499999999977895460, 0.8749999999988947730, 1.000000000000000000 ),
 .UNSPECIFIED. ) ;
#94830 = CARTESIAN_POINT ( 'NONE',  ( 13.55937018769710001, 1409.552481286539887, 191.5919570012989936 ) ) ;
#94831 = CARTESIAN_POINT ( 'NONE',  ( 2.402586825280000227, 1466.023001228489875, 198.3390201041990224 ) ) ;
#94832 = CARTESIAN_POINT ( 'NONE',  ( 0.001298364960140000043, 1507.624704233530110, 237.4156383742980267 ) ) ;
#94833 = ORIENTED_EDGE ( 'NONE', *, *, #83607, .T. ) ;
#94834 = CARTESIAN_POINT ( 'NONE',  ( -0.7578858299649979813, 1516.872851364150165, 206.6414186775969881 ) ) ;
#94835 = ORIENTED_EDGE ( 'NONE', *, *, #9898, .F. ) ;
#94836 = CARTESIAN_POINT ( 'NONE',  ( -103.8798399685330054, 1379.885066417289863, 304.5265232271229934 ) ) ;
#94837 = CIRCLE ( 'NONE', #23276, 1.999997796872630351 ) ;
#94838 = CARTESIAN_POINT ( 'NONE',  ( -18.67054469629999858, 1509.506033879029928, 231.0930226666980047 ) ) ;
#94839 = EDGE_LOOP ( 'NONE', ( #641, #45731, #107605 ) ) ;
#94840 = CARTESIAN_POINT ( 'NONE',  ( 25.89699081781530055, 1448.079192754820042, 137.6508162902210017 ) ) ;
#94841 = CARTESIAN_POINT ( 'NONE',  ( -7.284723200410000210, 1410.103078541930017, 187.5144291113979875 ) ) ;
#94842 = CARTESIAN_POINT ( 'NONE',  ( -24.35760538859999969, 1442.387172495660025, 212.1777658713180017 ) ) ;
#94844 = EDGE_LOOP ( 'NONE', ( #75936, #93843, #85061, #82306 ) ) ;
#94843 = CARTESIAN_POINT ( 'NONE',  ( 3.900198121993049938, 1423.884075158320002, 192.9473687097540164 ) ) ;
#94845 = CARTESIAN_POINT ( 'NONE',  ( -6.014475223502429913, 1511.645396655840159, 201.1712641573570011 ) ) ;
#94846 = DIRECTION ( 'NONE',  ( -1.734723475976805517E-14, 0.000000000000000000, 1.000000000000000000 ) ) ;
#94847 = DIRECTION ( 'NONE',  ( 0.9455185755993178454, 0.000000000000000000, -0.3255681544571537578 ) ) ;
#94848 = DIRECTION ( 'NONE',  ( 6.123233995736769734E-17, 1.000000000000000000, 1.124819836996399911E-32 ) ) ;
#94850 = CARTESIAN_POINT ( 'NONE',  ( -1.753571105566960053, 1484.238156075060033, 182.7741811579140006 ) ) ;
#94849 = CARTESIAN_POINT ( 'NONE',  ( 22.69876404240077505, 1522.382868172864164, 181.3483716558180276 ) ) ;
#94851 = B_SPLINE_CURVE_WITH_KNOTS ( 'NONE', 3,
 ( #103735, #85824, #94778, #9122, #52250, #33754 ),
 .UNSPECIFIED., .F., .F.,
 ( 4, 2, 4 ),
 ( 0.000000000000000000, 0.5000000000000000000, 1.000000000000000000 ),
 .UNSPECIFIED. ) ;
#94852 = CARTESIAN_POINT ( 'NONE',  ( 0.01244693565920149993, 1516.939646076049939, 214.9034317483770167 ) ) ;
#94853 = CARTESIAN_POINT ( 'NONE',  ( 24.05887429810000100, 1410.845155071830277, 209.6244263713389842 ) ) ;
#94854 = CARTESIAN_POINT ( 'NONE',  ( 24.05887576171189579, 1410.845155067154792, 209.6244200405261324 ) ) ;
#94855 = CARTESIAN_POINT ( 'NONE',  ( 28.28208337139999884, 1508.151294399930066, 209.1094497554269935 ) ) ;
#94856 = CARTESIAN_POINT ( 'NONE',  ( -4.026777524084999449, 1516.718889242609976, 211.4189316860469887 ) ) ;
#94857 = DIRECTION ( 'NONE',  ( -1.836970198721029688E-16, -1.000000000000000000, 0.000000000000000000 ) ) ;
#94858 =( BOUNDED_SURFACE ( )  B_SPLINE_SURFACE ( 4, 2, ( 
 ( #32511, #85097, #51514, #101888, #75077, #109762, #41468, #7302, #33042, #92391, #16224 ),
 ( #6738, #100786, #101327, #67231, #24079, #57732, #84002, #17319, #15664, #24617, #58812 ),
 ( #25180, #92952, #42011, #16766, #50429, #102447, #49317, #83443, #40896, #42557, #108657 ),
 ( #91851, #84554, #6193, #7843, #50969, #76160, #100260, #74526, #31944, #23540, #66139 ),
 ( #87892, #45345, #18428, #10620, #61049, #11183, #19551, #53182, #96274, #69443, #79484 ) ),
 .UNSPECIFIED., .F., .T., .F. ) 
 B_SPLINE_SURFACE_WITH_KNOTS ( ( 5, 5 ),
 ( 3, 2, 2, 2, 2, 3 ),
 ( 3.613988937050000239, 5.260361675040000407 ),
 ( 5.178099995975929737, 6.283185307179590673, 7.853981633974480125, 9.424777960769379348, 10.99557428756429900, 11.46128530315550087 ),
 .UNSPECIFIED. ) 
 GEOMETRIC_REPRESENTATION_ITEM ( )  RATIONAL_B_SPLINE_SURFACE ( (
 ( 0.8778166930676719604, 0.7939440089458740246, 1.000000000000000000, 0.7071067811865480168, 1.000000000000000000, 0.7071067811865480168, 1.000000000000000000, 0.7071067811865480168, 1.000000000000000000, 0.9131627722406739922, 0.8778166930676719604),
 ( 0.8778166930676719604, 0.7939440089458740246, 1.000000000000000000, 0.7071067811865480168, 1.000000000000000000, 0.7071067811865480168, 1.000000000000000000, 0.7071067811865480168, 1.000000000000000000, 0.9131627722406739922, 0.8778166930676719604),
 ( 0.8778166930676719604, 0.7939440089458740246, 1.000000000000000000, 0.7071067811865480168, 1.000000000000000000, 0.7071067811865480168, 1.000000000000000000, 0.7071067811865480168, 1.000000000000000000, 0.9131627722406739922, 0.8778166930676719604),
 ( 0.8778166930676719604, 0.7939440089458740246, 1.000000000000000000, 0.7071067811865480168, 1.000000000000000000, 0.7071067811865480168, 1.000000000000000000, 0.7071067811865480168, 1.000000000000000000, 0.9131627722406739922, 0.8778166930676719604),
 ( 0.8778166930676719604, 0.7939440089458740246, 1.000000000000000000, 0.7071067811865480168, 1.000000000000000000, 0.7071067811865480168, 1.000000000000000000, 0.7071067811865480168, 1.000000000000000000, 0.9131627722406739922, 0.8778166930676719604) ) ) 
 REPRESENTATION_ITEM ( '' )  SURFACE ( )  );
#94859 = CARTESIAN_POINT ( 'NONE',  ( 30.00389853323147804, 1524.843416604514459, 222.2743556717897775 ) ) ;
#94861 = ORIENTED_EDGE ( 'NONE', *, *, #78909, .T. ) ;
#94860 = CARTESIAN_POINT ( 'NONE',  ( -92.78054746879999470, 1385.201317530089909, 294.1545524748589742 ) ) ;
#94862 = CIRCLE ( 'NONE', #85980, 11.26398391340000060 ) ;
#94863 = CARTESIAN_POINT ( 'NONE',  ( 24.26836866860000086, 1463.758695672930116, 255.0044592737980054 ) ) ;
#94864 = CARTESIAN_POINT ( 'NONE',  ( 3.479472432754871392, 1450.884102103086661, 184.0533424794217581 ) ) ;
#94865 = CARTESIAN_POINT ( 'NONE',  ( 18.66420869458061205, 1526.382868172863937, 232.7837831374278039 ) ) ;
#94866 = CARTESIAN_POINT ( 'NONE',  ( -8.309204053089999320, 1507.619019172929939, 235.1728781061979987 ) ) ;
#94867 = CARTESIAN_POINT ( 'NONE',  ( -20.73227332440000126, 1454.210575483330103, 225.1076712988979978 ) ) ;
#94868 = B_SPLINE_CURVE_WITH_KNOTS ( 'NONE', 3,
 ( #40775, #93918, #67104, #26161, #34576, #102864, #92276, #7178, #93371, #49745, #14998, #76034, #7717 ),
 .UNSPECIFIED., .F., .F.,
 ( 4, 3, 3, 3, 4 ),
 ( -6.749361107549999517, -5.746593412767809994, -4.743825717985610702, -3.763266661680000347, -2.767901846390000031 ),
 .UNSPECIFIED. ) ;
#94870 = CARTESIAN_POINT ( 'NONE',  ( 17.84735382287039585, 1410.225448354170112, 222.8565957718949733 ) ) ;
#94869 = CARTESIAN_POINT ( 'NONE',  ( -19.43886440797159665, 1410.953638617170554, 197.3090217047405304 ) ) ;
#94871 = CARTESIAN_POINT ( 'NONE',  ( -10.33297333698109988, 1447.717229192940067, 209.8087386623969905 ) ) ;
#94872 = CARTESIAN_POINT ( 'NONE',  ( -108.4852562064530161, 1383.359514468059842, 310.9366048184130022 ) ) ;
#94873 = VERTEX_POINT ( 'NONE', #25991 ) ;
#94874 = CARTESIAN_POINT ( 'NONE',  ( 5.774609621945000271, 1516.777260590120022, 204.5018377250270021 ) ) ;
#94875 = CARTESIAN_POINT ( 'NONE',  ( 0.3398959847620000030, 1405.717602100329941, 267.8539949327980025 ) ) ;
#94876 = AXIS2_PLACEMENT_3D ( 'NONE', #28859, #13668, #14238 ) ;
#94877 = CARTESIAN_POINT ( 'NONE',  ( 10.78159844869479933, 1461.896569297480028, 211.1674770051990038 ) ) ;
#94878 = CARTESIAN_POINT ( 'NONE',  ( -18.87576674860000026, 1410.495261148229929, 223.1730055151980139 ) ) ;
#94879 = DIRECTION ( 'NONE',  ( 0.000000000000000000, 1.000000000000000000, 0.000000000000000000 ) ) ;
#94880 = CARTESIAN_POINT ( 'NONE',  ( 2.175409717514719593E-31, 1397.551704408390151, 209.1218459616989946 ) ) ;
#94881 = CARTESIAN_POINT ( 'NONE',  ( 3.578848130929999982, 1466.803391000889860, 218.7998462970390108 ) ) ;
#94882 = CARTESIAN_POINT ( 'NONE',  ( 3.919629339340000573, 1445.919245566989957, 204.1216026806789898 ) ) ;
#94883 = CARTESIAN_POINT ( 'NONE',  ( -37.65027717969969245, 1440.913060388920030, 255.7160772220900071 ) ) ;
#94884 = CARTESIAN_POINT ( 'NONE',  ( -27.00037440250000031, 1448.139615625060060, 136.8881630574980193 ) ) ;
#94885 = CARTESIAN_POINT ( 'NONE',  ( 3.127068336719009611E-15, 1468.922471155709900, 264.4545146619439606 ) ) ;
#94886 = CARTESIAN_POINT ( 'NONE',  ( -109.0712831559999927, 1385.610640481809924, 297.1783689030590381 ) ) ;
#94887 = EDGE_CURVE ( 'NONE', #92743, #105306, #20122, .T. ) ;
#94888 = CARTESIAN_POINT ( 'NONE',  ( -1.191524307911315583, 1526.382868172863937, 239.2353018730792087 ) ) ;
#94889 = CARTESIAN_POINT ( 'NONE',  ( 1.011935686670000001, 1508.279717064390070, 220.8600042037990079 ) ) ;
#94891 = CYLINDRICAL_SURFACE ( 'NONE', #95713, 1.999999999999995559 ) ;
#94890 = CIRCLE ( 'NONE', #105853, 11.23850026409999892 ) ;
#94892 = ORIENTED_EDGE ( 'NONE', *, *, #72894, .T. ) ;
#94893 = CARTESIAN_POINT ( 'NONE',  ( -3.996802888650000299E-15, 1409.413060387330006, 271.1218459616979999 ) ) ;
#94894 = CARTESIAN_POINT ( 'NONE',  ( 11.94168174870000065, 1433.614859990550030, 146.5967844433980076 ) ) ;
#94895 = CARTESIAN_POINT ( 'NONE',  ( 2.759147620390000277, 1485.169339790590129, 198.7305754187989919 ) ) ;
#94896 = CARTESIAN_POINT ( 'NONE',  ( 16.54279911444290008, 1495.117735635360077, 188.4866523640159812 ) ) ;
#94897 = AXIS2_PLACEMENT_3D ( 'NONE', #51537, #101349, #49339 ) ;
#94898 = CARTESIAN_POINT ( 'NONE',  ( -0.6608933561119999522, 1417.306151990130047, 234.7827825253980052 ) ) ;
#94900 = CARTESIAN_POINT ( 'NONE',  ( 30.04822308544829212, 1524.382868172804365, 196.4802968571190149 ) ) ;
#94899 = CARTESIAN_POINT ( 'NONE',  ( 12.08289755050000025, 1501.361268123389891, 211.3149880542889889 ) ) ;
#94901 = LINE ( 'NONE', #10904, #110296 ) ;
#94902 = CARTESIAN_POINT ( 'NONE',  ( 9.067034957830001574, 1422.697473312089869, 213.1748827745390145 ) ) ;
#94903 = DIRECTION ( 'NONE',  ( 0.000000000000000000, 0.8724564897876576630, -0.4886917979948086077 ) ) ;
#94904 = CARTESIAN_POINT ( 'NONE',  ( -11.86722885316952691, 1418.961735472639475, 228.9247715664120051 ) ) ;
#94906 = EDGE_CURVE ( 'NONE', #75901, #73175, #24883, .T. ) ;
#94905 = CARTESIAN_POINT ( 'NONE',  ( -18.82708389389999581, 1416.254459046630018, 208.1920681675479727 ) ) ;
#94907 = CARTESIAN_POINT ( 'NONE',  ( -8.160121199729999830, 1484.191520557689955, 200.3086294344790019 ) ) ;
#94908 = CARTESIAN_POINT ( 'NONE',  ( 25.53921057650000037, 1435.901306799000167, 136.7951300741979992 ) ) ;
#94909 = CARTESIAN_POINT ( 'NONE',  ( -7.684237820892370507, 1396.181399885199880, 201.1787653736790276 ) ) ;
#94910 = ORIENTED_EDGE ( 'NONE', *, *, #37285, .F. ) ;
#94911 = AXIS2_PLACEMENT_3D ( 'NONE', #37822, #21535, #12059 ) ;
#94912 = CARTESIAN_POINT ( 'NONE',  ( -16.95064093090770285, 1409.878458079239863, 225.6674120715180152 ) ) ;
#94913 = CARTESIAN_POINT ( 'NONE',  ( 2.451271202390000070, 1433.447543843880112, 150.3250444719979839 ) ) ;
#94914 = ORIENTED_EDGE ( 'NONE', *, *, #44571, .T. ) ;
#94915 = EDGE_LOOP ( 'NONE', ( #55878, #12980, #63625, #93302 ) ) ;
#94916 = CARTESIAN_POINT ( 'NONE',  ( -12.16304787920000052, 1501.912848009289746, 211.0099873911190116 ) ) ;
#94917 = CARTESIAN_POINT ( 'NONE',  ( -14.59132467482771212, 1416.165632769844024, 204.1513725631303942 ) ) ;
#94919 = CARTESIAN_POINT ( 'NONE',  ( -9.792917003243150731, 1438.431876507500192, 210.7357112484050106 ) ) ;
#94918 = CYLINDRICAL_SURFACE ( 'NONE', #87213, 2.000000000000001776 ) ;
#94920 = CARTESIAN_POINT ( 'NONE',  ( 2.963633255220000429, 1451.607057905790043, 190.1601877849990103 ) ) ;
#94921 = CARTESIAN_POINT ( 'NONE',  ( 4.172408078941279186, 1424.841910750820034, 185.1366873668810058 ) ) ;
#94922 = DIRECTION ( 'NONE',  ( -0.02616798426500965835, -0.9993150019883683122, -0.02616798426500960631 ) ) ;
#94923 = CARTESIAN_POINT ( 'NONE',  ( 7.490423649669999406, 1425.310147181990033, 212.2658099247589973 ) ) ;
#94924 = CARTESIAN_POINT ( 'NONE',  ( 18.28863238269999769, 1430.119121229389975, 201.0315571599689974 ) ) ;
#94925 = CARTESIAN_POINT ( 'NONE',  ( -5.385523200472070116, 1511.435001055929888, 200.4690698413500058 ) ) ;
#94926 = CARTESIAN_POINT ( 'NONE',  ( -109.5441724319999963, 1376.146465230639933, 306.5935542917590055 ) ) ;
#94927 = EDGE_CURVE ( 'NONE', #34771, #77131, #43099, .T. ) ;
#94928 = CARTESIAN_POINT ( 'NONE',  ( 9.011028107012984734, 1364.896662482048669, 207.6218459616988241 ) ) ;
#94930 = VERTEX_POINT ( 'NONE', #17587 ) ;
#94929 = CARTESIAN_POINT ( 'NONE',  ( 5.456719627610000067, 1455.595244131089885, 218.2350948550090095 ) ) ;
#94931 = EDGE_LOOP ( 'NONE', ( #49577, #5980, #26239, #105742 ) ) ;
#94932 = DIRECTION ( 'NONE',  ( 0.000000000000000000, 1.000000000000000000, 0.000000000000000000 ) ) ;
#94933 = CARTESIAN_POINT ( 'NONE',  ( -21.53008337650500081, 1505.945960034420068, 209.1889141163210013 ) ) ;
#94934 = CARTESIAN_POINT ( 'NONE',  ( -3.048592212130000423, 1471.356831017029890, 269.3358345869979757 ) ) ;
#94935 = CARTESIAN_POINT ( 'NONE',  ( 12.41107674216090828, 1434.349308524667094, 147.3453250864402264 ) ) ;
#94937 = EDGE_CURVE ( 'NONE', #18354, #103670, #32216, .T. ) ;
#94936 = CARTESIAN_POINT ( 'NONE',  ( -0.03226023477341029982, 1410.297896964309984, 185.0217421575940193 ) ) ;
#94938 = CARTESIAN_POINT ( 'NONE',  ( 19.05930086383896693, 1519.551704408389924, 195.1946787710221827 ) ) ;
#94939 = CARTESIAN_POINT ( 'NONE',  ( -7.989567273059999586, 1384.306348609750103, 199.5291464143689950 ) ) ;
#94940 = DIRECTION ( 'NONE',  ( 1.755985294532464991E-16, -1.000000000000000000, 1.338183447452830017E-16 ) ) ;
#94941 = B_SPLINE_SURFACE_WITH_KNOTS ( 'NONE', 5, 4, ( 
 ( #63561, #20949, #88187, #79794, #3100 ),
 ( #89275, #71425, #12572, #105541, #72491 ),
 ( #64099, #29907, #98220, #13095, #47279 ),
 ( #28828, #65195, #48951, #108280, #15304 ),
 ( #31567, #49496, #75790, #41635, #101509 ),
 ( #90923, #100429, #41074, #40521, #76337 ) ),
 .UNSPECIFIED., .F., .F., .F.,
 ( 6, 6 ),
 ( 5, 5 ),
 ( 0.000000000000000000, 11.48858425020000062 ),
 ( 40.20365518519999881, 50.26548245740000453 ),
 .UNSPECIFIED. ) ;
#94942 = PRESENTATION_STYLE_ASSIGNMENT (( #35579 ) ) ;
#94943 = CARTESIAN_POINT ( 'NONE',  ( -2.500000000000000000, 1448.308233332059899, 164.1021382917789992 ) ) ;
#94944 = CARTESIAN_POINT ( 'NONE',  ( 6.358435812139999754, 1368.427897723179740, 207.6218459616989946 ) ) ;
#94945 = CARTESIAN_POINT ( 'NONE',  ( 6.311810463515059588, 1408.080013037259960, 196.8766857931779839 ) ) ;
#94946 = CARTESIAN_POINT ( 'NONE',  ( -12.14058727293699924, 1406.960395450699934, 267.4746583413689791 ) ) ;
#94947 = CARTESIAN_POINT ( 'NONE',  ( 18.02574679518840028, 1424.482682570480165, 224.6196048480980210 ) ) ;
#94948 = VERTEX_POINT ( 'NONE', #84264 ) ;
#94949 = CARTESIAN_POINT ( 'NONE',  ( -10.96867220919999930, 1432.296152601269796, 151.7700998140979891 ) ) ;
#94950 = CARTESIAN_POINT ( 'NONE',  ( 13.87374158799999968, 1442.959733380379930, 189.3447062249979922 ) ) ;
#94951 = ORIENTED_EDGE ( 'NONE', *, *, #39126, .F. ) ;
#94952 = ORIENTED_EDGE ( 'NONE', *, *, #47370, .F. ) ;
#94953 = CARTESIAN_POINT ( 'NONE',  ( -3.179033943583710276, 1457.997354099609993, 219.3203918230290128 ) ) ;
#94954 = CARTESIAN_POINT ( 'NONE',  ( 7.877099145829999038, 1362.118768394180051, 207.6218459616989946 ) ) ;
#94955 = CARTESIAN_POINT ( 'NONE',  ( 7.334957356574999920, 1517.030858226499959, 213.7381182667970165 ) ) ;
#94956 = CARTESIAN_POINT ( 'NONE',  ( 2.830985213604999995, 1512.320675624280057, 216.9025790381570289 ) ) ;
#94957 = CIRCLE ( 'NONE', #46708, 2.000057822092189408 ) ;
#94958 = B_SPLINE_CURVE_WITH_KNOTS ( 'NONE', 3,
 ( #53097, #95633, #46364, #78276, #20020, #18902 ),
 .UNSPECIFIED., .F., .F.,
 ( 4, 2, 4 ),
 ( 0.000000000000000000, 0.5000000000000000000, 1.000000000000000000 ),
 .UNSPECIFIED. ) ;
#94959 = EDGE_LOOP ( 'NONE', ( #43205, #28148, #53371, #3403 ) ) ;
#94960 = CARTESIAN_POINT ( 'NONE',  ( -101.7780519309999931, 1379.485289779790037, 304.0160546798589962 ) ) ;
#94961 = VECTOR ( 'NONE', #69241, 1000.000000000000000 ) ;
#94962 = CARTESIAN_POINT ( 'NONE',  ( -107.1199205305639879, 1378.913060387299993, 301.0091205714350053 ) ) ;
#94963 = CARTESIAN_POINT ( 'NONE',  ( 5.775236792744999903, 1516.804776704140068, 204.1142572851869943 ) ) ;
#94964 = CARTESIAN_POINT ( 'NONE',  ( -27.24055943209999953, 1509.630994782629841, 201.8111112392580253 ) ) ;
#94965 = DIRECTION ( 'NONE',  ( -0.000000000000000000, -1.000000000000000000, -0.000000000000000000 ) ) ;
#94966 = CARTESIAN_POINT ( 'NONE',  ( -84.13119167140000343, 1384.814165098149942, 288.0554183306589948 ) ) ;
#94967 = CARTESIAN_POINT ( 'NONE',  ( -59.87499638670439595, 1384.672222060019976, 243.7406793530619780 ) ) ;
#94968 = CARTESIAN_POINT ( 'NONE',  ( -9.572080927779999334E-17, 1389.913060387289988, 209.1218459616989946 ) ) ;
#94969 = AXIS2_PLACEMENT_3D ( 'NONE', #76986, #27132, #87027 ) ;
#94970 = CARTESIAN_POINT ( 'NONE',  ( -10.55952072472410030, 1471.180150025179955, 209.5617685359960092 ) ) ;
#94972 = EDGE_LOOP ( 'NONE', ( #10585, #46761, #15825, #104121 ) ) ;
#94971 = CARTESIAN_POINT ( 'NONE',  ( -7.548561889089999255, 1445.758549893310146, 184.1610481276980238 ) ) ;
#94973 = CARTESIAN_POINT ( 'NONE',  ( 8.325276386639346882, 1512.905891558394842, 201.7177514598866424 ) ) ;
#94974 = CARTESIAN_POINT ( 'NONE',  ( 27.95183976710000096, 1508.132394785230190, 211.1111938569680149 ) ) ;
#94975 = CARTESIAN_POINT ( 'NONE',  ( -6.711262841758562914, 1442.278122625611786, 201.5834799348254194 ) ) ;
#94976 = CARTESIAN_POINT ( 'NONE',  ( -25.57615594259999980, 1435.901898142059963, 136.7757793872980017 ) ) ;
#94977 = AXIS2_PLACEMENT_3D ( 'NONE', #8669, #77557, #68072 ) ;
#94978 = CARTESIAN_POINT ( 'NONE',  ( -6.933879441005000643, 1516.560253536979872, 211.6083207129769903 ) ) ;
#94979 = CARTESIAN_POINT ( 'NONE',  ( -68.29164953469999944, 1379.747125763249869, 279.1059754382590086 ) ) ;
#94980 = CARTESIAN_POINT ( 'NONE',  ( -15.05055458040000005, 1410.738883427430210, 226.7232811513979982 ) ) ;
#94981 = CARTESIAN_POINT ( 'NONE',  ( -30.64459234690422207, 1525.163457223743762, 221.6135952602373891 ) ) ;
#94982 = CARTESIAN_POINT ( 'NONE',  ( 17.56829117542830332, 1410.890577958010226, 192.7553912862538255 ) ) ;
#94983 = CARTESIAN_POINT ( 'NONE',  ( 2.477975315464999717, 1516.839862955080207, 207.9852983471170091 ) ) ;
#94984 = ORIENTED_EDGE ( 'NONE', *, *, #92589, .F. ) ;
#94985 = CARTESIAN_POINT ( 'NONE',  ( -43.51386627571789489, 1440.913030677579854, 268.2728861700509810 ) ) ;
#94986 = CARTESIAN_POINT ( 'NONE',  ( -0.6856103501910000286, 1410.310356903130014, 233.1312677497980133 ) ) ;
#94988 = B_SPLINE_CURVE_WITH_KNOTS ( 'NONE', 3,
 ( #66328, #15320, #83098, #14781, #48967, #32142, #100446, #59016, #84190, #84737, #24812, #99876, #6392, #31582, #92586, #23729, #23175, #100982, #93676, #74715, #59562, #16956, #25370, #57915, #93143, #75268, #109417, #32693, #42204, #76354, #83638, #65760, #66873, #57375, #33783, #41650, #109958 ),
 .UNSPECIFIED., .F., .F.,
 ( 4, 3, 3, 3, 3, 3, 3, 3, 3, 3, 3, 3, 4 ),
 ( -1.999999927956309875, -1.972989624484049909, -1.798098438852570036, -1.621156865559949978, -1.442904648552300051, -1.257206222084299885, -1.076442897241259855, -0.8953608614236658880, -0.7144086979874439969, -0.5307528079918921726, -0.3521692608878350672, -0.1751745349638540450, -6.152018885430265982E-07 ),
 .UNSPECIFIED. ) ;
#94987 = CARTESIAN_POINT ( 'NONE',  ( -38.49145949329999894, 1384.794605546870116, 239.3122526757589981 ) ) ;
#94989 = VERTEX_POINT ( 'NONE', #59090 ) ;
#94991 = CIRCLE ( 'NONE', #25181, 1.000000000000000888 ) ;
#94990 = CARTESIAN_POINT ( 'NONE',  ( -17.16993831374970014, 1385.286989672689742, 219.9424929166420100 ) ) ;
#94992 = FACE_OUTER_BOUND ( 'NONE', #29149, .T. ) ;
#94993 = CARTESIAN_POINT ( 'NONE',  ( 12.43286703105460056, 1435.614820761110195, 150.9635431477080090 ) ) ;
#94994 = CARTESIAN_POINT ( 'NONE',  ( 18.58484988559350271, 1469.012271477369950, 228.1231286946100170 ) ) ;
#94995 = AXIS2_PLACEMENT_3D ( 'NONE', #38945, #5361, #22128 ) ;
#94996 = FACE_OUTER_BOUND ( 'NONE', #92694, .T. ) ;
#94997 = CARTESIAN_POINT ( 'NONE',  ( -2.325358437519999821, 1408.994263693330140, 187.9843026324979860 ) ) ;
#94998 = CARTESIAN_POINT ( 'NONE',  ( -0.3096201624669999708, 1409.092176881229989, 232.6500405377979916 ) ) ;
#94999 = CARTESIAN_POINT ( 'NONE',  ( 4.227028548029660548, 1441.559244791980063, 165.7750707031279944 ) ) ;
#95001 = CARTESIAN_POINT ( 'NONE',  ( -4.304697625840000264, 1420.046328294529985, 186.4088000267980192 ) ) ;
#95000 = CARTESIAN_POINT ( 'NONE',  ( -3.451033427095000050, 1517.025653221279981, 214.9083735325669977 ) ) ;
#95002 = CARTESIAN_POINT ( 'NONE',  ( 20.81915283020000018, 1509.403205473429807, 188.8735477223980013 ) ) ;
#95003 = CARTESIAN_POINT ( 'NONE',  ( 7.717505752974999744, 1516.857914730730045, 216.8393517232070167 ) ) ;
#95004 = ORIENTED_EDGE ( 'NONE', *, *, #108164, .T. ) ;
#95005 = CARTESIAN_POINT ( 'NONE',  ( -12.80019129569859970, 1416.529254608160045, 196.2487864292310178 ) ) ;
#95006 = CARTESIAN_POINT ( 'NONE',  ( -11.79695136760000018, 1504.313428625830056, 182.6247401251980023 ) ) ;
#95007 = ORIENTED_EDGE ( 'NONE', *, *, #3739, .T. ) ;
#95008 = AXIS2_PLACEMENT_3D ( 'NONE', #45620, #79760, #3067 ) ;
#95009 = CARTESIAN_POINT ( 'NONE',  ( 2.793917634100000047, 1420.174898411929917, 185.2234237461979944 ) ) ;
#95010 = CARTESIAN_POINT ( 'NONE',  ( 18.64588652299999794, 1416.828040475229955, 209.6843149956849857 ) ) ;
#95011 = UNCERTAINTY_MEASURE_WITH_UNIT (LENGTH_MEASURE( 1.000000000000000082E-05 ), #5435, 'distance_accuracy_value', 'NONE');
#95012 = CARTESIAN_POINT ( 'NONE',  ( 3.314835131729999773, 1443.023294147790011, 217.3780381071989893 ) ) ;
#95013 = CARTESIAN_POINT ( 'NONE',  ( -34.18677586421193837, 1522.382868172863937, 198.4504086008750505 ) ) ;
#95014 = CARTESIAN_POINT ( 'NONE',  ( -21.83550407203883736, 1523.678648413191695, 234.9693198511253627 ) ) ;
#95015 = CARTESIAN_POINT ( 'NONE',  ( 18.71036172829999700, 1415.996778984329922, 210.0886326743409995 ) ) ;
#95016 = CARTESIAN_POINT ( 'NONE',  ( -4.145978979534980458E-15, 1375.413060387289988, 209.1218459572589836 ) ) ;
#95017 = CARTESIAN_POINT ( 'NONE',  ( -4.772204876747930591, 1456.966521863563912, 217.3851231261082262 ) ) ;
#95018 = CARTESIAN_POINT ( 'NONE',  ( 17.45848092850000199, 1413.521836630329972, 192.3744159994980123 ) ) ;
#95020 = CARTESIAN_POINT ( 'NONE',  ( 0.5730919830699721107, 1440.103938664269890, 189.4488964803610145 ) ) ;
#95019 = FACE_OUTER_BOUND ( 'NONE', #109694, .T. ) ;
#95021 = DIRECTION ( 'NONE',  ( 1.224646799147353207E-16, -1.836970198721029688E-16, -1.000000000000000000 ) ) ;
#95022 = ORIENTED_EDGE ( 'NONE', *, *, #83173, .F. ) ;
#95023 = CARTESIAN_POINT ( 'NONE',  ( 1.552414559603289890, 1415.673583080789967, 190.6708713369849875 ) ) ;
#95024 = CARTESIAN_POINT ( 'NONE',  ( 26.37684233794689348, 1508.582724258994403, 216.7137066027032404 ) ) ;
#95025 = FACE_OUTER_BOUND ( 'NONE', #83876, .T. ) ;
#95026 = CARTESIAN_POINT ( 'NONE',  ( 7.548436927367426996, 1410.549687724076421, 187.4153570461994605 ) ) ;
#95027 = CARTESIAN_POINT ( 'NONE',  ( 0.3621993315900440269, 1416.825784014750070, 227.1772709241249970 ) ) ;
#95028 =( GEOMETRIC_REPRESENTATION_CONTEXT ( 3 ) GLOBAL_UNCERTAINTY_ASSIGNED_CONTEXT ( ( #110701 ) ) GLOBAL_UNIT_ASSIGNED_CONTEXT ( ( #31586, #32697, #100987 ) ) REPRESENTATION_CONTEXT ( 'NONE', 'WORKASPACE' ) );
#95029 = CARTESIAN_POINT ( 'NONE',  ( 16.16632277704777110, 1511.187213306747708, 181.3470724465435637 ) ) ;
#95030 = FACE_OUTER_BOUND ( 'NONE', #93368, .T. ) ;
#95031 = CARTESIAN_POINT ( 'NONE',  ( -4.635215035006506668, 1377.957596388888533, 204.0719524705168624 ) ) ;
#95032 = CARTESIAN_POINT ( 'NONE',  ( -17.11733429290000075, 1420.830776148560062, 201.6585816624789800 ) ) ;
#95034 = EDGE_CURVE ( 'NONE', #100575, #33927, #7009, .T. ) ;
#95033 = CARTESIAN_POINT ( 'NONE',  ( -95.12345330600079762, 1383.767095643290077, 309.8833154982480096 ) ) ;
#95035 = CARTESIAN_POINT ( 'NONE',  ( 3.484702367460000172, 1452.791371899229944, 152.5519604361979873 ) ) ;
#95036 = DIRECTION ( 'NONE',  ( 0.000000000000000000, -1.000000000000000000, -8.596382804469569442E-17 ) ) ;
#95038 = CONICAL_SURFACE ( 'NONE', #89675, 0.9999999999999910072, 0.7853981633970000820 ) ;
#95037 = CARTESIAN_POINT ( 'NONE',  ( -23.06762233478933055, 1409.889827747422032, 209.9527113325115408 ) ) ;
#95040 = ORIENTED_EDGE ( 'NONE', *, *, #2404, .T. ) ;
#95039 = CARTESIAN_POINT ( 'NONE',  ( 10.57019798174319902, 1452.578602367869962, 209.5296950901719981 ) ) ;
#95041 = CARTESIAN_POINT ( 'NONE',  ( -17.78552240860015488, 1460.054203228820370, 228.1338144972297926 ) ) ;
#95042 = CARTESIAN_POINT ( 'NONE',  ( -76.52635743460000128, 1382.336017472330013, 300.7162654001589885 ) ) ;
#95043 = CARTESIAN_POINT ( 'NONE',  ( -14.68737671657240007, 1419.645626571690173, 213.7540033288840107 ) ) ;
#95044 = ADVANCED_FACE ( 'NONE', ( #93212 ), #42826, .F. ) ;
#95045 = VERTEX_POINT ( 'NONE', #10316 ) ;
#95046 = EDGE_LOOP ( 'NONE', ( #99868, #84944, #44658, #88221, #69194 ) ) ;
#95047 = CARTESIAN_POINT ( 'NONE',  ( 19.56213531549639839, 1508.835144824000054, 229.7005312132949939 ) ) ;
#95048 = CARTESIAN_POINT ( 'NONE',  ( 29.00779973304130266, 1526.382868172863937, 200.9494832830834810 ) ) ;
#95049 = CARTESIAN_POINT ( 'NONE',  ( 40.27308693906149273, 1443.611999474700042, 137.1163322506119755 ) ) ;
#95051 = CARTESIAN_POINT ( 'NONE',  ( -37.17588026959999326, 1458.776664316129882, 264.1764829737979881 ) ) ;
#95050 = CARTESIAN_POINT ( 'NONE',  ( 14.55570725811163157, 1412.291795584168312, 269.3628599515130873 ) ) ;
#95052 = CARTESIAN_POINT ( 'NONE',  ( 9.782549294074950552, 1435.950597167319984, 210.1455436486230042 ) ) ;
#95053 = CARTESIAN_POINT ( 'NONE',  ( -109.9099220809999906, 1384.374201251870090, 297.0307877050590264 ) ) ;
#95054 = CIRCLE ( 'NONE', #107597, 1.000000000000000888 ) ;
#95055 = FACE_OUTER_BOUND ( 'NONE', #17092, .T. ) ;
#95056 = CARTESIAN_POINT ( 'NONE',  ( -19.85891451210000014, 1485.179989725129872, 190.7502780007980050 ) ) ;
#95057 = CARTESIAN_POINT ( 'NONE',  ( 1.441735424540000032, 1409.901586897629841, 185.3129409531979945 ) ) ;
#95058 = CARTESIAN_POINT ( 'NONE',  ( 2.502839789385249869, 1486.822988642699784, 197.4474283702710125 ) ) ;
#95059 = CARTESIAN_POINT ( 'NONE',  ( -7.036086178909999767, 1439.758762051160147, 154.1890771745979691 ) ) ;
#95060 = CARTESIAN_POINT ( 'NONE',  ( -9.188196878108460197, 1450.454516124349993, 208.3425459881050017 ) ) ;
#95061 = CARTESIAN_POINT ( 'NONE',  ( -11.61130078636250040, 1423.105448014539888, 204.1619613308869816 ) ) ;
#95062 = CARTESIAN_POINT ( 'NONE',  ( -3.146029458580000160, 1451.975600841429923, 154.0166248088980012 ) ) ;
#95063 = CARTESIAN_POINT ( 'NONE',  ( 1.393816646507355150, 1512.187213306747481, 243.1385343369520342 ) ) ;
#95064 = ORIENTED_EDGE ( 'NONE', *, *, #24232, .F. ) ;
#95065 = CARTESIAN_POINT ( 'NONE',  ( -4.303235405216489617, 1508.728291632010041, 212.9102526658959960 ) ) ;
#95066 = CARTESIAN_POINT ( 'NONE',  ( 18.43405782060979803, 1472.181634805399881, 195.1578483246480005 ) ) ;
#95067 = CARTESIAN_POINT ( 'NONE',  ( -44.93135410500000404, 1442.582777215279975, 269.6838066175980089 ) ) ;
#95068 = DIRECTION ( 'NONE',  ( -1.699538841806929935E-33, 1.000000000000000000, -1.698192320643030073E-16 ) ) ;
#95069 = CARTESIAN_POINT ( 'NONE',  ( 11.98951922200000020, 1442.759074889710064, 150.6922381223979812 ) ) ;
#95070 = CARTESIAN_POINT ( 'NONE',  ( -29.00779973304142345, 1526.382868172863937, 200.9494832830838789 ) ) ;
#95071 = CIRCLE ( 'NONE', #73586, 1.999999999999999556 ) ;
#95072 = CARTESIAN_POINT ( 'NONE',  ( 13.22806383169999833, 1431.113060387329824, 195.8937821296979962 ) ) ;
#95073 = CARTESIAN_POINT ( 'NONE',  ( 2.793203188579529872, 1409.027311659480119, 230.4220898241179896 ) ) ;
#95074 = CARTESIAN_POINT ( 'NONE',  ( -0.7440358369610000633, 1416.274718422629803, 227.8470358584980033 ) ) ;
#95075 = CARTESIAN_POINT ( 'NONE',  ( -2.256759385399999651, 1417.436677706029968, 235.4758680199980176 ) ) ;
#95076 = CARTESIAN_POINT ( 'NONE',  ( -0.6733940044856625562, 1485.373885326774371, 181.9506766061667804 ) ) ;
#95077 = CARTESIAN_POINT ( 'NONE',  ( -2.581985620920249414, 1358.634824676206335, 208.3718459617010978 ) ) ;
#95078 = CARTESIAN_POINT ( 'NONE',  ( -45.50576722784600037, 1438.311143129649963, 268.9784717228729960 ) ) ;
#95079 = CARTESIAN_POINT ( 'NONE',  ( -2.500000000000000000, 1425.929641636930000, 184.1455913746980002 ) ) ;
#95080 = ORIENTED_EDGE ( 'NONE', *, *, #33145, .F. ) ;
#95081 = CARTESIAN_POINT ( 'NONE',  ( -8.759598966840000500, 1423.140078425670026, 210.5148996192390030 ) ) ;
#95082 = ORIENTED_EDGE ( 'NONE', *, *, #3895, .T. ) ;
#95083 = CARTESIAN_POINT ( 'NONE',  ( -6.944466780504999548, 1516.939530130779985, 209.1331108864249870 ) ) ;
#95084 = CARTESIAN_POINT ( 'NONE',  ( -7.550503362055001055, 1510.480349266450048, 214.6730346442070072 ) ) ;
#95085 = CARTESIAN_POINT ( 'NONE',  ( 7.538438372221369477, 1425.706950029929885, 212.1947421841360040 ) ) ;
#95086 = CIRCLE ( 'NONE', #46834, 1.999999999999998668 ) ;
#95087 = DIRECTION ( 'NONE',  ( 5.980589973904019347E-17, -1.000000000000000000, 1.736889445713099699E-16 ) ) ;
#95088 = EDGE_LOOP ( 'NONE', ( #51940, #49812, #110057, #56125 ) ) ;
#95089 = CYLINDRICAL_SURFACE ( 'NONE', #68901, 2.000000000000000000 ) ;
#95091 = FACE_OUTER_BOUND ( 'NONE', #43944, .T. ) ;
#95090 = CARTESIAN_POINT ( 'NONE',  ( -2.646294106703095395, 1525.055402519452173, 176.5934494553323191 ) ) ;
#95092 = CARTESIAN_POINT ( 'NONE',  ( -0.4827268496605868764, 1487.916102923474682, 219.9679759818499747 ) ) ;
#95093 = CARTESIAN_POINT ( 'NONE',  ( -11.59871332934921639, 1426.255604624567468, 138.4425913800236287 ) ) ;
#95094 = CARTESIAN_POINT ( 'NONE',  ( -7.211935934568213469, 1517.051704408389924, 193.5679467272088345 ) ) ;
#95095 = CARTESIAN_POINT ( 'NONE',  ( -9.084504854676080043, 1439.262540927600185, 207.9197032644189846 ) ) ;
#95096 = VERTEX_POINT ( 'NONE', #95437 ) ;
#95097 = CARTESIAN_POINT ( 'NONE',  ( -3.098696616388379788, 1408.307991063760255, 270.3912379415129976 ) ) ;
#95098 = CARTESIAN_POINT ( 'NONE',  ( -2.881325412095000260, 1517.003078582959688, 208.0029426616869728 ) ) ;
#95099 = CARTESIAN_POINT ( 'NONE',  ( 12.42248214874839896, 1420.733284265709926, 230.8418435108919766 ) ) ;
#95100 = CARTESIAN_POINT ( 'NONE',  ( -20.59684415639999955, 1507.762623717429960, 190.9355247910979756 ) ) ;
#95102 = ORIENTED_EDGE ( 'NONE', *, *, #17773, .T. ) ;
#95101 = CARTESIAN_POINT ( 'NONE',  ( -7.922050983617392461, 1365.299968594369147, 208.3718459617061285 ) ) ;
#95103 = ORIENTED_EDGE ( 'NONE', *, *, #37265, .F. ) ;
#95104 = CARTESIAN_POINT ( 'NONE',  ( -23.73673603223410211, 1411.112104334589958, 210.2769570570919768 ) ) ;
#95105 = CARTESIAN_POINT ( 'NONE',  ( 8.652776089875690246, 1511.435001055579960, 203.7363227723449768 ) ) ;
#95106 = CARTESIAN_POINT ( 'NONE',  ( 3.653292041488962916, 1424.985912203865610, 184.9355336758895874 ) ) ;
#95107 = CARTESIAN_POINT ( 'NONE',  ( 12.18695065166680358, 1473.011202655907937, 192.8237078935919158 ) ) ;
#95108 = B_SPLINE_CURVE_WITH_KNOTS ( 'NONE', 3,
 ( #75086, #49878, #103005, #94061, #25743, #75637, #51523, #59393 ),
 .UNSPECIFIED., .F., .F.,
 ( 4, 2, 2, 4 ),
 ( 0.000000000000000000, 0.001073044933456172596, 0.001609567400184299226, 0.002146089866912425856 ),
 .UNSPECIFIED. ) ;
#95109 = CARTESIAN_POINT ( 'NONE',  ( -20.53774147538043238, 1436.446361497854241, 144.8508540958611093 ) ) ;
#95110 = CARTESIAN_POINT ( 'NONE',  ( -22.98589895030000108, 1420.827177425029959, 211.9705801624280070 ) ) ;
#95111 = CARTESIAN_POINT ( 'NONE',  ( 38.96315770833140135, 1459.274076524980046, 266.3799300039799505 ) ) ;
#95112 = EDGE_CURVE ( 'NONE', #19532, #21233, #85555, .T. ) ;
#95113 = CARTESIAN_POINT ( 'NONE',  ( -11.66989614716730017, 1391.913060387289988, 209.6445408818580063 ) ) ;
#95114 = CARTESIAN_POINT ( 'NONE',  ( 14.25613302710000063, 1464.413060387330006, 224.0689215379980226 ) ) ;
#95115 = CARTESIAN_POINT ( 'NONE',  ( 6.935133380425000382, 1516.613881697390070, 205.8602099992770036 ) ) ;
#95116 = EDGE_LOOP ( 'NONE', ( #28574, #20872, #48026, #92479, #109095 ) ) ;
#95117 = CARTESIAN_POINT ( 'NONE',  ( 23.51028611932632018, 1411.094384488653986, 211.8659750899354037 ) ) ;
#95118 = CARTESIAN_POINT ( 'NONE',  ( 1.486105993495000277, 1473.851208882719902, 182.5641111719070295 ) ) ;
#95119 = CARTESIAN_POINT ( 'NONE',  ( 22.69620822199999921, 1409.705526811329946, 208.7849502228380345 ) ) ;
#95120 = ORIENTED_EDGE ( 'NONE', *, *, #36144, .F. ) ;
#95121 = CARTESIAN_POINT ( 'NONE',  ( 4.410745166166449849, 1508.610338516509955, 205.2562926885780143 ) ) ;
#95122 = ADVANCED_FACE ( 'NONE', ( #18701 ), #61030, .T. ) ;
#95123 = CARTESIAN_POINT ( 'NONE',  ( 24.99678597100239585, 1451.803817917760171, 136.6927953316869946 ) ) ;
#95124 = ADVANCED_FACE ( 'NONE', ( #60756 ), #86471, .F. ) ;
#95125 = CARTESIAN_POINT ( 'NONE',  ( -4.980141907650089905, 1508.551704408389924, 211.7958595151590089 ) ) ;
#95126 = CARTESIAN_POINT ( 'NONE',  ( -17.47467951480000181, 1385.286067972039973, 219.9356668727590147 ) ) ;
#95127 = CARTESIAN_POINT ( 'NONE',  ( -4.145978979534980458E-15, 1375.413060387289988, 209.1218459572589836 ) ) ;
#95128 = CARTESIAN_POINT ( 'NONE',  ( 18.03578411879999877, 1409.707763031429749, 194.6290428685979919 ) ) ;
#95129 = CARTESIAN_POINT ( 'NONE',  ( 13.35741048202589809, 1444.324653571830822, 164.9741927960640453 ) ) ;
#95130 = CARTESIAN_POINT ( 'NONE',  ( 3.573960252902736556, 1439.695850415500217, 184.5435116089865915 ) ) ;
#95132 = CARTESIAN_POINT ( 'NONE',  ( -22.83130780170417395, 1432.445202165297133, 215.4846681824749908 ) ) ;
#95131 = CARTESIAN_POINT ( 'NONE',  ( 0.1707430212980000084, 1416.982709795129949, 234.1884028855980091 ) ) ;
#95133 = DIRECTION ( 'NONE',  ( -0.8960382015506694886, 0.4437655256578362795, 0.01370035034099489381 ) ) ;
#95134 = CIRCLE ( 'NONE', #80585, 2.000000000000003109 ) ;
#95135 = DIRECTION ( 'NONE',  ( -0.02616798426453448637, 0.9993150019883495494, 0.02616798426619628554 ) ) ;
#95136 = CARTESIAN_POINT ( 'NONE',  ( -9.700195692639999479, 1379.919833190730060, 216.8653063374690078 ) ) ;
#95137 = CARTESIAN_POINT ( 'NONE',  ( 3.459156578084999989, 1516.769879638719885, 213.7318425517769924 ) ) ;
#95138 = CARTESIAN_POINT ( 'NONE',  ( 10.63675272238868885, 1419.812825537269873, 232.2865147438434690 ) ) ;
#95139 = ORIENTED_EDGE ( 'NONE', *, *, #57862, .F. ) ;
#95140 = CARTESIAN_POINT ( 'NONE',  ( -7.611722247467775482, 1464.044227469945326, 227.3821205927781364 ) ) ;
#95141 = CARTESIAN_POINT ( 'NONE',  ( 21.98490254033135827, 1525.713797967456912, 235.3026395021878159 ) ) ;
#95142 = CARTESIAN_POINT ( 'NONE',  ( -0.4930154003685739972, 1409.658068983249905, 232.9865684859400119 ) ) ;
#95143 = CARTESIAN_POINT ( 'NONE',  ( -113.4000000000000057, 1391.913060387289988, 304.2218459572590064 ) ) ;
#95144 = CARTESIAN_POINT ( 'NONE',  ( -1.920602012799999869, 1420.567466289690174, 193.8392733480989989 ) ) ;
#95145 = CARTESIAN_POINT ( 'NONE',  ( -4.327495487222860149, 1515.139385973079925, 208.5392436879629940 ) ) ;
#95146 = CIRCLE ( 'NONE', #87974, 1.999999999999998668 ) ;
#95147 = CARTESIAN_POINT ( 'NONE',  ( -20.74408966469999882, 1445.748654444849990, 224.8635561966979708 ) ) ;
#95148 = CARTESIAN_POINT ( 'NONE',  ( -28.35863496383681692, 1526.382868172863482, 198.5269487343526293 ) ) ;
#95149 = CARTESIAN_POINT ( 'NONE',  ( 11.88679881449999876, 1433.350353069249877, 150.2822412956980145 ) ) ;
#95150 = CARTESIAN_POINT ( 'NONE',  ( 19.46212511719999938, 1448.109899942129914, 224.8635562210979799 ) ) ;
#95151 = CARTESIAN_POINT ( 'NONE',  ( -10.38333126256229910, 1461.681020311170187, 210.9775042442759911 ) ) ;
#95152 = ADVANCED_FACE ( 'NONE', ( #18156 ), #55555, .F. ) ;
#95153 = CARTESIAN_POINT ( 'NONE',  ( 14.20069603096709976, 1428.565903384720059, 195.1302447813920082 ) ) ;
#95154 = CARTESIAN_POINT ( 'NONE',  ( 10.72410096480519925, 1421.781422562299895, 200.2028139908449873 ) ) ;
#95155 = CARTESIAN_POINT ( 'NONE',  ( 23.77649893510000112, 1435.334014145809988, 137.3596790345980025 ) ) ;
#95156 = CARTESIAN_POINT ( 'NONE',  ( 22.60265952820000024, 1409.702346025430188, 208.8284293190110077 ) ) ;
#95157 = CARTESIAN_POINT ( 'NONE',  ( 11.91243657443186699, 1398.266254915216905, 214.3270314564130103 ) ) ;
#95158 = CARTESIAN_POINT ( 'NONE',  ( -29.74692510567269821, 1509.964815989430008, 211.8522445133610290 ) ) ;
#95159 = TOROIDAL_SURFACE ( 'NONE', #9319, 4.000000000000000000, 1.000000000000000000 ) ;
#95160 = CARTESIAN_POINT ( 'NONE',  ( 25.27895407529999972, 1469.239702721330104, 214.6649670560380230 ) ) ;
#95161 = B_SPLINE_CURVE_WITH_KNOTS ( 'NONE', 3,
 ( #107994, #22311, #31291, #23438, #38050, #90641, #22867, #65475, #74427, #40245, #63823, #97936, #83346, #73308, #66030, #12836, #91200, #82797, #107444, #106351, #55413, #57076, #100153, #89547, #57632, #91746, #72227, #4985, #47016, #81141, #72763, #38584, #106890, #47557, #90085, #92297, #480, #67127, #101789, #84458, #101227, #110761, #59282, #42449, #76609, #7745, #76063, #102351, #32406, #8837, #34051, #50863, #66587, #93400, #83900, #34604, #110205, #17214, #43020, #77178, #25078, #7206, #67681, #68790, #58168, #109664, #50332, #102890, #26189, #25634, #58715, #15567, #100690, #85540, #6644, #16665, #23973, #60377, #94498, #41909, #49768, #68242, #24527, #84992, #109125, #41362, #33479, #8287 ),
 .UNSPECIFIED., .F., .F.,
 ( 4, 3, 3, 3, 3, 3, 3, 3, 3, 3, 3, 3, 3, 3, 3, 3, 3, 3, 3, 3, 3, 3, 3, 3, 3, 3, 3, 3, 3, 4 ),
 ( -2.608805242767630261, -1.335759665544890007, -0.03842482041208983290, 1.300439966035479955, 2.667507357936759860, 4.080875363370900288, 4.341750878185000495, 5.839428055071511636, 7.370373697392469836, 8.938676201850199732, 10.62243765222589964, 12.30567332129900038, 14.04213788646359973, 15.10556603929509834, 15.67372200335319832, 16.64339347143850034, 17.60617660898700265, 18.59539778760229822, 19.57499817531500241, 20.56364872257519849, 21.56169445605650026, 22.52530327033359825, 23.60819854813160035, 24.64216807509990304, 25.68594691940390007, 26.73955916627750184, 27.85178574788760386, 28.92923767607740260, 30.05885158439770066, 31.18846549271799518 ),
 .UNSPECIFIED. ) ;
#95162 = CARTESIAN_POINT ( 'NONE',  ( -16.80221138011627957, 1420.025806103657942, 208.0932244396257715 ) ) ;
#95163 = CARTESIAN_POINT ( 'NONE',  ( 26.47820321154927470, 1436.726665921244148, 136.8127344866470025 ) ) ;
#95164 = CARTESIAN_POINT ( 'NONE',  ( -0.7442430207490000615, 1515.589102391990082, 205.1050341093590248 ) ) ;
#95165 =( BOUNDED_CURVE ( )  B_SPLINE_CURVE ( 3, ( #41601, #103703, #26431, #93087 ),
 .UNSPECIFIED., .F., .F. ) 
 B_SPLINE_CURVE_WITH_KNOTS ( ( 4, 4 ),
 ( 6.248344042517810948, 6.260122023476537123 ),
 .UNSPECIFIED. ) 
 CURVE ( )  GEOMETRIC_REPRESENTATION_ITEM ( )  RATIONAL_B_SPLINE_CURVE ( ( 1.000000000000000000, 0.9999884399637866128, 0.9999884399637866128, 1.000000000000000000 ) ) 
 REPRESENTATION_ITEM ( '' )  );
#95166 = CARTESIAN_POINT ( 'NONE',  ( 7.755379628513099810, 1459.738852961230123, 228.9106028297960052 ) ) ;
#95167 = CARTESIAN_POINT ( 'NONE',  ( -3.253462098795000035, 1516.874084700499907, 212.5832060635069922 ) ) ;
#95168 = CARTESIAN_POINT ( 'NONE',  ( 1.326713953160000070, 1454.806608698389937, 218.4390644836289823 ) ) ;
#95169 = CARTESIAN_POINT ( 'NONE',  ( 0.1596977958884080173, 1486.448930399509891, 181.8173153803849971 ) ) ;
#95171 = EDGE_LOOP ( 'NONE', ( #64565, #79267, #96523, #48328, #74816 ) ) ;
#95170 = CARTESIAN_POINT ( 'NONE',  ( 3.554603345999999942, 1442.390756379090135, 217.2531437058290180 ) ) ;
#95172 = CARTESIAN_POINT ( 'NONE',  ( -0.7133823615420000763, 1416.822694282129987, 227.9183241380980007 ) ) ;
#95173 = CARTESIAN_POINT ( 'NONE',  ( -6.280588687330000752, 1380.190335656839807, 203.2358530807489956 ) ) ;
#95174 = CARTESIAN_POINT ( 'NONE',  ( -20.59664500270120158, 1507.763472350329948, 190.3621299389660066 ) ) ;
#95175 = EDGE_CURVE ( 'NONE', #89888, #83385, #103252, .T. ) ;
#95176 = ORIENTED_EDGE ( 'NONE', *, *, #34939, .F. ) ;
#95177 = CARTESIAN_POINT ( 'NONE',  ( -5.000754081882999635, 1508.551704408389924, 219.6714415651769912 ) ) ;
#95178 = VERTEX_POINT ( 'NONE', #45614 ) ;
#95179 = SPHERICAL_SURFACE ( 'NONE', #82509, 2.000000000730000060 ) ;
#95180 = CARTESIAN_POINT ( 'NONE',  ( -14.36267855726159937, 1380.304917481549865, 209.5901700444179880 ) ) ;
#95181 = CARTESIAN_POINT ( 'NONE',  ( -12.70717216449999931, 1414.913060387329779, 220.4277423101980276 ) ) ;
#95182 = CARTESIAN_POINT ( 'NONE',  ( 0.007371176946978959775, 1430.919077003989969, 217.6339654454789923 ) ) ;
#95183 = CARTESIAN_POINT ( 'NONE',  ( -14.65245970860000035, 1420.119839379899986, 213.8659343334090011 ) ) ;
#95184 = CARTESIAN_POINT ( 'NONE',  ( -21.41971086555123449, 1512.187213306747481, 185.1638823089581081 ) ) ;
#95185 = DIRECTION ( 'NONE',  ( -1.755985294532469921E-16, 1.000000000000000000, -1.338183447452831989E-16 ) ) ;
#95186 = CARTESIAN_POINT ( 'NONE',  ( -82.75382724187160477, 1385.168106391910214, 286.4548433143800139 ) ) ;
#95187 = CARTESIAN_POINT ( 'NONE',  ( -10.14901568273809929, 1391.913060387289988, 214.2247289053989903 ) ) ;
#95188 = CARTESIAN_POINT ( 'NONE',  ( -59.96754922390000075, 1379.749011644449865, 261.8279529299589967 ) ) ;
#95189 = VERTEX_POINT ( 'NONE', #80841 ) ;
#95190 = CARTESIAN_POINT ( 'NONE',  ( 10.85576822019209864, 1490.211973181020085, 207.6231814341079769 ) ) ;
#95192 = ORIENTED_EDGE ( 'NONE', *, *, #7744, .T. ) ;
#95191 = CARTESIAN_POINT ( 'NONE',  ( -0.6259040480903699244, 1438.020704032760023, 227.6802023094499816 ) ) ;
#95193 = CARTESIAN_POINT ( 'NONE',  ( -19.27355791249999939, 1467.813399981289876, 204.3088842694490097 ) ) ;
#95194 = ORIENTED_EDGE ( 'NONE', *, *, #21547, .T. ) ;
#95195 = CARTESIAN_POINT ( 'NONE',  ( 24.66759386739999727, 1507.924354362629856, 220.6865237209979966 ) ) ;
#95196 = CARTESIAN_POINT ( 'NONE',  ( -7.744553022556359245, 1364.511030831803964, 209.6218459617148824 ) ) ;
#95197 = CARTESIAN_POINT ( 'NONE',  ( -6.855565616159999820, 1494.715409694790196, 199.7515626485690063 ) ) ;
#95198 = CARTESIAN_POINT ( 'NONE',  ( 29.14946092887392481, 1509.937924658664770, 213.7557683796928814 ) ) ;
#95199 = CARTESIAN_POINT ( 'NONE',  ( 11.45021740003180000, 1427.604960870419973, 209.5607445365500325 ) ) ;
#95200 = CARTESIAN_POINT ( 'NONE',  ( 19.15376622239216076, 1438.408328458145661, 212.9158144853951740 ) ) ;
#95201 = CARTESIAN_POINT ( 'NONE',  ( 1.723041758439999960, 1417.151714778930000, 232.9552265120979939 ) ) ;
#95202 = CARTESIAN_POINT ( 'NONE',  ( 3.329658494789999867, 1445.620183534490025, 200.6158397099989941 ) ) ;
#95203 = CARTESIAN_POINT ( 'NONE',  ( -8.655671105859999770, 1512.830360918489987, 210.0583268009119990 ) ) ;
#95204 = CARTESIAN_POINT ( 'NONE',  ( -6.779714480667859533, 1369.556064268209411, 210.6218459617030021 ) ) ;
#95205 = CARTESIAN_POINT ( 'NONE',  ( -8.444049741005709819, 1488.605066998670054, 190.0484225089540189 ) ) ;
#95206 = CARTESIAN_POINT ( 'NONE',  ( 1.676160982570000124, 1456.565164728689979, 199.0597759751990168 ) ) ;
#95207 = EDGE_CURVE ( 'NONE', #43746, #60804, #73486, .T. ) ;
#95208 = CARTESIAN_POINT ( 'NONE',  ( 2.476733476015000157, 1516.858326417339867, 206.6281461634669938 ) ) ;
#95210 = EDGE_CURVE ( 'NONE', #10931, #76626, #37013, .T. ) ;
#95209 = CARTESIAN_POINT ( 'NONE',  ( -2.404980717409123336, 1525.211477436245787, 176.1486445165030545 ) ) ;
#95211 = CARTESIAN_POINT ( 'NONE',  ( -2.500000000000000000, 1438.683324620350049, 157.7083961265980179 ) ) ;
#95212 = CARTESIAN_POINT ( 'NONE',  ( 14.20177175210000087, 1416.825532216630108, 196.5059038677979686 ) ) ;
#95214 = ORIENTED_EDGE ( 'NONE', *, *, #55537, .T. ) ;
#95213 = CARTESIAN_POINT ( 'NONE',  ( 0.8661595920449980390, 1495.979405726489858, 221.4595168884989960 ) ) ;
#95215 = CARTESIAN_POINT ( 'NONE',  ( 3.614551905308796432E-15, 1526.382868172863937, 179.6067898016248421 ) ) ;
#95216 = ORIENTED_EDGE ( 'NONE', *, *, #23342, .T. ) ;
#95217 = DIRECTION ( 'NONE',  ( 0.000000000000000000, 1.000000000000000000, 0.000000000000000000 ) ) ;
#95218 = CARTESIAN_POINT ( 'NONE',  ( -23.18005802010000238, 1410.911243146729930, 205.3224337777979827 ) ) ;
#95220 = CARTESIAN_POINT ( 'NONE',  ( 17.28255409390969888, 1410.597227212849930, 192.3502816095650019 ) ) ;
#95219 = CARTESIAN_POINT ( 'NONE',  ( -10.90887219343169967, 1425.661441503749757, 108.4510460995380043 ) ) ;
#95221 = CARTESIAN_POINT ( 'NONE',  ( 7.725372132234999967, 1517.158319634930194, 211.9946825927569876 ) ) ;
#95222 = CARTESIAN_POINT ( 'NONE',  ( 28.69212989171126083, 1510.026194129199666, 217.9223110541325923 ) ) ;
#95223 = CARTESIAN_POINT ( 'NONE',  ( -22.95908931529999819, 1507.624001450029937, 207.8018278714380074 ) ) ;
#95224 = CARTESIAN_POINT ( 'NONE',  ( -36.52133751200000233, 1436.268775032720214, 254.5789788204980084 ) ) ;
#95225 = CARTESIAN_POINT ( 'NONE',  ( -13.58429793331039903, 1379.610516642590028, 208.3569126637650015 ) ) ;
#95226 = CARTESIAN_POINT ( 'NONE',  ( 28.32839678142520157, 1508.625224770790055, 209.4146328292849830 ) ) ;
#95227 = CARTESIAN_POINT ( 'NONE',  ( -5.028437303939999659, 1391.796862042790053, 214.5333048971589847 ) ) ;
#95228 = CARTESIAN_POINT ( 'NONE',  ( -36.89672635344380325, 1437.851014151270192, 136.5554436358479791 ) ) ;
#95229 = ORIENTED_EDGE ( 'NONE', *, *, #80952, .T. ) ;
#95230 = CARTESIAN_POINT ( 'NONE',  ( 10.70562411493910027, 1396.809431658850144, 216.5037525343219897 ) ) ;
#95231 = CARTESIAN_POINT ( 'NONE',  ( 9.475842709078071024, 1461.102026927640054, 206.4900463968490101 ) ) ;
#95232 = CARTESIAN_POINT ( 'NONE',  ( -17.43039599940000173, 1458.275712043530120, 229.4620914164979979 ) ) ;
#95233 = ORIENTED_EDGE ( 'NONE', *, *, #31658, .T. ) ;
#95234 = ORIENTED_EDGE ( 'NONE', *, *, #70945, .F. ) ;
#95235 = LINE ( 'NONE', #28579, #18041 ) ;
#95236 = CARTESIAN_POINT ( 'NONE',  ( -1.748905610829809998, 1488.269106374019884, 219.8524659745219765 ) ) ;
#95237 = ORIENTED_EDGE ( 'NONE', *, *, #69676, .T. ) ;
#95238 = CARTESIAN_POINT ( 'NONE',  ( 0.1180531581219999987, 1410.296228957430003, 184.9798896325980024 ) ) ;
#95239 = DIRECTION ( 'NONE',  ( -0.8564730265368828421, -0.5161917810414575758, 0.000000000000000000 ) ) ;
#95240 = EDGE_CURVE ( 'NONE', #105229, #25916, #53693, .T. ) ;
#95241 = CARTESIAN_POINT ( 'NONE',  ( 27.43651637349223193, 1509.328400154276551, 206.1603289671332107 ) ) ;
#95242 = CARTESIAN_POINT ( 'NONE',  ( 6.827653005798030250, 1508.551704612109916, 202.6664205262289897 ) ) ;
#95243 = EDGE_CURVE ( 'NONE', #81651, #102101, #38579, .T. ) ;
#95244 = FILL_AREA_STYLE ('',( #79019 ) ) ;
#95245 = CARTESIAN_POINT ( 'NONE',  ( -12.54019908070000078, 1391.397792955739988, 209.7548876603800068 ) ) ;
#95246 = CARTESIAN_POINT ( 'NONE',  ( -94.75128443427969671, 1384.856503445179897, 294.8510205860830524 ) ) ;
#95247 = VERTEX_POINT ( 'NONE', #48354 ) ;
#95248 = CARTESIAN_POINT ( 'NONE',  ( 3.257220602695000355, 1517.040132827679827, 203.3350082531769942 ) ) ;
#95249 = CARTESIAN_POINT ( 'NONE',  ( -5.006259886824999228, 1516.939723362869927, 209.1347437590049765 ) ) ;
#95250 = ORIENTED_EDGE ( 'NONE', *, *, #68617, .F. ) ;
#95252 = EDGE_CURVE ( 'NONE', #80530, #100437, #86974, .T. ) ;
#95251 = CARTESIAN_POINT ( 'NONE',  ( 11.85930646257130050, 1431.861885083070092, 149.9617303242330308 ) ) ;
#95253 = B_SPLINE_CURVE_WITH_KNOTS ( 'NONE', 3,
 ( #43002, #100136, #53630, #27849, #87203, #70435, #104554, #35689, #103994, #19429, #60355, #36801, #62030 ),
 .UNSPECIFIED., .F., .F.,
 ( 4, 3, 3, 3, 4 ),
 ( -25.27124713432710124, -24.90871837163620128, -23.58501801755940264, -23.26424315256220154, -21.89878892990000026 ),
 .UNSPECIFIED. ) ;
#95254 = CARTESIAN_POINT ( 'NONE',  ( 5.496430422650386838, 1510.805212306365547, 216.6808561322358173 ) ) ;
#95255 = ORIENTED_EDGE ( 'NONE', *, *, #76298, .T. ) ;
#95256 = CARTESIAN_POINT ( 'NONE',  ( 7.254034580837151580, 1423.037804158368544, 139.1419882753651791 ) ) ;
#95257 = CARTESIAN_POINT ( 'NONE',  ( -7.701846892468879879, 1508.539045597550057, 219.2228727215799893 ) ) ;
#95258 = CARTESIAN_POINT ( 'NONE',  ( 9.157527028969999705, 1509.060285975029956, 235.8715647223980056 ) ) ;
#95259 = EDGE_CURVE ( 'NONE', #67251, #76272, #62065, .T. ) ;
#95260 = CARTESIAN_POINT ( 'NONE',  ( -9.658472698806898293, 1461.210338549909920, 208.2934798919299908 ) ) ;
#95261 = CARTESIAN_POINT ( 'NONE',  ( -4.605225103679999599, 1422.042318833529862, 184.9396219054979724 ) ) ;
#95262 = CARTESIAN_POINT ( 'NONE',  ( 1.462222899693720102, 1408.251425098729896, 270.3922974192450397 ) ) ;
#95263 = CARTESIAN_POINT ( 'NONE',  ( -4.738498500012391368, 1427.169020172040746, 137.0999999980979851 ) ) ;
#95264 = CARTESIAN_POINT ( 'NONE',  ( -12.78210459472699867, 1502.593308907019946, 209.4105061602950002 ) ) ;
#95265 = CARTESIAN_POINT ( 'NONE',  ( -2.334596864402660010, 1422.040517539739994, 193.1911830680820117 ) ) ;
#95266 = CARTESIAN_POINT ( 'NONE',  ( 14.91143818900724405, 1415.677402202029953, 209.1063111766177940 ) ) ;
#95267 = CARTESIAN_POINT ( 'NONE',  ( 7.653195889217795589, 1423.477952156526044, 195.7103289535878332 ) ) ;
#95268 = EDGE_CURVE ( 'NONE', #598, #11573, #4906, .T. ) ;
#95270 = CARTESIAN_POINT ( 'NONE',  ( 15.29853388839999973, 1471.323284329529770, 194.6523739445979970 ) ) ;
#95269 = CARTESIAN_POINT ( 'NONE',  ( -21.58396545289999935, 1505.929462060390051, 209.1867379206110229 ) ) ;
#95271 = CARTESIAN_POINT ( 'NONE',  ( -68.62231159911313227, 1379.747791814526636, 280.2140134007494794 ) ) ;
#95272 = CARTESIAN_POINT ( 'NONE',  ( 17.61568774148620165, 1411.200535208959991, 224.8174967984410273 ) ) ;
#95273 = CARTESIAN_POINT ( 'NONE',  ( -5.735709145435179401, 1423.321980822750220, 94.86005652877258854 ) ) ;
#95274 = ORIENTED_EDGE ( 'NONE', *, *, #13794, .F. ) ;
#95275 = CARTESIAN_POINT ( 'NONE',  ( 43.50000000000000000, 1440.913060387330006, 271.1218459616979999 ) ) ;
#95276 = EDGE_CURVE ( 'NONE', #53118, #21613, #76263, .T. ) ;
#95277 = CARTESIAN_POINT ( 'NONE',  ( 18.02694236555139895, 1424.485126976410129, 224.5424481119590041 ) ) ;
#95278 = CARTESIAN_POINT ( 'NONE',  ( -19.37774363895756480, 1525.878013734321485, 181.3897518523461656 ) ) ;
#95279 = CARTESIAN_POINT ( 'NONE',  ( -2.910649417096987435, 1484.739743472488044, 183.2378289904456210 ) ) ;
#95280 = CARTESIAN_POINT ( 'NONE',  ( -14.58197489760000032, 1416.181292664740113, 214.1195166561190035 ) ) ;
#95281 = EDGE_CURVE ( 'NONE', #24288, #72135, #97642, .T. ) ;
#95283 = VERTEX_POINT ( 'NONE', #110444 ) ;
#95282 = CARTESIAN_POINT ( 'NONE',  ( -0.7597457875130829708, 1515.127202858759802, 204.7940314484660007 ) ) ;
#95284 = CARTESIAN_POINT ( 'NONE',  ( 17.09817538404499970, 1414.913526854310021, 210.5930684982130003 ) ) ;
#95285 = CARTESIAN_POINT ( 'NONE',  ( -12.31752010984839885, 1377.944433743309901, 209.1218459601290078 ) ) ;
#95286 = CARTESIAN_POINT ( 'NONE',  ( -16.32138437919999774, 1416.733793783010015, 208.9008268797709889 ) ) ;
#95287 = DIRECTION ( 'NONE',  ( 0.4794255386042038380, 0.000000000000000000, 0.8775825618903722036 ) ) ;
#95288 = CARTESIAN_POINT ( 'NONE',  ( -10.85709873899809885, 1461.880737148149819, 210.9081126214580024 ) ) ;
#95289 = EDGE_CURVE ( 'NONE', #1678, #55998, #104426, .T. ) ;
#95290 = CARTESIAN_POINT ( 'NONE',  ( 7.848979634317430509, 1517.051704408389924, 215.9448598632019980 ) ) ;
#95291 = DIRECTION ( 'NONE',  ( -1.000000000000000000, 0.000000000000000000, 0.000000000000000000 ) ) ;
#95292 = CARTESIAN_POINT ( 'NONE',  ( -16.01627750966499875, 1512.526319173689899, 222.7161941950670041 ) ) ;
#95293 = EDGE_CURVE ( 'NONE', #69449, #42195, #28270, .T. ) ;
#95294 = CARTESIAN_POINT ( 'NONE',  ( 16.27592940589999770, 1412.749584434430062, 226.8352020966980263 ) ) ;
#95295 = CARTESIAN_POINT ( 'NONE',  ( -8.432300450239999634, 1478.613105400289896, 216.7664695459189943 ) ) ;
#95296 = CARTESIAN_POINT ( 'NONE',  ( -16.33051720469999779, 1460.522939258030192, 228.3433114430980027 ) ) ;
#95297 = CARTESIAN_POINT ( 'NONE',  ( 4.995725969715000048, 1516.651306816259876, 206.8263604310569690 ) ) ;
#95298 = CARTESIAN_POINT ( 'NONE',  ( 14.52947405539999970, 1407.976345905729886, 269.2157512787979954 ) ) ;
#95299 = CARTESIAN_POINT ( 'NONE',  ( 24.02336744349999620, 1436.564838698800031, 139.9832055672980005 ) ) ;
#95300 = EDGE_CURVE ( 'NONE', #24484, #40850, #63814, .T. ) ;
#95301 = CARTESIAN_POINT ( 'NONE',  ( 20.93632175249999960, 1469.156076992429917, 193.5744950039980097 ) ) ;
#95302 = CARTESIAN_POINT ( 'NONE',  ( -23.24680097320000272, 1434.020615140939981, 214.0512479341779795 ) ) ;
#95303 = CARTESIAN_POINT ( 'NONE',  ( -13.63528866819950025, 1379.581412608760047, 207.9504834338530088 ) ) ;
#95304 = CARTESIAN_POINT ( 'NONE',  ( 32.86470156657996000, 1523.580204110581690, 217.2021180770844069 ) ) ;
#95305 = CARTESIAN_POINT ( 'NONE',  ( -1.568427187249999966, 1452.094535719030091, 183.9924580127980107 ) ) ;
#95306 = CARTESIAN_POINT ( 'NONE',  ( -6.825986752669999547, 1409.091027441130109, 196.5037156953979718 ) ) ;
#95307 = CARTESIAN_POINT ( 'NONE',  ( -15.42042112429999889, 1415.259230628689920, 208.9538274143839942 ) ) ;
#95308 = CARTESIAN_POINT ( 'NONE',  ( -13.58597427780000011, 1441.854506128520143, 188.4823871297980133 ) ) ;
#95309 = DIRECTION ( 'NONE',  ( -0.6742693640212139572, -4.300014380382889521E-13, -0.7384854939282339270 ) ) ;
#95310 = CARTESIAN_POINT ( 'NONE',  ( 18.04903976654019715, 1429.245179625179844, 206.8954713348119867 ) ) ;
#95311 = CARTESIAN_POINT ( 'NONE',  ( 3.909710721586129534, 1522.051704408389924, 220.4764703678949900 ) ) ;
#95312 = ORIENTED_EDGE ( 'NONE', *, *, #19116, .F. ) ;
#95313 = CARTESIAN_POINT ( 'NONE',  ( -2.549111485395000098, 1512.332007210709889, 201.4919753869869794 ) ) ;
#95314 = CARTESIAN_POINT ( 'NONE',  ( -14.73919588483700061, 1409.427764449309734, 211.5316301116640147 ) ) ;
#95315 = FACE_OUTER_BOUND ( 'NONE', #104188, .T. ) ;
#95316 = CARTESIAN_POINT ( 'NONE',  ( 19.37374569213945463, 1526.382868172863937, 234.3668155954418637 ) ) ;
#95317 = CARTESIAN_POINT ( 'NONE',  ( -26.93323766929999863, 1469.218382335129945, 266.6753116650979791 ) ) ;
#95318 = CARTESIAN_POINT ( 'NONE',  ( -17.27558692971449972, 1507.606285623229951, 224.2552697136770234 ) ) ;
#95319 = CARTESIAN_POINT ( 'NONE',  ( 0.1904623309857999824, 1420.430684221689944, 183.1881945191479986 ) ) ;
#95320 = CARTESIAN_POINT ( 'NONE',  ( -24.17806289182839663, 1444.519329898075512, 211.5601904552849533 ) ) ;
#95321 = CARTESIAN_POINT ( 'NONE',  ( -65.68697704670019277, 1384.675462607609916, 289.6970332893050113 ) ) ;
#95322 = CARTESIAN_POINT ( 'NONE',  ( -21.16387757469560071, 1384.952792652959943, 201.9777141633980193 ) ) ;
#95323 = CARTESIAN_POINT ( 'NONE',  ( 17.04561243864089803, 1423.674420110669871, 228.9411243753750114 ) ) ;
#95324 = CARTESIAN_POINT ( 'NONE',  ( 20.59269117889999734, 1507.766073656829803, 227.7908422914979951 ) ) ;
#95325 = CARTESIAN_POINT ( 'NONE',  ( -28.25247054546100145, 1508.179583162469953, 208.8562385362949954 ) ) ;
#95326 = ADVANCED_FACE ( 'NONE', ( #34284 ), #22674, .F. ) ;
#95327 = DIRECTION ( 'NONE',  ( 0.3255681544571567554, 0.000000000000000000, 0.9455185755993167351 ) ) ;
#95328 = FACE_OUTER_BOUND ( 'NONE', #63584, .T. ) ;
#95329 = CARTESIAN_POINT ( 'NONE',  ( -5.818429214160000029, 1509.055275519029919, 180.2714693110980022 ) ) ;
#95330 = CARTESIAN_POINT ( 'NONE',  ( -23.26696311050000077, 1409.890070742030048, 207.5628654440679952 ) ) ;
#95331 = EDGE_CURVE ( 'NONE', #102504, #34771, #56688, .T. ) ;
#95332 = CARTESIAN_POINT ( 'NONE',  ( 17.48265376240000180, 1415.426210663629945, 208.8075711781490043 ) ) ;
#95333 = CARTESIAN_POINT ( 'NONE',  ( 3.513937425589999997, 1485.582095535989993, 219.4230302830989672 ) ) ;
#95334 = CARTESIAN_POINT ( 'NONE',  ( 4.997209437610000471, 1423.732853852190146, 194.0938684716990110 ) ) ;
#95335 = CARTESIAN_POINT ( 'NONE',  ( 19.53786426059039982, 1522.382868172863937, 236.7197124308265188 ) ) ;
#95336 = CARTESIAN_POINT ( 'NONE',  ( 0.6387483492823400333, 1461.179315971390224, 230.4375156181200168 ) ) ;
#95337 = CARTESIAN_POINT ( 'NONE',  ( -6.032863554449749088, 1508.551565390740279, 216.2881064706280085 ) ) ;
#95338 = CARTESIAN_POINT ( 'NONE',  ( -27.69925886641940238, 1441.434395751479997, 137.3015763626259798 ) ) ;
#95340 = CARTESIAN_POINT ( 'NONE',  ( -44.93136608500000051, 1440.913060387330006, 269.6838062106980374 ) ) ;
#95339 = CARTESIAN_POINT ( 'NONE',  ( -22.33897372919999924, 1410.187224172929746, 212.0108092242280122 ) ) ;
#95341 = CARTESIAN_POINT ( 'NONE',  ( -0.5089086897610000104, 1411.661826841030006, 233.2294965383979957 ) ) ;
#95342 = DIRECTION ( 'NONE',  ( 0.8090169943749551118, 0.000000000000000000, 0.5877852522924625900 ) ) ;
#95343 = CARTESIAN_POINT ( 'NONE',  ( -10.55591960359999959, 1490.955095264389911, 212.1910566715390019 ) ) ;
#95344 = CARTESIAN_POINT ( 'NONE',  ( -23.54487295850000095, 1420.914744205530042, 210.9134490421280077 ) ) ;
#95345 = CARTESIAN_POINT ( 'NONE',  ( -0.9591724243577970377, 1420.560689427859870, 184.1653156966539768 ) ) ;
#95346 = EDGE_CURVE ( 'NONE', #2466, #51946, #28057, .T. ) ;
#95347 = CARTESIAN_POINT ( 'NONE',  ( -7.334328310795000583, 1517.005755693489846, 204.1179978101270081 ) ) ;
#95348 = CARTESIAN_POINT ( 'NONE',  ( -30.90487439922555879, 1525.907212628473644, 201.8101144455182521 ) ) ;
#95349 = CARTESIAN_POINT ( 'NONE',  ( -3.356147517029587579, 1440.691650900622562, 156.8829035650872186 ) ) ;
#95350 = CARTESIAN_POINT ( 'NONE',  ( -17.42709856749150177, 1485.949155400869813, 188.1984452550049980 ) ) ;
#95351 = CARTESIAN_POINT ( 'NONE',  ( -17.72806394670000074, 1410.889176615030010, 194.8230026513979851 ) ) ;
#95352 = CARTESIAN_POINT ( 'NONE',  ( 9.444504587474009227, 1504.434930463329920, 216.0229134707260243 ) ) ;
#95353 = CARTESIAN_POINT ( 'NONE',  ( 39.23020515599449709, 1448.346468128479955, 136.4190043813750037 ) ) ;
#95355 = ORIENTED_EDGE ( 'NONE', *, *, #41982, .T. ) ;
#95354 = CARTESIAN_POINT ( 'NONE',  ( -66.34684761518089147, 1379.742662962009945, 277.0805805419040553 ) ) ;
#95356 = ORIENTED_EDGE ( 'NONE', *, *, #43968, .T. ) ;
#95357 = CARTESIAN_POINT ( 'NONE',  ( 11.95021264318459941, 1433.547364810169938, 150.0873180042360104 ) ) ;
#95358 = CARTESIAN_POINT ( 'NONE',  ( 0.06016801242969999769, 1397.283812744030001, 222.0600360843979786 ) ) ;
#95359 = ORIENTED_EDGE ( 'NONE', *, *, #103486, .F. ) ;
#95360 = FACE_OUTER_BOUND ( 'NONE', #13524, .T. ) ;
#95361 = CARTESIAN_POINT ( 'NONE',  ( -10.35873372929360059, 1448.228887144569853, 208.5914340594589760 ) ) ;
#95362 = CARTESIAN_POINT ( 'NONE',  ( -8.876070945589999539, 1385.242442397379818, 218.6685569028989846 ) ) ;
#95364 = CARTESIAN_POINT ( 'NONE',  ( 13.89896040166999924, 1452.843947645199933, 223.8762708690549914 ) ) ;
#95363 = CARTESIAN_POINT ( 'NONE',  ( -1.208150493920000068, 1443.877570131390030, 199.8977866975789937 ) ) ;
#95365 = CARTESIAN_POINT ( 'NONE',  ( 11.94206337009999963, 1438.199233188169956, 150.9847479746979957 ) ) ;
#95366 = EDGE_CURVE ( 'NONE', #16677, #34471, #4096, .T. ) ;
#95367 = CARTESIAN_POINT ( 'NONE',  ( 1.580841669900000079, 1507.641628515030106, 181.1142457626980331 ) ) ;
#95368 = CARTESIAN_POINT ( 'NONE',  ( 1.871223699670000018, 1467.140817989690049, 219.6429414212990139 ) ) ;
#95369 = CARTESIAN_POINT ( 'NONE',  ( 14.91703010720000044, 1409.433974557229931, 225.8933006754979829 ) ) ;
#95370 = CARTESIAN_POINT ( 'NONE',  ( 6.949574947644999945, 1517.102359858469754, 212.3809477691169718 ) ) ;
#95371 = CARTESIAN_POINT ( 'NONE',  ( 34.11564357267010195, 1435.688851149350285, 134.0999999980979851 ) ) ;
#95372 = CARTESIAN_POINT ( 'NONE',  ( -9.238451120100068081, 1424.071832880570128, 206.1097894639889887 ) ) ;
#95373 = CARTESIAN_POINT ( 'NONE',  ( 6.096095830864999954, 1514.881364185380107, 201.0808170114369773 ) ) ;
#95374 = ORIENTED_EDGE ( 'NONE', *, *, #41280, .T. ) ;
#95375 = CARTESIAN_POINT ( 'NONE',  ( 13.59790036228669940, 1434.964892464889999, 148.8305582646289906 ) ) ;
#95376 = ADVANCED_FACE ( 'NONE', ( #19686 ), #99577, .T. ) ;
#95377 = CARTESIAN_POINT ( 'NONE',  ( -15.55153481088430034, 1441.783360245790163, 219.6938892586900067 ) ) ;
#95378 = ORIENTED_EDGE ( 'NONE', *, *, #44686, .F. ) ;
#95379 = ORIENTED_EDGE ( 'NONE', *, *, #80268, .F. ) ;
#95380 = ORIENTED_EDGE ( 'NONE', *, *, #76897, .F. ) ;
#95381 = CARTESIAN_POINT ( 'NONE',  ( -7.922128378965000550, 1512.637906871319728, 215.9665121834669890 ) ) ;
#95382 = CARTESIAN_POINT ( 'NONE',  ( -1.139293766549999809, 1467.057741776030070, 235.4579552793979929 ) ) ;
#95383 = CARTESIAN_POINT ( 'NONE',  ( 28.86644038478740626, 1509.921098698501737, 202.4756158416115852 ) ) ;
#95384 = CARTESIAN_POINT ( 'NONE',  ( -4.487249770485409961, 1509.038615931769982, 206.6339108289169815 ) ) ;
#95385 = CARTESIAN_POINT ( 'NONE',  ( -1.773373219119749766, 1465.043355074880083, 198.2607089762770158 ) ) ;
#95386 = CARTESIAN_POINT ( 'NONE',  ( -19.08809138029046082, 1441.859548814234131, 210.2413154080126674 ) ) ;
#95387 = CARTESIAN_POINT ( 'NONE',  ( -55.54181829044275531, 1379.709133944529640, 251.3019363274339071 ) ) ;
#95388 = CARTESIAN_POINT ( 'NONE',  ( 4.225121941997549868, 1446.251017732170112, 166.4055522513860126 ) ) ;
#95389 = ADVANCED_FACE ( 'NONE', ( #94741 ), #35644, .F. ) ;
#95390 = CARTESIAN_POINT ( 'NONE',  ( 1.304108710279999972, 1508.717026135230071, 238.0028103276980289 ) ) ;
#95391 = ORIENTED_EDGE ( 'NONE', *, *, #106664, .F. ) ;
#95392 = CARTESIAN_POINT ( 'NONE',  ( 6.933879402874999265, 1516.560253536979872, 206.6353711893569880 ) ) ;
#95393 = ORIENTED_EDGE ( 'NONE', *, *, #47972, .F. ) ;
#95394 = CARTESIAN_POINT ( 'NONE',  ( 21.50585395376209874, 1440.913060387330006, 224.9641782112639987 ) ) ;
#95395 = CARTESIAN_POINT ( 'NONE',  ( -16.51373361550000141, 1508.736179495329907, 185.6988723191980171 ) ) ;
#95396 = EDGE_CURVE ( 'NONE', #48130, #31461, #62818, .T. ) ;
#95397 = ORIENTED_EDGE ( 'NONE', *, *, #16504, .T. ) ;
#95398 = CARTESIAN_POINT ( 'NONE',  ( -7.508705051315979873, 1508.884118747140064, 203.6086422076290035 ) ) ;
#95399 = CARTESIAN_POINT ( 'NONE',  ( -13.50724518150000009, 1409.886837265230042, 190.1809790390979913 ) ) ;
#95400 = CARTESIAN_POINT ( 'NONE',  ( -24.90968947180000015, 1441.637783390069899, 210.4505011253679925 ) ) ;
#95401 = CARTESIAN_POINT ( 'NONE',  ( -11.08206323070000110, 1414.913528139129994, 196.0394634478979867 ) ) ;
#95402 = CARTESIAN_POINT ( 'NONE',  ( -11.73701141503820011, 1426.696005490819971, 144.1689084034089774 ) ) ;
#95403 = CARTESIAN_POINT ( 'NONE',  ( -11.95702896124850945, 1433.550299325597734, 147.6125996980034927 ) ) ;
#95404 = CARTESIAN_POINT ( 'NONE',  ( -27.37591788248279911, 1439.764921109970146, 137.1160056607250226 ) ) ;
#95405 = CARTESIAN_POINT ( 'NONE',  ( -12.27023110815660090, 1416.839692126590080, 194.6640136892829958 ) ) ;
#95406 = EDGE_CURVE ( 'NONE', #73277, #102562, #78506, .T. ) ;
#95408 = CARTESIAN_POINT ( 'NONE',  ( 21.38516915557986309, 1522.382868172863937, 237.8497028174237471 ) ) ;
#95407 = CARTESIAN_POINT ( 'NONE',  ( -26.86204968941349946, 1508.007394745769943, 212.0120970035400205 ) ) ;
#95409 = CARTESIAN_POINT ( 'NONE',  ( 4.038637462725000127, 1516.734985836460055, 214.8955147850770118 ) ) ;
#95410 = EDGE_CURVE ( 'NONE', #29176, #77278, #47734, .T. ) ;
#95411 = CARTESIAN_POINT ( 'NONE',  ( -3.395951246300449977, 1428.698596373810233, 200.3955505136949853 ) ) ;
#95412 = CARTESIAN_POINT ( 'NONE',  ( 5.803572356819420186, 1510.929912129050081, 216.7181665413809810 ) ) ;
#95413 = CARTESIAN_POINT ( 'NONE',  ( 28.22027450670000093, 1509.158030589630016, 207.9424314675380003 ) ) ;
#95414 = CARTESIAN_POINT ( 'NONE',  ( -2.477986770365000257, 1516.922519270759949, 212.3907053662870226 ) ) ;
#95415 = B_SPLINE_CURVE_WITH_KNOTS ( 'NONE', 5,
 ( #100492, #23773, #57960, #92093, #15371, #75853 ),
 .UNSPECIFIED., .F., .F.,
 ( 6, 6 ),
 ( 0.000000000000000000, 1.000000000000000000 ),
 .UNSPECIFIED. ) ;
#95416 = CARTESIAN_POINT ( 'NONE',  ( -11.78939996719659966, 1482.318781070740215, 207.5200076686040234 ) ) ;
#95417 = CARTESIAN_POINT ( 'NONE',  ( 31.32995031131201458, 1523.678648413191695, 221.9013357025043831 ) ) ;
#95419 = ORIENTED_EDGE ( 'NONE', *, *, #106151, .F. ) ;
#95418 = CARTESIAN_POINT ( 'NONE',  ( -89.15245910350000713, 1385.190331364289932, 292.2648985219589690 ) ) ;
#95420 = CARTESIAN_POINT ( 'NONE',  ( 6.121216816089999737E-10, 1465.143864797330025, 238.2947585024979844 ) ) ;
#95421 = FACE_OUTER_BOUND ( 'NONE', #107242, .T. ) ;
#95422 = CARTESIAN_POINT ( 'NONE',  ( -28.07099224718820096, 1509.893321036980069, 217.6805618164050031 ) ) ;
#95423 = CARTESIAN_POINT ( 'NONE',  ( -7.384241671499998994, 1508.154784625329967, 235.7410849829979895 ) ) ;
#95424 = EDGE_CURVE ( 'NONE', #108761, #75688, #41350, .T. ) ;
#95425 = B_SPLINE_CURVE_WITH_KNOTS ( 'NONE', 5,
 ( #91734, #99569, #72746, #91186, #106336, #56498, #100139, #29622, #98477 ),
 .UNSPECIFIED., .F., .F.,
 ( 6, 3, 6 ),
 ( -2.813093253849999975, -1.406546626929999988, 0.000000000000000000 ),
 .UNSPECIFIED. ) ;
#95426 = CARTESIAN_POINT ( 'NONE',  ( -20.40418802339999615, 1454.957320663730115, 226.6330256287980092 ) ) ;
#95428 = CARTESIAN_POINT ( 'NONE',  ( -1.122592899216370017E-16, 1388.079727053959914, 209.1218459616989946 ) ) ;
#95427 = CARTESIAN_POINT ( 'NONE',  ( 11.77090819340000039, 1432.440121525590030, 150.8116842255979861 ) ) ;
#95429 = CARTESIAN_POINT ( 'NONE',  ( -9.231300103966539439, 1449.703421660030017, 207.7615902039960076 ) ) ;
#95430 = FACE_OUTER_BOUND ( 'NONE', #70534, .T. ) ;
#95431 = VERTEX_POINT ( 'NONE', #13464 ) ;
#95432 = CARTESIAN_POINT ( 'NONE',  ( 4.611879685325000366, 1516.858533673840157, 204.4999481076869756 ) ) ;
#95433 = CARTESIAN_POINT ( 'NONE',  ( -12.15118411454099956, 1508.442498811720043, 217.6820456900339877 ) ) ;
#95434 = ADVANCED_FACE ( 'NONE', ( #99127 ), #105919, .T. ) ;
#95435 = FACE_OUTER_BOUND ( 'NONE', #37674, .T. ) ;
#95436 = CARTESIAN_POINT ( 'NONE',  ( 19.66827358063540032, 1471.163942014939948, 270.2287850334790278 ) ) ;
#95437 = CARTESIAN_POINT ( 'NONE',  ( -12.87561223598270033, 1428.667272998819954, 222.5140706137790119 ) ) ;
#95438 = CARTESIAN_POINT ( 'NONE',  ( -39.89556624698280274, 1446.848291182909861, 136.6543435533029935 ) ) ;
#95439 = DIRECTION ( 'NONE',  ( 0.000000000000000000, 1.000000000000000000, 0.000000000000000000 ) ) ;
#95440 = CARTESIAN_POINT ( 'NONE',  ( -19.54391504031712401, 1526.306647125542668, 232.9578003497408361 ) ) ;
#95441 = FACE_OUTER_BOUND ( 'NONE', #68235, .T. ) ;
#95442 = CARTESIAN_POINT ( 'NONE',  ( -2.303292313784549794, 1449.840026941649967, 154.2474790842049970 ) ) ;
#95443 = CARTESIAN_POINT ( 'NONE',  ( 0.8927505473990010598, 1432.232264963090074, 200.7285312053789994 ) ) ;
#95444 = CARTESIAN_POINT ( 'NONE',  ( 10.50094040442339960, 1481.402766154620167, 210.3929528566290230 ) ) ;
#95445 = CARTESIAN_POINT ( 'NONE',  ( -1.137508020020000066, 1507.161920010990116, 221.5186969393989784 ) ) ;
#95446 = LINE ( 'NONE', #94318, #106510 ) ;
#95447 = ORIENTED_EDGE ( 'NONE', *, *, #91834, .T. ) ;
#95448 = CARTESIAN_POINT ( 'NONE',  ( 3.237924447490000190, 1448.965650011070238, 183.9353614378979955 ) ) ;
#95449 = AXIS2_PLACEMENT_3D ( 'NONE', #55462, #104196, #20717 ) ;
#95450 = CARTESIAN_POINT ( 'NONE',  ( -1.676215897828090107, 1450.511945644329899, 182.4451613505460159 ) ) ;
#95451 = CARTESIAN_POINT ( 'NONE',  ( 5.842913806858009984, 1467.176569223159959, 199.5123709362070201 ) ) ;
#95452 = CARTESIAN_POINT ( 'NONE',  ( -2.531216514170000106E-09, 1476.109324709230123, 267.8540375962979851 ) ) ;
#95453 = CARTESIAN_POINT ( 'NONE',  ( 11.85459483029999994, 1500.917689607990042, 208.6046481015860081 ) ) ;
#95454 = CARTESIAN_POINT ( 'NONE',  ( -28.45104125860000011, 1509.631525670130031, 210.7633834292879840 ) ) ;
#95455 = CARTESIAN_POINT ( 'NONE',  ( 8.481741098329999673, 1422.818662954220144, 213.7027547429590015 ) ) ;
#95456 = CARTESIAN_POINT ( 'NONE',  ( -13.26473696127539981, 1384.881707513919991, 219.1240188487190039 ) ) ;
#95457 = VECTOR ( 'NONE', #86301, 1000.000000000000000 ) ;
#95458 = B_SPLINE_SURFACE_WITH_KNOTS ( 'NONE', 5, 5, ( 
 ( #38683, #37039, #98036, #105356, #62850, #96963 ),
 ( #97501, #12383, #20770, #20228, #46569, #21309 ),
 ( #4549, #57723, #23531, #39799, #107546, #57174 ),
 ( #101319, #75068, #75619, #109217, #22967, #6731 ),
 ( #92944, #48212, #40887, #40337, #31935, #41456 ),
 ( #49859, #65565, #58261, #92382, #32503, #73410 ) ),
 .UNSPECIFIED., .F., .F., .F.,
 ( 6, 6 ),
 ( 6, 6 ),
 ( 6.286300432643599834, 8.359473755869998968 ),
 ( -6.051085639767849584E-05, 1.449160878988990042 ),
 .UNSPECIFIED. ) ;
#95459 = CARTESIAN_POINT ( 'NONE',  ( -18.94485037129999583, 1416.547221147930031, 207.7783220669780064 ) ) ;
#95460 = DIRECTION ( 'NONE',  ( -5.980589973904019347E-17, 1.000000000000000000, -1.736889445713099699E-16 ) ) ;
#95461 = CARTESIAN_POINT ( 'NONE',  ( 26.68817439343250086, 1436.428552520020048, 136.7217815448680085 ) ) ;
#95462 = CARTESIAN_POINT ( 'NONE',  ( -10.38565289721849894, 1396.275735379490015, 205.2936222502430041 ) ) ;
#95463 = ORIENTED_EDGE ( 'NONE', *, *, #109023, .T. ) ;
#95464 = B_SPLINE_CURVE_WITH_KNOTS ( 'NONE', 3,
 ( #64299, #98418, #89474, #12770, #13292, #45843, #30669, #21690, #72690, #79976, #81067, #105743, #47484, #46948, #56435, #90566, #3294, #37426, #28472, #4382, #13845, #38511, #81607, #4912, #39628, #39051, #82168, #71623, #29027, #63213, #97320, #20590, #54789, #88921, #12207, #46402, #80534 ),
 .UNSPECIFIED., .F., .F.,
 ( 4, 2, 2, 1, 1, 2, 2, 2, 2, 1, 1, 1, 2, 2, 2, 2, 1, 1, 1, 1, 2, 2, 4 ),
 ( 0.000000000000000000, 0.1249999999997495059, 0.1874999999996246336, 0.2187499999995654310, 0.2343749999995357880, 0.2421874999995215216, 0.2499999999995072830, 0.3749999999993752775, 0.4374999999993093858, 0.4687499999992708610, 0.4843749999992515987, 0.4921874999992420507, 0.4960937499992379984, 0.4999999999992339461, 0.6249999999992830180, 0.6874999999993065547, 0.7187499999993083311, 0.7343749999993101074, 0.7421874999993202104, 0.7460937499993262056, 0.7480468749993290922, 0.7499999999993318678, 1.000000000000000000 ),
 .UNSPECIFIED. ) ;
#95465 = CARTESIAN_POINT ( 'NONE',  ( -16.78826593861180072, 1409.746375843580154, 225.6242863346600132 ) ) ;
#95466 = CARTESIAN_POINT ( 'NONE',  ( 7.390160694869999602, 1438.194204504490017, 149.6789596403979772 ) ) ;
#95467 = ORIENTED_EDGE ( 'NONE', *, *, #94503, .F. ) ;
#95468 = CARTESIAN_POINT ( 'NONE',  ( -11.39360664099999987, 1501.071473199189995, 211.1722694495890096 ) ) ;
#95469 = FACE_OUTER_BOUND ( 'NONE', #72733, .T. ) ;
#95471 = CARTESIAN_POINT ( 'NONE',  ( -2.107860014578959884, 1457.626357230750273, 219.5693110658939986 ) ) ;
#95470 = CARTESIAN_POINT ( 'NONE',  ( 1.660747496199999951, 1456.055585494690149, 218.8271600400589989 ) ) ;
#95472 = CARTESIAN_POINT ( 'NONE',  ( -4.390466737189999691, 1449.947854720489886, 190.5483265708990075 ) ) ;
#95473 = CARTESIAN_POINT ( 'NONE',  ( 4.145890503519879644, 1424.386680318709978, 184.7442299159029915 ) ) ;
#95474 = CARTESIAN_POINT ( 'NONE',  ( 4.616272296565000488, 1517.030858226499959, 201.7868885755270014 ) ) ;
#95475 = CARTESIAN_POINT ( 'NONE',  ( 7.754157970519999665, 1425.611232019499994, 211.7686771286390126 ) ) ;
#95476 = CARTESIAN_POINT ( 'NONE',  ( 14.43085696089999992, 1426.807557149800004, 195.4949581795989957 ) ) ;
#95477 = FACE_BOUND ( 'NONE', #53483, .T. ) ;
#95478 = CARTESIAN_POINT ( 'NONE',  ( -101.5461033995489828, 1378.133454241549998, 306.5661732367119612 ) ) ;
#95479 = CARTESIAN_POINT ( 'NONE',  ( 9.971295257858800554, 1364.502667329735914, 210.6218459616987957 ) ) ;
#95481 = EDGE_LOOP ( 'NONE', ( #31494, #4741, #88450, #8280, #55978, #37960 ) ) ;
#95480 = CARTESIAN_POINT ( 'NONE',  ( 18.31941652029302858, 1517.151704408390060, 203.8280657238408651 ) ) ;
#95482 = ORIENTED_EDGE ( 'NONE', *, *, #10056, .F. ) ;
#95483 = CARTESIAN_POINT ( 'NONE',  ( -41.66135440509999910, 1443.796918820770088, 135.6885369501979994 ) ) ;
#95484 = CARTESIAN_POINT ( 'NONE',  ( -3.448830483803564828, 1511.187213306747708, 175.1594891075192209 ) ) ;
#95485 = CARTESIAN_POINT ( 'NONE',  ( 10.78871504700000017, 1416.913060387330006, 209.1218460627730167 ) ) ;
#95486 = CARTESIAN_POINT ( 'NONE',  ( -7.983219854955000194, 1511.369014903080142, 214.5214372678569816 ) ) ;
#95487 = CARTESIAN_POINT ( 'NONE',  ( -3.509122693450000163, 1486.112957707730175, 181.9976544228979662 ) ) ;
#95488 = CARTESIAN_POINT ( 'NONE',  ( -31.30542346655892771, 1525.651286436460396, 201.9631088232815443 ) ) ;
#95489 = CARTESIAN_POINT ( 'NONE',  ( 0.8761538346837720592, 1475.978191697550074, 197.6843414950239719 ) ) ;
#95490 = CARTESIAN_POINT ( 'NONE',  ( -33.92643878696880222, 1450.868569007310043, 136.1710250821759871 ) ) ;
#95491 = CARTESIAN_POINT ( 'NONE',  ( -2.500000000000000000, 1448.322085267190005, 163.7893231724509917 ) ) ;
#95492 = CARTESIAN_POINT ( 'NONE',  ( 7.037448402365139799, 1370.316676987425353, 209.6218459617033432 ) ) ;
#95493 = CARTESIAN_POINT ( 'NONE',  ( -0.06764688652389970469, 1408.848989328409971, 194.7501694707590048 ) ) ;
#95494 = CARTESIAN_POINT ( 'NONE',  ( -2.306328001459209798, 1405.753257883129891, 267.8520456273699892 ) ) ;
#95495 = CARTESIAN_POINT ( 'NONE',  ( -14.25060731567010031, 1435.219473732530105, 149.2644110217260334 ) ) ;
#95496 = ORIENTED_EDGE ( 'NONE', *, *, #104098, .F. ) ;
#95497 = CARTESIAN_POINT ( 'NONE',  ( -11.76945428679999850, 1432.334073391449920, 150.8119095936980045 ) ) ;
#95498 = CARTESIAN_POINT ( 'NONE',  ( 13.61829878390000026, 1442.132340210329858, 189.2393822471979945 ) ) ;
#95499 = EDGE_LOOP ( 'NONE', ( #12047, #92196 ) ) ;
#95500 = ORIENTED_EDGE ( 'NONE', *, *, #5277, .T. ) ;
#95501 = CARTESIAN_POINT ( 'NONE',  ( -3.786971751329999858, 1455.326410022090158, 200.4755219205989931 ) ) ;
#95502 = CARTESIAN_POINT ( 'NONE',  ( 0.05823133897989880153, 1360.390585217559874, 207.6218459616989946 ) ) ;
#95503 = CARTESIAN_POINT ( 'NONE',  ( -2.867803664234999772, 1516.994127245590107, 213.7465828294170080 ) ) ;
#95504 = CARTESIAN_POINT ( 'NONE',  ( 3.780286388835000011, 1510.542924508009946, 216.6739878845270084 ) ) ;
#95505 = ORIENTED_EDGE ( 'NONE', *, *, #99444, .F. ) ;
#95506 = CARTESIAN_POINT ( 'NONE',  ( -73.44525058019999619, 1378.783439397329857, 283.9849196026589766 ) ) ;
#95507 =( BOUNDED_CURVE ( )  B_SPLINE_CURVE ( 3, ( #86209, #43667, #70002, #86765 ),
 .UNSPECIFIED., .F., .T. ) 
 B_SPLINE_CURVE_WITH_KNOTS ( ( 4, 4 ),
 ( 4.409610686089010301, 5.070003787395050310 ),
 .UNSPECIFIED. ) 
 CURVE ( )  GEOMETRIC_REPRESENTATION_ITEM ( )  RATIONAL_B_SPLINE_CURVE ( ( 1.000000000000000000, 0.9639857562574201122, 0.9639857562574201122, 1.000000000000000000 ) ) 
 REPRESENTATION_ITEM ( '' )  );
#95508 = CARTESIAN_POINT ( 'NONE',  ( -106.2230645729750051, 1378.913060387289988, 302.3817510371559933 ) ) ;
#95509 = CARTESIAN_POINT ( 'NONE',  ( -2.875850132345000087, 1516.647618671360078, 203.3500485059169876 ) ) ;
#95510 = ADVANCED_FACE ( 'NONE', ( #98591 ), #3471, .F. ) ;
#95511 = CARTESIAN_POINT ( 'NONE',  ( -27.79260863660000069, 1509.155959128430140, 205.2888991007580159 ) ) ;
#95512 = EDGE_CURVE ( 'NONE', #32804, #8029, #104220, .T. ) ;
#95513 = CARTESIAN_POINT ( 'NONE',  ( -2.325731141814999958, 1511.751588929339960, 201.5380540260670159 ) ) ;
#95514 = CARTESIAN_POINT ( 'NONE',  ( -103.7369032989999909, 1385.230281736809957, 296.9336279125589613 ) ) ;
#95515 = CARTESIAN_POINT ( 'NONE',  ( -59.63489001104600362, 1384.670753463339906, 243.2267383120320119 ) ) ;
#95516 = DIRECTION ( 'NONE',  ( 0.03489949670250328678, -0.9993908270190956511, 0.000000000000000000 ) ) ;
#95517 = FACE_OUTER_BOUND ( 'NONE', #22063, .T. ) ;
#95519 = ORIENTED_EDGE ( 'NONE', *, *, #26905, .F. ) ;
#95518 = FACE_OUTER_BOUND ( 'NONE', #16577, .T. ) ;
#95520 = CARTESIAN_POINT ( 'NONE',  ( -14.33372314578957685, 1435.338670000912771, 149.4045306351138152 ) ) ;
#95521 = LINE ( 'NONE', #87691, #21023 ) ;
#95522 = AXIS2_PLACEMENT_3D ( 'NONE', #19373, #20471, #12651 ) ;
#95523 = CARTESIAN_POINT ( 'NONE',  ( -7.332236864109274777, 1441.976884069165862, 202.1892200067096041 ) ) ;
#95524 = CARTESIAN_POINT ( 'NONE',  ( -24.14015075980000091, 1435.359055859420096, 136.8785243455980094 ) ) ;
#95525 = CARTESIAN_POINT ( 'NONE',  ( 5.011678838024999472, 1516.989560013210166, 212.3778133565769792 ) ) ;
#95526 = CARTESIAN_POINT ( 'NONE',  ( -66.92355912140000385, 1379.746314988699851, 276.4200488462589647 ) ) ;
#95527 = ADVANCED_FACE ( 'NONE', ( #38141 ), #48214, .F. ) ;
#95528 = CARTESIAN_POINT ( 'NONE',  ( -9.528680398390617867, 1426.561164775804173, 224.8846064741542818 ) ) ;
#95529 = CARTESIAN_POINT ( 'NONE',  ( -5.292247061280000331, 1391.913060387289988, 214.4361776263990009 ) ) ;
#95530 = CARTESIAN_POINT ( 'NONE',  ( 18.24616163292674997, 1410.913102185548269, 193.8889752366858374 ) ) ;
#95531 = CARTESIAN_POINT ( 'NONE',  ( 1.701850457105000158, 1516.908147884120126, 207.9845492812970065 ) ) ;
#95532 = ORIENTED_EDGE ( 'NONE', *, *, #22963, .F. ) ;
#95533 = CARTESIAN_POINT ( 'NONE',  ( -109.2296128992090019, 1384.847618016620117, 295.1340898668969999 ) ) ;
#95534 = CARTESIAN_POINT ( 'NONE',  ( -5.188689607679999760, 1410.298383163330072, 231.7973492358979968 ) ) ;
#95535 = CARTESIAN_POINT ( 'NONE',  ( -36.11164246829999769, 1384.804902789069956, 235.4725595070590032 ) ) ;
#95536 = ORIENTED_EDGE ( 'NONE', *, *, #66449, .T. ) ;
#95537 = CARTESIAN_POINT ( 'NONE',  ( 21.84020450222056908, 1523.382868172864164, 234.9798068779740277 ) ) ;
#95538 = CARTESIAN_POINT ( 'NONE',  ( -3.471770239069999597, 1428.655773691090189, 200.4250886094789905 ) ) ;
#95539 = CARTESIAN_POINT ( 'NONE',  ( 11.77252734353980124, 1435.203425911839986, 151.2926090376209913 ) ) ;
#95540 = B_SPLINE_SURFACE_WITH_KNOTS ( 'NONE', 5, 5, ( 
 ( #43876, #28172, #70223, #78019, #26503, #45002, #104327, #103198, #95929 ),
 ( #782, #62932, #19189, #10260, #104882, #103779, #10830, #9709, #3003 ),
 ( #88098, #36572, #19763, #11385, #71324, #70771, #45557, #35467, #105438 ),
 ( #28726, #61265, #97044, #95381, #20307, #54510, #18645, #88647, #1326 ),
 ( #52844, #46103, #34912, #60699, #94822, #18099, #69657, #86970, #44437 ),
 ( #47730, #57256, #56683, #48291, #81311, #82434, #71880, #99758, #4627 ),
 ( #47184, #55050, #20855, #4092, #105996, #29272, #55601, #97583, #89178 ),
 ( #29817, #64552, #38762, #64005, #98672, #63464, #14661, #5730, #12470 ),
 ( #90819, #37675, #81863, #21391, #80233, #72936, #46653, #5164, #39322 ) ),
 .UNSPECIFIED., .F., .F., .F.,
 ( 6, 3, 6 ),
 ( 6, 3, 6 ),
 ( 3.580107477860000387, 6.558749095649999639, 9.700153431729999554 ),
 ( 0.000000000000000000, 0.5000000000000000000, 1.000000000000000000 ),
 .UNSPECIFIED. ) ;
#95541 = CARTESIAN_POINT ( 'NONE',  ( 13.45295784994999977, 1488.405218237079907, 232.0949692908260147 ) ) ;
#95542 = CARTESIAN_POINT ( 'NONE',  ( -24.20915078813088073, 1443.685751309060606, 212.4183354952696448 ) ) ;
#95543 = LINE ( 'NONE', #44606, #2877 ) ;
#95544 = CARTESIAN_POINT ( 'NONE',  ( 0.001557819129550000068, 1408.913005912429981, 232.2224884858979976 ) ) ;
#95545 = CARTESIAN_POINT ( 'NONE',  ( 0.01215979767472630084, 1420.444058567659795, 182.6726269972920136 ) ) ;
#95547 = CARTESIAN_POINT ( 'NONE',  ( -3.267314805130000277, 1421.579958532029877, 184.3265788884979770 ) ) ;
#95546 = CARTESIAN_POINT ( 'NONE',  ( 6.556651371285000529, 1516.858146885269889, 215.6747433371770057 ) ) ;
#95548 = CARTESIAN_POINT ( 'NONE',  ( 19.75308522730000149, 1509.626197197730107, 187.0190083296980106 ) ) ;
#95549 = DIRECTION ( 'NONE',  ( 0.000000000000000000, 0.000000000000000000, -1.000000000000000000 ) ) ;
#95550 = ORIENTED_EDGE ( 'NONE', *, *, #74187, .T. ) ;
#95551 = CARTESIAN_POINT ( 'NONE',  ( 2.485205649205000089, 1517.181921232829836, 201.3958557702769951 ) ) ;
#95552 = EDGE_CURVE ( 'NONE', #38397, #23724, #26206, .T. ) ;
#95553 = CARTESIAN_POINT ( 'NONE',  ( -16.44126801270000016, 1495.113783635430082, 185.9757610618979697 ) ) ;
#95554 = ORIENTED_EDGE ( 'NONE', *, *, #74972, .F. ) ;
#95555 = CARTESIAN_POINT ( 'NONE',  ( 3.741709429870000214, 1419.924742150030170, 185.5167356432980057 ) ) ;
#95556 = B_SPLINE_CURVE_WITH_KNOTS ( 'NONE', 3,
 ( #11952, #80264, #20884, #1352, #2484, #1924 ),
 .UNSPECIFIED., .F., .F.,
 ( 4, 2, 4 ),
 ( 0.000000000000000000, 0.5000000000000000000, 1.000000000000000000 ),
 .UNSPECIFIED. ) ;
#95557 = CYLINDRICAL_SURFACE ( 'NONE', #86919, 3.000000000000017764 ) ;
#95558 = EDGE_CURVE ( 'NONE', #4524, #105727, #21856, .T. ) ;
#95559 = CARTESIAN_POINT ( 'NONE',  ( 18.89905511659999959, 1416.828040475729949, 210.6687957193779823 ) ) ;
#95560 = CARTESIAN_POINT ( 'NONE',  ( 3.125212102749999943, 1443.129716313290146, 217.4566555861789823 ) ) ;
#95561 = CARTESIAN_POINT ( 'NONE',  ( 3.829619994797929916, 1515.551704292389786, 207.2788821832570250 ) ) ;
#95562 = CARTESIAN_POINT ( 'NONE',  ( -16.52123881059080190, 1410.013485281883277, 192.0114425483922673 ) ) ;
#95563 = CARTESIAN_POINT ( 'NONE',  ( 17.39559652730000039, 1414.988017874730076, 210.6209831520479838 ) ) ;
#95564 = CARTESIAN_POINT ( 'NONE',  ( -17.96561697639999977, 1423.613351837929940, 225.8447415086979788 ) ) ;
#95565 = CARTESIAN_POINT ( 'NONE',  ( 17.84338787571921614, 1523.382868172864164, 180.3600277896298110 ) ) ;
#95566 = CARTESIAN_POINT ( 'NONE',  ( -16.66936639845670598, 1523.382868172864164, 180.4828114240741854 ) ) ;
#95567 = CARTESIAN_POINT ( 'NONE',  ( -8.301987938657498844, 1517.051704408389924, 185.0111222839169898 ) ) ;
#95569 = CARTESIAN_POINT ( 'NONE',  ( -5.085989740509197610, 1391.850992569807204, 203.6120040231442658 ) ) ;
#95568 = CARTESIAN_POINT ( 'NONE',  ( 0.3188683952948129785, 1408.924195517089856, 231.6706331693599736 ) ) ;
#95570 = CARTESIAN_POINT ( 'NONE',  ( 0.5621804143070269211, 1416.843574548494644, 190.4753774787342593 ) ) ;
#95571 = ORIENTED_EDGE ( 'NONE', *, *, #58846, .T. ) ;
#95572 = CARTESIAN_POINT ( 'NONE',  ( 1.553043158554480163, 1415.595619977640126, 190.7368536681399860 ) ) ;
#95573 = CARTESIAN_POINT ( 'NONE',  ( 27.43355929049999986, 1507.980920699130138, 207.4175378521480013 ) ) ;
#95574 = CARTESIAN_POINT ( 'NONE',  ( -18.43525369369999822, 1507.707328976990084, 209.4281662339789705 ) ) ;
#95575 = CARTESIAN_POINT ( 'NONE',  ( 2.564108462820033907, 1410.380577510105013, 185.5928496559870666 ) ) ;
#95576 = CARTESIAN_POINT ( 'NONE',  ( -3.718627449938214813, 1426.012647860741481, 185.9856829451767908 ) ) ;
#95577 = B_SPLINE_SURFACE_WITH_KNOTS ( 'NONE', 5, 5, ( 
 ( #68821, #50361, #60411, #44158, #67709, #77752 ),
 ( #101818, #102922, #59316, #16697, #50897, #85027 ),
 ( #8320, #76638, #110790, #68276, #45824, #27897 ),
 ( #96206, #46381, #70484, #19481, #11113, #62645 ),
 ( #81047, #78870, #28451, #21117, #104604, #4361 ),
 ( #44718, #2176, #96766, #36291, #63729, #38490 ),
 ( #53683, #62080, #29007, #29542, #71603, #72667 ),
 ( #87825, #3830, #53116, #3274, #106793, #45274 ),
 ( #64277, #37958, #80513, #105159, #10544, #55322 ) ),
 .UNSPECIFIED., .F., .F., .F.,
 ( 6, 3, 6 ),
 ( 6, 6 ),
 ( 2.767471764330379891, 4.758631476969999774, 6.749791190855430223 ),
 ( -0.0004300833054265790429, 2.000000000000000000 ),
 .UNSPECIFIED. ) ;
#95578 = DIRECTION ( 'NONE',  ( -1.755985294532469921E-16, 1.000000000000000000, -1.338183447452831989E-16 ) ) ;
#95579 = CARTESIAN_POINT ( 'NONE',  ( -10.93162295028230169, 1470.132889486390013, 212.2376398131100075 ) ) ;
#95580 = CARTESIAN_POINT ( 'NONE',  ( -4.769978619596870750, 1487.672230412279987, 219.3630103478849946 ) ) ;
#95581 = B_SPLINE_CURVE_WITH_KNOTS ( 'NONE', 5,
 ( #97605, #20875, #80805, #47750, #4111, #55071 ),
 .UNSPECIFIED., .F., .F.,
 ( 6, 6 ),
 ( -65.26194322900001055, -30.28564970649999566 ),
 .UNSPECIFIED. ) ;
#95582 = CARTESIAN_POINT ( 'NONE',  ( -9.771923492860000948, 1448.872168905890021, 190.8346797514990101 ) ) ;
#95583 = CARTESIAN_POINT ( 'NONE',  ( -86.51864351971761380, 1383.772549446489847, 307.1887348928860320 ) ) ;
#95584 = CARTESIAN_POINT ( 'NONE',  ( -109.0938415789800047, 1384.498162415240131, 311.2419644568369677 ) ) ;
#95585 = CARTESIAN_POINT ( 'NONE',  ( -15.53981990976190986, 1506.512156827502622, 224.7632318306688148 ) ) ;
#95586 = CARTESIAN_POINT ( 'NONE',  ( -2.386618527720739902, 1516.532192033489991, 201.4128695281360137 ) ) ;
#95588 = EDGE_LOOP ( 'NONE', ( #98210, #107183, #91058, #23507 ) ) ;
#95587 = CARTESIAN_POINT ( 'NONE',  ( 23.72452558869999706, 1509.749085157929812, 191.5066069952979717 ) ) ;
#95589 = CARTESIAN_POINT ( 'NONE',  ( 17.27558691658489920, 1507.606285602530079, 193.9884222186300065 ) ) ;
#95590 = CARTESIAN_POINT ( 'NONE',  ( -62.22036486049999837, 1383.793512663130059, 284.6761640327590044 ) ) ;
#95591 = CARTESIAN_POINT ( 'NONE',  ( 20.12062199643419902, 1509.247360226100000, 229.8833160286590100 ) ) ;
#95592 = ORIENTED_EDGE ( 'NONE', *, *, #106154, .F. ) ;
#95593 = EDGE_LOOP ( 'NONE', ( #89046, #28817 ) ) ;
#95594 = SPHERICAL_SURFACE ( 'NONE', #11612, 2.000000000000000000 ) ;
#95595 = CARTESIAN_POINT ( 'NONE',  ( -8.921631616102883910, 1502.413060387330006, 192.7909088307800403 ) ) ;
#95596 = CARTESIAN_POINT ( 'NONE',  ( 12.80703219148647065, 1442.847939688957922, 169.4486344618227918 ) ) ;
#95598 = CARTESIAN_POINT ( 'NONE',  ( -39.02581886140000478, 1459.481847435529971, 266.4771544807979922 ) ) ;
#95597 = CARTESIAN_POINT ( 'NONE',  ( 4.613723315850000479E-06, 1474.175172091230024, 270.1377426632980132 ) ) ;
#95599 = AXIS2_PLACEMENT_3D ( 'NONE', #28028, #61661, #95787 ) ;
#95600 = CARTESIAN_POINT ( 'NONE',  ( 8.635265467701518816, 1437.313984394470026, 208.5984011097850157 ) ) ;
#95601 = CARTESIAN_POINT ( 'NONE',  ( -108.8873841550000066, 1383.761288468090015, 297.2879149401589984 ) ) ;
#95602 = CARTESIAN_POINT ( 'NONE',  ( 25.16176845089999858, 1509.119669543930058, 197.7765890071979982 ) ) ;
#95603 = FACE_OUTER_BOUND ( 'NONE', #33398, .T. ) ;
#95604 = CARTESIAN_POINT ( 'NONE',  ( 7.960762779720000459, 1409.191056350230156, 188.6635358462980037 ) ) ;
#95605 = CARTESIAN_POINT ( 'NONE',  ( 4.401092417150000102, 1420.174153566729956, 185.7217845719979721 ) ) ;
#95607 = CARTESIAN_POINT ( 'NONE',  ( -11.23219810570000021, 1436.456444669380062, 151.7916771637979991 ) ) ;
#95606 = CIRCLE ( 'NONE', #109912, 1.999999999999999556 ) ;
#95608 = CARTESIAN_POINT ( 'NONE',  ( 12.38112414749999957, 1436.607677747480011, 151.2275680718979913 ) ) ;
#95609 = CARTESIAN_POINT ( 'NONE',  ( -15.98649555842510139, 1420.860515612879908, 203.3512188490260257 ) ) ;
#95610 = CIRCLE ( 'NONE', #70622, 2.000000000027019720 ) ;
#95611 = CARTESIAN_POINT ( 'NONE',  ( -20.13596110940000017, 1451.396157091630130, 145.7046208320979872 ) ) ;
#95612 = DIRECTION ( 'NONE',  ( 0.000000000000000000, -1.000000000000000000, 0.000000000000000000 ) ) ;
#95613 = ORIENTED_EDGE ( 'NONE', *, *, #82141, .F. ) ;
#95614 = CARTESIAN_POINT ( 'NONE',  ( -3.117394561335489644, 1508.880976916049804, 213.6144879082389991 ) ) ;
#95615 = CARTESIAN_POINT ( 'NONE',  ( 20.63006355019999916, 1477.703139823589936, 217.6305604476790165 ) ) ;
#95616 = CARTESIAN_POINT ( 'NONE',  ( -41.90242663730000316, 1445.386761933250000, 269.8748730912980136 ) ) ;
#95617 = DIRECTION ( 'NONE',  ( 0.6709778558543610938, 0.000000000000000000, -0.7414773880254772465 ) ) ;
#95618 = CARTESIAN_POINT ( 'NONE',  ( 16.40067670619999873, 1409.485784638129871, 222.8653037321979866 ) ) ;
#95619 = CARTESIAN_POINT ( 'NONE',  ( -14.27723474240000101, 1474.170145399029934, 223.9306864886980009 ) ) ;
#95620 = B_SPLINE_CURVE_WITH_KNOTS ( 'NONE', 3,
 ( #47614, #56017, #80107, #29155, #89601, #45431, #3426, #81738, #70644, #63881, #5046, #79575, #97996, #37557, #2879, #63341, #20730, #62805, #30239, #20188, #12339, #46529, #11804, #13424, #104761, #62236, #36998, #87981, #19640, #80664, #3978, #38102, #55475, #12894, #47071, #4513, #72821, #106954, #64432, #98549, #66086, #99089, #90697, #32465, #50382, #39191, #82310, #22367, #108050, #56568, #100213, #92907, #5608, #58770, #15080, #40301, #32992, #41419, #39761, #64974, #74484, #6143, #67181, #66640, #13984, #23495, #48172 ),
 .UNSPECIFIED., .F., .F.,
 ( 4, 3, 3, 3, 3, 3, 3, 3, 3, 3, 3, 3, 3, 3, 3, 3, 3, 3, 3, 3, 3, 3, 4 ),
 ( 17.98526104458165165, 20.20158955684989976, 22.42882872137870010, 24.66064011719250004, 26.89515503936650020, 29.13043065886330041, 31.36321373294149950, 33.59263454627130585, 35.81471763752789883, 36.72584873329999766, 38.94364518594499458, 41.26471793637690411, 43.50295931855809783, 45.74609346697479850, 47.99249668729089535, 50.24046781578599052, 52.48759803034639049, 54.73251631032059095, 56.97222553069789797, 57.51222718939999368, 59.74002163354938943, 61.95813442111268898, 62.49779105520408962 ),
 .UNSPECIFIED. ) ;
#95621 = DIRECTION ( 'NONE',  ( -5.980589973904019347E-17, 1.000000000000000000, -1.736889445713099699E-16 ) ) ;
#95622 = FACE_OUTER_BOUND ( 'NONE', #1444, .T. ) ;
#95623 = CARTESIAN_POINT ( 'NONE',  ( 1.747240526799999971, 1508.468491276929853, 237.2463171569980034 ) ) ;
#95624 = CARTESIAN_POINT ( 'NONE',  ( -4.890835732880000286, 1416.493263303829963, 232.1969941459979907 ) ) ;
#95625 = CARTESIAN_POINT ( 'NONE',  ( -7.672540978279999813, 1458.367780384589878, 214.9746805944489836 ) ) ;
#95626 = CARTESIAN_POINT ( 'NONE',  ( -4.171500989025269668, 1359.775974105520163, 207.6218459616987673 ) ) ;
#95627 = CARTESIAN_POINT ( 'NONE',  ( -44.87017001119260584, 1433.746480055119946, 268.7864504627750080 ) ) ;
#95628 = DIRECTION ( 'NONE',  ( 0.000000000000000000, -1.000000000000000000, 0.000000000000000000 ) ) ;
#95629 = ORIENTED_EDGE ( 'NONE', *, *, #11777, .F. ) ;
#95630 = CARTESIAN_POINT ( 'NONE',  ( -8.813634211109999228, 1423.275147988690151, 209.8404090638680088 ) ) ;
#95631 = ORIENTED_EDGE ( 'NONE', *, *, #22009, .F. ) ;
#95632 = CARTESIAN_POINT ( 'NONE',  ( -0.7374509209069979310, 1516.978425811520083, 210.2554991112269818 ) ) ;
#95633 = CARTESIAN_POINT ( 'NONE',  ( -7.509380800793006294, 1508.909942010299346, 203.6084103740969908 ) ) ;
#95634 = CARTESIAN_POINT ( 'NONE',  ( -18.86688640473562373, 1511.187213306747708, 237.4611898188522332 ) ) ;
#95635 = CARTESIAN_POINT ( 'NONE',  ( -11.52403648599999997, 1410.397193419830046, 189.0409863546979921 ) ) ;
#95636 = CARTESIAN_POINT ( 'NONE',  ( 19.53786426059019021, 1511.187213306747708, 181.5239794925693388 ) ) ;
#95637 = ORIENTED_EDGE ( 'NONE', *, *, #36330, .T. ) ;
#95638 = DIRECTION ( 'NONE',  ( 0.000000000000000000, 0.000000000000000000, 1.000000000000000000 ) ) ;
#95640 = CARTESIAN_POINT ( 'NONE',  ( -15.10400618450110066, 1513.569700117909861, 223.6131665486809936 ) ) ;
#95639 = CARTESIAN_POINT ( 'NONE',  ( -14.45783243223209880, 1416.839692136300073, 221.3920770721769884 ) ) ;
#95641 = VECTOR ( 'NONE', #43711, 1000.000000000000000 ) ;
#95642 = CARTESIAN_POINT ( 'NONE',  ( -0.4375840930677259988, 1487.902785764265445, 219.9692466604490448 ) ) ;
#95643 = CARTESIAN_POINT ( 'NONE',  ( -18.74955383543489873, 1508.522973533499908, 210.3303428506329738 ) ) ;
#95644 = CARTESIAN_POINT ( 'NONE',  ( -0.8775825618903728698, 1398.755125754900064, 209.6012715003031985 ) ) ;
#95646 = AXIS2_PLACEMENT_3D ( 'NONE', #75565, #83938, #59321 ) ;
#95645 = CARTESIAN_POINT ( 'NONE',  ( -8.447729234144269128, 1439.539276948720044, 206.3527110188499876 ) ) ;
#95647 = ORIENTED_EDGE ( 'NONE', *, *, #91784, .F. ) ;
#95648 = CARTESIAN_POINT ( 'NONE',  ( -4.261227898591590346, 1409.354790215370031, 270.3708393906289302 ) ) ;
#95649 = CARTESIAN_POINT ( 'NONE',  ( -1.717139122245000094, 1516.949031626070109, 208.0040058453670042 ) ) ;
#95650 = CARTESIAN_POINT ( 'NONE',  ( 10.58452527300000057, 1419.025207297029965, 230.2384250536979948 ) ) ;
#95651 = CARTESIAN_POINT ( 'NONE',  ( -6.742044282776496367, 1509.032357808383040, 216.2339691194059696 ) ) ;
#95653 = VERTEX_POINT ( 'NONE', #4015 ) ;
#95652 = CARTESIAN_POINT ( 'NONE',  ( -8.232155009531579637, 1367.485244382311976, 210.6218459616987957 ) ) ;
#95654 = ORIENTED_EDGE ( 'NONE', *, *, #50275, .F. ) ;
#95655 = CARTESIAN_POINT ( 'NONE',  ( -4.576312612474010777, 1517.151704408390060, 222.3843417993991807 ) ) ;
#95656 = CARTESIAN_POINT ( 'NONE',  ( -0.1698155278098549825, 1408.918990476199951, 186.4893999992370084 ) ) ;
#95657 = CARTESIAN_POINT ( 'NONE',  ( 3.682239659044672209, 1424.213547858993707, 184.0104720422797300 ) ) ;
#95658 = CARTESIAN_POINT ( 'NONE',  ( -0.02314905646560709920, 1409.040033148099837, 185.8702696072230083 ) ) ;
#95659 = B_SPLINE_SURFACE_WITH_KNOTS ( 'NONE', 5, 5, ( 
 ( #27628, #35474, #45010, #105446, #62940, #11932 ),
 ( #9717, #61815, #104890, #95938, #69105, #19771 ),
 ( #80242, #103206, #19198, #28181, #26511, #94831 ),
 ( #96491, #4099, #108177, #81872, #4632, #13551 ),
 ( #48858, #98123, #82983, #47192, #38223, #48300 ),
 ( #71888, #64012, #5739, #37683, #46660, #107637 ),
 ( #90268, #106003, #106536, #20863, #21940, #22490 ),
 ( #30920, #29279, #21398, #73503, #5173, #39881 ),
 ( #55058, #30371, #63472, #29825, #13006, #99766 ) ),
 .UNSPECIFIED., .F., .F., .F.,
 ( 6, 3, 6 ),
 ( 6, 6 ),
 ( 3.948767879310000062, 7.805279617920000135, 12.92009085129999946 ),
 ( 0.000000000000000000, 2.000000000000000000 ),
 .UNSPECIFIED. ) ;
#95660 = CARTESIAN_POINT ( 'NONE',  ( -18.84390879411339981, 1416.449138223469845, 207.5741054101650036 ) ) ;
#95661 = CARTESIAN_POINT ( 'NONE',  ( -18.65840353449999967, 1420.836464136229779, 224.4798604198980172 ) ) ;
#95662 = EDGE_CURVE ( 'NONE', #44452, #102315, #14764, .T. ) ;
#95663 = CARTESIAN_POINT ( 'NONE',  ( 30.10075563091589856, 1467.602242830489786, 267.1542540607859451 ) ) ;
#95664 = CARTESIAN_POINT ( 'NONE',  ( -2.672061128083995207, 1466.864270888973124, 235.1107451349035955 ) ) ;
#95665 = CARTESIAN_POINT ( 'NONE',  ( 10.57001467410000117, 1445.512273588180051, 185.9502834991980080 ) ) ;
#95666 = CARTESIAN_POINT ( 'NONE',  ( -7.337153806245000354, 1517.119374999550018, 205.8621166342670108 ) ) ;
#95667 = VERTEX_POINT ( 'NONE', #82895 ) ;
#95668 = CARTESIAN_POINT ( 'NONE',  ( 1.751672294820000086, 1443.909066847590111, 215.1365789184590085 ) ) ;
#95669 = CARTESIAN_POINT ( 'NONE',  ( -3.724929251180815193, 1516.669760784821392, 202.6114878535433945 ) ) ;
#95670 = CARTESIAN_POINT ( 'NONE',  ( 22.58840255639999839, 1409.701846760530088, 208.8102578915460015 ) ) ;
#95671 = ORIENTED_EDGE ( 'NONE', *, *, #91834, .F. ) ;
#95672 = CARTESIAN_POINT ( 'NONE',  ( 3.137381254594810542, 1508.729448404669938, 204.5649390561709993 ) ) ;
#95674 = EDGE_CURVE ( 'NONE', #58146, #72871, #84175, .T. ) ;
#95673 = CARTESIAN_POINT ( 'NONE',  ( 25.76476011969039703, 1450.791939427479974, 136.8860263216379849 ) ) ;
#95675 = CARTESIAN_POINT ( 'NONE',  ( -13.58268883541719951, 1416.851343898680170, 221.9096085506480165 ) ) ;
#95676 = CARTESIAN_POINT ( 'NONE',  ( -1.130432680880949984E-15, 1385.340268378329938, 218.5931445290690078 ) ) ;
#95677 = CARTESIAN_POINT ( 'NONE',  ( 6.541070334811199594, 1517.051704644130041, 212.7912326336579838 ) ) ;
#95679 = B_SPLINE_SURFACE_WITH_KNOTS ( 'NONE', 5, 5, ( 
 ( #95676, #10012, #8895, #77234, #43626, #44182, #43074, #535, #27363 ),
 ( #35212, #8341, #35771, #102946, #76118, #77774, #78320, #59339, #86168 ),
 ( #34659, #52586, #68843, #26248, #53139, #60436, #94554, #110814, #33534 ),
 ( #17827, #52032, #42505, #69954, #61545, #110258, #76665, #25136, #93449 ),
 ( #41964, #1086, #16719, #69398, #103509, #26812, #61000, #104068, #34107 ),
 ( #95126, #86719, #68298, #102406, #1634, #99931, #27922, #97323, #88380 ),
 ( #62104, #23225, #11136, #105184, #56300, #2199, #96228, #65266, #2748 ),
 ( #13709, #73667, #36868, #62669, #19505, #28476, #36313, #79979, #47895 ),
 ( #22101, #99376, #5335, #11670, #87277, #53709, #70510, #45296, #104625 ),
 ( #31632, #87848, #108351, #63216, #45846, #82603, #90986, #79436, #71062 ),
 ( #107798, #82031, #96790, #20060, #14274, #90431, #39495, #31083, #54254 ),
 ( #22651, #56855, #3298, #48465, #37429, #10571, #5893, #40039, #71626 ),
 ( #105747, #29031, #74222, #65813, #44743, #78893, #59068, #68573, #93191 ),
 ( #42804, #32741, #58511, #76399, #108901, #66921, #102676, #57425, #16460 ),
 ( #32191, #50654, #101030, #66376, #24328, #92641, #49563, #17003, #92095 ),
 ( #110553, #67472, #84243, #40591, #6987, #84785, #34400, #6445, #8629 ),
 ( #75320, #33839, #25417, #7541, #15915, #109462, #50114, #101577, #102139 ),
 ( #41696, #24865, #75855, #74762, #76964, #57962, #83692, #8083, #15374 ),
 ( #41141, #59612, #274, #110005, #33282, #91550, #23775, #42252, #68029 ),
 ( #100494, #93725, #51203, #14827, #85332, #49014, #83150, #17567, #18135 ),
 ( #1361, #817, #1933, #3042, #43368, #43912, #103815, #28208, #26545 ),
 ( #103233, #45592, #36070, #27115, #19799, #62397, #60738, #51767, #61299 ),
 ( #19226, #77516, #52332, #96522, #70255, #104362, #27659, #9746, #95418 ),
 ( #61846, #95965, #18681, #53433, #78056, #37168, #54003, #87580, #94860 ),
 ( #86455, #35503, #52879, #69696, #36609, #10868, #87007, #71364, #85901 ),
 ( #25972, #10296, #9208, #44472, #78617, #45041, #79186, #88135, #60171 ),
 ( #2492, #70810, #34945, #69130, #104923, #94289, #11423, #79733, #106569 ),
 ( #46146, #5772, #29307, #12512, #72977, #20345, #80276, #81904, #20892 ),
 ( #30403, #90302, #55090, #80822, #37714, #46691, #54549, #98158, #64594 ),
 ( #38802, #5209, #21973, #29855, #105476, #71916, #88683, #63506, #11960 ) ),
 .UNSPECIFIED., .F., .F., .F.,
 ( 6, 3, 3, 3, 3, 3, 3, 3, 3, 6 ),
 ( 6, 3, 6 ),
 ( 0.000000000000000000, 15.39383910899999997, 27.58084801740000103, 41.39509552349999666, 65.53909258059999843, 90.91108773649999364, 117.6367619669999982, 132.4493970709999928, 144.8160795070000120, 161.8240513320000105 ),
 ( 34.48604544350000367, 51.30231389200000081, 68.11858234059999972 ),
 .UNSPECIFIED. ) ;
#95678 = CARTESIAN_POINT ( 'NONE',  ( 18.58065462780000132, 1409.726647492329903, 195.6460095527979774 ) ) ;
#95680 = CARTESIAN_POINT ( 'NONE',  ( 27.40283359139997543, 1444.740067931808653, 161.6370709818978639 ) ) ;
#95681 = CIRCLE ( 'NONE', #86724, 1.999999999999999556 ) ;
#95682 = SPHERICAL_SURFACE ( 'NONE', #37460, 2.000000000000000000 ) ;
#95684 = CARTESIAN_POINT ( 'NONE',  ( -19.31676357336673533, 1425.378157214008525, 223.6971631259767719 ) ) ;
#95683 = CARTESIAN_POINT ( 'NONE',  ( -9.094129269030000629, 1384.954944735329946, 199.9429221374590213 ) ) ;
#95685 = CARTESIAN_POINT ( 'NONE',  ( 0.5746359205532659553, 1452.648651194650029, 183.3151952156349864 ) ) ;
#95686 = LINE ( 'NONE', #77784, #30303 ) ;
#95687 = CARTESIAN_POINT ( 'NONE',  ( 28.17856934087275889, 1509.667335739465443, 207.1106753066228237 ) ) ;
#95688 = CARTESIAN_POINT ( 'NONE',  ( 2.489617538345000103, 1516.665179208830068, 214.1178407578070164 ) ) ;
#95689 = CARTESIAN_POINT ( 'NONE',  ( 3.177699364621945133, 1525.042337199240137, 241.6057670631459473 ) ) ;
#95690 = ORIENTED_EDGE ( 'NONE', *, *, #56468, .T. ) ;
#95691 = FACE_OUTER_BOUND ( 'NONE', #84967, .T. ) ;
#95692 = CARTESIAN_POINT ( 'NONE',  ( 20.38673671613172900, 1525.878013734320803, 236.1208636900216788 ) ) ;
#95693 = CARTESIAN_POINT ( 'NONE',  ( -0.4973741856806139783, 1409.710427932380071, 233.0131125714380005 ) ) ;
#95694 = CARTESIAN_POINT ( 'NONE',  ( -20.46845896326908587, 1507.979024348134317, 209.5470984320012917 ) ) ;
#95695 = CARTESIAN_POINT ( 'NONE',  ( -0.2472255341746696089, 1420.996142865428283, 193.7190874371098346 ) ) ;
#95696 = DIRECTION ( 'NONE',  ( 0.000000000000000000, 1.000000000000000000, 0.000000000000000000 ) ) ;
#95697 = CARTESIAN_POINT ( 'NONE',  ( -19.02913997099999932, 1445.216574189620133, 214.3676144198679765 ) ) ;
#95698 = CARTESIAN_POINT ( 'NONE',  ( -28.62143996450560834, 1526.335487865669165, 198.0561880438515914 ) ) ;
#95699 = DIRECTION ( 'NONE',  ( -0.07713599384728302144, -0.9969860201949398704, 0.008301444997534872250 ) ) ;
#95700 = CARTESIAN_POINT ( 'NONE',  ( 6.850948855039999508, 1456.378850165029917, 224.8635561905979898 ) ) ;
#95701 = B_SPLINE_SURFACE_WITH_KNOTS ( 'NONE', 5, 5, ( 
 ( #7466, #99440, #22717, #56918, #91048, #93119 ),
 ( #18060, #104293, #11891, #61227, #63428, #87503 ),
 ( #43838, #104845, #35993, #2966, #28132, #46063 ),
 ( #103738, #77984, #35430, #88609, #61765, #44402 ),
 ( #10224, #69617, #79662, #96448, #19151, #78544 ),
 ( #9666, #88063, #11348, #1858, #79111, #27039 ) ),
 .UNSPECIFIED., .F., .F., .F.,
 ( 6, 6 ),
 ( 6, 6 ),
 ( 2.088384708059999983, 2.452169171380000012 ),
 ( 0.000000000000000000, 0.2999999999999999889 ),
 .UNSPECIFIED. ) ;
#95702 = CARTESIAN_POINT ( 'NONE',  ( -16.87240959569610155, 1409.502257913620042, 196.1298155364530089 ) ) ;
#95703 = CARTESIAN_POINT ( 'NONE',  ( 14.04725111459999987, 1429.738167031290004, 194.8870957077990340 ) ) ;
#95704 = CARTESIAN_POINT ( 'NONE',  ( -106.0556725455072211, 1391.049867165201249, 307.0681147628054646 ) ) ;
#95705 = CARTESIAN_POINT ( 'NONE',  ( 10.71266894638830003, 1462.053231644700190, 211.5459097712770244 ) ) ;
#95706 = CARTESIAN_POINT ( 'NONE',  ( 0.000000000000000000, 1512.187213306747481, 209.1218459616979999 ) ) ;
#95707 = CARTESIAN_POINT ( 'NONE',  ( -1.689251544525047333, 1526.344110814223541, 239.7716210576163576 ) ) ;
#95708 = CARTESIAN_POINT ( 'NONE',  ( -7.613477210479999258, 1509.311637010430104, 239.1480524702979835 ) ) ;
#95709 = CARTESIAN_POINT ( 'NONE',  ( 25.44333967330000235, 1449.802117268759957, 210.9399225570080034 ) ) ;
#95710 = CARTESIAN_POINT ( 'NONE',  ( -15.60279201232230406, 1420.350159234621287, 210.5032511881165931 ) ) ;
#95711 = CARTESIAN_POINT ( 'NONE',  ( 26.41054897472661978, 1436.719299170789100, 136.8255246990474348 ) ) ;
#95712 = CARTESIAN_POINT ( 'NONE',  ( -32.73835355732309438, 1383.838552529339950, 230.9115847139019877 ) ) ;
#95713 = AXIS2_PLACEMENT_3D ( 'NONE', #18711, #16492, #17596 ) ;
#95714 = CARTESIAN_POINT ( 'NONE',  ( 20.75865324819899982, 1455.056399446189971, 207.3304374463790225 ) ) ;
#95715 = CARTESIAN_POINT ( 'NONE',  ( -2.284526496774999860, 1516.956048353049937, 212.5847947667770086 ) ) ;
#95716 = CARTESIAN_POINT ( 'NONE',  ( -4.038582018629999659, 1515.598601288590089, 209.1218459616989946 ) ) ;
#95717 = CARTESIAN_POINT ( 'NONE',  ( 0.1612883661501749999, 1485.492233344150009, 181.8584284546379877 ) ) ;
#95719 = ORIENTED_EDGE ( 'NONE', *, *, #53684, .F. ) ;
#95718 = CARTESIAN_POINT ( 'NONE',  ( 3.616466670889999957, 1441.209878957790124, 217.9421667894289953 ) ) ;
#95720 = CARTESIAN_POINT ( 'NONE',  ( -0.7132217361829999991, 1416.830001031129996, 227.9186326107979994 ) ) ;
#95721 = CARTESIAN_POINT ( 'NONE',  ( -5.504892848440839376E-16, 1382.319254473250112, 217.9325275017089893 ) ) ;
#95722 = CARTESIAN_POINT ( 'NONE',  ( -4.519117204389999642, 1475.824012005989971, 199.8305589088090244 ) ) ;
#95724 = VERTEX_POINT ( 'NONE', #31385 ) ;
#95723 = CARTESIAN_POINT ( 'NONE',  ( -39.03583412959209653, 1449.647124672839936, 134.0999999981079895 ) ) ;
#95725 = CARTESIAN_POINT ( 'NONE',  ( -6.857441324633220425, 1508.551704407529996, 219.2237596246229714 ) ) ;
#95726 = ORIENTED_EDGE ( 'NONE', *, *, #97295, .T. ) ;
#95727 = CIRCLE ( 'NONE', #81394, 1.000006598386372847 ) ;
#95728 = CARTESIAN_POINT ( 'NONE',  ( -14.51787070936009805, 1379.822861006080075, 208.4144866268740088 ) ) ;
#95729 = CARTESIAN_POINT ( 'NONE',  ( -15.72677893080000011, 1414.913060387329779, 214.0342601902979993 ) ) ;
#95730 = DIRECTION ( 'NONE',  ( 0.000000000000000000, 0.000000000000000000, 1.000000000000000000 ) ) ;
#95731 = CARTESIAN_POINT ( 'NONE',  ( -2.929459774008567052, 1368.457002613392888, 210.4238567519766718 ) ) ;
#95732 = CARTESIAN_POINT ( 'NONE',  ( 0.8465099650069989323, 1430.128328917089902, 217.4134727424889775 ) ) ;
#95733 = CARTESIAN_POINT ( 'NONE',  ( -12.31752010984839885, 1377.944433743309901, 209.1218459601290078 ) ) ;
#95734 = CARTESIAN_POINT ( 'NONE',  ( 14.04090786536569979, 1409.403379694359955, 204.0234149207160215 ) ) ;
#95735 = CARTESIAN_POINT ( 'NONE',  ( -11.76014441919999953, 1391.665771868209958, 205.8582101077390121 ) ) ;
#95736 = CARTESIAN_POINT ( 'NONE',  ( -96.75293248057811013, 1385.212375750189949, 295.5163800457769980 ) ) ;
#95737 = DIRECTION ( 'NONE',  ( -0.000000000000000000, -1.000000000000000000, -0.000000000000000000 ) ) ;
#95738 = CARTESIAN_POINT ( 'NONE',  ( 11.19141260661350046, 1422.145557588919928, 210.4507437126630123 ) ) ;
#95739 = ORIENTED_EDGE ( 'NONE', *, *, #52786, .T. ) ;
#95740 = CARTESIAN_POINT ( 'NONE',  ( 13.51812398686129590, 1443.913060387330006, 169.4008117781763190 ) ) ;
#95742 = EDGE_LOOP ( 'NONE', ( #80978, #53021, #95744, #11024 ) ) ;
#95741 = DIRECTION ( 'NONE',  ( 0.000000000000000000, 1.000000000000000000, 0.000000000000000000 ) ) ;
#95743 = CARTESIAN_POINT ( 'NONE',  ( 26.79413740735880367, 1436.761939593030093, 136.7822073642480234 ) ) ;
#95744 = ORIENTED_EDGE ( 'NONE', *, *, #48902, .F. ) ;
#95745 = CARTESIAN_POINT ( 'NONE',  ( 1.842962215208693078, 1515.492058412108918, 204.9833025688982104 ) ) ;
#95746 = CARTESIAN_POINT ( 'NONE',  ( -3.982247585419859792, 1360.759224656412016, 210.6218459616987957 ) ) ;
#95747 = CARTESIAN_POINT ( 'NONE',  ( 2.500000000000000000, 1432.413060387330006, 146.1721969590979882 ) ) ;
#95748 = CARTESIAN_POINT ( 'NONE',  ( 29.34286956283065351, 1509.949564053853237, 212.7810611423796274 ) ) ;
#95749 = CARTESIAN_POINT ( 'NONE',  ( -31.55762699681115180, 1523.390106123591067, 221.9258384720632478 ) ) ;
#95750 = CARTESIAN_POINT ( 'NONE',  ( 3.730133759040000108, 1396.578896005830075, 221.1163315688980049 ) ) ;
#95751 = CARTESIAN_POINT ( 'NONE',  ( 32.28351601132058590, 1524.972613296804866, 201.2030752716693485 ) ) ;
#95752 = CARTESIAN_POINT ( 'NONE',  ( -7.151171913976369865, 1516.544165615068778, 211.3944463322366687 ) ) ;
#95753 = CARTESIAN_POINT ( 'NONE',  ( -0.1410079938730000038, 1452.166108153929827, 183.2447143824980174 ) ) ;
#95754 = CARTESIAN_POINT ( 'NONE',  ( -8.696701630024261220, 1367.135748871425903, 210.6218459616991936 ) ) ;
#95755 = CARTESIAN_POINT ( 'NONE',  ( -8.788316527315000570, 1511.741868877540128, 215.3741124244170067 ) ) ;
#95756 = CARTESIAN_POINT ( 'NONE',  ( 1.145290941939999918, 1458.110488011190000, 199.6352770980190030 ) ) ;
#95757 = CARTESIAN_POINT ( 'NONE',  ( -2.299983615734999987, 1516.861367446839949, 206.8392230197369770 ) ) ;
#95758 = CARTESIAN_POINT ( 'NONE',  ( -12.93890803109800025, 1435.979775554859998, 150.7709582610100085 ) ) ;
#95759 = CARTESIAN_POINT ( 'NONE',  ( -2.500000000000000000, 1432.399285533179864, 157.4964730843979908 ) ) ;
#95760 = CARTESIAN_POINT ( 'NONE',  ( 20.59684415428669979, 1507.762623717989982, 227.6602567528719874 ) ) ;
#95762 = ORIENTED_EDGE ( 'NONE', *, *, #87210, .F. ) ;
#95761 = CARTESIAN_POINT ( 'NONE',  ( -3.584843346320000013, 1496.864215273689979, 220.1846651968990045 ) ) ;
#95763 = CARTESIAN_POINT ( 'NONE',  ( 10.98592888559996261, 1414.913372219064513, 222.1709358777573300 ) ) ;
#95764 = ORIENTED_EDGE ( 'NONE', *, *, #68472, .T. ) ;
#95765 = CARTESIAN_POINT ( 'NONE',  ( 40.44435966889999889, 1427.769452941630107, 264.0385845990979874 ) ) ;
#95766 = CARTESIAN_POINT ( 'NONE',  ( -25.80166435900000010, 1469.242112534130229, 205.3110786689379950 ) ) ;
#95769 = CARTESIAN_POINT ( 'NONE',  ( 16.54156502434519993, 1409.738807616770146, 192.3741591556930075 ) ) ;
#95768 = AXIS2_PLACEMENT_3D ( 'NONE', #40647, #74277, #58567 ) ;
#95767 = CARTESIAN_POINT ( 'NONE',  ( -11.09416012139399932, 1426.481981508449962, 97.52552186591471184 ) ) ;
#95770 = CARTESIAN_POINT ( 'NONE',  ( 2.879956924955000108, 1516.827328999679821, 212.3743765858270081 ) ) ;
#95771 = CARTESIAN_POINT ( 'NONE',  ( -20.56075711880000156, 1453.152003547930008, 208.0036112637379802 ) ) ;
#95772 = CARTESIAN_POINT ( 'NONE',  ( -30.53571888319999772, 1440.913060383969878, 240.1260121746980190 ) ) ;
#95773 = CARTESIAN_POINT ( 'NONE',  ( -13.79573821373410070, 1379.664681114740006, 208.3123142327969788 ) ) ;
#95774 = CARTESIAN_POINT ( 'NONE',  ( 28.26734827506700043, 1508.339354035630095, 209.3952658968800051 ) ) ;
#95775 = CARTESIAN_POINT ( 'NONE',  ( 3.892100939925419834, 1508.551704408389924, 213.6765049832410170 ) ) ;
#95776 = CARTESIAN_POINT ( 'NONE',  ( 30.81588140580000257, 1450.976146373729762, 136.2622935297980007 ) ) ;
#95777 = VERTEX_POINT ( 'NONE', #16218 ) ;
#95778 = CARTESIAN_POINT ( 'NONE',  ( 13.97631160088559987, 1398.327271670460050, 206.9408228097399842 ) ) ;
#95779 = CARTESIAN_POINT ( 'NONE',  ( 10.21143262099270110, 1460.458462329770100, 206.7445078786060151 ) ) ;
#95780 = CARTESIAN_POINT ( 'NONE',  ( -16.96621030040000022, 1460.582762785830027, 228.2621070505979901 ) ) ;
#95781 = ORIENTED_EDGE ( 'NONE', *, *, #17357, .T. ) ;
#95782 = EDGE_LOOP ( 'NONE', ( #66408, #85574, #41081, #46505, #43887, #109713 ) ) ;
#95783 = CARTESIAN_POINT ( 'NONE',  ( 8.916180505392530264, 1451.556357916370189, 211.6695736768569986 ) ) ;
#95784 = CARTESIAN_POINT ( 'NONE',  ( 8.766925616880000049, 1424.448725112169996, 196.2368360184990195 ) ) ;
#95785 = ORIENTED_EDGE ( 'NONE', *, *, #63283, .F. ) ;
#95786 = CARTESIAN_POINT ( 'NONE',  ( -0.3007994230680000602, 1410.295996030029983, 184.9875845314979870 ) ) ;
#95787 = DIRECTION ( 'NONE',  ( 0.9455185755993178454, 0.000000000000000000, -0.3255681544571539243 ) ) ;
#95788 = CARTESIAN_POINT ( 'NONE',  ( -17.13440814833080239, 1415.954755713489931, 207.6490729647759963 ) ) ;
#95789 = CARTESIAN_POINT ( 'NONE',  ( 27.73009239421291738, 1509.592381426173688, 206.1248223153826018 ) ) ;
#95790 = CARTESIAN_POINT ( 'NONE',  ( 7.260542949781179978, 1508.878901734200099, 202.3557440548540285 ) ) ;
#95791 = VECTOR ( 'NONE', #105921, 1000.000000000000000 ) ;
#95792 = CARTESIAN_POINT ( 'NONE',  ( 3.586339042944246103, 1515.071394417499278, 213.2045494097142182 ) ) ;
#95793 = CARTESIAN_POINT ( 'NONE',  ( 14.61618271530000079, 1485.702860713229938, 225.6110866044979844 ) ) ;
#95794 = ORIENTED_EDGE ( 'NONE', *, *, #47144, .F. ) ;
#95795 = CARTESIAN_POINT ( 'NONE',  ( -5.780861274184998955, 1516.783701990830195, 202.1826264492970324 ) ) ;
#95796 = CARTESIAN_POINT ( 'NONE',  ( -3.449647478144999724, 1516.829948096479939, 209.8791439064560223 ) ) ;
#95797 = ORIENTED_EDGE ( 'NONE', *, *, #5805, .T. ) ;
#95798 = CARTESIAN_POINT ( 'NONE',  ( 11.86596557949130037, 1432.326593078920041, 149.9824129838200122 ) ) ;
#95799 = CARTESIAN_POINT ( 'NONE',  ( 12.97442686480655105, 1444.894871287640854, 186.8703375745810433 ) ) ;
#95800 = EDGE_LOOP ( 'NONE', ( #46384, #101975, #101665, #9064 ) ) ;
#95801 = CARTESIAN_POINT ( 'NONE',  ( -15.64138586705021439, 1506.512156834081452, 193.5820260421716341 ) ) ;
#95802 = CARTESIAN_POINT ( 'NONE',  ( -17.22654844235838567, 1443.501467202828508, 162.9224179604370590 ) ) ;
#95803 = CARTESIAN_POINT ( 'NONE',  ( 9.320231801240000280, 1509.238530053529985, 236.4405149249979843 ) ) ;
#95804 = AXIS2_PLACEMENT_3D ( 'NONE', #58368, #43223, #130 ) ;
#95805 = CARTESIAN_POINT ( 'NONE',  ( -6.232811146862309748, 1469.026420360470183, 218.0650955369210067 ) ) ;
#95806 = CARTESIAN_POINT ( 'NONE',  ( -4.917472706919999936, 1423.551379642630081, 185.2203775299980180 ) ) ;
#95807 = CARTESIAN_POINT ( 'NONE',  ( 1.408315213735060079, 1410.404276229229936, 269.3348398410649907 ) ) ;
#95808 = CARTESIAN_POINT ( 'NONE',  ( -0.4346943098025670138, 1517.051704408590012, 216.8444262844809884 ) ) ;
#95809 = CARTESIAN_POINT ( 'NONE',  ( -109.8548145285198387, 1383.584493755403855, 297.0890030339772352 ) ) ;
#95810 = CARTESIAN_POINT ( 'NONE',  ( 10.13319077529999923, 1492.435480105489887, 213.9998358472890061 ) ) ;
#95811 = CARTESIAN_POINT ( 'NONE',  ( -32.61735071319999690, 1379.648822273989936, 216.0058851815090009 ) ) ;
#95812 = CARTESIAN_POINT ( 'NONE',  ( 0.02397233824938014776, 1410.267331098299337, 233.2206758637736641 ) ) ;
#95814 = CARTESIAN_POINT ( 'NONE',  ( 9.322115572355668789, 1468.760034264159913, 202.8348514626249823 ) ) ;
#95813 = CARTESIAN_POINT ( 'NONE',  ( -17.66977881397309957, 1441.975104135429774, 190.8615125109639905 ) ) ;
#95815 = CARTESIAN_POINT ( 'NONE',  ( -4.659955688642280158, 1423.687082602238888, 184.4627326681991519 ) ) ;
#95816 = CARTESIAN_POINT ( 'NONE',  ( 17.83380995714600203, 1418.265691733389986, 225.0226617803320153 ) ) ;
#95817 = CARTESIAN_POINT ( 'NONE',  ( -6.998420887974999616, 1512.696049264740168, 200.9299854953570161 ) ) ;
#95818 = ORIENTED_EDGE ( 'NONE', *, *, #60246, .T. ) ;
#95819 = CARTESIAN_POINT ( 'NONE',  ( 13.21926162809999994, 1421.359897795430015, 248.0989693021979861 ) ) ;
#95820 = CARTESIAN_POINT ( 'NONE',  ( 12.89607781515299934, 1434.724834403989917, 149.2206011272099886 ) ) ;
#95821 = CARTESIAN_POINT ( 'NONE',  ( 41.61761706904538016, 1445.085543264303851, 135.5084622535695189 ) ) ;
#95822 = CARTESIAN_POINT ( 'NONE',  ( 3.753799318440000032, 1506.440767537289958, 220.3044440926989864 ) ) ;
#95823 =( BOUNDED_CURVE ( )  B_SPLINE_CURVE ( 3, ( #41498, #51001, #56, #92983 ),
 .UNSPECIFIED., .F., .F. ) 
 B_SPLINE_CURVE_WITH_KNOTS ( ( 4, 4 ),
 ( 2.356690338815510266, 3.926801539092879878 ),
 .UNSPECIFIED. ) 
 CURVE ( )  GEOMETRIC_REPRESENTATION_ITEM ( )  RATIONAL_B_SPLINE_CURVE ( ( 1.000000000000000000, 0.8048993123304821751, 0.8048993123304821751, 1.000000000000000000 ) ) 
 REPRESENTATION_ITEM ( '' )  );
#95824 = DIRECTION ( 'NONE',  ( 0.9942586961433743653, 0.000000000000000000, -0.1070030146457445208 ) ) ;
#95826 = ORIENTED_EDGE ( 'NONE', *, *, #24225, .F. ) ;
#95825 = CARTESIAN_POINT ( 'NONE',  ( -1.324264359524509826, 1515.084669001950033, 204.7929176606560304 ) ) ;
#95827 = CARTESIAN_POINT ( 'NONE',  ( -16.88834672024129802, 1418.279337056010036, 203.8013833312560052 ) ) ;
#95828 = FACE_OUTER_BOUND ( 'NONE', #72833, .T. ) ;
#95829 = CARTESIAN_POINT ( 'NONE',  ( -16.53913957400000001, 1417.008824413999946, 208.4907982911209956 ) ) ;
#95830 = CARTESIAN_POINT ( 'NONE',  ( -0.02536948887749890247, 1430.362855603430035, 199.7013224701310037 ) ) ;
#95831 = CARTESIAN_POINT ( 'NONE',  ( 2.000821305087136182, 1443.721900349954467, 217.8590849949153210 ) ) ;
#95832 = CARTESIAN_POINT ( 'NONE',  ( 3.145310910306181373, 1370.220870732725871, 208.0282141261312461 ) ) ;
#95833 = CARTESIAN_POINT ( 'NONE',  ( -4.992349871978174924, 1391.620913784733830, 203.7130789026546154 ) ) ;
#95834 = DIRECTION ( 'NONE',  ( 1.000000000000000000, 0.000000000000000000, 0.000000000000000000 ) ) ;
#95835 = CARTESIAN_POINT ( 'NONE',  ( -3.462069005146249712, 1432.317263652611473, 156.5316857334014742 ) ) ;
#95836 = CARTESIAN_POINT ( 'NONE',  ( 16.05001174970000122, 1415.088660905229972, 227.0871310919980033 ) ) ;
#95837 = EDGE_CURVE ( 'NONE', #91956, #74589, #88814, .T. ) ;
#95838 = DIRECTION ( 'NONE',  ( 0.000000000000000000, 0.000000000000000000, -1.000000000000000000 ) ) ;
#95839 = CARTESIAN_POINT ( 'NONE',  ( 3.487592431604999987, 1508.551704408389924, 204.1347675156769981 ) ) ;
#95840 = CARTESIAN_POINT ( 'NONE',  ( -4.043366258305000294, 1516.951766529250108, 206.2549880390970145 ) ) ;
#95841 = CARTESIAN_POINT ( 'NONE',  ( 45.88373594299999780, 1440.913082249800027, 266.4124089362979930 ) ) ;
#95842 = CARTESIAN_POINT ( 'NONE',  ( -31.97190655716442009, 1524.330813522192102, 216.6896206998355296 ) ) ;
#95843 = CARTESIAN_POINT ( 'NONE',  ( 22.52657835689999644, 1435.284668822589992, 140.3430705305979984 ) ) ;
#95844 = CARTESIAN_POINT ( 'NONE',  ( 18.82137020720000109, 1469.164158803430155, 190.2666150881979945 ) ) ;
#95845 = CARTESIAN_POINT ( 'NONE',  ( -22.44438185779999984, 1431.713525257879837, 217.1040214957579906 ) ) ;
#95846 = AXIS2_PLACEMENT_3D ( 'NONE', #102791, #41802, #9858 ) ;
#95847 = CARTESIAN_POINT ( 'NONE',  ( -14.43005995440260136, 1379.618177126189948, 208.1145997592700212 ) ) ;
#95848 = CIRCLE ( 'NONE', #26044, 95.87906523535615122 ) ;
#95849 = CARTESIAN_POINT ( 'NONE',  ( -30.02861084270000092, 1467.289302230230078, 266.6068817451980522 ) ) ;
#95850 = CARTESIAN_POINT ( 'NONE',  ( 0.000000000000000000, 1512.187213306747481, 209.1218459616979999 ) ) ;
#95851 = CARTESIAN_POINT ( 'NONE',  ( -41.62602271621380368, 1442.681057008499920, 135.5698544226029867 ) ) ;
#95852 = CARTESIAN_POINT ( 'NONE',  ( -13.30361715113500054, 1409.377633542329932, 226.2974599518520336 ) ) ;
#95853 = CARTESIAN_POINT ( 'NONE',  ( -15.41862096090000200, 1414.824310420299980, 208.6539393912370031 ) ) ;
#95854 = CARTESIAN_POINT ( 'NONE',  ( -12.24704195820000052, 1441.485080693249984, 187.8203993633979962 ) ) ;
#95855 = CARTESIAN_POINT ( 'NONE',  ( -7.596271589240429556, 1384.058932579810062, 219.0207375155539751 ) ) ;
#95856 = CARTESIAN_POINT ( 'NONE',  ( 17.85886714360680116, 1428.995146824200219, 205.7472297062370217 ) ) ;
#95857 = CARTESIAN_POINT ( 'NONE',  ( 9.682511080499990541, 1436.279831232390052, 210.8541354582289955 ) ) ;
#95858 = ORIENTED_EDGE ( 'NONE', *, *, #125, .F. ) ;
#95859 = CARTESIAN_POINT ( 'NONE',  ( 5.750872949060175543, 1510.549724832337461, 216.6642929926275087 ) ) ;
#95860 = CARTESIAN_POINT ( 'NONE',  ( -14.05364299196800104, 1409.403824414780047, 214.1745042107170036 ) ) ;
#95861 = FACE_OUTER_BOUND ( 'NONE', #101119, .T. ) ;
#95862 = CARTESIAN_POINT ( 'NONE',  ( -22.12673812478050195, 1409.685743108969973, 209.8966867368829980 ) ) ;
#95863 = CARTESIAN_POINT ( 'NONE',  ( -42.07525187489999752, 1455.849900366930115, 266.2935987290980506 ) ) ;
#95864 = CARTESIAN_POINT ( 'NONE',  ( -11.64243205524850033, 1481.168562452440028, 211.2324576138770169 ) ) ;
#95865 = CARTESIAN_POINT ( 'NONE',  ( 0.1666873299777550110, 1420.332927348350040, 183.4666007823460063 ) ) ;
#95866 = CARTESIAN_POINT ( 'NONE',  ( -28.08612064899999794, 1509.893849332430136, 216.7264453898779948 ) ) ;
#95867 = CARTESIAN_POINT ( 'NONE',  ( -69.80456196563160631, 1384.663061549279973, 294.8462645368060180 ) ) ;
#95868 = CARTESIAN_POINT ( 'NONE',  ( -34.80461611804459920, 1384.978283401549788, 208.5676735308819900 ) ) ;
#95869 = CARTESIAN_POINT ( 'NONE',  ( 17.18900436376040020, 1422.349201594700162, 226.7290623181470153 ) ) ;
#95870 = CARTESIAN_POINT ( 'NONE',  ( 13.02322702420000056, 1416.825784011830137, 221.6328457789979893 ) ) ;
#95871 = CARTESIAN_POINT ( 'NONE',  ( 14.97303230589999856, 1485.053194597530137, 223.9694979347979711 ) ) ;
#95872 = CIRCLE ( 'NONE', #40479, 1.000000000000000888 ) ;
#95873 = DIRECTION ( 'NONE',  ( 0.000000000000000000, 0.000000000000000000, 1.000000000000000000 ) ) ;
#95874 = CARTESIAN_POINT ( 'NONE',  ( 4.201107383170000098, 1515.456955069890228, 208.0103411306490102 ) ) ;
#95875 = CARTESIAN_POINT ( 'NONE',  ( -7.966081152810000177, 1384.918389262350047, 199.4892680610689979 ) ) ;
#95876 = ADVANCED_FACE ( 'NONE', ( #23533 ), #104336, .T. ) ;
#95877 = CARTESIAN_POINT ( 'NONE',  ( -9.767576865947649623, 1416.948096802409964, 202.3623712837820108 ) ) ;
#95878 = EDGE_CURVE ( 'NONE', #33349, #90510, #53101, .T. ) ;
#95879 = EDGE_CURVE ( 'NONE', #21200, #22768, #53472, .T. ) ;
#95880 = CARTESIAN_POINT ( 'NONE',  ( 15.58852162090000171, 1416.217772597929979, 199.0820666858980132 ) ) ;
#95881 = CARTESIAN_POINT ( 'NONE',  ( -12.78690713350000152, 1416.828040475229955, 195.5394874918979724 ) ) ;
#95882 = CARTESIAN_POINT ( 'NONE',  ( 11.76015609417409991, 1479.338828819800028, 208.6267683045179808 ) ) ;
#95883 = ADVANCED_FACE ( 'NONE', ( #68886 ), #53734, .T. ) ;
#95884 = CARTESIAN_POINT ( 'NONE',  ( 23.75354970140000432, 1410.237980908829968, 210.1586681567179937 ) ) ;
#95885 = CARTESIAN_POINT ( 'NONE',  ( 3.908823033620000498, 1430.579202973829979, 185.0915024236979889 ) ) ;
#95886 = EDGE_CURVE ( 'NONE', #46147, #52400, #47110, .T. ) ;
#95887 = CARTESIAN_POINT ( 'NONE',  ( 18.87014351247420052, 1458.714671120490038, 220.5051382869739882 ) ) ;
#95888 = CARTESIAN_POINT ( 'NONE',  ( -5.359920746595229879, 1422.532334412899900, 146.8567192038190115 ) ) ;
#95890 = LINE ( 'NONE', #95340, #73693 ) ;
#95889 = CARTESIAN_POINT ( 'NONE',  ( -11.77480480780000072, 1432.721983468549979, 150.8108403777980016 ) ) ;
#95891 = CARTESIAN_POINT ( 'NONE',  ( 1.073626246609999724, 1413.031385993829872, 233.0405009011980155 ) ) ;
#95892 = DIRECTION ( 'NONE',  ( -1.755985294532469921E-16, 1.000000000000000000, -1.338183447452831989E-16 ) ) ;
#95893 = CARTESIAN_POINT ( 'NONE',  ( -10.97860730640000071, 1492.014415902390056, 210.2726032398089728 ) ) ;
#95894 = DIRECTION ( 'NONE',  ( 1.000000000000000000, 0.000000000000000000, 0.000000000000000000 ) ) ;
#95895 = CARTESIAN_POINT ( 'NONE',  ( -1.018590187505569844, 1419.107239897679847, 184.9305502371729801 ) ) ;
#95896 = CARTESIAN_POINT ( 'NONE',  ( -5.784638357945000031, 1516.939574742129935, 204.5080835752170003 ) ) ;
#95897 = DIRECTION ( 'NONE',  ( 1.755985294532469921E-16, -1.000000000000000000, 1.338183447452831989E-16 ) ) ;
#95898 = CARTESIAN_POINT ( 'NONE',  ( -14.13418362532219952, 1485.258468063590044, 186.5543704135239977 ) ) ;
#95899 = CARTESIAN_POINT ( 'NONE',  ( 2.370878939379999828, 1508.995853304430057, 237.7496061722980016 ) ) ;
#95900 = CARTESIAN_POINT ( 'NONE',  ( 10.92782285068519954, 1503.815843204259863, 213.0813150825409821 ) ) ;
#95901 = CARTESIAN_POINT ( 'NONE',  ( 40.26396674155190425, 1444.186481489339940, 137.1012378630869932 ) ) ;
#95903 = ORIENTED_EDGE ( 'NONE', *, *, #18621, .F. ) ;
#95902 = CARTESIAN_POINT ( 'NONE',  ( -66.97548518297490716, 1379.744360727889898, 277.9508606322140167 ) ) ;
#95904 = VERTEX_POINT ( 'NONE', #79340 ) ;
#95905 = CARTESIAN_POINT ( 'NONE',  ( 11.93812031068550006, 1433.479819799799998, 149.8964887876289822 ) ) ;
#95906 = CARTESIAN_POINT ( 'NONE',  ( 21.45464262047749671, 1525.320827368861273, 184.8030334685298044 ) ) ;
#95907 = ORIENTED_EDGE ( 'NONE', *, *, #43312, .F. ) ;
#95908 = CARTESIAN_POINT ( 'NONE',  ( -0.05883584365174199943, 1457.642074517544415, 199.5869934370919054 ) ) ;
#95909 = FACE_OUTER_BOUND ( 'NONE', #15564, .T. ) ;
#95911 = CARTESIAN_POINT ( 'NONE',  ( -0.1670782863309999977, 1507.623008746229971, 180.8803229349979915 ) ) ;
#95910 = CARTESIAN_POINT ( 'NONE',  ( 18.23239277690950289, 1497.487356725759810, 188.8422295970860034 ) ) ;
#95912 = CARTESIAN_POINT ( 'NONE',  ( 1.191524307911315805, 1526.382868172863937, 239.2353018730792087 ) ) ;
#95913 = EDGE_CURVE ( 'NONE', #84894, #25549, #11998, .T. ) ;
#95914 = CARTESIAN_POINT ( 'NONE',  ( 0.1008259851559999976, 1507.644663146129915, 180.8662990920980178 ) ) ;
#95915 = CARTESIAN_POINT ( 'NONE',  ( -105.8906218209530010, 1378.913060388219719, 304.9510362749820160 ) ) ;
#95916 = CARTESIAN_POINT ( 'NONE',  ( 16.31714699009999947, 1410.414996249630121, 226.6977280599979849 ) ) ;
#95917 = CARTESIAN_POINT ( 'NONE',  ( -2.477986770365000257, 1516.922519270759949, 212.3907053662870226 ) ) ;
#95918 = EDGE_CURVE ( 'NONE', #14236, #18748, #70971, .T. ) ;
#95919 = CARTESIAN_POINT ( 'NONE',  ( 13.90692152919330127, 1415.348334734199852, 197.4141063975939971 ) ) ;
#95920 = CARTESIAN_POINT ( 'NONE',  ( -4.949448334325509791, 1426.816921726720011, 207.3013729964370100 ) ) ;
#95921 = CARTESIAN_POINT ( 'NONE',  ( -6.918225063430000432, 1481.313522505289939, 206.5729028383990169 ) ) ;
#95922 = ORIENTED_EDGE ( 'NONE', *, *, #9660, .F. ) ;
#95923 = CARTESIAN_POINT ( 'NONE',  ( 14.13836065253160079, 1435.304170572160047, 149.4741414661730232 ) ) ;
#95924 = CARTESIAN_POINT ( 'NONE',  ( -17.21523805317120193, 1442.518106596560074, 216.7674110779969965 ) ) ;
#95925 = ORIENTED_EDGE ( 'NONE', *, *, #90442, .T. ) ;
#95926 = ORIENTED_EDGE ( 'NONE', *, *, #69911, .F. ) ;
#95927 = EDGE_CURVE ( 'NONE', #54399, #54705, #93482, .T. ) ;
#95928 = ORIENTED_EDGE ( 'NONE', *, *, #36788, .F. ) ;
#95929 = CARTESIAN_POINT ( 'NONE',  ( -7.396545081264999766, 1511.069621805459974, 215.4940135707870184 ) ) ;
#95930 = CARTESIAN_POINT ( 'NONE',  ( -0.3157389373359999474, 1466.373614209230027, 235.6705073726980117 ) ) ;
#95931 = CARTESIAN_POINT ( 'NONE',  ( 7.943111102253434197, 1451.391306100884776, 152.9620345468942162 ) ) ;
#95932 = CARTESIAN_POINT ( 'NONE',  ( -8.581228205849999568, 1384.934619283940037, 218.6696012310689810 ) ) ;
#95933 = CARTESIAN_POINT ( 'NONE',  ( 10.12978361029999874, 1461.480643167490143, 208.6898772595120306 ) ) ;
#95934 = EDGE_CURVE ( 'NONE', #31591, #68013, #65647, .T. ) ;
#95935 = DIRECTION ( 'NONE',  ( -0.000000000000000000, -1.000000000000000000, -0.000000000000000000 ) ) ;
#95936 = CARTESIAN_POINT ( 'NONE',  ( -18.40088546307429951, 1508.551704408389924, 210.4144978082819648 ) ) ;
#95937 = CARTESIAN_POINT ( 'NONE',  ( -38.67752440520889934, 1379.650603488850038, 221.7945647579082333 ) ) ;
#95938 = CARTESIAN_POINT ( 'NONE',  ( 2.745476835439999874, 1465.706481184990025, 199.2183696094690220 ) ) ;
#95939 = CARTESIAN_POINT ( 'NONE',  ( 0.7447930487909999453, 1508.354245354229988, 237.7262685846980048 ) ) ;
#95940 = ORIENTED_EDGE ( 'NONE', *, *, #57775, .T. ) ;
#95941 = CARTESIAN_POINT ( 'NONE',  ( -6.951175166914999259, 1517.170721208160103, 206.8315896683770063 ) ) ;
#95942 = EDGE_LOOP ( 'NONE', ( #84576, #51947, #64389, #104618 ) ) ;
#95943 = CARTESIAN_POINT ( 'NONE',  ( 24.41278939130150150, 1440.913060387330006, 237.1198172069220220 ) ) ;
#95944 = CARTESIAN_POINT ( 'NONE',  ( 11.47796531776959839, 1478.826507664550036, 206.6271712911859879 ) ) ;
#95945 = ORIENTED_EDGE ( 'NONE', *, *, #6296, .T. ) ;
#95946 = CARTESIAN_POINT ( 'NONE',  ( -6.120078482172389478, 1508.729259781710198, 201.6787668352259857 ) ) ;
#95947 = CARTESIAN_POINT ( 'NONE',  ( -14.70848724120000028, 1409.928546724029957, 190.8190897573979896 ) ) ;
#95948 = CARTESIAN_POINT ( 'NONE',  ( -54.27566527714611766, 1379.707491775901872, 254.2935361429743466 ) ) ;
#95949 = CARTESIAN_POINT ( 'NONE',  ( -24.23995371788353026, 1438.560025134897842, 212.1200462699911213 ) ) ;
#95950 = CARTESIAN_POINT ( 'NONE',  ( -1.127400696442319994, 1422.674730469140059, 192.5292151802170224 ) ) ;
#95951 = CARTESIAN_POINT ( 'NONE',  ( 0.0003311604216102360292, 1396.810862911885124, 196.4330027040883238 ) ) ;
#95952 = CARTESIAN_POINT ( 'NONE',  ( -12.59821692533909498, 1434.524816250457661, 147.2310560251989671 ) ) ;
#95953 = CARTESIAN_POINT ( 'NONE',  ( -9.803834995107230554, 1517.051704408389924, 196.6215198571080123 ) ) ;
#95954 = CARTESIAN_POINT ( 'NONE',  ( -5.482980402289999944, 1508.348588800990001, 220.2461224233989867 ) ) ;
#95956 = CARTESIAN_POINT ( 'NONE',  ( -3.061699073614430500, 1369.389631199361702, 207.6218459616989662 ) ) ;
#95955 = CARTESIAN_POINT ( 'NONE',  ( -0.4537870827523895478, 1465.110980022260946, 238.1114895919644994 ) ) ;
#95957 = CARTESIAN_POINT ( 'NONE',  ( -2.482067898354999969, 1517.099836525840146, 214.9099431973869798 ) ) ;
#95958 = CARTESIAN_POINT ( 'NONE',  ( 3.897009772517886717, 1517.051704408389924, 231.0205787110200788 ) ) ;
#95959 = AXIS2_PLACEMENT_3D ( 'NONE', #40943, #15171, #90794 ) ;
#95960 = CARTESIAN_POINT ( 'NONE',  ( 5.570674229300860425, 1511.275365984429982, 217.0209262882389964 ) ) ;
#95961 = CARTESIAN_POINT ( 'NONE',  ( -17.11714618750000128, 1443.086052842849995, 162.7561046190980107 ) ) ;
#95962 = CARTESIAN_POINT ( 'NONE',  ( -4.609673279564999504, 1516.754149861460064, 212.3872530880769887 ) ) ;
#95963 = CARTESIAN_POINT ( 'NONE',  ( -21.20812184460000083, 1488.814055421829835, 209.5007742268749951 ) ) ;
#95964 = CARTESIAN_POINT ( 'NONE',  ( -17.82472165217326321, 1486.162070320810017, 188.3324638760118717 ) ) ;
#95966 = ORIENTED_EDGE ( 'NONE', *, *, #81590, .T. ) ;
#95965 = CARTESIAN_POINT ( 'NONE',  ( -86.94526474789999781, 1386.534739258749823, 307.6971543075589466 ) ) ;
#95967 = CARTESIAN_POINT ( 'NONE',  ( -18.53418666356940037, 1507.620785846770104, 229.7143111648900060 ) ) ;
#95968 = CARTESIAN_POINT ( 'NONE',  ( 27.39151915920000135, 1446.363612851640255, 231.9651322872979904 ) ) ;
#95969 = DIRECTION ( 'NONE',  ( -1.755985294532469921E-16, 1.000000000000000000, -1.338183447452831989E-16 ) ) ;
#95970 = CARTESIAN_POINT ( 'NONE',  ( -7.599227184291730275, 1512.341036968809931, 211.3567690145959830 ) ) ;
#95971 = CARTESIAN_POINT ( 'NONE',  ( -7.824074142530000664, 1507.599096865930051, 235.3676831994980034 ) ) ;
#95972 = CARTESIAN_POINT ( 'NONE',  ( -18.93166004669999936, 1457.983850899830031, 226.9910905844980107 ) ) ;
#95973 = EDGE_CURVE ( 'NONE', #25318, #27899, #80237, .T. ) ;
#95975 = CARTESIAN_POINT ( 'NONE',  ( 19.01929472089999962, 1456.664510428530093, 226.1307736208979975 ) ) ;
#95974 = CARTESIAN_POINT ( 'NONE',  ( -20.37974553509161524, 1410.985820951756523, 198.9094803766706718 ) ) ;
#95976 = CARTESIAN_POINT ( 'NONE',  ( -0.08692450656670000497, 1452.817890303729882, 189.4446534707980163 ) ) ;
#95977 = CARTESIAN_POINT ( 'NONE',  ( -104.5971662677009988, 1379.798410771470117, 305.4970342620409838 ) ) ;
#95978 = VERTEX_POINT ( 'NONE', #41734 ) ;
#95979 = CARTESIAN_POINT ( 'NONE',  ( -1.132949114555000136, 1516.693851263360102, 204.1241276937270186 ) ) ;
#95980 = CARTESIAN_POINT ( 'NONE',  ( 0.1080863654920000139, 1405.716796065530161, 267.8540375961979407 ) ) ;
#95981 = CARTESIAN_POINT ( 'NONE',  ( 4.545982227442832979, 1508.783371655767723, 211.6097810847320204 ) ) ;
#95982 = CARTESIAN_POINT ( 'NONE',  ( 42.60984463329660343, 1451.659711123250190, 270.2297449080399474 ) ) ;
#95983 = CARTESIAN_POINT ( 'NONE',  ( 5.426920751279999955, 1436.492768174659886, 154.6973185947979914 ) ) ;
#95984 = CARTESIAN_POINT ( 'NONE',  ( -40.35744760560000088, 1444.177753733350073, 137.0994330816980096 ) ) ;
#95985 = CARTESIAN_POINT ( 'NONE',  ( -40.15144253337770408, 1440.913060403469899, 259.4983307252720124 ) ) ;
#95986 = EDGE_CURVE ( 'NONE', #104164, #92476, #77448, .T. ) ;
#95987 = CARTESIAN_POINT ( 'NONE',  ( -27.43419230599999992, 1448.208631761229981, 136.8608613106979988 ) ) ;
#95988 = CARTESIAN_POINT ( 'NONE',  ( 1.536514403073885315, 1450.607110032781748, 154.2727822066727299 ) ) ;
#95989 = CARTESIAN_POINT ( 'NONE',  ( -0.5525097125479990767, 1430.369002146489947, 200.0800212161890101 ) ) ;
#95990 = CARTESIAN_POINT ( 'NONE',  ( -1.271867600325184311, 1450.975052772127356, 183.1634528063702305 ) ) ;
#95991 = CARTESIAN_POINT ( 'NONE',  ( 25.31189446751989891, 1438.152406002519911, 138.1036420975650003 ) ) ;
#95992 = FACE_OUTER_BOUND ( 'NONE', #800, .T. ) ;
#95993 = ORIENTED_EDGE ( 'NONE', *, *, #7519, .T. ) ;
#95994 = CARTESIAN_POINT ( 'NONE',  ( -38.34143788450000301, 1440.913060387330006, 265.6112250856980381 ) ) ;
#95995 = CARTESIAN_POINT ( 'NONE',  ( -1.545976657695036005, 1450.600942636307991, 182.1937731406511034 ) ) ;
#95996 = CARTESIAN_POINT ( 'NONE',  ( 3.168149218889090069, 1465.479944987909903, 199.6312225713100190 ) ) ;
#95997 = CARTESIAN_POINT ( 'NONE',  ( -0.7781779465670000118, 1476.071789383429859, 267.5369107683980019 ) ) ;
#95998 = CARTESIAN_POINT ( 'NONE',  ( 7.271691885010000078, 1501.094707673489893, 204.7367163811290141 ) ) ;
#95999 = CARTESIAN_POINT ( 'NONE',  ( -29.78220350812357964, 1524.382868172863937, 196.5089261231635476 ) ) ;
#96000 = CARTESIAN_POINT ( 'NONE',  ( -3.885048638823741740, 1448.296104563261451, 185.0431407441832334 ) ) ;
#96001 = CARTESIAN_POINT ( 'NONE',  ( -20.42440048154189824, 1384.860985728550077, 221.1297803709319965 ) ) ;
#96002 = VECTOR ( 'NONE', #90324, 1000.000000000000114 ) ;
#96003 = CARTESIAN_POINT ( 'NONE',  ( -18.01569507700000017, 1415.245980409429876, 207.9371297658080096 ) ) ;
#96004 = CARTESIAN_POINT ( 'NONE',  ( 15.58948595390000058, 1452.698291846990060, 196.7507890572990163 ) ) ;
#96005 = CARTESIAN_POINT ( 'NONE',  ( 26.08096834208760129, 1435.935456896660071, 136.5582649592650171 ) ) ;
#96006 = ADVANCED_FACE ( 'NONE', ( #85374 ), #96627, .F. ) ;
#96007 = CARTESIAN_POINT ( 'NONE',  ( -13.35899836846294875, 1443.328976958492376, 169.3723828192563587 ) ) ;
#96008 = CARTESIAN_POINT ( 'NONE',  ( -16.16218761038539853, 1409.477383793439913, 225.2079466252519921 ) ) ;
#96009 = EDGE_CURVE ( 'NONE', #68646, #55731, #94901, .T. ) ;
#96010 = CARTESIAN_POINT ( 'NONE',  ( -18.97541190666909827, 1485.183224067069887, 218.3497724515069933 ) ) ;
#96011 = ORIENTED_EDGE ( 'NONE', *, *, #65850, .F. ) ;
#96012 = CARTESIAN_POINT ( 'NONE',  ( -6.569077902550000125, 1472.000453826989997, 211.3893757803390088 ) ) ;
#96013 = CARTESIAN_POINT ( 'NONE',  ( 2.883409987159999854, 1409.181735908430028, 231.0710517162980011 ) ) ;
#96014 = CARTESIAN_POINT ( 'NONE',  ( 22.03465957474552184, 1512.187213306747481, 182.8300405912328301 ) ) ;
#96016 = CARTESIAN_POINT ( 'NONE',  ( -9.898687722262419442, 1438.737011691519911, 210.1098268883750109 ) ) ;
#96015 = CARTESIAN_POINT ( 'NONE',  ( 26.57484134623869920, 1440.913038224569846, 213.0553080370949885 ) ) ;
#96017 = CARTESIAN_POINT ( 'NONE',  ( -0.1613635714646410035, 1507.107001889669846, 180.9028745560509890 ) ) ;
#96018 = CARTESIAN_POINT ( 'NONE',  ( 4.198017029517449927, 1424.053073258670111, 184.2502146191590100 ) ) ;
#96019 = ADVANCED_FACE ( 'NONE', ( #104402 ), #7836, .T. ) ;
#96020 = CARTESIAN_POINT ( 'NONE',  ( 5.004475574535000248, 1517.026025493960105, 201.3999380438669959 ) ) ;
#96021 = CARTESIAN_POINT ( 'NONE',  ( 7.880635186530000169, 1425.932163105479958, 211.6468907411690168 ) ) ;
#96023 = CARTESIAN_POINT ( 'NONE',  ( 0.5708672984259970384, 1460.784242392889837, 230.4191149236990270 ) ) ;
#96022 = CIRCLE ( 'NONE', #1329, 6.868727599660006788 ) ;
#96024 = FACE_OUTER_BOUND ( 'NONE', #91514, .T. ) ;
#96025 = CARTESIAN_POINT ( 'NONE',  ( 7.691516654014999510, 1512.326491219019999, 206.4237331406770011 ) ) ;
#96026 = CARTESIAN_POINT ( 'NONE',  ( 2.476654626830000261, 1449.226390938449867, 182.5716736920980168 ) ) ;
#96027 = CARTESIAN_POINT ( 'NONE',  ( 8.003402032965700741, 1365.192785687681635, 208.3718459617061285 ) ) ;
#96028 = EDGE_CURVE ( 'NONE', #22743, #59443, #19269, .T. ) ;
#96030 = VERTEX_POINT ( 'NONE', #98748 ) ;
#96029 = CARTESIAN_POINT ( 'NONE',  ( 5.853197488659999337, 1455.236944383789933, 217.5027156205790106 ) ) ;
#96031 = ORIENTED_EDGE ( 'NONE', *, *, #43271, .F. ) ;
#96032 = CARTESIAN_POINT ( 'NONE',  ( -10.10023367162169983, 1522.051704408389924, 185.1638560673330005 ) ) ;
#96033 = CARTESIAN_POINT ( 'NONE',  ( 1.448807010176029975, 1499.064327800129831, 236.4215994981330198 ) ) ;
#96034 = CARTESIAN_POINT ( 'NONE',  ( -1.566309006410000032E-09, 1473.264972808529819, 270.4290818598980195 ) ) ;
#96035 = CARTESIAN_POINT ( 'NONE',  ( -7.559673342214999536, 1510.830536680500245, 212.2954481221070182 ) ) ;
#96036 = CARTESIAN_POINT ( 'NONE',  ( -108.6418955636174672, 1309.112692017088193, 312.2430413686188331 ) ) ;
#96037 = CARTESIAN_POINT ( 'NONE',  ( 24.02863916850529691, 1507.902931906480035, 195.9323055859989893 ) ) ;
#96038 = CARTESIAN_POINT ( 'NONE',  ( -2.711955045610519921, 1463.961042537189996, 199.5488283424340068 ) ) ;
#96039 = CARTESIAN_POINT ( 'NONE',  ( 22.76038310810000098, 1410.633847097429907, 206.9447164962780334 ) ) ;
#96040 = DIRECTION ( 'NONE',  ( 1.000000000000000000, 0.000000000000000000, 0.000000000000000000 ) ) ;
#96041 = CARTESIAN_POINT ( 'NONE',  ( 33.91368447396819619, 1437.010588082029926, 136.5611905281099894 ) ) ;
#96042 = CARTESIAN_POINT ( 'NONE',  ( 27.58305910952065432, 1435.460669043382723, 135.2629866813300623 ) ) ;
#96043 = CARTESIAN_POINT ( 'NONE',  ( 3.137687880864949985, 1407.958752388860148, 195.9309462285740153 ) ) ;
#96044 = CARTESIAN_POINT ( 'NONE',  ( -0.7722441410959061114, 1405.989132518979886, 266.9610481760290099 ) ) ;
#96045 = CARTESIAN_POINT ( 'NONE',  ( 41.66021864449999867, 1443.875655612860101, 135.6929158170979974 ) ) ;
#96046 = ORIENTED_EDGE ( 'NONE', *, *, #32935, .F. ) ;
#96047 = DIRECTION ( 'NONE',  ( 0.000000000000000000, 1.000000000000000000, 0.000000000000000000 ) ) ;
#96048 = CARTESIAN_POINT ( 'NONE',  ( 13.74650104269999851, 1441.983649238280123, 189.3366583681979876 ) ) ;
#96049 = B_SPLINE_CURVE_WITH_KNOTS ( 'NONE', 3,
 ( #18444, #52643, #104684, #19566, #36925, #21749 ),
 .UNSPECIFIED., .F., .F.,
 ( 4, 2, 4 ),
 ( 0.002076474971749801314, 0.005958898312071419720, 0.009841321652393038993 ),
 .UNSPECIFIED. ) ;
#96050 = ORIENTED_EDGE ( 'NONE', *, *, #102051, .F. ) ;
#96051 = EDGE_CURVE ( 'NONE', #12135, #104137, #21277, .T. ) ;
#96052 = VERTEX_POINT ( 'NONE', #81941 ) ;
#96053 = DIRECTION ( 'NONE',  ( 0.000000000000000000, 1.000000000000000000, 0.000000000000000000 ) ) ;
#96054 = CARTESIAN_POINT ( 'NONE',  ( 9.663424421700000266, 1363.752474719049815, 207.6218459616989946 ) ) ;
#96055 = AXIS2_PLACEMENT_3D ( 'NONE', #23365, #57555, #83828 ) ;
#96056 = EDGE_CURVE ( 'NONE', #13254, #89963, #38766, .T. ) ;
#96057 = CARTESIAN_POINT ( 'NONE',  ( 6.945490048805000427, 1516.932669162149978, 214.9002185338470099 ) ) ;
#96058 = CARTESIAN_POINT ( 'NONE',  ( 3.558864023334999960, 1511.483345606789953, 217.0119653402770155 ) ) ;
#96059 = ORIENTED_EDGE ( 'NONE', *, *, #3506, .T. ) ;
#96060 = CARTESIAN_POINT ( 'NONE',  ( 8.377020731070000892, 1427.910351821989934, 212.6460221678989910 ) ) ;
#96061 = CARTESIAN_POINT ( 'NONE',  ( -78.35932141380000360, 1374.964007173050049, 291.3894706323590071 ) ) ;
#96062 = CARTESIAN_POINT ( 'NONE',  ( 9.507369708760000648, 1414.971339025629959, 223.5168404978979879 ) ) ;
#96063 = CARTESIAN_POINT ( 'NONE',  ( -6.557909920764999789, 1516.908489800550115, 203.3441005368270282 ) ) ;
#96064 = CARTESIAN_POINT ( 'NONE',  ( 10.51054176719999944, 1491.593345921790160, 212.4262175969289785 ) ) ;
#96065 = DIRECTION ( 'NONE',  ( 8.673617379884002932E-16, 0.02617694830786544691, -0.9996573249755575929 ) ) ;
#96066 = CARTESIAN_POINT ( 'NONE',  ( 3.801734845580006183, 1509.034509900239755, 204.6344869756675848 ) ) ;
#96067 = CARTESIAN_POINT ( 'NONE',  ( -4.474334996270000531, 1410.445275992929965, 232.0547894430980023 ) ) ;
#96069 = VERTEX_POINT ( 'NONE', #4694 ) ;
#96068 = CARTESIAN_POINT ( 'NONE',  ( -5.689439854299999766, 1447.123656070790048, 185.2293832585979771 ) ) ;
#96070 = CARTESIAN_POINT ( 'NONE',  ( 11.86716023049999968, 1432.353341358199941, 147.6509521729980179 ) ) ;
#96071 = CARTESIAN_POINT ( 'NONE',  ( -25.49263425876450029, 1440.913060497309971, 219.0479588355970009 ) ) ;
#96072 = CARTESIAN_POINT ( 'NONE',  ( -2.793439186891359949, 1486.025328193850100, 182.0741020391329812 ) ) ;
#96073 = CARTESIAN_POINT ( 'NONE',  ( 15.62937150409696940, 1506.527232284255660, 224.6916783686666008 ) ) ;
#96074 = CARTESIAN_POINT ( 'NONE',  ( -25.57374439069999994, 1436.479224125469955, 137.1536659212979998 ) ) ;
#96075 = CARTESIAN_POINT ( 'NONE',  ( 6.562635822504999439, 1517.111322026010157, 211.9927976380170094 ) ) ;
#96076 = CARTESIAN_POINT ( 'NONE',  ( -67.33401983280000991, 1379.744965387350021, 277.0816680017589988 ) ) ;
#96077 = CIRCLE ( 'NONE', #103173, 0.5000000000000147660 ) ;
#96078 = CARTESIAN_POINT ( 'NONE',  ( -12.98226561589999939, 1414.913060387329779, 219.9156672276980089 ) ) ;
#96079 = CARTESIAN_POINT ( 'NONE',  ( 19.23929248577682927, 1410.946498287256873, 195.7385929941525546 ) ) ;
#96080 = CARTESIAN_POINT ( 'NONE',  ( -6.944466780504999548, 1516.939530130779985, 209.1331108864249870 ) ) ;
#96081 = ORIENTED_EDGE ( 'NONE', *, *, #74749, .F. ) ;
#96082 = CARTESIAN_POINT ( 'NONE',  ( 0.000000000000000000, 1508.551704408389924, 209.1218459616989946 ) ) ;
#96083 = CARTESIAN_POINT ( 'NONE',  ( -4.407453029090000030, 1410.299935115230028, 232.0713108462980188 ) ) ;
#96084 = CARTESIAN_POINT ( 'NONE',  ( -62.06522312460000279, 1384.809685994470101, 284.7693067110590164 ) ) ;
#96085 = VERTEX_POINT ( 'NONE', #5810 ) ;
#96086 = CARTESIAN_POINT ( 'NONE',  ( -10.61669498371649922, 1508.551704408389924, 207.6874897006059939 ) ) ;
#96087 = CARTESIAN_POINT ( 'NONE',  ( -2.942964642939999820, 1430.286447874990245, 201.3134892009489931 ) ) ;
#96088 = CARTESIAN_POINT ( 'NONE',  ( 17.40247493689940228, 1469.008714942930055, 228.9206246928509927 ) ) ;
#96089 = CARTESIAN_POINT ( 'NONE',  ( 20.12564951288285542, 1512.187213306747481, 237.5287294252014192 ) ) ;
#96090 = CARTESIAN_POINT ( 'NONE',  ( 3.415183242699999955, 1486.712733892290089, 198.4695611698990092 ) ) ;
#96091 = CARTESIAN_POINT ( 'NONE',  ( 11.20716745179999840, 1422.288374914430278, 203.3912787612890156 ) ) ;
#96092 = CARTESIAN_POINT ( 'NONE',  ( -13.95592190008845179, 1416.839570625314309, 221.9092780320571023 ) ) ;
#96093 = EDGE_CURVE ( 'NONE', #20112, #58764, #48369, .T. ) ;
#96095 = CARTESIAN_POINT ( 'NONE',  ( -3.189739596009999456, 1421.552253087029840, 184.9104270198979805 ) ) ;
#96094 = CARTESIAN_POINT ( 'NONE',  ( 0.7543881828220019292, 1516.727502608469877, 215.6727161143369926 ) ) ;
#96096 = CARTESIAN_POINT ( 'NONE',  ( -5.932239102140000497, 1391.913060387289988, 215.1144410137189880 ) ) ;
#96097 = CARTESIAN_POINT ( 'NONE',  ( -11.03930834155172747, 1425.182627338753264, 139.1363278504886125 ) ) ;
#96098 = CIRCLE ( 'NONE', #108646, 33.13701971169416538 ) ;
#96099 = ORIENTED_EDGE ( 'NONE', *, *, #102990, .T. ) ;
#96100 = CARTESIAN_POINT ( 'NONE',  ( 5.161034791280000533, 1485.814572579490005, 218.5690567784690188 ) ) ;
#96101 = CARTESIAN_POINT ( 'NONE',  ( 8.214063898797519414, 1423.929538348540291, 211.6355982495960006 ) ) ;
#96102 = CARTESIAN_POINT ( 'NONE',  ( -16.55737386589999716, 1499.713794654230014, 185.8142580502980081 ) ) ;
#96103 = VERTEX_POINT ( 'NONE', #56205 ) ;
#96104 = CARTESIAN_POINT ( 'NONE',  ( 3.104086163079999849, 1421.303663037730075, 184.6144243675980192 ) ) ;
#96105 = CARTESIAN_POINT ( 'NONE',  ( 10.46157297396847952, 1435.041345384508304, 152.1695804010182655 ) ) ;
#96106 = CARTESIAN_POINT ( 'NONE',  ( 7.546131039266060547, 1510.764648358900104, 203.2669580094189996 ) ) ;
#96107 = PRODUCT_DEFINITION_CONTEXT ( 'detailed design', #34140, 'design' ) ;
#96108 = CARTESIAN_POINT ( 'NONE',  ( -109.1309839890330124, 1384.924126711810004, 311.2646841801559958 ) ) ;
#96109 = DIRECTION ( 'NONE',  ( -1.755985294532469921E-16, 1.000000000000000000, -1.338183447452831989E-16 ) ) ;
#96110 = CARTESIAN_POINT ( 'NONE',  ( 295.4396770967078965, -8387.357407334289746, 2232.807573057129957 ) ) ;
#96111 = EDGE_CURVE ( 'NONE', #75452, #14195, #78849, .T. ) ;
#96112 = CARTESIAN_POINT ( 'NONE',  ( 17.74184486700000107, 1415.163755984130148, 210.1742778932080000 ) ) ;
#96113 = CARTESIAN_POINT ( 'NONE',  ( -18.65358896220000062, 1425.523870256030023, 225.5826184276980086 ) ) ;
#96114 = CARTESIAN_POINT ( 'NONE',  ( -14.51975326280000012, 1434.998496940630048, 148.5999626668979943 ) ) ;
#96115 = CARTESIAN_POINT ( 'NONE',  ( -4.391428885256890347, 1464.583814225909919, 199.0196702316530093 ) ) ;
#96116 = CARTESIAN_POINT ( 'NONE',  ( -1.725662463192670248, 1484.236887848700007, 182.7463278875050037 ) ) ;
#96118 = CARTESIAN_POINT ( 'NONE',  ( -5.093685840561368749, 1391.856767254725355, 203.6189120034268853 ) ) ;
#96117 = CARTESIAN_POINT ( 'NONE',  ( 1.159637561179999832, 1415.063410489729904, 191.5788536471979739 ) ) ;
#96119 = CARTESIAN_POINT ( 'NONE',  ( 10.88722667122907239, 1426.866889159644870, 149.3503661776646538 ) ) ;
#96120 = VERTEX_POINT ( 'NONE', #46727 ) ;
#96121 = CARTESIAN_POINT ( 'NONE',  ( 15.27152964737910068, 1506.433683733550197, 193.3098315259690025 ) ) ;
#96122 = CARTESIAN_POINT ( 'NONE',  ( 22.92154238690000057, 1411.040135702729913, 207.1380470637979840 ) ) ;
#96123 = AXIS2_PLACEMENT_3D ( 'NONE', #89381, #12673, #21601 ) ;
#96124 = CARTESIAN_POINT ( 'NONE',  ( -11.90000415720300175, 1434.913060496859998, 147.6452464505769910 ) ) ;
#96125 = CARTESIAN_POINT ( 'NONE',  ( -4.542064733420000167, 1483.636937311689962, 199.4558309895289767 ) ) ;
#96126 = DIRECTION ( 'NONE',  ( -0.6736849260863841948, 0.000000000000000000, 0.7390186874254148774 ) ) ;
#96127 = CARTESIAN_POINT ( 'NONE',  ( -2.340429037510286747, 1525.425665131969026, 241.8895524149548919 ) ) ;
#96128 = CARTESIAN_POINT ( 'NONE',  ( 14.69722372230000040, 1408.913060387329779, 219.1592431274980299 ) ) ;
#96129 = CARTESIAN_POINT ( 'NONE',  ( 19.02704169900689735, 1456.915441405320053, 225.6706379604710264 ) ) ;
#96130 = CARTESIAN_POINT ( 'NONE',  ( -11.39064650766950137, 1470.655863615889984, 209.6027845347450125 ) ) ;
#96131 = CARTESIAN_POINT ( 'NONE',  ( -4.592827604961299492, 1488.079576444790064, 219.1748425648949876 ) ) ;
#96132 = CARTESIAN_POINT ( 'NONE',  ( 18.99431323780000014, 1459.501207708489801, 220.3864241394989847 ) ) ;
#96133 = CARTESIAN_POINT ( 'NONE',  ( -92.50840546082399385, 1383.768738235890169, 309.2665542712870206 ) ) ;
#96134 = CARTESIAN_POINT ( 'NONE',  ( -109.5946542274029980, 1383.641284564509988, 311.2236547677540557 ) ) ;
#96135 = CARTESIAN_POINT ( 'NONE',  ( -5.108150090387360009, 1391.866415515492235, 214.6117004621733599 ) ) ;
#96136 = CARTESIAN_POINT ( 'NONE',  ( -1.677883752140799878, 1516.549122391340006, 201.4124261911130134 ) ) ;
#96138 = EDGE_LOOP ( 'NONE', ( #106716, #8575, #99886, #62429 ) ) ;
#96137 = CARTESIAN_POINT ( 'NONE',  ( 24.57377048660000085, 1509.773436695229975, 192.8657111338980030 ) ) ;
#96139 = CARTESIAN_POINT ( 'NONE',  ( -18.35253423818827301, 1459.074742763881659, 227.7717061293672316 ) ) ;
#96140 = CARTESIAN_POINT ( 'NONE',  ( -91.82171654609999223, 1380.714193802210048, 296.3822057022590002 ) ) ;
#96141 = EDGE_CURVE ( 'NONE', #93417, #52697, #86754, .T. ) ;
#96142 = CARTESIAN_POINT ( 'NONE',  ( -14.93718008229999938, 1416.181292664740113, 212.9156384192889959 ) ) ;
#96143 = ORIENTED_EDGE ( 'NONE', *, *, #2736, .F. ) ;
#96144 = ORIENTED_EDGE ( 'NONE', *, *, #50627, .T. ) ;
#96145 = CARTESIAN_POINT ( 'NONE',  ( 18.23773974694429967, 1416.535698381769862, 209.2906403974349985 ) ) ;
#96146 = CARTESIAN_POINT ( 'NONE',  ( 29.33475263078180006, 1526.373507135059754, 201.1007689730743380 ) ) ;
#96147 = CARTESIAN_POINT ( 'NONE',  ( 13.20333953265802585, 1443.120703127549177, 169.3908102670497442 ) ) ;
#96149 = CARTESIAN_POINT ( 'NONE',  ( -21.01922260210000104, 1472.811049260129948, 267.0603657249980074 ) ) ;
#96148 = CARTESIAN_POINT ( 'NONE',  ( 21.21614429629999776, 1488.813684182329780, 208.8886841255019817 ) ) ;
#96150 = EDGE_CURVE ( 'NONE', #110163, #103208, #106702, .T. ) ;
#96151 = CARTESIAN_POINT ( 'NONE',  ( 8.610988768402860316, 1436.778401557170127, 208.5600591984729988 ) ) ;
#96152 = AXIS2_PLACEMENT_3D ( 'NONE', #70148, #20782, #70700 ) ;
#96153 = CARTESIAN_POINT ( 'NONE',  ( -11.72697064220000129, 1433.670490598739889, 150.9444907361979915 ) ) ;
#96154 = EDGE_CURVE ( 'NONE', #21147, #55064, #17307, .T. ) ;
#96155 = CARTESIAN_POINT ( 'NONE',  ( 0.9431357159449988981, 1487.666359187690205, 217.1994056721289894 ) ) ;
#96156 = CARTESIAN_POINT ( 'NONE',  ( -19.92213080605079867, 1499.851339543129825, 228.6477981121460061 ) ) ;
#96157 = CARTESIAN_POINT ( 'NONE',  ( 8.147242326480000685, 1409.364186213629864, 188.2664186143980203 ) ) ;
#96158 = CARTESIAN_POINT ( 'NONE',  ( 4.123035104040000398, 1421.670591005329925, 184.9173806230979835 ) ) ;
#96159 = CARTESIAN_POINT ( 'NONE',  ( -10.43358988419999989, 1436.699218663759893, 152.2773048742980109 ) ) ;
#96160 = CARTESIAN_POINT ( 'NONE',  ( 9.012266058079999809, 1437.710537269130100, 153.1651548905980178 ) ) ;
#96161 = CARTESIAN_POINT ( 'NONE',  ( -14.41439834266500064, 1421.637802249239940, 203.6166032916469817 ) ) ;
#96162 = AXIS2_PLACEMENT_3D ( 'NONE', #53105, #87243, #20561 ) ;
#96163 = EDGE_CURVE ( 'NONE', #5297, #9014, #73499, .T. ) ;
#96164 = CARTESIAN_POINT ( 'NONE',  ( 3.263276722441742717, 1524.760046179776054, 241.7717505690895052 ) ) ;
#96165 = DIRECTION ( 'NONE',  ( 0.1070030146457217196, 0.000000000000000000, -0.9942586961433766968 ) ) ;
#96166 = VERTEX_POINT ( 'NONE', #106600 ) ;
#96167 = DIRECTION ( 'NONE',  ( -1.755985294532469921E-16, 1.000000000000000000, -1.338183447452831989E-16 ) ) ;
#96168 = COLOUR_RGB ( '', 0.66274510, 0.83137255, 0.94901961) ;
#96169 = CARTESIAN_POINT ( 'NONE',  ( -17.89922477309999849, 1489.399004187290075, 195.2216578317990070 ) ) ;
#96170 = CARTESIAN_POINT ( 'NONE',  ( -41.12099125829999480, 1454.819569115930108, 269.7572481037980197 ) ) ;
#96171 = DIRECTION ( 'NONE',  ( -0.9455185755993177343, 0.000000000000000000, 0.3255681544571540909 ) ) ;
#96172 =( BOUNDED_CURVE ( )  B_SPLINE_CURVE ( 3, ( #38059, #3379, #13938, #63293 ),
 .UNSPECIFIED., .F., .F. ) 
 B_SPLINE_CURVE_WITH_KNOTS ( ( 4, 4 ),
 ( 4.168090934964655325, 5.256687371692810196 ),
 .UNSPECIFIED. ) 
 CURVE ( )  GEOMETRIC_REPRESENTATION_ITEM ( )  RATIONAL_B_SPLINE_CURVE ( ( 1.000000000000000000, 0.9036605976482073865, 0.9036605976482073865, 1.000000000000000000 ) ) 
 REPRESENTATION_ITEM ( '' )  );
#96173 = CARTESIAN_POINT ( 'NONE',  ( 17.64684481400000138, 1410.891992924130136, 223.6671000665980102 ) ) ;
#96174 = CYLINDRICAL_SURFACE ( 'NONE', #84066, 1.999999999999995337 ) ;
#96175 = CARTESIAN_POINT ( 'NONE',  ( 4.329271545279290478, 1515.071561052290008, 210.6721986880200177 ) ) ;
#96176 = CARTESIAN_POINT ( 'NONE',  ( 2.912741334778549795, 1409.643588917339912, 231.3796457533279920 ) ) ;
#96177 = CARTESIAN_POINT ( 'NONE',  ( 1.456020689590000083, 1508.396344578629851, 237.4407949434980196 ) ) ;
#96178 = CARTESIAN_POINT ( 'NONE',  ( -8.272300520779998223, 1417.569710766430035, 230.8453573205979978 ) ) ;
#96179 = CARTESIAN_POINT ( 'NONE',  ( -1.082042371095176314, 1484.833744122492590, 182.1605000476520786 ) ) ;
#96180 = CARTESIAN_POINT ( 'NONE',  ( 11.20850749315819428, 1362.682805967720014, 208.3718459617010978 ) ) ;
#96181 = CARTESIAN_POINT ( 'NONE',  ( -43.62459105522109581, 1430.012141993600153, 266.4825913953999930 ) ) ;
#96182 = DIRECTION ( 'NONE',  ( -0.6736849260863839728, 0.000000000000000000, 0.7390186874254150995 ) ) ;
#96183 = ORIENTED_EDGE ( 'NONE', *, *, #34944, .T. ) ;
#96184 = CARTESIAN_POINT ( 'NONE',  ( -9.205204419190000209, 1422.968094939250022, 210.4274292779389839 ) ) ;
#96185 = ORIENTED_EDGE ( 'NONE', *, *, #93976, .T. ) ;
#96186 = CARTESIAN_POINT ( 'NONE',  ( -5.000330033664999618, 1516.770163853809890, 209.8779366980180328 ) ) ;
#96187 = CARTESIAN_POINT ( 'NONE',  ( -9.754833734307490900, 1446.835976941670197, 212.2157276707299900 ) ) ;
#96188 = CIRCLE ( 'NONE', #64076, 1.999999999999999556 ) ;
#96189 = EDGE_CURVE ( 'NONE', #24269, #89941, #40527, .T. ) ;
#96190 = CARTESIAN_POINT ( 'NONE',  ( 13.15366522099999891, 1428.703228679929907, 223.0784815109979888 ) ) ;
#96191 = CARTESIAN_POINT ( 'NONE',  ( -16.64352143049999810, 1410.411353541330072, 191.7486415517980163 ) ) ;
#96192 = CARTESIAN_POINT ( 'NONE',  ( -0.9609375957247829891, 1496.458315686089918, 221.4414273593889959 ) ) ;
#96193 = VERTEX_POINT ( 'NONE', #82512 ) ;
#96194 = CARTESIAN_POINT ( 'NONE',  ( -17.38483621660000011, 1410.884422118429939, 225.7833436061980024 ) ) ;
#96196 = DIRECTION ( 'NONE',  ( -0.6736849260863837507, 0.000000000000000000, 0.7390186874254154326 ) ) ;
#96195 = CARTESIAN_POINT ( 'NONE',  ( -14.45771159784271376, 1416.835807144213277, 221.3919539079676611 ) ) ;
#96197 = EDGE_CURVE ( 'NONE', #21616, #56695, #2708, .T. ) ;
#96198 = CARTESIAN_POINT ( 'NONE',  ( -0.1535940140686828936, 1487.818612005767591, 219.9756013004578676 ) ) ;
#96199 = CARTESIAN_POINT ( 'NONE',  ( -18.30804477475249925, 1508.522800635979820, 211.1085587802360237 ) ) ;
#96200 = FACE_OUTER_BOUND ( 'NONE', #73841, .T. ) ;
#96201 = CARTESIAN_POINT ( 'NONE',  ( -8.630929624523329124, 1438.255171044090048, 208.1083491479620022 ) ) ;
#96202 = ORIENTED_EDGE ( 'NONE', *, *, #35093, .T. ) ;
#96203 = CARTESIAN_POINT ( 'NONE',  ( -9.846959627583329322, 1409.027766033789931, 270.3779765466370577 ) ) ;
#96204 = CARTESIAN_POINT ( 'NONE',  ( -1.135898823814999847, 1516.958737650239982, 208.0022537503870126 ) ) ;
#96205 = CARTESIAN_POINT ( 'NONE',  ( -1.580871945720000005, 1426.963505220229990, 133.6118001900980232 ) ) ;
#96206 = CARTESIAN_POINT ( 'NONE',  ( 8.257535438202340927, 1436.457248292470013, 206.6719407321619997 ) ) ;
#96208 = ORIENTED_EDGE ( 'NONE', *, *, #65192, .F. ) ;
#96207 = CARTESIAN_POINT ( 'NONE',  ( -6.899207507289689900, 1366.097715433741996, 208.3718459617061285 ) ) ;
#96209 = VERTEX_POINT ( 'NONE', #6889 ) ;
#96210 = CARTESIAN_POINT ( 'NONE',  ( 43.34298913515119978, 1451.640137698500439, 269.0390372527960494 ) ) ;
#96211 = CARTESIAN_POINT ( 'NONE',  ( -2.130922739038390024, 1467.954349360780043, 220.0452206896550251 ) ) ;
#96212 = CARTESIAN_POINT ( 'NONE',  ( -20.49321649319999850, 1486.267955954489935, 212.0899509670090026 ) ) ;
#96213 = AXIS2_PLACEMENT_3D ( 'NONE', #53057, #87764, #51944 ) ;
#96214 = CARTESIAN_POINT ( 'NONE',  ( -0.004275337162772009994, 1408.915998917759907, 186.3744338923069961 ) ) ;
#96215 = CARTESIAN_POINT ( 'NONE',  ( -18.17106232659159915, 1415.393085339859908, 207.5671356270640047 ) ) ;
#96216 = CARTESIAN_POINT ( 'NONE',  ( -18.45191180620000182, 1425.817450471429993, 225.2353046319980194 ) ) ;
#96217 = CARTESIAN_POINT ( 'NONE',  ( 5.256383990386860106, 1475.048120302939878, 269.6502184949890193 ) ) ;
#96218 = CARTESIAN_POINT ( 'NONE',  ( -11.53051474154809952, 1391.913060387269979, 207.8395204436380084 ) ) ;
#96219 = CARTESIAN_POINT ( 'NONE',  ( -17.35007289223692695, 1422.602586090401246, 226.5892681115564642 ) ) ;
#96220 = CARTESIAN_POINT ( 'NONE',  ( 7.321193707744999557, 1516.534976163889951, 206.8301696586770220 ) ) ;
#96221 = ORIENTED_EDGE ( 'NONE', *, *, #99936, .T. ) ;
#96222 = FACE_OUTER_BOUND ( 'NONE', #33375, .T. ) ;
#96223 = CARTESIAN_POINT ( 'NONE',  ( 1.471676140451410042, 1484.933433129259811, 182.0806043343100100 ) ) ;
#96224 = EDGE_LOOP ( 'NONE', ( #107475, #101007, #90930, #69762 ) ) ;
#96225 = CARTESIAN_POINT ( 'NONE',  ( 3.176056732109850067, 1508.610720109290014, 204.4420549359030019 ) ) ;
#96226 = CARTESIAN_POINT ( 'NONE',  ( 25.51839591191980006, 1450.803344685250295, 137.1473335183449933 ) ) ;
#96227 = LINE ( 'NONE', #27362, #109751 ) ;
#96228 = CARTESIAN_POINT ( 'NONE',  ( -25.50709298239999967, 1388.283930419619992, 204.4842806613090147 ) ) ;
#96229 = CARTESIAN_POINT ( 'NONE',  ( 7.550314398180000275, 1423.033197812850176, 195.6993106477989954 ) ) ;
#96230 = CARTESIAN_POINT ( 'NONE',  ( 17.08762417599999850, 1409.674908758129959, 193.0190955581979892 ) ) ;
#96231 = CARTESIAN_POINT ( 'NONE',  ( 20.82705473220000059, 1444.994950788469851, 176.6587301488980017 ) ) ;
#96232 = DIRECTION ( 'NONE',  ( 0.000000000000000000, 1.000000000000000000, 0.000000000000000000 ) ) ;
#96234 = CARTESIAN_POINT ( 'NONE',  ( -20.94045403861742827, 1428.001502734700580, 220.5823066705793565 ) ) ;
#96233 = DIRECTION ( 'NONE',  ( -0.2054769195713296304, 0.000000000000000000, -0.9786619618251631847 ) ) ;
#96235 = AXIS2_PLACEMENT_3D ( 'NONE', #105057, #34533, #78753 ) ;
#96236 = CARTESIAN_POINT ( 'NONE',  ( 0.7101137637400629643, 1451.084754322919935, 182.2944934625020039 ) ) ;
#96237 = CARTESIAN_POINT ( 'NONE',  ( -9.129868668039998525, 1382.253540356249914, 217.9228041959689790 ) ) ;
#96238 = AXIS2_PLACEMENT_3D ( 'NONE', #100797, #92399, #35828 ) ;
#96239 = CARTESIAN_POINT ( 'NONE',  ( 0.7564342142240020328, 1516.783665406140017, 213.7345173100169973 ) ) ;
#96240 = CARTESIAN_POINT ( 'NONE',  ( 26.72687756924920066, 1447.183547681790060, 137.1848390478849922 ) ) ;
#96241 = ORIENTED_EDGE ( 'NONE', *, *, #6203, .F. ) ;
#96242 = CARTESIAN_POINT ( 'NONE',  ( 30.25425994617003767, 1522.382868172863937, 199.2916410102368729 ) ) ;
#96243 = B_SPLINE_SURFACE_WITH_KNOTS ( 'NONE', 5, 1, ( 
 ( #43417, #54050 ),
 ( #52926, #68627 ),
 ( #9258, #51818 ),
 ( #10914, #18187 ),
 ( #52383, #96010 ),
 ( #19280, #61346 ) ),
 .UNSPECIFIED., .F., .F., .F.,
 ( 6, 6 ),
 ( 2, 2 ),
 ( -8.513468052107540614E-05, 17.21697013008050092 ),
 ( 0.000000000000000000, 14.00008513468049998 ),
 .UNSPECIFIED. ) ;
#96244 = CARTESIAN_POINT ( 'NONE',  ( 21.30823923614806858, 1524.382868172804365, 233.7929508216638510 ) ) ;
#96245 = AXIS2_PLACEMENT_3D ( 'NONE', #77804, #103542, #26846 ) ;
#96246 = CARTESIAN_POINT ( 'NONE',  ( -0.3676572738806710428, 1409.061418105000030, 232.3593742318309978 ) ) ;
#96247 = AXIS2_PLACEMENT_3D ( 'NONE', #67729, #67176, #17267 ) ;
#96248 = CARTESIAN_POINT ( 'NONE',  ( 32.28466283162156714, 1501.977400791986611, 219.1752493337713190 ) ) ;
#96249 = CARTESIAN_POINT ( 'NONE',  ( -4.327045307008839714, 1515.156577661799929, 208.9300209000519999 ) ) ;
#96250 = CARTESIAN_POINT ( 'NONE',  ( -26.42714720800000094, 1443.942861155959918, 243.9198229428980085 ) ) ;
#96251 = CARTESIAN_POINT ( 'NONE',  ( -2.395580532111799776, 1451.953014703720100, 184.6449581330110163 ) ) ;
#96252 = CARTESIAN_POINT ( 'NONE',  ( 10.98083629090000102, 1433.016921068679949, 151.7694307944979926 ) ) ;
#96253 = CARTESIAN_POINT ( 'NONE',  ( 9.061802757597490208E-06, 1475.058218891730121, 269.6445798169980321 ) ) ;
#96254 = CARTESIAN_POINT ( 'NONE',  ( 27.35810488257520134, 1440.913060388870008, 228.4442125759339888 ) ) ;
#96255 = CARTESIAN_POINT ( 'NONE',  ( -23.99877502900000081, 1508.007102827230256, 222.4169432911980095 ) ) ;
#96256 = CARTESIAN_POINT ( 'NONE',  ( -17.72527547369999823, 1420.469651944000134, 207.4580708041989965 ) ) ;
#96257 = ORIENTED_EDGE ( 'NONE', *, *, #6871, .T. ) ;
#96258 = CARTESIAN_POINT ( 'NONE',  ( -29.40443212115373939, 1511.187213306747708, 222.0897836382247306 ) ) ;
#96259 = CARTESIAN_POINT ( 'NONE',  ( 22.91663120903140083, 1507.606285602550088, 210.6365840681099826 ) ) ;
#96260 = CARTESIAN_POINT ( 'NONE',  ( -15.78519159560000062, 1486.362372667630098, 186.5259617109979899 ) ) ;
#96261 = CARTESIAN_POINT ( 'NONE',  ( 4.200862373802610072, 1398.037452366075058, 196.7985206626544539 ) ) ;
#96262 = CARTESIAN_POINT ( 'NONE',  ( 2.133183460910000218, 1482.812097613729975, 235.0898365658979969 ) ) ;
#96263 = CIRCLE ( 'NONE', #99838, 3.500000000000003109 ) ;
#96264 = CARTESIAN_POINT ( 'NONE',  ( 24.55148953060000139, 1430.358502415830117, 211.1312658929579982 ) ) ;
#96265 = CARTESIAN_POINT ( 'NONE',  ( 0.4151546846821903003, 1512.187213306747481, 243.9330574173806951 ) ) ;
#96266 = CARTESIAN_POINT ( 'NONE',  ( -10.82593705289999875, 1509.291110439329941, 235.9458924929979844 ) ) ;
#96267 = CARTESIAN_POINT ( 'NONE',  ( -36.25285754200669430, 1383.833716293010184, 235.7112261900410033 ) ) ;
#96268 = CARTESIAN_POINT ( 'NONE',  ( -3.788228201615989832, 1508.728292637470076, 204.8186040600340050 ) ) ;
#96269 = CARTESIAN_POINT ( 'NONE',  ( 6.232532001850000114, 1407.162969929529936, 220.5304192662980256 ) ) ;
#96270 = CARTESIAN_POINT ( 'NONE',  ( -27.01473127741192570, 1509.856435591600302, 196.9755962829802343 ) ) ;
#96271 = CARTESIAN_POINT ( 'NONE',  ( 0.1605139477524830105, 1485.957458676359920, 181.8384362477690104 ) ) ;
#96273 = ORIENTED_EDGE ( 'NONE', *, *, #50285, .F. ) ;
#96272 = CARTESIAN_POINT ( 'NONE',  ( 18.28406076839999983, 1431.588999307289896, 208.2780601718820037 ) ) ;
#96274 = CARTESIAN_POINT ( 'NONE',  ( -20.12133088869999753, 1445.052233488290085, 161.1306464489979930 ) ) ;
#96275 = CARTESIAN_POINT ( 'NONE',  ( -3.078458354199999913, 1382.920902153249926, 199.9060629954589956 ) ) ;
#96276 = EDGE_CURVE ( 'NONE', #74738, #96843, #109575, .T. ) ;
#96277 = CARTESIAN_POINT ( 'NONE',  ( -3.950036120199999612, 1475.164021116390131, 199.1854335113090144 ) ) ;
#96279 = ORIENTED_EDGE ( 'NONE', *, *, #88850, .F. ) ;
#96278 = CARTESIAN_POINT ( 'NONE',  ( -36.33941889825980809, 1451.266910394130036, 134.0999999986779869 ) ) ;
#96280 = CARTESIAN_POINT ( 'NONE',  ( -3.200625999729659554, 1508.551704408389924, 219.9719447069430203 ) ) ;
#96281 = VERTEX_POINT ( 'NONE', #75764 ) ;
#96282 = CARTESIAN_POINT ( 'NONE',  ( -14.41810545100110019, 1380.214461174779899, 209.1805091506649887 ) ) ;
#96283 = CARTESIAN_POINT ( 'NONE',  ( -2.869809977300000092, 1489.506021206889955, 188.4705320259990060 ) ) ;
#96284 = FACE_OUTER_BOUND ( 'NONE', #9984, .T. ) ;
#96285 = DIRECTION ( 'NONE',  ( -0.09978697244513583253, 0.9945729288003561930, -0.02944909892875140905 ) ) ;
#96286 = CARTESIAN_POINT ( 'NONE',  ( -1.324219039799999997, 1431.506123345290007, 217.5609468189390157 ) ) ;
#96287 = CARTESIAN_POINT ( 'NONE',  ( -15.61813151019999957, 1420.484314087570056, 211.1660300703989890 ) ) ;
#96288 = CARTESIAN_POINT ( 'NONE',  ( 10.72705856214020059, 1409.287657520459788, 219.5401174626420016 ) ) ;
#96289 = FACE_OUTER_BOUND ( 'NONE', #8498, .T. ) ;
#96290 = CARTESIAN_POINT ( 'NONE',  ( -99.64099788066441477, 1385.219955568270052, 296.2123915739539939 ) ) ;
#96291 = CARTESIAN_POINT ( 'NONE',  ( -17.71575766480000169, 1417.732977527630055, 192.4301206783980263 ) ) ;
#96292 = CARTESIAN_POINT ( 'NONE',  ( -44.12060424749999754, 1379.737242085850085, 229.5711980135589840 ) ) ;
#96293 = VERTEX_POINT ( 'NONE', #33192 ) ;
#96294 = CARTESIAN_POINT ( 'NONE',  ( 10.96709298812059963, 1490.204820260260021, 209.1517527257469737 ) ) ;
#96295 = EDGE_CURVE ( 'NONE', #55409, #69449, #82787, .T. ) ;
#96297 = ORIENTED_EDGE ( 'NONE', *, *, #4232, .T. ) ;
#96296 = DIRECTION ( 'NONE',  ( -0.9455185755993178454, 0.000000000000000000, 0.3255681544571537578 ) ) ;
#96298 = ORIENTED_EDGE ( 'NONE', *, *, #62445, .T. ) ;
#96299 = CARTESIAN_POINT ( 'NONE',  ( -12.08615242673420020, 1415.948038442749976, 194.8431646156840031 ) ) ;
#96300 = CARTESIAN_POINT ( 'NONE',  ( -3.755143501086812829, 1361.939125317512662, 210.6218459617142003 ) ) ;
#96301 = CARTESIAN_POINT ( 'NONE',  ( -11.77299894129999913, 1433.946611324799960, 151.0520174426980020 ) ) ;
#96302 = EDGE_CURVE ( 'NONE', #49611, #17686, #74882, .T. ) ;
#96303 = CARTESIAN_POINT ( 'NONE',  ( 2.753149778868899666, 1471.436294210167489, 269.3346708043688409 ) ) ;
#96304 = CARTESIAN_POINT ( 'NONE',  ( -31.02592223166947250, 1526.278758871496620, 219.9652544506489562 ) ) ;
#96305 = CARTESIAN_POINT ( 'NONE',  ( 2.562074494179999995, 1397.677066227130126, 221.9695021218980173 ) ) ;
#96306 = CARTESIAN_POINT ( 'NONE',  ( -6.073016847162494791, 1516.743606062366780, 213.5232657706371810 ) ) ;
#96307 = CARTESIAN_POINT ( 'NONE',  ( -0.8670487806669999742, 1452.172290198730025, 183.4042211072979853 ) ) ;
#96308 = CARTESIAN_POINT ( 'NONE',  ( -11.16448629964019190, 1365.517506221394797, 210.6218459617030021 ) ) ;
#96309 = CARTESIAN_POINT ( 'NONE',  ( -25.41904847911940735, 1436.620868978935960, 137.2922833411249144 ) ) ;
#96310 = CARTESIAN_POINT ( 'NONE',  ( -3.462948834675000143, 1516.956048353049937, 206.8373194734570006 ) ) ;
#96311 = AXIS2_PLACEMENT_3D ( 'NONE', #50060, #103182, #42751 ) ;
#96312 = CARTESIAN_POINT ( 'NONE',  ( -13.01880433582340046, 1435.354293861170163, 150.4303184084199927 ) ) ;
#96313 = CARTESIAN_POINT ( 'NONE',  ( 21.13431379670319998, 1409.651086887829933, 206.4149708788170301 ) ) ;
#96314 = DIRECTION ( 'NONE',  ( 1.000000000000000000, 0.000000000000000000, -0.000000000000000000 ) ) ;
#96316 = CARTESIAN_POINT ( 'NONE',  ( -3.703568382519999869, 1497.311625982490114, 220.9591690777990038 ) ) ;
#96315 = CIRCLE ( 'NONE', #17629, 8.104319688360000384 ) ;
#96317 = CARTESIAN_POINT ( 'NONE',  ( 41.65274031657839515, 1444.011424526299834, 135.7904737122629797 ) ) ;
#96318 = ORIENTED_EDGE ( 'NONE', *, *, #72188, .F. ) ;
#96319 = AXIS2_PLACEMENT_3D ( 'NONE', #108496, #13861, #14416 ) ;
#96320 = CARTESIAN_POINT ( 'NONE',  ( 35.25149216619999493, 1420.828141007130171, 264.2529782732980266 ) ) ;
#96321 = CARTESIAN_POINT ( 'NONE',  ( -26.83695571260000179, 1488.686901730929776, 205.9593982892680231 ) ) ;
#96323 = CARTESIAN_POINT ( 'NONE',  ( 13.22475641109999955, 1415.063410489729904, 197.5370647170979623 ) ) ;
#96322 = CARTESIAN_POINT ( 'NONE',  ( -10.71072610778340106, 1425.695308460959950, 95.13476052875000732 ) ) ;
#96324 = CARTESIAN_POINT ( 'NONE',  ( -2.476733514145000203, 1516.858326417339867, 211.6155457388669845 ) ) ;
#96325 = EDGE_CURVE ( 'NONE', #100339, #86845, #108547, .T. ) ;
#96326 = DIRECTION ( 'NONE',  ( 2.473221764039894783E-17, 0.000000000000000000, 1.000000000000000000 ) ) ;
#96327 = CARTESIAN_POINT ( 'NONE',  ( -10.82132307030000007, 1413.960774651630118, 250.5360043753979653 ) ) ;
#96328 = CARTESIAN_POINT ( 'NONE',  ( 3.153551286829999967, 1486.681966494889821, 219.4644408646990144 ) ) ;
#96329 = CARTESIAN_POINT ( 'NONE',  ( 29.27865644803159739, 1509.812245387229950, 209.6041006200670154 ) ) ;
#96330 = CARTESIAN_POINT ( 'NONE',  ( 2.684965486993618811, 1448.122735116655349, 154.7390415180112200 ) ) ;
#96331 = DIRECTION ( 'NONE',  ( -0.7071067576156506718, 3.866377236683057960E-11, 0.7071068047574436966 ) ) ;
#96332 = VERTEX_POINT ( 'NONE', #35969 ) ;
#96333 = CARTESIAN_POINT ( 'NONE',  ( -1.546949757679999760, 1416.828040475729949, 228.0209010782980101 ) ) ;
#96334 = CARTESIAN_POINT ( 'NONE',  ( 12.24386287430722575, 1513.118420038113072, 225.7974128742104369 ) ) ;
#96335 = CARTESIAN_POINT ( 'NONE',  ( 14.31461351079999922, 1509.452791170529963, 235.1998141392979846 ) ) ;
#96336 = ORIENTED_EDGE ( 'NONE', *, *, #109314, .T. ) ;
#96337 = ORIENTED_EDGE ( 'NONE', *, *, #54901, .F. ) ;
#96338 = CARTESIAN_POINT ( 'NONE',  ( -2.424063131930000115, 1427.257651041929876, 147.9020499575979954 ) ) ;
#96339 = CARTESIAN_POINT ( 'NONE',  ( -3.149355042448929609, 1421.363409048820131, 147.6430095841799925 ) ) ;
#96340 = ORIENTED_EDGE ( 'NONE', *, *, #48707, .F. ) ;
#96341 = CARTESIAN_POINT ( 'NONE',  ( -0.1629132599120000080, 1424.309591313030069, 227.6950206218980099 ) ) ;
#96342 = AXIS2_PLACEMENT_3D ( 'NONE', #23332, #30079, #22760 ) ;
#96343 = CARTESIAN_POINT ( 'NONE',  ( 7.735000377495650170, 1446.700284064708057, 154.1094615265521384 ) ) ;
#96344 = FACE_OUTER_BOUND ( 'NONE', #81999, .T. ) ;
#96345 = B_SPLINE_CURVE_WITH_KNOTS ( 'NONE', 3,
 ( #89356, #81487, #96097, #2624 ),
 .UNSPECIFIED., .F., .F.,
 ( 4, 4 ),
 ( 0.0004474573906021131627, 0.001555588287050983787 ),
 .UNSPECIFIED. ) ;
#96346 = CARTESIAN_POINT ( 'NONE',  ( -2.338091437230000125, 1489.062396073530181, 236.1656132279979943 ) ) ;
#96347 = CARTESIAN_POINT ( 'NONE',  ( 7.203707678260440339, 1508.728101425929935, 202.3962581857610132 ) ) ;
#96348 = DIRECTION ( 'NONE',  ( 0.9955685427536684617, -0.04363816682463440150, -0.08330058268416962175 ) ) ;
#96349 = CARTESIAN_POINT ( 'NONE',  ( 6.277696993560000216, 1462.172825430389821, 207.2400390766889871 ) ) ;
#96350 = CARTESIAN_POINT ( 'NONE',  ( 0.07204350251990000731, 1420.438792470029966, 183.3235075831980225 ) ) ;
#96351 = ORIENTED_EDGE ( 'NONE', *, *, #73055, .T. ) ;
#96352 = CARTESIAN_POINT ( 'NONE',  ( 7.715625202974999652, 1516.786099423779888, 202.5670817708370066 ) ) ;
#96353 = CARTESIAN_POINT ( 'NONE',  ( 4.626591867355000609, 1517.096587378560116, 210.8266407735670214 ) ) ;
#96354 = VERTEX_POINT ( 'NONE', #70160 ) ;
#96355 = CARTESIAN_POINT ( 'NONE',  ( 11.86000693848920129, 1431.910640742250052, 149.9657772557100088 ) ) ;
#96356 = DIRECTION ( 'NONE',  ( 0.3363363969979655810, -0.9417419115949056119, 0.000000000000000000 ) ) ;
#96357 = ORIENTED_EDGE ( 'NONE', *, *, #27666, .F. ) ;
#96358 = CARTESIAN_POINT ( 'NONE',  ( -9.813597492012577916, 1516.551188145990182, 203.5583050039579973 ) ) ;
#96359 = CARTESIAN_POINT ( 'NONE',  ( -7.026031763481809911, 1508.551704408389924, 219.1713198989909870 ) ) ;
#96360 = CARTESIAN_POINT ( 'NONE',  ( -17.02584102842030234, 1420.296749622020116, 203.9584675048969871 ) ) ;
#96361 = CARTESIAN_POINT ( 'NONE',  ( -9.762135819850678686, 1470.449700743350149, 213.1189514009770107 ) ) ;
#96362 = CARTESIAN_POINT ( 'NONE',  ( -1.514738108749209999, 1507.606285622480073, 232.0384771855580084 ) ) ;
#96363 = CARTESIAN_POINT ( 'NONE',  ( 0.9912764913912639475, 1407.655978583209844, 270.1376065755259788 ) ) ;
#96364 = CARTESIAN_POINT ( 'NONE',  ( -106.9747615859999996, 1387.585777271070128, 298.0968282848589865 ) ) ;
#96365 = CARTESIAN_POINT ( 'NONE',  ( -5.062209827260000239, 1474.342206524190033, 198.8731686433990262 ) ) ;
#96366 = CARTESIAN_POINT ( 'NONE',  ( -2.472546487080370170, 1422.360492482099744, 192.6709265187130029 ) ) ;
#96367 = CARTESIAN_POINT ( 'NONE',  ( -16.46152824260000003, 1379.712491941360213, 208.5854493838049848 ) ) ;
#96368 = CARTESIAN_POINT ( 'NONE',  ( 7.539561783740881040, 1423.272083796969127, 195.6671181022157100 ) ) ;
#96370 = CARTESIAN_POINT ( 'NONE',  ( 10.94478922204540083, 1470.010321155669772, 206.1681359757739926 ) ) ;
#96369 = CARTESIAN_POINT ( 'NONE',  ( -17.60187515309999995, 1504.668623956589954, 208.9385782990950133 ) ) ;
#96371 = CARTESIAN_POINT ( 'NONE',  ( -66.42203761248978822, 1379.747445253714659, 277.0326445464845619 ) ) ;
#96372 = CARTESIAN_POINT ( 'NONE',  ( 17.67562304467840306, 1413.141888578579938, 224.8738151114190202 ) ) ;
#96373 = CARTESIAN_POINT ( 'NONE',  ( -7.587489932915000068, 1513.914017980330073, 202.7196074656669964 ) ) ;
#96374 = ORIENTED_EDGE ( 'NONE', *, *, #75587, .T. ) ;
#96375 = CARTESIAN_POINT ( 'NONE',  ( 29.75208676439999778, 1419.160608152629948, 268.3665355202980436 ) ) ;
#96376 = CIRCLE ( 'NONE', #98199, 5.000000000000000888 ) ;
#96377 = CARTESIAN_POINT ( 'NONE',  ( 19.75084982879439721, 1455.504334177440114, 226.5702129464319796 ) ) ;
#96378 = CARTESIAN_POINT ( 'NONE',  ( -71.67062476821969597, 1385.018456839120063, 296.8795409282479909 ) ) ;
#96379 = B_SPLINE_SURFACE_WITH_KNOTS ( 'NONE', 5, 4, ( 
 ( #63104, #19376, #71506, #104505, #44615 ),
 ( #9347, #27800, #88263, #9889, #11004 ),
 ( #35090, #61429, #44057, #95553, #105063 ),
 ( #11556, #26681, #45176, #96102, #69272 ),
 ( #78197, #97201, #95006, #28352, #1509 ),
 ( #45733, #18274, #79317, #79869, #103950 ) ),
 .UNSPECIFIED., .F., .F., .F.,
 ( 6, 6 ),
 ( 5, 5 ),
 ( -1.065814103640000080E-14, 23.05527389429999729 ),
 ( 130.1608902480000154, 151.7353186150000113 ),
 .UNSPECIFIED. ) ;
#96380 = CARTESIAN_POINT ( 'NONE',  ( 1.338019250827790163, 1431.361302059610125, 218.5179660117710227 ) ) ;
#96381 = CARTESIAN_POINT ( 'NONE',  ( 5.137469271169999629, 1505.238374756890153, 220.3656813046989953 ) ) ;
#96382 = CARTESIAN_POINT ( 'NONE',  ( -14.93717996069999998, 1416.181292681839977, 212.9156383665589942 ) ) ;
#96384 = ORIENTED_EDGE ( 'NONE', *, *, #59616, .F. ) ;
#96383 = CARTESIAN_POINT ( 'NONE',  ( -1.554992009257179841, 1515.071272245639875, 204.7925668544159805 ) ) ;
#96385 = B_SPLINE_CURVE_WITH_KNOTS ( 'NONE', 3,
 ( #45095, #85964, #94919, #104419, #1988, #36123, #61899, #70862, #96016, #28262, #26029, #2544, #19287, #53488, #87632, #880, #79235, #18193, #52389, #9804, #104973, #35004, #62456, #96579, #51257 ),
 .UNSPECIFIED., .F., .F.,
 ( 4, 3, 3, 3, 3, 3, 3, 3, 4 ),
 ( -7.174290254210000661, -7.054144120975740506, -6.393701831169590122, -5.726089240763790222, -5.061843816283770003, -4.939077517077059554, -4.323976577597050230, -3.586109338910330013, -2.949396961920000670 ),
 .UNSPECIFIED. ) ;
#96386 = CARTESIAN_POINT ( 'NONE',  ( -15.71805126636130545, 1415.757702161196903, 209.6739713832304233 ) ) ;
#96387 = CARTESIAN_POINT ( 'NONE',  ( -24.75614383750000158, 1444.003657534250124, 210.7102618898479705 ) ) ;
#96388 = CIRCLE ( 'NONE', #60684, 2.000000000000003109 ) ;
#96389 = CARTESIAN_POINT ( 'NONE',  ( -2.299601840677758968, 1449.771133279514743, 154.4058190498332976 ) ) ;
#96390 = CARTESIAN_POINT ( 'NONE',  ( -0.4909561157465350267, 1430.166341371809949, 199.7248743074169965 ) ) ;
#96391 = CARTESIAN_POINT ( 'NONE',  ( 15.21523570123499880, 1514.242353506929931, 224.0841638630670047 ) ) ;
#96392 = CARTESIAN_POINT ( 'NONE',  ( -10.44063514870000020, 1441.240651982340069, 187.1052350852980055 ) ) ;
#96393 = CARTESIAN_POINT ( 'NONE',  ( 13.23644882699999847, 1509.506897669330101, 180.9128671145980150 ) ) ;
#96394 = B_SPLINE_CURVE_WITH_KNOTS ( 'NONE', 3,
 ( #40973, #25253, #14109, #48299, #104192, #42635 ),
 .UNSPECIFIED., .F., .F.,
 ( 4, 2, 4 ),
 ( 0.000000000000000000, 0.5000000000000000000, 1.000000000000000000 ),
 .UNSPECIFIED. ) ;
#96395 = DIRECTION ( 'NONE',  ( -0.000000000000000000, -1.000000000000000000, -0.000000000000000000 ) ) ;
#96396 = CARTESIAN_POINT ( 'NONE',  ( -0.9746356023110001043, 1408.913060387329779, 227.8345159065979715 ) ) ;
#96397 = CARTESIAN_POINT ( 'NONE',  ( 11.29156966579999910, 1417.418038064730126, 229.6347434530979967 ) ) ;
#96398 = CARTESIAN_POINT ( 'NONE',  ( -6.343596359860000256, 1477.040213282090008, 217.6105473213789878 ) ) ;
#96399 = CARTESIAN_POINT ( 'NONE',  ( -16.13220469984199923, 1459.078176189990018, 230.3616190125399896 ) ) ;
#96400 = CARTESIAN_POINT ( 'NONE',  ( 3.251888829344999898, 1516.793978928989873, 206.6294022811970024 ) ) ;
#96401 = CARTESIAN_POINT ( 'NONE',  ( 39.60334749029999557, 1422.313230794130277, 267.8221855244979679 ) ) ;
#96402 = CARTESIAN_POINT ( 'NONE',  ( -34.18677586421173942, 1522.382868172863937, 219.7932833225216882 ) ) ;
#96403 = CARTESIAN_POINT ( 'NONE',  ( 20.70415920599999637, 1436.034498798209825, 144.5456087543980175 ) ) ;
#96404 = AXIS2_PLACEMENT_3D ( 'NONE', #54263, #80546, #45309 ) ;
#96405 = CARTESIAN_POINT ( 'NONE',  ( 26.29659629110000196, 1508.005140778730038, 202.4501866991980137 ) ) ;
#96406 = CARTESIAN_POINT ( 'NONE',  ( 5.359760538142340103, 1422.219520672319959, 145.5218257772459935 ) ) ;
#96407 = TOROIDAL_SURFACE ( 'NONE', #78589, 3.500000000000000000, 2.000000000000000000 ) ;
#96408 = CARTESIAN_POINT ( 'NONE',  ( -13.02155667789130078, 1379.339783279080166, 208.0032768703970021 ) ) ;
#96409 = CARTESIAN_POINT ( 'NONE',  ( 12.45665488799999920, 1416.827520120730014, 223.4764148226980183 ) ) ;
#96410 = CARTESIAN_POINT ( 'NONE',  ( 32.86802468386292020, 1523.382868172864164, 217.2040256693915410 ) ) ;
#96411 = CARTESIAN_POINT ( 'NONE',  ( -39.99259053121770080, 1438.670161830759753, 135.1922219426939762 ) ) ;
#96412 = CARTESIAN_POINT ( 'NONE',  ( -13.55937006006110046, 1409.552480571150227, 226.6517346244539794 ) ) ;
#96413 = CARTESIAN_POINT ( 'NONE',  ( -17.66282533229999885, 1415.426091369230107, 205.3741255001079935 ) ) ;
#96414 = CARTESIAN_POINT ( 'NONE',  ( -12.33746580920000113, 1440.929426004120160, 187.9427475994980057 ) ) ;
#96415 = SPHERICAL_SURFACE ( 'NONE', #26535, 18.16666666670000296 ) ;
#96416 = CARTESIAN_POINT ( 'NONE',  ( -33.15526401089999808, 1436.131197805709917, 136.3224491675979948 ) ) ;
#96417 = CARTESIAN_POINT ( 'NONE',  ( 8.959051896893781120, 1436.612241212953904, 210.6498963299843012 ) ) ;
#96418 = VERTEX_POINT ( 'NONE', #10204 ) ;
#96419 = CARTESIAN_POINT ( 'NONE',  ( -2.930838077694999821, 1510.983859056260144, 201.5581577403170002 ) ) ;
#96420 = CARTESIAN_POINT ( 'NONE',  ( -7.298806753422620197, 1409.167940335549929, 222.1915275659999907 ) ) ;
#96421 = DIRECTION ( 'NONE',  ( 0.000000000000000000, -1.000000000000000000, 0.000000000000000000 ) ) ;
#96422 = CARTESIAN_POINT ( 'NONE',  ( -2.745154014197499937, 1419.769956470485113, 137.0999999980979851 ) ) ;
#96423 = CARTESIAN_POINT ( 'NONE',  ( -46.05258988370000139, 1440.913037442780023, 266.6770556630980309 ) ) ;
#96425 = TOROIDAL_SURFACE ( 'NONE', #46411, 2.000000000000000000, 1.000000000000000000 ) ;
#96424 = CARTESIAN_POINT ( 'NONE',  ( -16.09266893903710383, 1469.459467177870010, 223.0552979758230094 ) ) ;
#96426 = CARTESIAN_POINT ( 'NONE',  ( 0.2286803964500180031, 1420.490562101879959, 182.9054483574730057 ) ) ;
#96427 = CARTESIAN_POINT ( 'NONE',  ( 19.98413504155174181, 1526.143142182265819, 233.2906832177060039 ) ) ;
#96428 = CARTESIAN_POINT ( 'NONE',  ( -97.79596852057099454, 1384.604925093459997, 310.5386097793889917 ) ) ;
#96429 = CARTESIAN_POINT ( 'NONE',  ( -47.40790290358329884, 1385.010400382010175, 221.4590170555140105 ) ) ;
#96430 = CARTESIAN_POINT ( 'NONE',  ( 17.10099828737380179, 1423.827771296450010, 227.6321784446419940 ) ) ;
#96431 = FACE_OUTER_BOUND ( 'NONE', #67007, .T. ) ;
#96432 = CARTESIAN_POINT ( 'NONE',  ( 15.25592359020000011, 1495.928552999029989, 224.4451643109979955 ) ) ;
#96433 = CARTESIAN_POINT ( 'NONE',  ( -26.29993148601639774, 1495.365167192059971, 212.0160643654880062 ) ) ;
#96434 = EDGE_CURVE ( 'NONE', #24399, #38170, #58801, .T. ) ;
#96435 = CARTESIAN_POINT ( 'NONE',  ( -5.013435694540000043, 1375.426148861440197, 214.7180213005390215 ) ) ;
#96436 = CARTESIAN_POINT ( 'NONE',  ( -9.094817557369999861, 1384.935820800019883, 199.9428001500290293 ) ) ;
#96437 = CARTESIAN_POINT ( 'NONE',  ( 3.281831459213320201, 1466.303209658950209, 198.5678429405679992 ) ) ;
#96438 = CARTESIAN_POINT ( 'NONE',  ( 13.95470622120000037, 1415.426952350729835, 197.1288800259980292 ) ) ;
#96439 = CARTESIAN_POINT ( 'NONE',  ( -12.71684466930000035, 1416.535385209229844, 195.1197337799980005 ) ) ;
#96440 = CYLINDRICAL_SURFACE ( 'NONE', #72968, 2.000000000000003109 ) ;
#96441 = ADVANCED_FACE ( 'NONE', ( #27015 ), #19704, .F. ) ;
#96442 = CARTESIAN_POINT ( 'NONE',  ( 23.42036295790000366, 1410.652421255329955, 212.1072478527780163 ) ) ;
#96443 = CARTESIAN_POINT ( 'NONE',  ( 13.89554995500000167, 1452.733480491630189, 223.3956528723979886 ) ) ;
#96444 = CARTESIAN_POINT ( 'NONE',  ( 18.95586338705119900, 1455.565549131589933, 200.3905214973929958 ) ) ;
#96445 = CARTESIAN_POINT ( 'NONE',  ( -5.374474455745339441, 1429.012600464609932, 154.0236767292889795 ) ) ;
#96447 = CARTESIAN_POINT ( 'NONE',  ( -11.38166339569999863, 1381.807649517150139, 201.7589817661390157 ) ) ;
#96446 = CARTESIAN_POINT ( 'NONE',  ( -11.58007427770000142, 1432.582736770090150, 151.1961013139979855 ) ) ;
#96448 = CARTESIAN_POINT ( 'NONE',  ( -5.081549580979999980, 1391.866816822089959, 203.6256639786390110 ) ) ;
#96449 = CARTESIAN_POINT ( 'NONE',  ( 0.3744602044770000138, 1467.547738470929971, 229.3988225936980143 ) ) ;
#96450 = CARTESIAN_POINT ( 'NONE',  ( -10.99273643789999966, 1491.630725559690063, 209.8916748351909973 ) ) ;
#96451 = CARTESIAN_POINT ( 'NONE',  ( 7.146147325059948763, 1378.399971913189802, 209.1218459616989946 ) ) ;
#96452 = CARTESIAN_POINT ( 'NONE',  ( -9.977700672470000143, 1365.292605733889786, 210.6218459616991936 ) ) ;
#96453 = CARTESIAN_POINT ( 'NONE',  ( 4.998515157294999511, 1516.787536375099990, 205.0819486540370065 ) ) ;
#96454 = CARTESIAN_POINT ( 'NONE',  ( -6.799851167021637721, 1423.999032497903045, 192.0811406717795080 ) ) ;
#96455 = CARTESIAN_POINT ( 'NONE',  ( -15.64556917516660128, 1486.082452306300183, 186.7299835657600227 ) ) ;
#96456 = CARTESIAN_POINT ( 'NONE',  ( -8.742754168010000271, 1424.489613839150024, 206.0336725849989818 ) ) ;
#96457 = CIRCLE ( 'NONE', #46435, 0.9999999999999986677 ) ;
#96458 = CARTESIAN_POINT ( 'NONE',  ( -4.272053644645270154, 1441.099711618939864, 157.6237339584640154 ) ) ;
#96460 = ORIENTED_EDGE ( 'NONE', *, *, #66461, .T. ) ;
#96459 = CARTESIAN_POINT ( 'NONE',  ( -67.00076415430000054, 1379.747503662089912, 277.9341329109589651 ) ) ;
#96461 = VERTEX_POINT ( 'NONE', #79639 ) ;
#96462 = CARTESIAN_POINT ( 'NONE',  ( 27.80989915279999991, 1508.614438783829883, 211.9044001959479999 ) ) ;
#96463 = ORIENTED_EDGE ( 'NONE', *, *, #3499, .F. ) ;
#96464 = CARTESIAN_POINT ( 'NONE',  ( -8.861333410889999485, 1384.870662623839962, 218.6848950059789729 ) ) ;
#96465 = CARTESIAN_POINT ( 'NONE',  ( 11.44321141689999877, 1500.298942533189802, 206.0875178983189926 ) ) ;
#96467 = CARTESIAN_POINT ( 'NONE',  ( -2.372478608332514671, 1512.187213306747481, 243.3440112565233449 ) ) ;
#96466 = CARTESIAN_POINT ( 'NONE',  ( 15.89484604643729959, 1418.061013547770017, 191.2943550237069985 ) ) ;
#96468 = CARTESIAN_POINT ( 'NONE',  ( 12.00000000000000000, 1443.913060387330006, 147.5878346084980137 ) ) ;
#96469 = CIRCLE ( 'NONE', #10621, 1.999999999999999556 ) ;
#96470 = CARTESIAN_POINT ( 'NONE',  ( -24.64113440033070290, 1451.811919332890056, 137.3348792521310031 ) ) ;
#96471 = CARTESIAN_POINT ( 'NONE',  ( -106.0957693905839960, 1378.913060388589884, 305.6009486211909802 ) ) ;
#96472 = CARTESIAN_POINT ( 'NONE',  ( 11.37232255049999807, 1409.477095359130089, 228.6758770766980149 ) ) ;
#96473 = CARTESIAN_POINT ( 'NONE',  ( -4.997250192034999650, 1516.727068157269969, 212.3866247496169990 ) ) ;
#96474 = CARTESIAN_POINT ( 'NONE',  ( 40.11569180289929903, 1438.966375984099841, 134.0999999981379744 ) ) ;
#96475 = CARTESIAN_POINT ( 'NONE',  ( -7.175751430708140255, 1425.273472374989979, 206.5995256342289963 ) ) ;
#96476 = CARTESIAN_POINT ( 'NONE',  ( -10603.70820142147204, 2837.742859910728839, -4739.672918702562129 ) ) ;
#96477 = ORIENTED_EDGE ( 'NONE', *, *, #49662, .F. ) ;
#96478 = CARTESIAN_POINT ( 'NONE',  ( -3.076366055149999834, 1424.853903601579987, 191.3970713258989917 ) ) ;
#96479 = CARTESIAN_POINT ( 'NONE',  ( 0.6340598045975409658, 1432.588596709849980, 200.7036721141990085 ) ) ;
#96480 = ORIENTED_EDGE ( 'NONE', *, *, #87728, .T. ) ;
#96481 = VERTEX_POINT ( 'NONE', #2942 ) ;
#96482 = VERTEX_POINT ( 'NONE', #77961 ) ;
#96483 = CARTESIAN_POINT ( 'NONE',  ( 12.80760530667942199, 1444.977579513412593, 169.4484619471895712 ) ) ;
#96484 = CARTESIAN_POINT ( 'NONE',  ( -2.779180994119999859, 1465.191645338429907, 235.7831128362979882 ) ) ;
#96485 = CARTESIAN_POINT ( 'NONE',  ( 21.81318580550076192, 1450.920854193619562, 143.4612878731137755 ) ) ;
#96486 = DIRECTION ( 'NONE',  ( -1.000000000000000000, 0.000000000000000000, 0.000000000000000000 ) ) ;
#96487 = CARTESIAN_POINT ( 'NONE',  ( 2.183557716942239768, 1465.964082040959738, 198.3088933049640161 ) ) ;
#96488 = AXIS2_PLACEMENT_3D ( 'NONE', #84673, #85783, #59503 ) ;
#96489 = CARTESIAN_POINT ( 'NONE',  ( -2.470168521978398868, 1501.977400791986611, 175.3649660270905315 ) ) ;
#96490 = CARTESIAN_POINT ( 'NONE',  ( -49.24152454686350922, 1379.685811767087898, 238.1174555105647528 ) ) ;
#96491 = CARTESIAN_POINT ( 'NONE',  ( 2.128647007970000171, 1464.204386043490103, 199.5196855943389949 ) ) ;
#96492 =( BOUNDED_CURVE ( )  B_SPLINE_CURVE ( 3, ( #65437, #75491, #83313, #108516 ),
 .UNSPECIFIED., .F., .F. ) 
 B_SPLINE_CURVE_WITH_KNOTS ( ( 4, 4 ),
 ( 1.092045427080897246, 2.049540592268306316 ),
 .UNSPECIFIED. ) 
 CURVE ( )  GEOMETRIC_REPRESENTATION_ITEM ( )  RATIONAL_B_SPLINE_CURVE ( ( 1.000000000000000000, 0.9250483781718910059, 0.9250483781718910059, 1.000000000000000000 ) ) 
 REPRESENTATION_ITEM ( '' )  );
#96493 = CARTESIAN_POINT ( 'NONE',  ( 0.3248775019619999926, 1507.888195423030083, 237.5163462374979702 ) ) ;
#96494 = ORIENTED_EDGE ( 'NONE', *, *, #99292, .F. ) ;
#96495 = CARTESIAN_POINT ( 'NONE',  ( 7.708745647785000266, 1516.523379810429788, 207.4137536659370085 ) ) ;
#96496 = ORIENTED_EDGE ( 'NONE', *, *, #9938, .F. ) ;
#96497 = CARTESIAN_POINT ( 'NONE',  ( 24.88822351442950165, 1440.913060387330006, 238.7353654863360077 ) ) ;
#96498 = CARTESIAN_POINT ( 'NONE',  ( 11.75720880967569926, 1479.323378685179932, 208.5706975412350062 ) ) ;
#96499 = ORIENTED_EDGE ( 'NONE', *, *, #98917, .F. ) ;
#96500 = CARTESIAN_POINT ( 'NONE',  ( 26.03221818079370209, 1448.976886533850120, 137.1487683874059940 ) ) ;
#96501 = CARTESIAN_POINT ( 'NONE',  ( -13.70448594279999988, 1409.558350370729841, 190.6766190893979740 ) ) ;
#96502 = CARTESIAN_POINT ( 'NONE',  ( -60.50191481579621922, 1379.727517218082312, 266.7693724609832202 ) ) ;
#96504 = CARTESIAN_POINT ( 'NONE',  ( -33.36586802512168504, 1511.187213306747708, 216.3367586934473366 ) ) ;
#96503 = CARTESIAN_POINT ( 'NONE',  ( -24.35991799298464855, 1439.691670408465825, 212.0269959679101817 ) ) ;
#96505 = CARTESIAN_POINT ( 'NONE',  ( -11.03427950878080210, 1414.913526845469960, 195.9671336867000093 ) ) ;
#96506 = CARTESIAN_POINT ( 'NONE',  ( 0.0002639953367722339020, 1396.486682381765377, 196.7203582614270658 ) ) ;
#96507 = CARTESIAN_POINT ( 'NONE',  ( -12.92957505356057268, 1434.745003379313857, 147.0228562061483615 ) ) ;
#96508 = CARTESIAN_POINT ( 'NONE',  ( -12.40397477760000022, 1434.420140970890088, 149.9806264060980254 ) ) ;
#96509 = CARTESIAN_POINT ( 'NONE',  ( -5.303775421610000151, 1508.737782198590139, 220.0395200587989848 ) ) ;
#96511 = CARTESIAN_POINT ( 'NONE',  ( -3.180365954810094209, 1370.226539215819685, 208.0370721656823321 ) ) ;
#96510 = CARTESIAN_POINT ( 'NONE',  ( -0.6774325393469999845, 1465.095555782530027, 238.0673157071979915 ) ) ;
#96512 = B_SPLINE_SURFACE_WITH_KNOTS ( 'NONE', 5, 5, ( 
 ( #19894, #45135, #69788, #86003, #54097, #52425, #88225, #86552, #71465 ),
 ( #17664, #51865, #96062, #69225, #36162, #103336, #53534, #60835, #2030 ),
 ( #44016, #70347, #1460, #35597, #87109, #87678, #44568, #78714, #10963 ),
 ( #89865, #82005, #4753, #5310, #31056, #89316, #13134, #72006, #47868 ),
 ( #20987, #12612, #4220, #97165, #37820, #46245, #107218, #20436, #106122 ),
 ( #64696, #72530, #30506, #56272, #98814, #80375, #97716, #65237, #29396 ) ),
 .UNSPECIFIED., .F., .F., .F.,
 ( 6, 6 ),
 ( 6, 3, 6 ),
 ( 25.26541776610000056, 42.22156255719999507 ),
 ( -1.734723475979999901E-18, 1.000000000000000000, 2.000000000000000000 ),
 .UNSPECIFIED. ) ;
#96513 = CARTESIAN_POINT ( 'NONE',  ( 7.330554133425000174, 1516.857992118400034, 216.4511490482170188 ) ) ;
#96514 = CARTESIAN_POINT ( 'NONE',  ( 0.8923934389429990510, 1469.297510594290088, 216.3874288503389778 ) ) ;
#96515 = CARTESIAN_POINT ( 'NONE',  ( 6.092700134410669932, 1510.714321716100130, 216.6162777139399793 ) ) ;
#96517 = EDGE_CURVE ( 'NONE', #65641, #31476, #1269, .T. ) ;
#96516 = CARTESIAN_POINT ( 'NONE',  ( -11.81780673814840021, 1517.151704408390060, 222.7166774759110126 ) ) ;
#96518 = CARTESIAN_POINT ( 'NONE',  ( 3.267603515704999850, 1516.858171774179937, 212.3749871074670068 ) ) ;
#96519 = EDGE_CURVE ( 'NONE', #2979, #73174, #13354, .T. ) ;
#96520 = CARTESIAN_POINT ( 'NONE',  ( 4.329448802989709577, 1515.064791341159889, 211.4517443316900085 ) ) ;
#96521 = CARTESIAN_POINT ( 'NONE',  ( -4.978441812830840085, 1483.044991982689908, 199.7126697438380063 ) ) ;
#96523 = ORIENTED_EDGE ( 'NONE', *, *, #34948, .T. ) ;
#96522 = CARTESIAN_POINT ( 'NONE',  ( -82.65821105559999182, 1389.340475723369991, 302.6007231854590032 ) ) ;
#96524 = CARTESIAN_POINT ( 'NONE',  ( -0.5624690339869999889, 1416.828040475229955, 227.7677324846980014 ) ) ;
#96525 = AXIS2_PLACEMENT_3D ( 'NONE', #36233, #22012, #44650 ) ;
#96526 = CARTESIAN_POINT ( 'NONE',  ( 9.325404908590000375, 1464.388850156630042, 238.2842644183980099 ) ) ;
#96527 = EDGE_CURVE ( 'NONE', #74353, #45174, #5243, .T. ) ;
#96528 = CARTESIAN_POINT ( 'NONE',  ( -11.52225187220090774, 1489.339478244986822, 213.1483457362718070 ) ) ;
#96529 = CARTESIAN_POINT ( 'NONE',  ( -14.21441912100000060, 1415.677402202029953, 204.5785383627490148 ) ) ;
#96530 = EDGE_CURVE ( 'NONE', #20210, #97770, #105939, .T. ) ;
#96531 = CARTESIAN_POINT ( 'NONE',  ( 2.192264041240000072, 1411.750906532329964, 231.9235146910980063 ) ) ;
#96532 = CARTESIAN_POINT ( 'NONE',  ( -18.61729373430000223, 1457.059787195529907, 228.1786572008979874 ) ) ;
#96534 = CARTESIAN_POINT ( 'NONE',  ( 5.359824864149300261, 1422.430743802070083, 146.5258976672799918 ) ) ;
#96533 = CARTESIAN_POINT ( 'NONE',  ( -23.33460350828938346, 1411.088256419169738, 205.7888481793357585 ) ) ;
#96535 = CARTESIAN_POINT ( 'NONE',  ( -9.077189760424749565, 1449.419093657679923, 210.4763515235329976 ) ) ;
#96536 = CARTESIAN_POINT ( 'NONE',  ( -105.9035083438030114, 1380.145576709830038, 307.7816103815599718 ) ) ;
#96537 = ORIENTED_EDGE ( 'NONE', *, *, #4136, .T. ) ;
#96538 = CARTESIAN_POINT ( 'NONE',  ( 6.937338745574999521, 1516.706638732659940, 204.5037262658370025 ) ) ;
#96539 = CARTESIAN_POINT ( 'NONE',  ( 0.7785906040469999789, 1405.721630737029955, 267.8537809838979911 ) ) ;
#96540 = CARTESIAN_POINT ( 'NONE',  ( -0.008286608719400527859, 1515.284302758789863, 213.4455463337289984 ) ) ;
#96541 = CARTESIAN_POINT ( 'NONE',  ( 40.68248255500660093, 1450.744721969779903, 269.6225847687520059 ) ) ;
#96542 = CARTESIAN_POINT ( 'NONE',  ( 2.478110446250000098, 1439.827425895250144, 157.7784414222979876 ) ) ;
#96543 = EDGE_CURVE ( 'NONE', #72135, #82048, #70739, .T. ) ;
#96544 = CARTESIAN_POINT ( 'NONE',  ( -27.42679497377470099, 1448.207341916110181, 136.8613450941129770 ) ) ;
#96545 = CARTESIAN_POINT ( 'NONE',  ( -43.31543451723249660, 1440.913060408729962, 263.5607854574880093 ) ) ;
#96546 = AXIS2_PLACEMENT_3D ( 'NONE', #67984, #92052, #22601 ) ;
#96547 = CARTESIAN_POINT ( 'NONE',  ( -25.89815699820000106, 1448.079688286479950, 137.6494510301980085 ) ) ;
#96548 = CARTESIAN_POINT ( 'NONE',  ( 2.366976281752488198, 1449.615526741430131, 154.4348212163478706 ) ) ;
#96549 = DIRECTION ( 'NONE',  ( 0.000000000000000000, 0.9989884989440152019, -0.04496642055560280682 ) ) ;
#96550 = CARTESIAN_POINT ( 'NONE',  ( 13.73040295794826626, 1517.051704408389924, 227.6346699037790984 ) ) ;
#96551 = CARTESIAN_POINT ( 'NONE',  ( -21.64985223704988115, 1524.547395018738143, 183.5513639746648664 ) ) ;
#96552 = CARTESIAN_POINT ( 'NONE',  ( 0.8350686643532192477, 1524.382868172863937, 240.9330574173806951 ) ) ;
#96553 = ADVANCED_FACE ( 'NONE', ( #56073 ), #16331, .F. ) ;
#96555 = ORIENTED_EDGE ( 'NONE', *, *, #93352, .F. ) ;
#96554 = B_SPLINE_CURVE_WITH_KNOTS ( 'NONE', 3,
 ( #43760, #77912, #70647, #78466, #104212, #61686, #95809, #28049, #53280, #104764, #62239, #20733, #82313, #97999, #57136, #5049, #48175, #22371, #99092, #56020, #56571, #73924, #5611, #13427, #108053, #39194, #31349, #91263, #21269, #47617, #3981, #65533, #98552, #14542, #97464 ),
 .UNSPECIFIED., .F., .F.,
 ( 4, 2, 2, 1, 1, 1, 2, 2, 2, 2, 1, 1, 1, 2, 2, 2, 2, 1, 2, 2, 4 ),
 ( 0.000000000000000000, 0.1249999999977491338, 0.1874999999966215636, 0.2187499999960577646, 0.2343749999957791263, 0.2421874999956387942, 0.2460937499956126484, 0.2499999999955865304, 0.3749999999950853757, 0.4374999999947900009, 0.4687499999946407869, 0.4843749999946093676, 0.4921874999945921592, 0.4960937499945835549, 0.4999999999945750062, 0.6249999999958929520, 0.6874999999965575315, 0.7187499999968445241, 0.7343749999969880760, 0.7499999999971316278, 1.000000000000000000 ),
 .UNSPECIFIED. ) ;
#96556 = AXIS2_PLACEMENT_3D ( 'NONE', #77305, #9527, #25207 ) ;
#96557 = CARTESIAN_POINT ( 'NONE',  ( 0.4274149980285910089, 1409.096032488900164, 185.6227922226819942 ) ) ;
#96558 = DIRECTION ( 'NONE',  ( -0.000000000000000000, -1.000000000000000000, -0.000000000000000000 ) ) ;
#96559 = CARTESIAN_POINT ( 'NONE',  ( 10.44087869485973030, 1522.051704408389924, 212.8912867333128531 ) ) ;
#96560 = CARTESIAN_POINT ( 'NONE',  ( -0.1075335950709999933, 1475.759805456229969, 269.0456997844980265 ) ) ;
#96561 = CARTESIAN_POINT ( 'NONE',  ( -27.52167012590000184, 1451.951932214330100, 134.9033768147980084 ) ) ;
#96562 = CARTESIAN_POINT ( 'NONE',  ( -28.56957206459999909, 1509.608813672329916, 210.5224072855680220 ) ) ;
#96563 = CARTESIAN_POINT ( 'NONE',  ( -3.507940209892664196, 1448.288539702621165, 184.8766609435331532 ) ) ;
#96564 = CARTESIAN_POINT ( 'NONE',  ( -22.64763560905369744, 1384.853897193610010, 222.2275427940429893 ) ) ;
#96565 = VECTOR ( 'NONE', #24106, 1000.000000000000000 ) ;
#96566 = CARTESIAN_POINT ( 'NONE',  ( -18.94857910520000033, 1416.535385209630022, 207.9974517727780210 ) ) ;
#96567 = CARTESIAN_POINT ( 'NONE',  ( -9.383290498310000061, 1483.074069049089985, 203.0916503736390268 ) ) ;
#96568 = CARTESIAN_POINT ( 'NONE',  ( 26.15004714006070330, 1436.377686502539973, 136.8027247401129785 ) ) ;
#96569 = CARTESIAN_POINT ( 'NONE',  ( -10.32233395612670002, 1396.273524232049795, 213.1164902434229873 ) ) ;
#96570 = CARTESIAN_POINT ( 'NONE',  ( -15.03569022279999956, 1422.461937768830012, 228.7610668756979919 ) ) ;
#96571 = CARTESIAN_POINT ( 'NONE',  ( -16.65433881542789862, 1409.742294580739781, 225.7750875776860369 ) ) ;
#96572 = CARTESIAN_POINT ( 'NONE',  ( 22.52609212299890018, 1509.699688857919909, 227.3081665486540146 ) ) ;
#96573 = ORIENTED_EDGE ( 'NONE', *, *, #91097, .T. ) ;
#96574 = ADVANCED_FACE ( 'NONE', ( #80170 ), #82394, .T. ) ;
#96575 = CARTESIAN_POINT ( 'NONE',  ( -19.23853081770000273, 1466.576780668189940, 213.8528554934590034 ) ) ;
#96576 = CARTESIAN_POINT ( 'NONE',  ( -15.77825334036446492, 1415.905193579931620, 209.0522866884972188 ) ) ;
#96577 = CARTESIAN_POINT ( 'NONE',  ( -4.987275435840000881, 1510.323409146890071, 216.8373829782190114 ) ) ;
#96579 = CARTESIAN_POINT ( 'NONE',  ( -9.972556032338060206, 1439.430100340180161, 208.5509081778830023 ) ) ;
#96578 = CARTESIAN_POINT ( 'NONE',  ( 11.41497667239999991, 1426.868608979929832, 121.0051946870979975 ) ) ;
#96580 = DIRECTION ( 'NONE',  ( 1.000000000000000000, 0.000000000000000000, 0.000000000000000000 ) ) ;
#96581 = CARTESIAN_POINT ( 'NONE',  ( -12.58289157959999827, 1379.610106932609824, 209.8104170840169900 ) ) ;
#96582 = VECTOR ( 'NONE', #20086, 1000.000000000000000 ) ;
#96583 = CARTESIAN_POINT ( 'NONE',  ( -6.554764199395000546, 1516.786099423779888, 201.4062207291269999 ) ) ;
#96584 = CARTESIAN_POINT ( 'NONE',  ( 7.603387035110000802, 1425.782375950509959, 212.0439570241190097 ) ) ;
#96585 = DIRECTION ( 'NONE',  ( -0.000000000000000000, -1.000000000000000000, -0.000000000000000000 ) ) ;
#96586 = CARTESIAN_POINT ( 'NONE',  ( 2.343685733500000090, 1507.684322289930151, 181.2031450514980122 ) ) ;
#96587 = CARTESIAN_POINT ( 'NONE',  ( 7.780733067925000412, 1512.320675624280057, 206.2908607184970151 ) ) ;
#96588 = CARTESIAN_POINT ( 'NONE',  ( -82.87519116838579691, 1378.248460717899889, 300.2215825002689940 ) ) ;
#96589 = B_SPLINE_SURFACE_WITH_KNOTS ( 'NONE', 5, 5, ( 
 ( #22904, #64408, #13405, #81177, #90123, #30218 ),
 ( #100193, #14518, #73904, #82832, #72802, #99070 ),
 ( #6124, #4493, #15059, #21799, #97974, #108593 ),
 ( #90678, #73346, #40280, #22349, #74465, #91782 ),
 ( #39170, #31880, #57669, #81718, #31327, #56550 ),
 ( #13964, #98531, #108030, #55999, #106929, #82290 ) ),
 .UNSPECIFIED., .F., .F., .F.,
 ( 6, 6 ),
 ( 6, 6 ),
 ( 4.250940516431700011, 7.082035122218299783 ),
 ( -9.670478295150139691E-06, 0.5000000000000000000 ),
 .UNSPECIFIED. ) ;
#96590 = CARTESIAN_POINT ( 'NONE',  ( 8.106045534377265938, 1365.012046367625999, 208.3718459617061285 ) ) ;
#96592 = ORIENTED_EDGE ( 'NONE', *, *, #28400, .F. ) ;
#96591 = CARTESIAN_POINT ( 'NONE',  ( -3.347801439296150150, 1523.382868172864164, 242.0893193391992497 ) ) ;
#96593 = VERTEX_POINT ( 'NONE', #92404 ) ;
#96594 = CARTESIAN_POINT ( 'NONE',  ( -41.14953178369999875, 1443.861422506349982, 136.9341304683979956 ) ) ;
#96595 = CARTESIAN_POINT ( 'NONE',  ( 1.173613536004610047, 1490.965225197780001, 236.3431785357499848 ) ) ;
#96596 = DIRECTION ( 'NONE',  ( 0.01668530547205149608, 0.7071067811868640973, -0.7069098956591685079 ) ) ;
#96597 = CARTESIAN_POINT ( 'NONE',  ( -7.888956606115001158, 1511.220390575160081, 213.9483244531670039 ) ) ;
#96599 = CARTESIAN_POINT ( 'NONE',  ( -2.762672730830000312, 1485.977692311530063, 182.1582024225980092 ) ) ;
#96598 = CARTESIAN_POINT ( 'NONE',  ( -8.537909486209999343, 1383.668034227369844, 218.4909987399589966 ) ) ;
#96600 = AXIS2_PLACEMENT_3D ( 'NONE', #69070, #27049, #15843 ) ;
#96601 = CARTESIAN_POINT ( 'NONE',  ( 8.181958942834999249, 1517.051704408389924, 212.1568108385370124 ) ) ;
#96602 = CARTESIAN_POINT ( 'NONE',  ( 11.41288121311350068, 1427.618783885739958, 209.6357582931089780 ) ) ;
#96603 = FACE_OUTER_BOUND ( 'NONE', #69467, .T. ) ;
#96604 = LINE ( 'NONE', #63043, #70157 ) ;
#96605 = CARTESIAN_POINT ( 'NONE',  ( 8.233125739818301980, 1396.200567475059870, 216.4997438228709825 ) ) ;
#96606 = CARTESIAN_POINT ( 'NONE',  ( 3.387628330345790140, 1408.970309133350156, 194.7468131480869999 ) ) ;
#96607 = CARTESIAN_POINT ( 'NONE',  ( 5.344396406567219923E-05, 1406.506757891989992, 269.4987579911870057 ) ) ;
#96608 = CARTESIAN_POINT ( 'NONE',  ( 40.70526341139999715, 1444.199266155760142, 137.0833901977979963 ) ) ;
#96609 = VERTEX_POINT ( 'NONE', #76723 ) ;
#96610 = CARTESIAN_POINT ( 'NONE',  ( -11.57581721210000048, 1432.288378091340064, 151.1967356772979940 ) ) ;
#96611 = CARTESIAN_POINT ( 'NONE',  ( 13.12363690099999936, 1441.384603101129869, 188.9419487780980091 ) ) ;
#96612 = VERTEX_POINT ( 'NONE', #41479 ) ;
#96613 = ORIENTED_EDGE ( 'NONE', *, *, #65808, .T. ) ;
#96614 = EDGE_CURVE ( 'NONE', #34413, #60257, #24442, .T. ) ;
#96615 = CARTESIAN_POINT ( 'NONE',  ( -3.720950966109999758, 1454.058771263989911, 199.3235536337890039 ) ) ;
#96616 = CARTESIAN_POINT ( 'NONE',  ( -3.982247585420000124, 1360.759224656429978, 207.6218459616989946 ) ) ;
#96617 = EDGE_CURVE ( 'NONE', #49504, #75704, #10161, .T. ) ;
#96618 = CARTESIAN_POINT ( 'NONE',  ( 7.331812085974999782, 1516.906641539930206, 215.6759973964769870 ) ) ;
#96619 = CARTESIAN_POINT ( 'NONE',  ( 4.495269857704999872, 1510.967342883699985, 216.7778746379670167 ) ) ;
#96620 = ORIENTED_EDGE ( 'NONE', *, *, #85617, .F. ) ;
#96621 = CARTESIAN_POINT ( 'NONE',  ( -17.71193100849139768, 1517.151704408390060, 221.5709757781449980 ) ) ;
#96622 = CARTESIAN_POINT ( 'NONE',  ( -84.75344743939999148, 1374.600296256490083, 297.4377104198590018 ) ) ;
#96623 = CARTESIAN_POINT ( 'NONE',  ( -106.3928623033740024, 1378.913060387289988, 302.0630715194479876 ) ) ;
#96624 = CARTESIAN_POINT ( 'NONE',  ( 6.936398355645000180, 1516.667393516340098, 205.0850970932970085 ) ) ;
#96625 = VECTOR ( 'NONE', #6085, 1000.000000000000000 ) ;
#96626 = CARTESIAN_POINT ( 'NONE',  ( -12.23218726772509868, 1490.223478903719979, 209.6887218936990109 ) ) ;
#96627 = B_SPLINE_SURFACE_WITH_KNOTS ( 'NONE', 5, 5, ( 
 ( #24366, #859, #34986, #50158, #33317, #67513 ),
 ( #94327, #50690, #83735, #101615, #76439, #25462 ),
 ( #33878, #92137, #34440, #17605, #59110, #15412 ),
 ( #49603, #84821, #110592, #59657, #93765, #17043 ),
 ( #8668, #102717, #60208, #11456, #88717, #28246 ),
 ( #53471, #71949, #62436, #20377, #2527, #18174 ),
 ( #35537, #45632, #96562, #11997, #106061, #71399 ),
 ( #9786, #46181, #95454, #37757, #79771, #3078 ),
 ( #19834, #54039, #60776, #104956, #1970, #27150 ) ),
 .UNSPECIFIED., .F., .F., .F.,
 ( 6, 3, 6 ),
 ( 6, 6 ),
 ( 1.123321935180000120, 3.227816461920000268, 6.189575054660000575 ),
 ( 0.000000000000000000, 2.000000000000000000 ),
 .UNSPECIFIED. ) ;
#96628 = CARTESIAN_POINT ( 'NONE',  ( -113.4000000000000057, 1385.251674955540238, 297.2379167808589955 ) ) ;
#96629 = CYLINDRICAL_SURFACE ( 'NONE', #9670, 2.000000000000003109 ) ;
#96630 = CARTESIAN_POINT ( 'NONE',  ( -8.142670621130001507, 1409.364027242329939, 229.9797211375979771 ) ) ;
#96631 = AXIS2_PLACEMENT_3D ( 'NONE', #62188, #88470, #19593 ) ;
#96633 = ORIENTED_EDGE ( 'NONE', *, *, #3780, .F. ) ;
#96632 = CARTESIAN_POINT ( 'NONE',  ( -5.691423665590000347, 1446.578623823169892, 184.8819865835980067 ) ) ;
#96634 = CARTESIAN_POINT ( 'NONE',  ( 5.940539708128936169, 1521.951704408389787, 189.0391861795680768 ) ) ;
#96635 = CARTESIAN_POINT ( 'NONE',  ( 11.36600848118518137, 1425.633665734278793, 139.1352670123650341 ) ) ;
#96636 = CARTESIAN_POINT ( 'NONE',  ( -17.46768317430000295, 1384.870099884450156, 219.9576826991589940 ) ) ;
#96637 = CARTESIAN_POINT ( 'NONE',  ( 16.27172383310000114, 1476.104910058290216, 222.3698031616989965 ) ) ;
#96638 = EDGE_CURVE ( 'NONE', #101763, #101515, #84566, .T. ) ;
#96639 = CARTESIAN_POINT ( 'NONE',  ( 41.44433335099289195, 1427.311881607490022, 269.9656476501689326 ) ) ;
#96641 = CARTESIAN_POINT ( 'NONE',  ( 4.042417777704999438, 1516.904492006980036, 212.5700528489170154 ) ) ;
#96640 = VECTOR ( 'NONE', #85995, 1000.000000000000000 ) ;
#96642 = CARTESIAN_POINT ( 'NONE',  ( -67.92939999230000581, 1379.746255314009886, 278.2862461588590008 ) ) ;
#96643 = CARTESIAN_POINT ( 'NONE',  ( 0.006933964948642189902, 1508.593138409394896, 238.1018653665563534 ) ) ;
#96644 = CARTESIAN_POINT ( 'NONE',  ( 9.305981717835429379, 1425.677315260519890, 193.6786577638000040 ) ) ;
#96646 = EDGE_CURVE ( 'NONE', #44905, #20112, #72946, .T. ) ;
#96645 = CARTESIAN_POINT ( 'NONE',  ( 20.88760228492832027, 1411.001959330801583, 199.6026542048159627 ) ) ;
#96647 = CARTESIAN_POINT ( 'NONE',  ( -6.556851034704999748, 1516.939568781210028, 209.1335575761840175 ) ) ;
#96648 = ORIENTED_EDGE ( 'NONE', *, *, #1576, .T. ) ;
#96649 = CARTESIAN_POINT ( 'NONE',  ( 3.203789175851970288E-09, 1424.294192408320214, 227.6053815985079893 ) ) ;
#96650 = CARTESIAN_POINT ( 'NONE',  ( -4.152492679409998999, 1417.909732061129944, 232.5032652226979906 ) ) ;
#96651 = CARTESIAN_POINT ( 'NONE',  ( -54.13172275060000516, 1384.971233722779971, 270.3676613534589706 ) ) ;
#96652 = EDGE_CURVE ( 'NONE', #10270, #91917, #4794, .T. ) ;
#96653 = EDGE_LOOP ( 'NONE', ( #62368, #56336, #25114, #33228 ) ) ;
#96654 = CARTESIAN_POINT ( 'NONE',  ( -22.28602175699319687, 1385.267146508269889, 222.0073600989599925 ) ) ;
#96655 = DIRECTION ( 'NONE',  ( 0.7384854939285241393, 0.000000000000000000, -0.6742693640208961003 ) ) ;
#96656 = CARTESIAN_POINT ( 'NONE',  ( 16.98147855194190470, 1478.708851325969817, 229.6812432133669972 ) ) ;
#96657 = CARTESIAN_POINT ( 'NONE',  ( 20.06869819519999965, 1507.849569125829930, 189.2236336047979819 ) ) ;
#96658 = CARTESIAN_POINT ( 'NONE',  ( -14.88313348660000024, 1507.493288264930015, 229.7103749383979903 ) ) ;
#96659 = CARTESIAN_POINT ( 'NONE',  ( -0.5238577372009999289, 1409.870336964829903, 233.1507187614980126 ) ) ;
#96660 = LINE ( 'NONE', #105055, #18246 ) ;
#96661 = EDGE_CURVE ( 'NONE', #61894, #67570, #83433, .T. ) ;
#96663 = CARTESIAN_POINT ( 'NONE',  ( -3.889576884872586682, 1455.763526873609408, 200.4986044836267922 ) ) ;
#96662 = CARTESIAN_POINT ( 'NONE',  ( 2.294209629405000062, 1516.603620185149794, 214.8927295341169952 ) ) ;
#96664 = CARTESIAN_POINT ( 'NONE',  ( 19.11260941699999805, 1509.007777225030168, 188.0781932532979965 ) ) ;
#96665 = CARTESIAN_POINT ( 'NONE',  ( 10.04074129076350097, 1469.832169069019983, 209.8604891245049942 ) ) ;
#96666 = ORIENTED_EDGE ( 'NONE', *, *, #106740, .F. ) ;
#96667 = CARTESIAN_POINT ( 'NONE',  ( 5.779627054084999216, 1516.977993847330026, 201.4011957967969977 ) ) ;
#96668 = CARTESIAN_POINT ( 'NONE',  ( -7.105427357599999217E-15, 1418.913060387330006, 172.2701767054979882 ) ) ;
#96669 = ORIENTED_EDGE ( 'NONE', *, *, #92115, .F. ) ;
#96670 = CARTESIAN_POINT ( 'NONE',  ( 11.60004869885204570, 1426.698742054508330, 134.5125446557153168 ) ) ;
#96671 = ADVANCED_FACE ( 'NONE', ( #23554 ), #35797, .F. ) ;
#96672 = CARTESIAN_POINT ( 'NONE',  ( -4.155669664704369382, 1439.704322410719897, 185.4969487652249995 ) ) ;
#96673 = CARTESIAN_POINT ( 'NONE',  ( 19.00254649709379606, 1416.818673806565812, 210.3102538504050472 ) ) ;
#96674 = CARTESIAN_POINT ( 'NONE',  ( 3.074701863640000088, 1441.333177043090018, 218.5515105840890158 ) ) ;
#96675 = CARTESIAN_POINT ( 'NONE',  ( -30.99338347248506409, 1526.382868172863937, 199.8717226395886257 ) ) ;
#96676 = DIRECTION ( 'NONE',  ( -1.836970198721029688E-16, -1.000000000000000000, -8.835242138475329394E-33 ) ) ;
#96677 = VECTOR ( 'NONE', #19368, 1000.000000000000000 ) ;
#96678 = CARTESIAN_POINT ( 'NONE',  ( 18.45314936670000350, 1415.553739809529816, 210.3484166225879903 ) ) ;
#96679 = CARTESIAN_POINT ( 'NONE',  ( -18.47206917109999935, 1424.236406309129961, 225.0732636529979800 ) ) ;
#96680 = CARTESIAN_POINT ( 'NONE',  ( -20.86574809109999862, 1435.370602116739974, 143.5212114325979940 ) ) ;
#96681 = CARTESIAN_POINT ( 'NONE',  ( -4.139067334555820210, 1464.629524841519924, 198.9111649813920053 ) ) ;
#96682 = CARTESIAN_POINT ( 'NONE',  ( -29.00779973304124937, 1526.382868172863937, 217.2942086403127178 ) ) ;
#96684 = CARTESIAN_POINT ( 'NONE',  ( -6.954065720117950100, 1519.551704408389924, 183.5505540514350002 ) ) ;
#96683 = DIRECTION ( 'NONE',  ( -0.8090169943749507819, 0.000000000000000000, -0.5877852522924685852 ) ) ;
#96685 = EDGE_CURVE ( 'NONE', #40573, #41312, #87050, .T. ) ;
#96686 = CARTESIAN_POINT ( 'NONE',  ( 2.127574403376955026, 1524.244163922423013, 244.5104606571598538 ) ) ;
#96687 = ORIENTED_EDGE ( 'NONE', *, *, #7202, .T. ) ;
#96688 = CARTESIAN_POINT ( 'NONE',  ( -7.737321863080000028, 1508.477796734990079, 219.4085941960990169 ) ) ;
#96689 = CARTESIAN_POINT ( 'NONE',  ( 22.57618181349999986, 1411.056460407229906, 206.4508663819080141 ) ) ;
#96690 = EDGE_CURVE ( 'NONE', #71185, #24039, #38767, .T. ) ;
#96691 = CARTESIAN_POINT ( 'NONE',  ( -11.92876424382160039, 1433.442611883628388, 149.9100498133672943 ) ) ;
#96692 = CARTESIAN_POINT ( 'NONE',  ( -1.637262557069999902, 1483.893433194890122, 198.5669152071990027 ) ) ;
#96693 = CARTESIAN_POINT ( 'NONE',  ( -18.61766197840000103, 1509.563203468529991, 231.0956455985979972 ) ) ;
#96694 = DIRECTION ( 'NONE',  ( -0.000000000000000000, -1.000000000000000000, -0.000000000000000000 ) ) ;
#96695 = CARTESIAN_POINT ( 'NONE',  ( 15.96958168569999970, 1519.913060387329779, 225.0914276473980067 ) ) ;
#96696 = DIRECTION ( 'NONE',  ( 0.8672669759446636206, 0.000000000000000000, 0.4978433412588729734 ) ) ;
#96697 = CARTESIAN_POINT ( 'NONE',  ( -11.32770374180210027, 1470.496536099929926, 210.3424180843229863 ) ) ;
#96698 = ADVANCED_FACE ( 'NONE', ( #70017 ), #43681, .T. ) ;
#96699 = CARTESIAN_POINT ( 'NONE',  ( -9.247716023661459062, 1489.608888726200121, 215.3272058384319791 ) ) ;
#96700 = CARTESIAN_POINT ( 'NONE',  ( -18.92739421348260009, 1503.346059615760169, 222.1981729787850099 ) ) ;
#96701 = CARTESIAN_POINT ( 'NONE',  ( -80.60779555424529974, 1383.776547664450163, 304.0453241665860560 ) ) ;
#96702 = CARTESIAN_POINT ( 'NONE',  ( -108.9251951694480027, 1383.742096774909896, 311.0727769249569974 ) ) ;
#96703 = CARTESIAN_POINT ( 'NONE',  ( -5.114744891480448530, 1391.870385291815182, 214.6056989427710562 ) ) ;
#96704 = CARTESIAN_POINT ( 'NONE',  ( 4.271857500090000315, 1429.250640823790036, 216.3852677031590019 ) ) ;
#96706 = ORIENTED_EDGE ( 'NONE', *, *, #22928, .F. ) ;
#96705 = LINE ( 'NONE', #54170, #4971 ) ;
#96707 = VECTOR ( 'NONE', #33367, 1000.000000000000000 ) ;
#96708 = CARTESIAN_POINT ( 'NONE',  ( -92.45138929590000032, 1381.911264019279770, 294.9202873905589968 ) ) ;
#96709 = CARTESIAN_POINT ( 'NONE',  ( -0.7603233172752421609, 1417.366985054399720, 235.2447777849411636 ) ) ;
#96710 = ORIENTED_EDGE ( 'NONE', *, *, #95406, .T. ) ;
#96711 = EDGE_LOOP ( 'NONE', ( #28100, #95312, #90468, #64691, #73229 ) ) ;
#96712 = CARTESIAN_POINT ( 'NONE',  ( -7.835191567469999896, 1492.420539004689999, 209.1441751587790066 ) ) ;
#96713 = CARTESIAN_POINT ( 'NONE',  ( -109.3493624629999914, 1384.903260851859841, 297.1385571428590424 ) ) ;
#96714 = CARTESIAN_POINT ( 'NONE',  ( 13.25931364579099814, 1443.184772872878057, 169.3835527203846425 ) ) ;
#96716 = CARTESIAN_POINT ( 'NONE',  ( -7.132053279490000008, 1475.995192518030080, 267.2558860548979851 ) ) ;
#96715 = CARTESIAN_POINT ( 'NONE',  ( 28.87453514628182205, 1418.771342272429820, 269.4592184128185863 ) ) ;
#96717 = CARTESIAN_POINT ( 'NONE',  ( 9.022884344052069849, 1436.030640010990055, 209.0591187573379841 ) ) ;
#96718 = CARTESIAN_POINT ( 'NONE',  ( -109.6260819770000126, 1384.887353564230125, 297.0994507507589901 ) ) ;
#96719 = CARTESIAN_POINT ( 'NONE',  ( -19.16475049499999983, 1485.565701775930165, 189.6829647518980266 ) ) ;
#96720 = CARTESIAN_POINT ( 'NONE',  ( 12.14561940090000114, 1409.337194763229718, 191.0894207074980216 ) ) ;
#96721 = CARTESIAN_POINT ( 'NONE',  ( 5.013886338179999846, 1423.124965184129906, 184.3797681692980177 ) ) ;
#96722 = CARTESIAN_POINT ( 'NONE',  ( -1.403832662453629920, 1515.079617817460075, 213.4509065325290180 ) ) ;
#96723 = CARTESIAN_POINT ( 'NONE',  ( -20.70484064406422320, 1525.907212628473644, 185.0411015109855839 ) ) ;
#96724 = CARTESIAN_POINT ( 'NONE',  ( 1.925297170580940076, 1519.551704408389924, 230.6853930747409720 ) ) ;
#96725 = AXIS2_PLACEMENT_3D ( 'NONE', #64972, #99087, #39758 ) ;
#96726 = CARTESIAN_POINT ( 'NONE',  ( -15.30199789809999977, 1451.561028161330114, 149.9720795101980002 ) ) ;
#96727 = EDGE_CURVE ( 'NONE', #64454, #24504, #81671, .T. ) ;
#96729 = ORIENTED_EDGE ( 'NONE', *, *, #76798, .T. ) ;
#96728 = CARTESIAN_POINT ( 'NONE',  ( 7.722580314274999580, 1517.051704408389924, 210.6910072246569996 ) ) ;
#96730 = ORIENTED_EDGE ( 'NONE', *, *, #82212, .F. ) ;
#96731 = CARTESIAN_POINT ( 'NONE',  ( -2.409586283469999923, 1426.663880916129983, 144.1938086916980239 ) ) ;
#96732 = EDGE_CURVE ( 'NONE', #47285, #60389, #94064, .T. ) ;
#96733 = CARTESIAN_POINT ( 'NONE',  ( -22.14393498469999955, 1486.559014183590079, 217.4067828909289801 ) ) ;
#96734 = CARTESIAN_POINT ( 'NONE',  ( -25.61285747580000205, 1467.494200632129832, 270.3573890266980015 ) ) ;
#96735 = CARTESIAN_POINT ( 'NONE',  ( -23.76373184819366813, 1436.064358996370402, 211.6811140537201652 ) ) ;
#96737 = VECTOR ( 'NONE', #103488, 1000.000000000000114 ) ;
#96736 = CARTESIAN_POINT ( 'NONE',  ( 3.282394052629999948, 1438.199601172570055, 155.5836490844979778 ) ) ;
#96738 = CARTESIAN_POINT ( 'NONE',  ( -14.45760119950000089, 1463.281480820829984, 223.3430437907979922 ) ) ;
#96739 = CARTESIAN_POINT ( 'NONE',  ( 15.96958168569999970, 1519.913060387329779, 193.1522642759980215 ) ) ;
#96740 = CARTESIAN_POINT ( 'NONE',  ( -13.95121136070000034, 1421.607743136130011, 228.2237463402980211 ) ) ;
#96741 = VECTOR ( 'NONE', #22147, 1000.000000000000114 ) ;
#96742 = CARTESIAN_POINT ( 'NONE',  ( -9.442727158709999458, 1460.560438940789709, 211.9848800811889760 ) ) ;
#96743 = CARTESIAN_POINT ( 'NONE',  ( 10.63741388148666545, 1363.043374934216899, 210.6218459617030021 ) ) ;
#96744 = CARTESIAN_POINT ( 'NONE',  ( -45.08400256209149859, 1433.680806341129937, 266.7087657724729866 ) ) ;
#96745 = ORIENTED_EDGE ( 'NONE', *, *, #18526, .F. ) ;
#96746 = CARTESIAN_POINT ( 'NONE',  ( 31.23437356469435144, 1511.187213306747708, 195.3468678195113739 ) ) ;
#96747 = EDGE_LOOP ( 'NONE', ( #61633, #86764, #99705 ) ) ;
#96748 = CARTESIAN_POINT ( 'NONE',  ( -4.610079871555000430, 1516.713079096360161, 210.2553629353369899 ) ) ;
#96749 = EDGE_CURVE ( 'NONE', #86208, #234, #90710, .T. ) ;
#96750 = AXIS2_PLACEMENT_3D ( 'NONE', #57757, #7325, #59958 ) ;
#96751 = CARTESIAN_POINT ( 'NONE',  ( -9.593461995991589220, 1446.925636462349985, 212.1822515110659992 ) ) ;
#96752 = CARTESIAN_POINT ( 'NONE',  ( 12.78776258895000062, 1416.851343899079893, 222.7045348340550106 ) ) ;
#96753 = CARTESIAN_POINT ( 'NONE',  ( -14.95559069659999984, 1425.419646131229911, 190.0114300131980087 ) ) ;
#96754 = CARTESIAN_POINT ( 'NONE',  ( 15.90990255763500016, 1515.867682058960099, 193.9190501556669801 ) ) ;
#96755 = ORIENTED_EDGE ( 'NONE', *, *, #93209, .F. ) ;
#96756 = CARTESIAN_POINT ( 'NONE',  ( -2.622430729443011366, 1523.621879633029266, 176.0901726876731743 ) ) ;
#96757 = CARTESIAN_POINT ( 'NONE',  ( -2.291047527245000381, 1516.524310051880093, 201.4130759250869858 ) ) ;
#96758 = AXIS2_PLACEMENT_3D ( 'NONE', #19670, #9613, #45465 ) ;
#96759 = EDGE_CURVE ( 'NONE', #78937, #46370, #101398, .T. ) ;
#96760 = CARTESIAN_POINT ( 'NONE',  ( 9.585967232940001637, 1472.264498658589901, 214.5747525333089811 ) ) ;
#96761 = DIRECTION ( 'NONE',  ( 0.4090087482554177756, 1.419034154957278791E-15, -0.9125304618754029873 ) ) ;
#96762 = ORIENTED_EDGE ( 'NONE', *, *, #95837, .F. ) ;
#96763 = CARTESIAN_POINT ( 'NONE',  ( -16.31723503134719877, 1412.721052651110085, 269.3692194093940202 ) ) ;
#96764 = CARTESIAN_POINT ( 'NONE',  ( 3.447128460625000113, 1516.778853242349896, 207.9866608880570027 ) ) ;
#96765 = CARTESIAN_POINT ( 'NONE',  ( -27.68327768569999847, 1435.464602415119771, 135.2595507401980228 ) ) ;
#96766 = CARTESIAN_POINT ( 'NONE',  ( 8.616327664749301007, 1435.881562212750168, 207.7018527875740119 ) ) ;
#96767 = EDGE_CURVE ( 'NONE', #53387, #69529, #10606, .T. ) ;
#96769 = ORIENTED_EDGE ( 'NONE', *, *, #6359, .T. ) ;
#96768 = CARTESIAN_POINT ( 'NONE',  ( -8.292274593569779029, 1366.175860171049408, 207.6218459616988241 ) ) ;
#96770 = ORIENTED_EDGE ( 'NONE', *, *, #11981, .T. ) ;
#96771 = CARTESIAN_POINT ( 'NONE',  ( 45.63459694424612678, 1441.288710710889291, 268.9748222008650487 ) ) ;
#96772 = CARTESIAN_POINT ( 'NONE',  ( 3.114565223550959772, 1466.517051284160061, 219.7262097583810032 ) ) ;
#96773 = PLANE ( 'NONE',  #106522 ) ;
#96774 = CARTESIAN_POINT ( 'NONE',  ( 4.967684365510000255, 1469.890599266690060, 189.7939106698990201 ) ) ;
#96775 = CIRCLE ( 'NONE', #62848, 1.000000000000000888 ) ;
#96776 = CARTESIAN_POINT ( 'NONE',  ( -20.59848284610770008, 1506.575640312069936, 217.1340086378183400 ) ) ;
#96777 = CARTESIAN_POINT ( 'NONE',  ( -19.34575562749999733, 1435.773310684580110, 224.5584730475980280 ) ) ;
#96778 = CARTESIAN_POINT ( 'NONE',  ( -14.00912997540000049, 1416.839648771730026, 221.8523350237979912 ) ) ;
#96779 = CARTESIAN_POINT ( 'NONE',  ( 12.77426335350000031, 1416.547221146729953, 222.9124519587980160 ) ) ;
#96780 = CARTESIAN_POINT ( 'NONE',  ( 7.205930508499999831, 1446.348252743489866, 184.8949001284980227 ) ) ;
#96781 = CARTESIAN_POINT ( 'NONE',  ( 6.546302742015000398, 1516.577434278289957, 206.6347425125669872 ) ) ;
#96782 = ORIENTED_EDGE ( 'NONE', *, *, #108896, .T. ) ;
#96783 = CARTESIAN_POINT ( 'NONE',  ( 2.564080367290000328, 1443.257105434990081, 214.7475390850690076 ) ) ;
#96784 = CARTESIAN_POINT ( 'NONE',  ( 1.522490431809080169, 1455.721078906920184, 183.3572470959660166 ) ) ;
#96785 = ORIENTED_EDGE ( 'NONE', *, *, #42194, .T. ) ;
#96786 = DIRECTION ( 'NONE',  ( -1.755985294532469921E-16, 1.000000000000000000, -1.338183447452831989E-16 ) ) ;
#96787 = ADVANCED_FACE ( 'NONE', ( #54855 ), #63271, .T. ) ;
#96788 = CARTESIAN_POINT ( 'NONE',  ( 25.48798889943779855, 1450.979438871130014, 137.1176068765460059 ) ) ;
#96789 = CARTESIAN_POINT ( 'NONE',  ( 14.34604702270000054, 1416.547221147930031, 196.6758286521979926 ) ) ;
#96790 = CARTESIAN_POINT ( 'NONE',  ( -33.19360111489999809, 1388.470894590589978, 229.1017553306589889 ) ) ;
#96791 = CARTESIAN_POINT ( 'NONE',  ( 7.722580339391510229, 1517.051704402239920, 213.7119063846940037 ) ) ;
#96792 = CARTESIAN_POINT ( 'NONE',  ( 20.28790900150000098, 1410.981725563229929, 198.0270821811979829 ) ) ;
#96793 = CARTESIAN_POINT ( 'NONE',  ( 12.53380499169999851, 1445.052233488290085, 169.4755105685979970 ) ) ;
#96794 = CARTESIAN_POINT ( 'NONE',  ( 17.06446797460000298, 1409.673996215429952, 225.0967169420980269 ) ) ;
#96795 = CARTESIAN_POINT ( 'NONE',  ( -14.04885618097836897, 1379.586891663671850, 211.8295121144176676 ) ) ;
#96796 = CARTESIAN_POINT ( 'NONE',  ( 21.29509819372636059, 1454.121024500114800, 221.5516887311115966 ) ) ;
#96797 = ADVANCED_FACE ( 'NONE', ( #20653 ), #27803, .F. ) ;
#96798 = CARTESIAN_POINT ( 'NONE',  ( -11.39126005979999867, 1381.496251003520001, 216.9356158229890070 ) ) ;
#96799 = CARTESIAN_POINT ( 'NONE',  ( 0.01171160595180150039, 1516.939568781210028, 215.6786969668069958 ) ) ;
#96800 = CARTESIAN_POINT ( 'NONE',  ( 2.410659749415533071, 1525.163457223744217, 242.1267480251479753 ) ) ;
#96801 = ORIENTED_EDGE ( 'NONE', *, *, #44116, .T. ) ;
#96802 = DIRECTION ( 'NONE',  ( -0.6736849260863841948, 0.000000000000000000, 0.7390186874254148774 ) ) ;
#96803 = CARTESIAN_POINT ( 'NONE',  ( 22.69876404238873846, 1522.861859112239017, 236.8953202675596401 ) ) ;
#96804 = CARTESIAN_POINT ( 'NONE',  ( -0.5138428465688279489, 1410.035027812230055, 233.1323959473689911 ) ) ;
#96805 = EDGE_CURVE ( 'NONE', #67505, #45568, #65722, .T. ) ;
#96806 = CARTESIAN_POINT ( 'NONE',  ( -19.32547173205315971, 1508.392602783547318, 209.8687894484399408 ) ) ;
#96807 = CARTESIAN_POINT ( 'NONE',  ( -39.69692591273509663, 1446.534400439990122, 136.7156208858029913 ) ) ;
#96808 = CIRCLE ( 'NONE', #34127, 1.999999999999999556 ) ;
#96809 = CARTESIAN_POINT ( 'NONE',  ( -4.328546746085120134, 1515.099240016830208, 207.9973207389659819 ) ) ;
#96810 = CARTESIAN_POINT ( 'NONE',  ( -3.804422480509999982, 1458.952956304630106, 234.3916895958979865 ) ) ;
#96811 = DIRECTION ( 'NONE',  ( -0.6736849260863841948, 0.000000000000000000, 0.7390186874254148774 ) ) ;
#96812 = CARTESIAN_POINT ( 'NONE',  ( -12.31211413366879981, 1378.375898250180171, 209.7639663314890015 ) ) ;
#96813 = CARTESIAN_POINT ( 'NONE',  ( -0.5964932758231209498, 1474.173341595109832, 270.1376979220820544 ) ) ;
#96814 = CARTESIAN_POINT ( 'NONE',  ( -32.02808312589908013, 1522.382868172863937, 219.9649204700466782 ) ) ;
#96815 = CARTESIAN_POINT ( 'NONE',  ( 0.8350686643532192477, 1526.382868172863937, 240.9330574173806951 ) ) ;
#96816 = CARTESIAN_POINT ( 'NONE',  ( 9.378915144369848633, 1500.841300073399907, 202.4402467813089856 ) ) ;
#96817 = ORIENTED_EDGE ( 'NONE', *, *, #40476, .F. ) ;
#96818 = ADVANCED_FACE ( 'NONE', ( #64910 ), #79656, .T. ) ;
#96819 = B_SPLINE_CURVE_WITH_KNOTS ( 'NONE', 5,
 ( #85541, #93948, #25635, #25080, #51410, #50333 ),
 .UNSPECIFIED., .F., .F.,
 ( 6, 6 ),
 ( -1.999999605764219979, -2.592271335366547191E-07 ),
 .UNSPECIFIED. ) ;
#96820 = DIRECTION ( 'NONE',  ( -0.000000000000000000, -0.000000000000000000, -1.000000000000000000 ) ) ;
#96821 = CARTESIAN_POINT ( 'NONE',  ( 9.885290350402808457, 1462.702877345079969, 211.5948837706700090 ) ) ;
#96822 = CARTESIAN_POINT ( 'NONE',  ( -3.481446190449999811, 1485.993219827530083, 182.2119038017980017 ) ) ;
#96823 = VECTOR ( 'NONE', #48505, 1000.000000000000000 ) ;
#96824 = CARTESIAN_POINT ( 'NONE',  ( -1.430538850779999871, 1444.328264147990012, 199.1703828715889983 ) ) ;
#96825 = CARTESIAN_POINT ( 'NONE',  ( 2.627197941649999979, 1499.011965180429797, 235.6151326529979997 ) ) ;
#96826 = EDGE_CURVE ( 'NONE', #18369, #81651, #110746, .T. ) ;
#96827 = CARTESIAN_POINT ( 'NONE',  ( 24.79630737949999997, 1449.797614621719958, 213.3734452447980061 ) ) ;
#96828 = CARTESIAN_POINT ( 'NONE',  ( -15.97653678204605221, 1420.243090095628986, 209.7114017956471343 ) ) ;
#96829 = CARTESIAN_POINT ( 'NONE',  ( 4.363122647530000009, 1418.913060387330006, 172.2701767054979882 ) ) ;
#96830 = CARTESIAN_POINT ( 'NONE',  ( -21.32959704448400018, 1383.852165897360010, 221.3536186575369982 ) ) ;
#96831 = CARTESIAN_POINT ( 'NONE',  ( 19.74177095050000119, 1466.547268800929942, 224.7591543658979845 ) ) ;
#96832 = CARTESIAN_POINT ( 'NONE',  ( -16.37730547380552082, 1414.913060387329779, 208.0632427977511725 ) ) ;
#96834 =( BOUNDED_CURVE ( )  B_SPLINE_CURVE ( 3, ( #103963, #18837, #62563, #27260 ),
 .UNSPECIFIED., .F., .T. ) 
 B_SPLINE_CURVE_WITH_KNOTS ( ( 4, 4 ),
 ( 2.356690340185370047, 3.926801538374500300 ),
 .UNSPECIFIED. ) 
 CURVE ( )  GEOMETRIC_REPRESENTATION_ITEM ( )  RATIONAL_B_SPLINE_CURVE ( ( 1.000000000000000000, 0.8048993128225162552, 0.8048993128225162552, 1.000000000000000000 ) ) 
 REPRESENTATION_ITEM ( '' )  );
#96833 = FACE_OUTER_BOUND ( 'NONE', #36931, .T. ) ;
#96835 = CARTESIAN_POINT ( 'NONE',  ( -2.330134126678749418, 1515.492058413688255, 204.9833025705414116 ) ) ;
#96837 = ORIENTED_EDGE ( 'NONE', *, *, #61205, .T. ) ;
#96836 = CARTESIAN_POINT ( 'NONE',  ( 32.16776790210105474, 1524.538969332612623, 216.0987814432344578 ) ) ;
#96838 = LINE ( 'NONE', #68894, #87817 ) ;
#96839 = CIRCLE ( 'NONE', #37847, 12.73448142120000171 ) ;
#96840 = CARTESIAN_POINT ( 'NONE',  ( -6.349985216170000335, 1382.931437671549929, 199.9495528202790240 ) ) ;
#96841 = CARTESIAN_POINT ( 'NONE',  ( -4.735819760670000100, 1474.606130560490101, 199.1616167749889712 ) ) ;
#96843 = VERTEX_POINT ( 'NONE', #14468 ) ;
#96842 = CARTESIAN_POINT ( 'NONE',  ( -18.29057181139999955, 1416.237488680629895, 208.8052359792139896 ) ) ;
#96844 = CARTESIAN_POINT ( 'NONE',  ( -5.950684562925319554, 1508.551704408389924, 219.4535821075459978 ) ) ;
#96845 = EDGE_LOOP ( 'NONE', ( #18346, #78161, #87438, #102677, #42215 ) ) ;
#96846 = AXIS2_PLACEMENT_3D ( 'NONE', #50273, #83848, #76002 ) ;
#96847 = CARTESIAN_POINT ( 'NONE',  ( -8.974550634399999893, 1388.636165673550295, 217.7040576462889874 ) ) ;
#96848 = CARTESIAN_POINT ( 'NONE',  ( -16.67302254290000008, 1414.971352895729979, 209.3683777951139859 ) ) ;
#96849 =( LENGTH_UNIT ( ) NAMED_UNIT ( * ) SI_UNIT ( .MILLI., .METRE. ) );
#96850 = CARTESIAN_POINT ( 'NONE',  ( 14.46805569519750101, 1471.430981385289897, 194.8600923975780006 ) ) ;
#96851 = CARTESIAN_POINT ( 'NONE',  ( -1.452023954020000174, 1431.108953371590133, 217.3997850383090054 ) ) ;
#96852 = DIRECTION ( 'NONE',  ( -0.4794255386042019507, 0.000000000000000000, 0.8775825618903732028 ) ) ;
#96853 = CARTESIAN_POINT ( 'NONE',  ( 14.90637800594289963, 1409.433602577639931, 208.2132206234400087 ) ) ;
#96854 = CARTESIAN_POINT ( 'NONE',  ( -7.966093458541450012, 1384.918002514549926, 199.4892729902699955 ) ) ;
#96855 = CARTESIAN_POINT ( 'NONE',  ( -95.36803178986139073, 1385.208579419249872, 295.0786609535289813 ) ) ;
#96856 = CARTESIAN_POINT ( 'NONE',  ( 2.750555068763795852, 1464.695220856118340, 236.8701281407333283 ) ) ;
#96857 = CARTESIAN_POINT ( 'NONE',  ( -41.85969401239999854, 1379.735023715520128, 226.1594769080589913 ) ) ;
#96858 = CIRCLE ( 'NONE', #109329, 1.999999999999998668 ) ;
#96859 = CARTESIAN_POINT ( 'NONE',  ( 17.22592482065197927, 1443.913060387330233, 162.9227486220069920 ) ) ;
#96860 = ORIENTED_EDGE ( 'NONE', *, *, #83626, .F. ) ;
#96861 = ORIENTED_EDGE ( 'NONE', *, *, #57615, .F. ) ;
#96862 = CARTESIAN_POINT ( 'NONE',  ( -11.78977346134420046, 1415.441076448340027, 195.1339339561199893 ) ) ;
#96863 = CARTESIAN_POINT ( 'NONE',  ( -11.45855569280000097, 1433.892739005809972, 151.4107738152980289 ) ) ;
#96864 = CARTESIAN_POINT ( 'NONE',  ( 16.18935668596350297, 1469.063782001718891, 269.3698815738000576 ) ) ;
#96865 = CARTESIAN_POINT ( 'NONE',  ( 0.4151546846821903003, 1511.187213306747708, 242.9330574173806951 ) ) ;
#96866 = CARTESIAN_POINT ( 'NONE',  ( -28.27265633500000064, 1508.146186371529893, 208.9956447143910054 ) ) ;
#96867 = CARTESIAN_POINT ( 'NONE',  ( 31.65140982495767830, 1525.320827368860819, 202.0582358972276609 ) ) ;
#96868 = CARTESIAN_POINT ( 'NONE',  ( -0.5257632930290000450, 1462.357837080030095, 182.8478810461979833 ) ) ;
#96869 = CARTESIAN_POINT ( 'NONE',  ( -9.978586514379999883, 1364.539968386210148, 207.6218459616989946 ) ) ;
#96870 = CARTESIAN_POINT ( 'NONE',  ( -25.82488450470238917, 1436.659123590438639, 137.0441985079759490 ) ) ;
#96871 = CARTESIAN_POINT ( 'NONE',  ( 2.282915183265000092, 1516.876240617270014, 206.6278256496669883 ) ) ;
#96872 = CARTESIAN_POINT ( 'NONE',  ( -13.04350371379999984, 1435.138103787100135, 150.1848718228980033 ) ) ;
#96873 = COLOUR_RGB ( '', 0.08235294, 0.09019608, 0.10196078) ;
#96874 = CARTESIAN_POINT ( 'NONE',  ( 17.05796332999999976, 1409.508737592730085, 194.6785584388979942 ) ) ;
#96875 = CARTESIAN_POINT ( 'NONE',  ( -4.869779319875719992, 1491.215858047409938, 188.8099518120989728 ) ) ;
#96876 = CARTESIAN_POINT ( 'NONE',  ( -107.0843635519999992, 1382.329134876569924, 298.0462323021590691 ) ) ;
#96877 = EDGE_LOOP ( 'NONE', ( #21733, #110235, #24954, #98110 ) ) ;
#96878 = CARTESIAN_POINT ( 'NONE',  ( 41.23304493959999917, 1435.760838929649935, 261.5842297915980339 ) ) ;
#96879 = CARTESIAN_POINT ( 'NONE',  ( -22.70805116070000196, 1469.235391021629994, 197.6311956375980117 ) ) ;
#96881 = CARTESIAN_POINT ( 'NONE',  ( 3.203789175851970288E-09, 1424.294192408320214, 227.6053815985079893 ) ) ;
#96880 = CARTESIAN_POINT ( 'NONE',  ( -0.5378215255980000054, 1504.643126066929881, 180.9356492381979820 ) ) ;
#96882 = DIRECTION ( 'NONE',  ( 0.8775825618903754233, 0.000000000000000000, 0.4794255386041978984 ) ) ;
#96883 = CARTESIAN_POINT ( 'NONE',  ( -24.26836096399999931, 1418.067431480530104, 255.0044362610979647 ) ) ;
#96884 = CARTESIAN_POINT ( 'NONE',  ( 3.018304369310000013, 1486.259445700090055, 219.4861415874989916 ) ) ;
#96885 = CARTESIAN_POINT ( 'NONE',  ( -5.106893094720000192, 1391.877272790489997, 214.4361776263990009 ) ) ;
#96886 = CARTESIAN_POINT ( 'NONE',  ( 33.93392841120000014, 1451.575795592029863, 135.5855060888980006 ) ) ;
#96887 = ORIENTED_EDGE ( 'NONE', *, *, #108297, .F. ) ;
#96888 = CARTESIAN_POINT ( 'NONE',  ( 3.741929523840420213, 1397.105479193189922, 196.2901283285229965 ) ) ;
#96889 = CARTESIAN_POINT ( 'NONE',  ( 17.30126322281391893, 1523.382868172863937, 237.3930845920473303 ) ) ;
#96890 = CARTESIAN_POINT ( 'NONE',  ( -4.086314366678965193, 1515.499673595108106, 206.7917118397523666 ) ) ;
#96891 = EDGE_LOOP ( 'NONE', ( #105155, #3421, #74726, #88513 ) ) ;
#96892 = ORIENTED_EDGE ( 'NONE', *, *, #6253, .T. ) ;
#96893 = CARTESIAN_POINT ( 'NONE',  ( 9.133139594464850575, 1451.141730094770082, 210.6182008139099935 ) ) ;
#96894 = CARTESIAN_POINT ( 'NONE',  ( -23.58016236440349900, 1410.013568677760077, 208.8036717605170054 ) ) ;
#96895 = B_SPLINE_CURVE_WITH_KNOTS ( 'NONE', 3,
 ( #53439, #1937, #87585, #29859, #20896, #63510, #20349, #10874, #11966, #4134 ),
 .UNSPECIFIED., .F., .F.,
 ( 4, 2, 2, 2, 4 ),
 ( 0.000000000000000000, 0.2500000000000000000, 0.5000000000000000000, 0.7500000000000000000, 1.000000000000000000 ),
 .UNSPECIFIED. ) ;
#96896 = ORIENTED_EDGE ( 'NONE', *, *, #85035, .F. ) ;
#96897 = AXIS2_PLACEMENT_3D ( 'NONE', #21484, #45650, #62457 ) ;
#96898 = CARTESIAN_POINT ( 'NONE',  ( -1.358844237360000040, 1412.076917109029864, 185.5300820243980127 ) ) ;
#96899 = CARTESIAN_POINT ( 'NONE',  ( -9.833393186232900263, 1522.051704408389924, 212.5077547680540135 ) ) ;
#96900 = CARTESIAN_POINT ( 'NONE',  ( 0.4407570218449999855, 1450.897668812970096, 181.9257963629979997 ) ) ;
#96901 = CARTESIAN_POINT ( 'NONE',  ( -1.656928908930000111, 1479.774557543030141, 235.9029919223980016 ) ) ;
#96902 = DIRECTION ( 'NONE',  ( -0.02307801285194388888, -0.7475172515513471838, 0.6638413695725249308 ) ) ;
#96903 = VERTEX_POINT ( 'NONE', #92836 ) ;
#96904 = CARTESIAN_POINT ( 'NONE',  ( 11.43735029920000024, 1425.481221014229959, 144.1633320283980026 ) ) ;
#96905 = CARTESIAN_POINT ( 'NONE',  ( -12.28448271699999950, 1391.742831493179892, 209.7423336216829739 ) ) ;
#96906 = CARTESIAN_POINT ( 'NONE',  ( 14.52328904310000013, 1474.745154377930021, 224.9348462990979840 ) ) ;
#96907 = ORIENTED_EDGE ( 'NONE', *, *, #101266, .T. ) ;
#96908 = CARTESIAN_POINT ( 'NONE',  ( 6.937338745574999521, 1516.706638732659940, 204.5037262658370025 ) ) ;
#96909 = ORIENTED_EDGE ( 'NONE', *, *, #3535, .T. ) ;
#96910 = CARTESIAN_POINT ( 'NONE',  ( 11.86522610041399872, 1432.274900462119831, 149.9820474266710164 ) ) ;
#96911 = AXIS2_PLACEMENT_3D ( 'NONE', #7278, #56591, #57711 ) ;
#96912 = EDGE_CURVE ( 'NONE', #94116, #55879, #31386, .T. ) ;
#96913 = CARTESIAN_POINT ( 'NONE',  ( 13.42472599018740276, 1444.364182771770857, 187.7916057231489617 ) ) ;
#96914 = EDGE_LOOP ( 'NONE', ( #81168, #32823, #92690, #90837 ) ) ;
#96915 = ORIENTED_EDGE ( 'NONE', *, *, #108907, .F. ) ;
#96916 = CARTESIAN_POINT ( 'NONE',  ( -15.68254779151874523, 1506.474306126180863, 193.6687607889768969 ) ) ;
#96917 = EDGE_CURVE ( 'NONE', #105177, #60257, #13811, .T. ) ;
#96918 = CARTESIAN_POINT ( 'NONE',  ( -7.656877098949100180, 1508.551704408389924, 219.0266944425760016 ) ) ;
#96919 = CARTESIAN_POINT ( 'NONE',  ( 13.19514936480000067, 1509.316610144029937, 234.6191713803979724 ) ) ;
#96920 = CARTESIAN_POINT ( 'NONE',  ( -3.622938608617219725, 1468.835452661259978, 218.9451918032920048 ) ) ;
#96921 = CARTESIAN_POINT ( 'NONE',  ( -4.306224067269999622, 1423.875121241730085, 184.5583045049980058 ) ) ;
#96922 = CARTESIAN_POINT ( 'NONE',  ( 0.9513729900170889708, 1410.039306745070007, 269.8654762829310130 ) ) ;
#96923 = CARTESIAN_POINT ( 'NONE',  ( 9.225032543388721251, 1450.630799636350048, 209.4288614389280099 ) ) ;
#96924 = CARTESIAN_POINT ( 'NONE',  ( -6.281153590029999734, 1475.159552144489908, 200.8925845212189927 ) ) ;
#96925 = CARTESIAN_POINT ( 'NONE',  ( 8.502412689479999841, 1494.223831056089921, 218.1490364173589853 ) ) ;
#96926 = CYLINDRICAL_SURFACE ( 'NONE', #82303, 1.999999999999999556 ) ;
#96927 = DIRECTION ( 'NONE',  ( -3.659266894335750173E-33, 6.123233995736769734E-17, 1.000000000000000000 ) ) ;
#96929 = CARTESIAN_POINT ( 'NONE',  ( 15.58680661270000023, 1453.154034702829904, 195.7020206013980044 ) ) ;
#96928 = CARTESIAN_POINT ( 'NONE',  ( -20.17395953629999994, 1505.644431352489846, 209.1238650338669913 ) ) ;
#96930 = CARTESIAN_POINT ( 'NONE',  ( 12.32667913303630058, 1421.670227258269961, 207.4634014051960094 ) ) ;
#96931 = CARTESIAN_POINT ( 'NONE',  ( -9.914173110146720092, 1439.743127349719998, 207.7929445919720024 ) ) ;
#96932 = CARTESIAN_POINT ( 'NONE',  ( -6.560424634844999936, 1512.053281741900037, 200.4573988352969707 ) ) ;
#96933 = ORIENTED_EDGE ( 'NONE', *, *, #12302, .T. ) ;
#96934 = CARTESIAN_POINT ( 'NONE',  ( 34.97756116859999764, 1432.582706846070096, 262.6648722463980334 ) ) ;
#96935 = CIRCLE ( 'NONE', #12828, 2.000007505163727828 ) ;
#96936 = CARTESIAN_POINT ( 'NONE',  ( 19.74853702175585823, 1455.472137957127870, 226.4474092902466396 ) ) ;
#96937 = CARTESIAN_POINT ( 'NONE',  ( -61.62696079022420292, 1385.058290879319884, 283.6552644066600237 ) ) ;
#96938 = ADVANCED_FACE ( 'NONE', ( #57619 ), #19162, .T. ) ;
#96939 = DIRECTION ( 'NONE',  ( -0.9125304618753937724, 0.000000000000000000, 0.4090087482554383147 ) ) ;
#96940 = CARTESIAN_POINT ( 'NONE',  ( 5.057785354339999984, 1505.946855220289990, 219.7575345696990041 ) ) ;
#96941 = DIRECTION ( 'NONE',  ( -0.9081805863301267712, -0.3859282978888783910, 0.1620721182118019799 ) ) ;
#96942 = VECTOR ( 'NONE', #71983, 1000.000000000000000 ) ;
#96944 = ORIENTED_EDGE ( 'NONE', *, *, #73385, .T. ) ;
#96943 = CARTESIAN_POINT ( 'NONE',  ( -4.152733088471870282, 1435.142315282680102, 185.7019193756299842 ) ) ;
#96945 = FACE_OUTER_BOUND ( 'NONE', #25047, .T. ) ;
#96946 = CARTESIAN_POINT ( 'NONE',  ( -24.34269059140000024, 1442.549324342949831, 212.2035682044480041 ) ) ;
#96947 = CARTESIAN_POINT ( 'NONE',  ( -16.00209757519999698, 1416.197507335639784, 209.0643480693830156 ) ) ;
#96948 = CARTESIAN_POINT ( 'NONE',  ( -12.35978978633600001, 1391.723785652940933, 209.7460346078842974 ) ) ;
#96949 = CARTESIAN_POINT ( 'NONE',  ( 13.06501229733500047, 1513.192861445620110, 226.0202954981670302 ) ) ;
#96950 = DIRECTION ( 'NONE',  ( 0.000000000000000000, 0.000000000000000000, 1.000000000000000000 ) ) ;
#96951 = CARTESIAN_POINT ( 'NONE',  ( 30.67697261150000188, 1510.112560769530091, 213.7284012127280164 ) ) ;
#96952 = CARTESIAN_POINT ( 'NONE',  ( 2.835689136585590298, 1456.955521931160092, 199.2250932076429990 ) ) ;
#96953 = CARTESIAN_POINT ( 'NONE',  ( -5.371346839175000554, 1517.051704408389924, 218.7599618298069970 ) ) ;
#96954 = CARTESIAN_POINT ( 'NONE',  ( 16.34175718830000079, 1410.409901383030046, 226.6814971688980052 ) ) ;
#96955 = CARTESIAN_POINT ( 'NONE',  ( -7.980349849529399187, 1424.821740665096513, 210.5240757545262511 ) ) ;
#96956 = CARTESIAN_POINT ( 'NONE',  ( -16.13005433389999865, 1459.079426146030073, 230.3616589300980024 ) ) ;
#96957 = CARTESIAN_POINT ( 'NONE',  ( 4.026777485955000735, 1516.718889242609976, 206.8247602162870180 ) ) ;
#96958 = CARTESIAN_POINT ( 'NONE',  ( 45.95995674830000155, 1436.878729300550049, 268.2107401488980258 ) ) ;
#96959 = CARTESIAN_POINT ( 'NONE',  ( -18.12385451149999938, 1410.042553338630114, 224.1601288465979849 ) ) ;
#96960 = EDGE_CURVE ( 'NONE', #87844, #75143, #76048, .T. ) ;
#96961 = CARTESIAN_POINT ( 'NONE',  ( 19.17690546040000044, 1435.982630086400150, 146.1499213334980141 ) ) ;
#96962 = CARTESIAN_POINT ( 'NONE',  ( 23.21287423860000132, 1488.579583080329940, 196.1738562084979947 ) ) ;
#96963 = CARTESIAN_POINT ( 'NONE',  ( -16.66096088174899847, 1410.867477246420094, 191.7374981741809847 ) ) ;
#96964 = FACE_OUTER_BOUND ( 'NONE', #28837, .T. ) ;
#96965 = CARTESIAN_POINT ( 'NONE',  ( -16.37880298289999814, 1420.875924758830024, 227.0362411946979933 ) ) ;
#96966 = CARTESIAN_POINT ( 'NONE',  ( -14.85956138398720050, 1417.764634060990147, 203.2214948970120361 ) ) ;
#96967 = CARTESIAN_POINT ( 'NONE',  ( -35.57568823278909775, 1437.203474868449803, 136.5255046917930031 ) ) ;
#96968 = EDGE_CURVE ( 'NONE', #46415, #18694, #54657, .T. ) ;
#96969 = CARTESIAN_POINT ( 'NONE',  ( -8.706022017420000481, 1409.217081375429871, 196.8236899110980005 ) ) ;
#96970 = CARTESIAN_POINT ( 'NONE',  ( -18.69410140469999959, 1415.934222461130048, 207.6343539392380251 ) ) ;
#96971 = CARTESIAN_POINT ( 'NONE',  ( -17.56004599463900817, 1410.529980821251456, 193.4350317141646940 ) ) ;
#96972 = CARTESIAN_POINT ( 'NONE',  ( -7.548201923578629291, 1384.559186287549892, 219.0738854171599996 ) ) ;
#96973 = CARTESIAN_POINT ( 'NONE',  ( 3.002126187839210480, 1456.245863093199887, 219.3132837443019980 ) ) ;
#96974 = CARTESIAN_POINT ( 'NONE',  ( 17.92652493019800275, 1429.078765382750134, 206.1304143520609955 ) ) ;
#96975 = CARTESIAN_POINT ( 'NONE',  ( -1.368191914778909890, 1419.344528075180278, 185.2221190139939893 ) ) ;
#96976 = EDGE_LOOP ( 'NONE', ( #10385, #86505, #30711, #39340 ) ) ;
#96977 = B_SPLINE_CURVE_WITH_KNOTS ( 'NONE', 3,
 ( #11467, #26022, #18729, #52382 ),
 .UNSPECIFIED., .F., .F.,
 ( 4, 4 ),
 ( 0.000000000000000000, 0.0002220129587134776392 ),
 .UNSPECIFIED. ) ;
#96978 = CARTESIAN_POINT ( 'NONE',  ( 4.387476684030000129, 1477.221828185889990, 199.1648530448690053 ) ) ;
#96979 = CARTESIAN_POINT ( 'NONE',  ( -0.9045544433440699805, 1408.944648124569994, 224.0901810006990047 ) ) ;
#96980 = CARTESIAN_POINT ( 'NONE',  ( -1.836970198721029983E-15, 1374.913060387289988, 209.1218459572589836 ) ) ;
#96981 = CARTESIAN_POINT ( 'NONE',  ( 17.78284146230000218, 1432.724246433989947, 213.5810953123289835 ) ) ;
#96982 = CARTESIAN_POINT ( 'NONE',  ( -17.22592475669953416, 1443.501467202839649, 162.9227486557969655 ) ) ;
#96983 = CARTESIAN_POINT ( 'NONE',  ( -42.53834064419999805, 1456.148668462929891, 267.7255875186979779 ) ) ;
#96984 = CARTESIAN_POINT ( 'NONE',  ( -12.97254895038339839, 1428.741066686509839, 222.4354626778209933 ) ) ;
#96985 = CARTESIAN_POINT ( 'NONE',  ( 0.2181331577922970000, 1420.478474626580009, 182.9759614564109711 ) ) ;
#96986 = CARTESIAN_POINT ( 'NONE',  ( 19.92151515271066842, 1526.208281990539717, 233.5199663060478201 ) ) ;
#96987 = CARTESIAN_POINT ( 'NONE',  ( -105.8373447700190013, 1384.589731091189833, 311.2092883949439965 ) ) ;
#96988 = CARTESIAN_POINT ( 'NONE',  ( -49.08829210262739906, 1385.015916341950060, 223.8650612806140145 ) ) ;
#96989 = CARTESIAN_POINT ( 'NONE',  ( -5.101748558636990616, 1375.122757580649932, 214.7573637342229915 ) ) ;
#96990 = CARTESIAN_POINT ( 'NONE',  ( 33.36586802512179162, 1523.382868172864164, 216.3367586934468818 ) ) ;
#96991 = CARTESIAN_POINT ( 'NONE',  ( -28.25996323917220110, 1508.267047293149972, 208.8520637241439886 ) ) ;
#96992 = B_SPLINE_CURVE_WITH_KNOTS ( 'NONE', 3,
 ( #23637, #16312, #75167, #84637, #7934, #76251, #91944, #70641, #96360, #85742 ),
 .UNSPECIFIED., .F., .F.,
 ( 4, 2, 2, 2, 4 ),
 ( -0.2944084045147770112, -0.1489376058949150039, -0.07511920350920017753, -0.03772615716977101297, 0.000000000000000000 ),
 .UNSPECIFIED. ) ;
#96993 = CARTESIAN_POINT ( 'NONE',  ( -3.348647037815419836, 1523.530870145310246, 176.1572109406604625 ) ) ;
#96995 = ORIENTED_EDGE ( 'NONE', *, *, #56962, .T. ) ;
#96994 = CARTESIAN_POINT ( 'NONE',  ( 3.970093244310000102, 1515.569676282289947, 207.9973965014289945 ) ) ;
#96996 = CARTESIAN_POINT ( 'NONE',  ( -5.909457418149999697, 1509.192346212930033, 179.7976553797979875 ) ) ;
#96997 = LINE ( 'NONE', #20260, #67196 ) ;
#96998 = DIRECTION ( 'NONE',  ( 1.387778780781444413E-14, 0.000000000000000000, 1.000000000000000000 ) ) ;
#96999 = CARTESIAN_POINT ( 'NONE',  ( -12.65530650809999891, 1416.254459046630018, 195.1516350870979863 ) ) ;
#97000 = CARTESIAN_POINT ( 'NONE',  ( -1.191029124920000015, 1421.235635819999970, 193.7391320501990322 ) ) ;
#97001 = CARTESIAN_POINT ( 'NONE',  ( 23.54238912610000156, 1411.095556395429867, 211.7543428466179876 ) ) ;
#97002 = CARTESIAN_POINT ( 'NONE',  ( 3.902542035141590038, 1426.015650130040058, 185.2953857556300079 ) ) ;
#97003 = CARTESIAN_POINT ( 'NONE',  ( 10.30424762810000061, 1453.480958077889909, 189.9461784470989869 ) ) ;
#97004 = CARTESIAN_POINT ( 'NONE',  ( -5.361099102583589016, 1423.467400204739988, 149.3859628662110026 ) ) ;
#97006 = CARTESIAN_POINT ( 'NONE',  ( -11.99335295539999890, 1380.187651171090010, 204.2174947147890123 ) ) ;
#97005 = CARTESIAN_POINT ( 'NONE',  ( -11.31015099709999916, 1432.869308247210029, 151.5208831367980054 ) ) ;
#97007 = CARTESIAN_POINT ( 'NONE',  ( -0.5133987858209999589, 1410.300672046529826, 233.1712545434979802 ) ) ;
#97008 = CARTESIAN_POINT ( 'NONE',  ( -104.3512419886430109, 1378.528619065190469, 309.1652051103151848 ) ) ;
#97009 = CARTESIAN_POINT ( 'NONE',  ( -12.23489737639999930, 1490.237667550689821, 209.6383003343199789 ) ) ;
#97010 = CARTESIAN_POINT ( 'NONE',  ( -11.60387546109999946, 1481.105535807389970, 211.4044418313389997 ) ) ;
#97011 = CARTESIAN_POINT ( 'NONE',  ( -6.376409808237344379, 1368.420764496007450, 210.6218459616991936 ) ) ;
#97012 = B_SPLINE_CURVE_WITH_KNOTS ( 'NONE', 3,
 ( #9252, #32240, #43409, #23816, #92143, #68075, #319, #101073, #93769, #17048 ),
 .UNSPECIFIED., .F., .F.,
 ( 4, 2, 2, 2, 4 ),
 ( 3.551066926146560086E-09, 0.03694625896444130031, 0.07332082148824449475, 0.1158698472050300049, 0.1380128657416029858 ),
 .UNSPECIFIED. ) ;
#97013 = CARTESIAN_POINT ( 'NONE',  ( 2.287084270065000258, 1517.068517094990057, 204.1085709707169826 ) ) ;
#97014 = CARTESIAN_POINT ( 'NONE',  ( 13.37391227950199912, 1507.591760071039971, 233.0544810109369962 ) ) ;
#97015 = CARTESIAN_POINT ( 'NONE',  ( -18.97045675350529947, 1486.106069708590212, 189.3881501793050290 ) ) ;
#97016 = AXIS2_PLACEMENT_3D ( 'NONE', #36320, #12779, #70517 ) ;
#97017 = CARTESIAN_POINT ( 'NONE',  ( -9.205204419190000209, 1422.968094939250022, 210.4274292779389839 ) ) ;
#97018 = CARTESIAN_POINT ( 'NONE',  ( -15.57808073540140015, 1420.358152465259991, 210.5578313205389804 ) ) ;
#97020 = ORIENTED_EDGE ( 'NONE', *, *, #22570, .F. ) ;
#97019 = CARTESIAN_POINT ( 'NONE',  ( -68.31098214269999858, 1379.747686652819993, 279.8373429270589554 ) ) ;
#97021 = EDGE_LOOP ( 'NONE', ( #7868, #54767, #107369, #5388, #47010 ) ) ;
#97022 = CARTESIAN_POINT ( 'NONE',  ( 29.54377282369999946, 1509.965350294430209, 211.5458056821180151 ) ) ;
#97023 = ORIENTED_EDGE ( 'NONE', *, *, #102697, .F. ) ;
#97024 = CARTESIAN_POINT ( 'NONE',  ( -1.973026181207146124, 1456.791506541725994, 199.8306417962847092 ) ) ;
#97025 = CARTESIAN_POINT ( 'NONE',  ( -109.4842782119999924, 1384.933317133270066, 311.2840723172590174 ) ) ;
#97027 = CARTESIAN_POINT ( 'NONE',  ( 15.77036826645290191, 1409.489309249800044, 192.6567201191820118 ) ) ;
#97026 = CARTESIAN_POINT ( 'NONE',  ( 2.368833328420000051, 1427.018531676430030, 133.6118001900980232 ) ) ;
#97028 = FACE_OUTER_BOUND ( 'NONE', #12982, .T. ) ;
#97029 = CARTESIAN_POINT ( 'NONE',  ( -24.51797533977270049, 1451.993604082630100, 136.7394497936419953 ) ) ;
#97030 = FACE_OUTER_BOUND ( 'NONE', #32891, .T. ) ;
#97031 = CARTESIAN_POINT ( 'NONE',  ( 11.01620263480000084, 1409.800477099530099, 229.2053215475979755 ) ) ;
#97032 = CARTESIAN_POINT ( 'NONE',  ( 12.48512064311860037, 1501.209728726249978, 211.5369004838399860 ) ) ;
#97033 = SURFACE_STYLE_USAGE ( .BOTH. , #53953 ) ;
#97034 = CARTESIAN_POINT ( 'NONE',  ( -7.322709724964999722, 1516.596789218710001, 212.3828531017969965 ) ) ;
#97035 = CARTESIAN_POINT ( 'NONE',  ( 41.44976345430139730, 1445.539178997240015, 134.0999999985149884 ) ) ;
#97036 = FACE_OUTER_BOUND ( 'NONE', #109291, .T. ) ;
#97037 = ORIENTED_EDGE ( 'NONE', *, *, #46642, .T. ) ;
#97038 = CARTESIAN_POINT ( 'NONE',  ( 14.51818222938589997, 1436.251066462949893, 149.9197869802679861 ) ) ;
#97039 = CARTESIAN_POINT ( 'NONE',  ( -2.425229330588690058, 1431.099637562449971, 201.1035349865409785 ) ) ;
#97040 = B_SPLINE_CURVE_WITH_KNOTS ( 'NONE', 3,
 ( #53484, #10916, #106071, #104969, #97667, #79231, #36119, #29896, #2540, #80325, #63016, #36664, #88728, #105529, #54594, #87061, #70858, #28258, #62451, #87628, #72481, #80872, #3641, #44520, #12561, #19847, #12011, #3090, #38301, #21479, #45645, #55144, #70303 ),
 .UNSPECIFIED., .F., .F.,
 ( 4, 1, 1, 2, 2, 1, 1, 2, 2, 2, 1, 1, 1, 2, 2, 2, 1, 1, 2, 2, 4 ),
 ( 0.000000000000000000, 0.06250000000018264557, 0.09375000000028335667, 0.1093750000003022582, 0.1250000000003211598, 0.1875000000005473677, 0.2187500000006051826, 0.2343750000006341039, 0.2500000000006630252, 0.3750000000007583378, 0.4375000000008123502, 0.4687500000008393286, 0.4843750000007667200, 0.4921875000007259193, 0.5000000000006850076, 0.6250000000008451018, 0.6875000000009251488, 0.7187500000009674483, 0.7343750000008923973, 0.7500000000008173462, 1.000000000000000000 ),
 .UNSPECIFIED. ) ;
#97041 = ORIENTED_EDGE ( 'NONE', *, *, #92875, .F. ) ;
#97042 = ORIENTED_EDGE ( 'NONE', *, *, #24725, .F. ) ;
#97043 = EDGE_LOOP ( 'NONE', ( #104859, #37199, #89861, #102321, #9873, #21598, #6382, #581, #97859, #43345, #103061, #96592, #62883, #98684, #70028, #92325, #99777, #102995, #105865, #7646, #54671 ) ) ;
#97044 = CARTESIAN_POINT ( 'NONE',  ( -8.061256588785001398, 1512.677556571460173, 216.0330363529270130 ) ) ;
#97045 = CARTESIAN_POINT ( 'NONE',  ( 16.75056590446115479, 1513.749562441641729, 195.5293526489948874 ) ) ;
#97046 = CARTESIAN_POINT ( 'NONE',  ( 9.248771300983904098, 1451.347040920142035, 152.5423568881176948 ) ) ;
#97047 = CARTESIAN_POINT ( 'NONE',  ( -7.545183853529999318, 1384.918586394910108, 219.0875716720989885 ) ) ;
#97048 = CARTESIAN_POINT ( 'NONE',  ( -0.1084292933363149997, 1465.381382752510035, 198.1171392823189876 ) ) ;
#97049 = CARTESIAN_POINT ( 'NONE',  ( -14.52404855940000061, 1379.696583046410069, 208.2610545982349777 ) ) ;
#97050 = CARTESIAN_POINT ( 'NONE',  ( -67.62931585915434596, 1379.745611060300917, 277.6776758072804228 ) ) ;
#97051 = CARTESIAN_POINT ( 'NONE',  ( 4.224261702798199458, 1446.243936627659878, 166.7668577399350056 ) ) ;
#97052 = CARTESIAN_POINT ( 'NONE',  ( 0.6279831788249999880, 1507.650420244430052, 237.3702373079979964 ) ) ;
#97053 = ORIENTED_EDGE ( 'NONE', *, *, #28772, .F. ) ;
#97054 = CARTESIAN_POINT ( 'NONE',  ( 4.026777485955000735, 1516.718889242609976, 206.8247602162870180 ) ) ;
#97055 = ORIENTED_EDGE ( 'NONE', *, *, #9842, .F. ) ;
#97056 = CARTESIAN_POINT ( 'NONE',  ( 23.52342552954910104, 1440.913060387330006, 233.8510226637129961 ) ) ;
#97057 = CARTESIAN_POINT ( 'NONE',  ( -16.42216134770000124, 1507.747023505630068, 185.8766527436980027 ) ) ;
#97058 = EDGE_LOOP ( 'NONE', ( #41259, #60593 ) ) ;
#97059 = CARTESIAN_POINT ( 'NONE',  ( -7.443079267411500055, 1508.729259695960081, 203.0017376064890016 ) ) ;
#97060 = CARTESIAN_POINT ( 'NONE',  ( -14.92380019159999982, 1409.936028048729895, 190.9400102447980032 ) ) ;
#97061 = CARTESIAN_POINT ( 'NONE',  ( -46.83417551517494104, 1379.681032646411495, 239.8460456441436293 ) ) ;
#97063 = FACE_OUTER_BOUND ( 'NONE', #108044, .T. ) ;
#97062 = CARTESIAN_POINT ( 'NONE',  ( -24.36535764299999940, 1440.954195507719987, 211.6879696047379866 ) ) ;
#97064 = CARTESIAN_POINT ( 'NONE',  ( -4.823731843395559160, 1434.139159376030193, 217.4489446990200179 ) ) ;
#97065 = CARTESIAN_POINT ( 'NONE',  ( 0.0002591936723112243891, 1396.150190320668798, 197.1672001813749944 ) ) ;
#97066 = DIRECTION ( 'NONE',  ( -0.4770263929453589236, -0.7067418228232984490, -0.5224574779883445208 ) ) ;
#97067 = CARTESIAN_POINT ( 'NONE',  ( -27.69925886641940238, 1441.434395751479997, 137.3015763626259798 ) ) ;
#97068 = CARTESIAN_POINT ( 'NONE',  ( -2.469737752589999946, 1507.227429050490173, 221.7265311398990093 ) ) ;
#97070 = CARTESIAN_POINT ( 'NONE',  ( 29.30029655192942073, 1525.907212628473644, 196.8717316207784620 ) ) ;
#97069 = CARTESIAN_POINT ( 'NONE',  ( 4.725705173089999711, 1464.404288624430137, 236.3620497209980158 ) ) ;
#97071 = CARTESIAN_POINT ( 'NONE',  ( 6.942973629204999497, 1516.833844030519913, 216.4505221401170161 ) ) ;
#97072 = CARTESIAN_POINT ( 'NONE',  ( -32.10254378951861298, 1525.211473355384669, 217.0238571822993379 ) ) ;
#97073 = CARTESIAN_POINT ( 'NONE',  ( 5.863482170922579506, 1511.603576927810082, 217.5746331517350143 ) ) ;
#97074 = EDGE_CURVE ( 'NONE', #53387, #110093, #24514, .T. ) ;
#97075 = CARTESIAN_POINT ( 'NONE',  ( 28.48686854299999993, 1509.161777454930188, 208.9464261767249980 ) ) ;
#97076 = CARTESIAN_POINT ( 'NONE',  ( 4.624736859184999993, 1516.994127245590107, 211.9896495963369887 ) ) ;
#97077 = CARTESIAN_POINT ( 'NONE',  ( 4.261662194147191052, 1515.372228416590133, 211.4517523138519834 ) ) ;
#97078 = CARTESIAN_POINT ( 'NONE',  ( 4.781276783620000081, 1452.020048942890071, 190.5513815401990030 ) ) ;
#97080 = EDGE_LOOP ( 'NONE', ( #57774, #107164, #28523, #63855, #13645, #89361 ) ) ;
#97079 = CARTESIAN_POINT ( 'NONE',  ( -3.076366055149999834, 1424.853903601579987, 191.3970713258989917 ) ) ;
#97081 = CARTESIAN_POINT ( 'NONE',  ( -18.47399052110256434, 1509.320896586165190, 230.4813978297956396 ) ) ;
#97082 = CARTESIAN_POINT ( 'NONE',  ( 10.01186952849999834, 1466.025750516530024, 244.5548898277980072 ) ) ;
#97083 = EDGE_CURVE ( 'NONE', #61329, #11259, #86099, .T. ) ;
#97084 = CARTESIAN_POINT ( 'NONE',  ( 29.35747451428154875, 1526.382868173645647, 217.1997937176751350 ) ) ;
#97085 = CARTESIAN_POINT ( 'NONE',  ( -1.993187091982024040, 1485.308211440273226, 198.1316096946227390 ) ) ;
#97086 = CARTESIAN_POINT ( 'NONE',  ( 1.981508872149999601, 1413.133198254829949, 232.1370634949979888 ) ) ;
#97087 = CARTESIAN_POINT ( 'NONE',  ( -18.82336198069999966, 1456.812963125929855, 227.8489049708979906 ) ) ;
#97089 = CARTESIAN_POINT ( 'NONE',  ( -0.4794255386038975830, 1547.913060387330006, 208.2442633998076076 ) ) ;
#97088 = FACE_OUTER_BOUND ( 'NONE', #17946, .T. ) ;
#97090 = CARTESIAN_POINT ( 'NONE',  ( 0.04790323992079999205, 1506.806593688130079, 187.0235095034979906 ) ) ;
#97091 = CARTESIAN_POINT ( 'NONE',  ( -106.9481960069999928, 1379.492203629369897, 308.7579988892589995 ) ) ;
#97092 = ORIENTED_EDGE ( 'NONE', *, *, #98012, .F. ) ;
#97093 = CARTESIAN_POINT ( 'NONE',  ( -3.460101890015000237, 1516.812923327049930, 205.0932153474469715 ) ) ;
#97094 = CARTESIAN_POINT ( 'NONE',  ( 0.7767783220340001016, 1405.847574658930171, 267.2347138816979850 ) ) ;
#97095 = CARTESIAN_POINT ( 'NONE',  ( 1.105873109660000075, 1515.456834174690130, 213.3233725384289983 ) ) ;
#97096 = CARTESIAN_POINT ( 'NONE',  ( 13.24698951656310086, 1472.683393104890229, 270.3756650808729773 ) ) ;
#97097 = CARTESIAN_POINT ( 'NONE',  ( 5.459750082109999347, 1438.302868353570148, 154.7313708644979897 ) ) ;
#97098 = CARTESIAN_POINT ( 'NONE',  ( 10.16645255423411065, 1422.467695525055433, 137.0999999980980135 ) ) ;
#97099 = CARTESIAN_POINT ( 'NONE',  ( -37.48482910262209344, 1440.913060388469830, 255.4418995164979833 ) ) ;
#97100 = CARTESIAN_POINT ( 'NONE',  ( -25.40278959089999589, 1449.930493708720178, 137.7546507675980081 ) ) ;
#97101 = CARTESIAN_POINT ( 'NONE',  ( -106.3976693117229928, 1390.939243848519936, 307.7527733253859878 ) ) ;
#97102 = CARTESIAN_POINT ( 'NONE',  ( 2.494611379217050118, 1449.235110048550041, 154.7922943218019896 ) ) ;
#97103 = CARTESIAN_POINT ( 'NONE',  ( 2.154904617470000172, 1507.931312947989909, 220.6735988848989791 ) ) ;
#97104 = CARTESIAN_POINT ( 'NONE',  ( -17.84338787571901364, 1523.382868172864164, 237.8836641337663309 ) ) ;
#97105 = EDGE_LOOP ( 'NONE', ( #59165, #4090, #40813, #69369, #12240 ) ) ;
#97106 = CARTESIAN_POINT ( 'NONE',  ( -28.05448514099999713, 1420.250147149929944, 265.6112250856980381 ) ) ;
#97108 = DIRECTION ( 'NONE',  ( 0.000000000000000000, 1.000000000000000000, 0.000000000000000000 ) ) ;
#97107 = APPLICATION_CONTEXT ( 'automotive_design' ) ;
#97109 = CARTESIAN_POINT ( 'NONE',  ( -0.1080292017569999957, 1476.076643212830049, 267.5371647991979671 ) ) ;
#97110 = CARTESIAN_POINT ( 'NONE',  ( -4.279554597526510129, 1446.812741322220063, 156.5769576174630231 ) ) ;
#97111 = CARTESIAN_POINT ( 'NONE',  ( -29.78220350812360806, 1526.382868172863937, 196.5089261231637181 ) ) ;
#97112 = DIRECTION ( 'NONE',  ( -4.222254822704964968E-17, -1.000000000000000000, 7.728785610902679540E-17 ) ) ;
#97113 = CARTESIAN_POINT ( 'NONE',  ( -38.50602658467759909, 1384.794211068249979, 239.5861974842979976 ) ) ;
#97114 = CARTESIAN_POINT ( 'NONE',  ( -18.08041632129999954, 1415.296882296330068, 207.5662767683379855 ) ) ;
#97115 = CARTESIAN_POINT ( 'NONE',  ( 4.760896992130000172, 1449.971761959190189, 190.6385172635989704 ) ) ;
#97116 = CARTESIAN_POINT ( 'NONE',  ( 26.31830653128389841, 1435.497073113130000, 135.8492962503879937 ) ) ;
#97117 = CARTESIAN_POINT ( 'NONE',  ( -4.896674508190200115, 1396.084056030580086, 219.0076142901629908 ) ) ;
#97118 = CARTESIAN_POINT ( 'NONE',  ( -2.740438610378060247, 1508.551704408389924, 204.1475582648899945 ) ) ;
#97119 = CARTESIAN_POINT ( 'NONE',  ( -16.14471337837490239, 1409.485024636370099, 225.3510067295860040 ) ) ;
#97120 = CARTESIAN_POINT ( 'NONE',  ( 19.63348512848709504, 1455.443522392392879, 225.9404624130569914 ) ) ;
#97121 = ORIENTED_EDGE ( 'NONE', *, *, #108302, .F. ) ;
#97122 = CARTESIAN_POINT ( 'NONE',  ( -1.418378755168210104, 1436.146031861469964, 227.5501453695390239 ) ) ;
#97123 = CARTESIAN_POINT ( 'NONE',  ( 1.682318894840000079, 1409.475163267829885, 232.0401757884979759 ) ) ;
#97124 = CARTESIAN_POINT ( 'NONE',  ( -11.79165747303489908, 1429.416857826700152, 146.4064127303859948 ) ) ;
#97126 = CARTESIAN_POINT ( 'NONE',  ( -13.59755241946499993, 1512.525301340730039, 193.3332859498670189 ) ) ;
#97125 = CARTESIAN_POINT ( 'NONE',  ( 10.79671730919999995, 1425.341881714829924, 121.0042872764980046 ) ) ;
#97127 = DIRECTION ( 'NONE',  ( 3.922329127182935292E-10, 2.146905620200830005E-11, -1.000000000000000000 ) ) ;
#97128 = CARTESIAN_POINT ( 'NONE',  ( 4.252688412790660344, 1423.944491522370072, 183.9806639160489965 ) ) ;
#97129 = CARTESIAN_POINT ( 'NONE',  ( -109.9838524239499975, 1384.633113356680042, 311.4476818303249388 ) ) ;
#97130 = CARTESIAN_POINT ( 'NONE',  ( 7.814950425870000217, 1425.209952447059777, 211.6921920394489973 ) ) ;
#97131 = CARTESIAN_POINT ( 'NONE',  ( -0.3862240863000029889, 1500.063269133189806, 233.1571802061990013 ) ) ;
#97132 = CARTESIAN_POINT ( 'NONE',  ( 5.865902423269999666, 1509.102301102529964, 180.5560850680980138 ) ) ;
#97133 = CARTESIAN_POINT ( 'NONE',  ( -8.301987938657498844, 1519.913060387329779, 185.0111222839169898 ) ) ;
#97134 = CARTESIAN_POINT ( 'NONE',  ( -49.29737642897650574, 1380.010108409559962, 242.9177998910799658 ) ) ;
#97135 = CARTESIAN_POINT ( 'NONE',  ( 8.653423937779999520, 1367.169888897630017, 207.6218459616989946 ) ) ;
#97137 = ORIENTED_EDGE ( 'NONE', *, *, #54271, .T. ) ;
#97136 = CARTESIAN_POINT ( 'NONE',  ( -17.10989647720995777, 1517.051704408390151, 195.2932400735099066 ) ) ;
#97138 = EDGE_LOOP ( 'NONE', ( #41114, #89420, #91355, #89446, #47968 ) ) ;
#97139 = CARTESIAN_POINT ( 'NONE',  ( -6.232532193409999977, 1398.098440471930189, 197.7132727529979945 ) ) ;
#97140 = CARTESIAN_POINT ( 'NONE',  ( 1.181642411293839956, 1499.053114097589969, 236.6882745191989841 ) ) ;
#97141 = CARTESIAN_POINT ( 'NONE',  ( -23.03159172119999809, 1435.301732086839138, 138.5817198000980000 ) ) ;
#97142 = CARTESIAN_POINT ( 'NONE',  ( -7.890119408174999904, 1511.483345606789953, 212.6807099935669783 ) ) ;
#97143 =( BOUNDED_CURVE ( )  B_SPLINE_CURVE ( 3, ( #67639, #41319, #25038, #93358 ),
 .UNSPECIFIED., .F., .F. ) 
 B_SPLINE_CURVE_WITH_KNOTS ( ( 4, 4 ),
 ( 0.8259411502862069598, 1.074666572263723863 ),
 .UNSPECIFIED. ) 
 CURVE ( )  GEOMETRIC_REPRESENTATION_ITEM ( )  RATIONAL_B_SPLINE_CURVE ( ( 1.000000000000000000, 0.9948512797181937595, 0.9948512797181937595, 1.000000000000000000 ) ) 
 REPRESENTATION_ITEM ( '' )  );
#97145 = CARTESIAN_POINT ( 'NONE',  ( -1.365744575143430062, 1417.411668549410024, 185.3040620841360067 ) ) ;
#97144 = CARTESIAN_POINT ( 'NONE',  ( -8.296394296239999022, 1384.634392827019838, 218.6956713340389911 ) ) ;
#97146 = CARTESIAN_POINT ( 'NONE',  ( 2.573164677909999920, 1410.304154922730049, 185.5984138544979771 ) ) ;
#97147 = SURFACE_STYLE_USAGE ( .BOTH. , #89840 ) ;
#97148 = CARTESIAN_POINT ( 'NONE',  ( -39.10159291891720557, 1449.758070488810063, 135.2941250337750034 ) ) ;
#97149 = CARTESIAN_POINT ( 'NONE',  ( -2.500000000000000000, 1448.624837927950011, 158.8309530183670120 ) ) ;
#97150 = CARTESIAN_POINT ( 'NONE',  ( 3.756023522784067925, 1369.098589419774044, 210.6218459616991936 ) ) ;
#97151 = CARTESIAN_POINT ( 'NONE',  ( -40.32569152789999833, 1443.160161259170081, 137.0611730016980232 ) ) ;
#97152 = CARTESIAN_POINT ( 'NONE',  ( -5.362056993596479693, 1405.980634290770240, 267.5249872241790285 ) ) ;
#97153 = CARTESIAN_POINT ( 'NONE',  ( 41.65407234159999916, 1444.067060240220144, 136.1145731235980065 ) ) ;
#97154 = VERTEX_POINT ( 'NONE', #104557 ) ;
#97155 = CARTESIAN_POINT ( 'NONE',  ( 21.30909630337538729, 1524.964158026965833, 233.9181086290231235 ) ) ;
#97156 = ORIENTED_EDGE ( 'NONE', *, *, #36424, .F. ) ;
#97157 = ORIENTED_EDGE ( 'NONE', *, *, #71499, .F. ) ;
#97158 = CARTESIAN_POINT ( 'NONE',  ( -9.505471540889999460, 1363.500209798499782, 207.6218459616989946 ) ) ;
#97159 = CARTESIAN_POINT ( 'NONE',  ( -1.705466448594999962, 1517.120861839400050, 214.1360410720469929 ) ) ;
#97160 = CARTESIAN_POINT ( 'NONE',  ( 5.181410150655000990, 1510.418062979269962, 216.6707182703270291 ) ) ;
#97161 = B_SPLINE_SURFACE_WITH_KNOTS ( 'NONE', 5, 1, ( 
 ( #80087, #58075 ),
 ( #15480, #49675 ),
 ( #7106, #63322 ),
 ( #20708, #16565 ),
 ( #43477, #69238 ),
 ( #933, #84895 ) ),
 .UNSPECIFIED., .F., .F., .F.,
 ( 6, 6 ),
 ( 2, 2 ),
 ( 0.000000000000000000, 3.596547541650000124 ),
 ( 0.000000000000000000, 14.00000000000000000 ),
 .UNSPECIFIED. ) ;
#97162 = ORIENTED_EDGE ( 'NONE', *, *, #22644, .T. ) ;
#97163 = CARTESIAN_POINT ( 'NONE',  ( 0.05242611179130000215, 1509.026403085430047, 179.1712902077980232 ) ) ;
#97164 = CARTESIAN_POINT ( 'NONE',  ( -94.75917113079999865, 1374.839168173989947, 301.3391293692590125 ) ) ;
#97165 = CARTESIAN_POINT ( 'NONE',  ( 2.676552135149999678, 1415.087818611729972, 225.8826422939979750 ) ) ;
#97166 = CARTESIAN_POINT ( 'NONE',  ( -6.947377821305000367, 1517.009964551830080, 204.5062011277169916 ) ) ;
#97167 = CARTESIAN_POINT ( 'NONE',  ( -28.79939581020000006, 1509.589065601529910, 208.7222536069020009 ) ) ;
#97168 = CARTESIAN_POINT ( 'NONE',  ( -40.12837905666719251, 1431.802959192438948, 269.6125927220242033 ) ) ;
#97169 = CARTESIAN_POINT ( 'NONE',  ( -10.14900592729999929, 1410.638279238530231, 229.5672309112980258 ) ) ;
#97171 = ORIENTED_EDGE ( 'NONE', *, *, #32902, .T. ) ;
#97170 = DIRECTION ( 'NONE',  ( 0.01430194049125190457, -0.9998977151614593106, 0.0001171028509539070479 ) ) ;
#97172 = CARTESIAN_POINT ( 'NONE',  ( 30.22858968940000324, 1451.857573268230226, 134.8239104374980002 ) ) ;
#97173 = CARTESIAN_POINT ( 'NONE',  ( 28.34110756910000006, 1508.137170137529893, 208.7852603947239913 ) ) ;
#97174 = CARTESIAN_POINT ( 'NONE',  ( -5.962417602059999489, 1383.866448007470126, 218.3533362890090075 ) ) ;
#97175 = CARTESIAN_POINT ( 'NONE',  ( -5.303285988883490454, 1442.879254652209966, 200.5943008362860098 ) ) ;
#97176 = CARTESIAN_POINT ( 'NONE',  ( 15.38665937780000093, 1409.887291428229901, 270.2482212356980540 ) ) ;
#97177 = CARTESIAN_POINT ( 'NONE',  ( -1.119717754394999876, 1517.038650117239968, 212.5846815975970117 ) ) ;
#97178 = CARTESIAN_POINT ( 'NONE',  ( -67.98666868309999245, 1379.746563024860052, 278.4884602742590118 ) ) ;
#97179 = CARTESIAN_POINT ( 'NONE',  ( 0.02018220001661512678, 1507.197434269262885, 237.3577821747751955 ) ) ;
#97180 = CARTESIAN_POINT ( 'NONE',  ( 13.00946304068309978, 1426.713679829950024, 196.5727733038569909 ) ) ;
#97181 = CARTESIAN_POINT ( 'NONE',  ( -17.55006637065400099, 1487.029424903359995, 194.9701071948420008 ) ) ;
#97182 = CARTESIAN_POINT ( 'NONE',  ( 5.011551368014999674, 1517.080322339569875, 209.8587501411369942 ) ) ;
#97183 = VERTEX_POINT ( 'NONE', #51393 ) ;
#97184 = CARTESIAN_POINT ( 'NONE',  ( 22.60252566574085265, 1411.062741202461893, 206.6262987201641579 ) ) ;
#97185 = CARTESIAN_POINT ( 'NONE',  ( -5.992618678210000382, 1415.369965543630087, 231.7268348280979922 ) ) ;
#97186 = CARTESIAN_POINT ( 'NONE',  ( -113.4000000000000057, 1384.800102265719943, 311.2218459572590064 ) ) ;
#97187 = EDGE_LOOP ( 'NONE', ( #92257, #87994, #44999 ) ) ;
#97188 = CARTESIAN_POINT ( 'NONE',  ( -37.35614046057779802, 1385.196686404090087, 237.6971322074060140 ) ) ;
#97189 = CARTESIAN_POINT ( 'NONE',  ( -2.435720662160000050, 1429.409294711090070, 200.4602889503590006 ) ) ;
#97190 = EDGE_CURVE ( 'NONE', #29004, #8321, #80013, .T. ) ;
#97191 = CARTESIAN_POINT ( 'NONE',  ( 6.759474678068709608, 1416.948096802419968, 199.3542690954639909 ) ) ;
#97192 = DIRECTION ( 'NONE',  ( 0.9993902469235411701, -0.03489947644508400310, -0.001077449749359510062 ) ) ;
#97193 = CARTESIAN_POINT ( 'NONE',  ( -3.347801439296141268, 1512.187213306747481, 242.0893193391992497 ) ) ;
#97194 = LINE ( 'NONE', #62540, #28994 ) ;
#97196 = CARTESIAN_POINT ( 'NONE',  ( -16.28895431073521749, 1416.654488107960333, 208.3339384829398853 ) ) ;
#97195 = CARTESIAN_POINT ( 'NONE',  ( 6.943602653455000606, 1516.858069504249897, 216.0629462479770098 ) ) ;
#97197 = CARTESIAN_POINT ( 'NONE',  ( -5.444242866291760130, 1391.534755755089918, 214.9072828329470042 ) ) ;
#97198 = CARTESIAN_POINT ( 'NONE',  ( 10.21694293408019938, 1469.929603999700021, 208.6439139955809878 ) ) ;
#97199 = ORIENTED_EDGE ( 'NONE', *, *, #93972, .F. ) ;
#97200 = CARTESIAN_POINT ( 'NONE',  ( -12.85972207402410028, 1415.932840154009909, 196.7491075114069758 ) ) ;
#97201 = CARTESIAN_POINT ( 'NONE',  ( -6.284474420099999570, 1504.313428625830056, 181.0267274810979927 ) ) ;
#97202 = ORIENTED_EDGE ( 'NONE', *, *, #102943, .F. ) ;
#97203 = CARTESIAN_POINT ( 'NONE',  ( 11.60004869885204570, 1426.721831229858708, 134.4552184562548121 ) ) ;
#97204 = CARTESIAN_POINT ( 'NONE',  ( 11.05580244138281110, 1434.160380231334329, 151.7245384693764265 ) ) ;
#97206 = B_SPLINE_CURVE_WITH_KNOTS ( 'NONE', 3,
 ( #28329, #62521, #12632, #10418, #96643, #63616, #36181, #46809, #89336, #70364, #104480, #19912, #61963, #106139, #72547, #45153, #19352, #10979, #71480, #72023, #3157, #79293, #11534, #46265, #106678, #61405, #2604, #36728, #97733, #80393, #54113, #21004, #45708, #28884, #97179, #20453, #12072, #83683, #89881, #40032, #47336 ),
 .UNSPECIFIED., .F., .F.,
 ( 4, 2, 2, 2, 2, 2, 2, 2, 1, 2, 2, 2, 1, 2, 2, 2, 1, 2, 2, 2, 2, 4 ),
 ( 0.000000000000000000, 0.2500000000005749845, 0.3750000000008624768, 0.4375000000010931811, 0.4687500000011134427, 0.5000000000011337598, 0.6250000000012745360, 0.6875000000013369306, 0.7187500000013611334, 0.7343750000012517765, 0.7500000000011425305, 0.8125000000011113332, 0.8437500000009711121, 0.8593750000007701617, 0.8750000000005691003, 0.9374999999997651878, 0.9531249999996305178, 0.9609374999996921352, 0.9687499999997537525, 0.9765624999998152589, 0.9843749999998768763, 1.000000000000000000 ),
 .UNSPECIFIED. ) ;
#97205 = CARTESIAN_POINT ( 'NONE',  ( 8.629219820895000836, 1511.600194708689969, 203.2115927965309936 ) ) ;
#97207 = UNCERTAINTY_MEASURE_WITH_UNIT (LENGTH_MEASURE( 1.000000000000000082E-05 ), #106100, 'distance_accuracy_value', 'NONE');
#97208 = CARTESIAN_POINT ( 'NONE',  ( 1.786066050100000080, 1443.335463714089883, 217.8608858550190064 ) ) ;
#97209 = CARTESIAN_POINT ( 'NONE',  ( 16.27911523319127696, 1421.519124619010199, 227.2603791194927112 ) ) ;
#97210 = B_SPLINE_CURVE_WITH_KNOTS ( 'NONE', 5,
 ( #93626, #58408, #76301, #60627, #101472, #109367, #8527, #34291, #110451, #32645, #50006, #41603, #33730, #42703, #33183, #66822, #76859, #94750, #92533, #58957, #68474, #93090, #102575, #60073 ),
 .UNSPECIFIED., .F., .F.,
 ( 6, 3, 3, 3, 3, 3, 3, 6 ),
 ( 0.000000000000000000, 0.03529544314845208669, 0.06179047381933735344, 0.08828550449022262714, 0.1412755658236120593, 0.2826075209337656768, 0.5644368487256844480, 1.000000000000000000 ),
 .UNSPECIFIED. ) ;
#97211 = CARTESIAN_POINT ( 'NONE',  ( 7.066689964004210012, 1470.190416163020245, 190.3198042189900150 ) ) ;
#97212 = CARTESIAN_POINT ( 'NONE',  ( -18.48452897440000342, 1425.095849964330000, 227.3281627736979829 ) ) ;
#97213 = CARTESIAN_POINT ( 'NONE',  ( -18.88473658259999866, 1435.156969464529766, 145.0455764213979819 ) ) ;
#97214 = CARTESIAN_POINT ( 'NONE',  ( -19.41733818020000157, 1465.673979701889948, 205.2701344044189966 ) ) ;
#97215 = CARTESIAN_POINT ( 'NONE',  ( 17.53366402320000006, 1416.208575665629951, 192.2869590761980021 ) ) ;
#97217 = CARTESIAN_POINT ( 'NONE',  ( -18.56596160438178345, 1436.937764507165639, 212.4410944778063879 ) ) ;
#97216 = CARTESIAN_POINT ( 'NONE',  ( 0.5470371568191350065, 1409.436771746549994, 232.9505920115730078 ) ) ;
#97218 = DIRECTION ( 'NONE',  ( 0.9510565162951496454, 0.000000000000000000, -0.3090169943749593862 ) ) ;
#97219 = ORIENTED_EDGE ( 'NONE', *, *, #75435, .T. ) ;
#97220 = CARTESIAN_POINT ( 'NONE',  ( -2.109962112465985307, 1410.360755925830745, 186.3561355254459215 ) ) ;
#97221 = CARTESIAN_POINT ( 'NONE',  ( -13.17280652390000029, 1508.540907300989829, 216.8072460398490193 ) ) ;
#97222 = B_SPLINE_CURVE_WITH_KNOTS ( 'NONE', 5,
 ( #42761, #67432, #93149, #33242, #34356, #92592 ),
 .UNSPECIFIED., .F., .F.,
 ( 6, 6 ),
 ( -1.999999979519569981, 0.000000000000000000 ),
 .UNSPECIFIED. ) ;
#97223 = CARTESIAN_POINT ( 'NONE',  ( 15.90990255763500016, 1516.551704408390151, 198.1616908427670296 ) ) ;
#97224 = EDGE_CURVE ( 'NONE', #51642, #88625, #108626, .T. ) ;
#97225 = CYLINDRICAL_SURFACE ( 'NONE', #14467, 0.9999999999999988898 ) ;
#97226 = CARTESIAN_POINT ( 'NONE',  ( -2.710273452790000093, 1484.982664535189770, 198.3319090041989909 ) ) ;
#97227 = CARTESIAN_POINT ( 'NONE',  ( -18.46505093760000094, 1509.557874173729942, 231.0973782673979713 ) ) ;
#97228 = CARTESIAN_POINT ( 'NONE',  ( 0.2759407239221501884, 1408.922696449764544, 231.7129903492111396 ) ) ;
#97229 = CARTESIAN_POINT ( 'NONE',  ( 12.18840501149665201, 1435.566324351502544, 151.0986007949610439 ) ) ;
#97230 = CARTESIAN_POINT ( 'NONE',  ( 4.363122647530000009, 1422.407399603929889, 168.7758374889979791 ) ) ;
#97231 = CARTESIAN_POINT ( 'NONE',  ( 5.989314528585920172, 1494.629792490379941, 219.4239423612390283 ) ) ;
#97232 = CARTESIAN_POINT ( 'NONE',  ( -9.853265956016100446, 1488.872806762260097, 215.5614415617639850 ) ) ;
#97233 = CARTESIAN_POINT ( 'NONE',  ( -13.32684181309999971, 1469.522592936189994, 191.9925905970989959 ) ) ;
#97234 = CARTESIAN_POINT ( 'NONE',  ( -89.28949325252699509, 1383.770769996720219, 308.2764280168249797 ) ) ;
#97235 = CARTESIAN_POINT ( 'NONE',  ( -108.8493753602240020, 1383.998071234949975, 311.1481355889490032 ) ) ;
#97236 = CARTESIAN_POINT ( 'NONE',  ( -0.5542586829518019176, 1516.774419107840004, 201.4065265889630041 ) ) ;
#97238 = ORIENTED_EDGE ( 'NONE', *, *, #71049, .F. ) ;
#97237 = CARTESIAN_POINT ( 'NONE',  ( 20.61689931789999974, 1509.299814820330084, 189.0201468792980108 ) ) ;
#97239 = CARTESIAN_POINT ( 'NONE',  ( -113.4000000000000057, 1383.754957750760013, 311.0314894602589675 ) ) ;
#97240 = CARTESIAN_POINT ( 'NONE',  ( 13.40617544342749845, 1512.633419863019981, 224.4245124526530049 ) ) ;
#97241 = ORIENTED_EDGE ( 'NONE', *, *, #26674, .F. ) ;
#97242 = VERTEX_POINT ( 'NONE', #110745 ) ;
#97243 = CARTESIAN_POINT ( 'NONE',  ( 25.33052504582559905, 1453.000140514270015, 207.7150163121590083 ) ) ;
#97244 = CARTESIAN_POINT ( 'NONE',  ( -109.5348967119999912, 1384.904918197099732, 297.1231116118590307 ) ) ;
#97245 = CARTESIAN_POINT ( 'NONE',  ( 12.77355678467065303, 1442.835118811306529, 169.4523574570036430 ) ) ;
#97247 = CARTESIAN_POINT ( 'NONE',  ( -29.87496815480000123, 1442.835664418360011, 238.0574314900979971 ) ) ;
#97246 = CARTESIAN_POINT ( 'NONE',  ( 39.46380715081631507, 1430.354105498958688, 269.6007763216737203 ) ) ;
#97248 = CARTESIAN_POINT ( 'NONE',  ( -20.08779309810000058, 1491.274044621930216, 190.8703246068980093 ) ) ;
#97249 = CARTESIAN_POINT ( 'NONE',  ( -11.38815357430000041, 1433.875739129769954, 151.4350069040980031 ) ) ;
#97250 = CARTESIAN_POINT ( 'NONE',  ( 26.20829668540000057, 1507.984234506930079, 201.9879544258380122 ) ) ;
#97251 = CARTESIAN_POINT ( 'NONE',  ( -19.21256531279999891, 1485.592793457429934, 189.7209763221979983 ) ) ;
#97252 = CARTESIAN_POINT ( 'NONE',  ( -7.499365986679999985, 1445.290603318090007, 216.2717625584189989 ) ) ;
#97253 = CARTESIAN_POINT ( 'NONE',  ( 5.044474169190000801, 1422.662929545129828, 184.9412868827979821 ) ) ;
#97254 = CARTESIAN_POINT ( 'NONE',  ( 0.2432117948283340214, 1515.155210303460080, 213.4489270742160159 ) ) ;
#97255 = CARTESIAN_POINT ( 'NONE',  ( 7.733452464780000035, 1440.968359251539823, 154.0956077494979866 ) ) ;
#97256 = CARTESIAN_POINT ( 'NONE',  ( 12.63038619288439968, 1428.207532477410041, 223.9332333053530135 ) ) ;
#97257 = CARTESIAN_POINT ( 'NONE',  ( 0.3083741877719999858, 1507.133244740429973, 237.3561682571980214 ) ) ;
#97259 = ORIENTED_EDGE ( 'NONE', *, *, #76038, .F. ) ;
#97258 = CARTESIAN_POINT ( 'NONE',  ( 1.396945595908719806, 1473.097535771269804, 219.2356281669150064 ) ) ;
#97260 = ORIENTED_EDGE ( 'NONE', *, *, #14146, .F. ) ;
#97261 = CARTESIAN_POINT ( 'NONE',  ( 30.31940284292409515, 1518.913060387330006, 195.7503880523414352 ) ) ;
#97262 = EDGE_CURVE ( 'NONE', #88507, #87844, #85526, .T. ) ;
#97263 = ADVANCED_FACE ( 'NONE', ( #95603 ), #34037, .F. ) ;
#97264 = CARTESIAN_POINT ( 'NONE',  ( 16.46134999639999563, 1495.070035120589864, 192.9350266946989905 ) ) ;
#97265 = CARTESIAN_POINT ( 'NONE',  ( -20.73365673589999858, 1470.033777940730033, 270.3294707277980251 ) ) ;
#97266 = CARTESIAN_POINT ( 'NONE',  ( -23.76173655485600378, 1436.066805062839194, 211.6885914087122558 ) ) ;
#97267 = CARTESIAN_POINT ( 'NONE',  ( 16.60786453549999919, 1409.493019796529779, 222.4680777416979822 ) ) ;
#97268 = EDGE_CURVE ( 'NONE', #95724, #79870, #87128, .T. ) ;
#97269 = CARTESIAN_POINT ( 'NONE',  ( -15.95383389570000077, 1506.798305147730161, 224.6865364803979901 ) ) ;
#97271 = EDGE_CURVE ( 'NONE', #22747, #96120, #19432, .T. ) ;
#97270 = CARTESIAN_POINT ( 'NONE',  ( 0.9776412681320001408, 1475.513060387329915, 187.4983515543979991 ) ) ;
#97272 = CARTESIAN_POINT ( 'NONE',  ( -11.62261217039999828, 1420.448898375830140, 230.7381671621980104 ) ) ;
#97273 = EDGE_CURVE ( 'NONE', #30516, #13874, #33471, .T. ) ;
#97274 =( BOUNDED_SURFACE ( )  B_SPLINE_SURFACE ( 1, 2, ( 
 ( #55977, #45386, #27823 ),
 ( #2093, #103969, #44637 ) ),
 .UNSPECIFIED., .F., .F., .T. ) 
 B_SPLINE_SURFACE_WITH_KNOTS ( ( 2, 2 ),
 ( 3, 3 ),
 ( -10000.00000000000000, 10000.00000000000000 ),
 ( 5.300753508068400066, 6.146881668114829722 ),
 .UNSPECIFIED. ) 
 GEOMETRIC_REPRESENTATION_ITEM ( )  RATIONAL_B_SPLINE_SURFACE ( (
 ( 0.8627701935022100699, 0.8231901671853920632, 0.9535799773420449155),
 ( 0.8627701935022100699, 0.8231901671853920632, 0.9535799773420449155) ) ) 
 REPRESENTATION_ITEM ( '' )  SURFACE ( )  );
#97275 = CARTESIAN_POINT ( 'NONE',  ( -8.977785982439998591, 1459.740360813789948, 212.8396695563389756 ) ) ;
#97276 = CARTESIAN_POINT ( 'NONE',  ( 8.476942927299997876, 1362.523913559720086, 207.6218459616989946 ) ) ;
#97277 = CARTESIAN_POINT ( 'NONE',  ( -45.94972966655959823, 1436.699121074330151, 267.6009661011610206 ) ) ;
#97278 = VERTEX_POINT ( 'NONE', #8820 ) ;
#97279 = DIRECTION ( 'NONE',  ( 0.000000000000000000, 0.000000000000000000, -1.000000000000000000 ) ) ;
#97280 = AXIS2_PLACEMENT_3D ( 'NONE', #68680, #68140, #102251 ) ;
#97281 = ADVANCED_FACE ( 'NONE', ( #26738 ), #1851, .T. ) ;
#97282 = ORIENTED_EDGE ( 'NONE', *, *, #109023, .F. ) ;
#97283 = CARTESIAN_POINT ( 'NONE',  ( 6.951175128784999657, 1517.170721208160103, 211.4121022339570004 ) ) ;
#97284 = CARTESIAN_POINT ( 'NONE',  ( -0.8350686643532190256, 1526.382868172863937, 240.9330574173806951 ) ) ;
#97285 = CARTESIAN_POINT ( 'NONE',  ( 17.60061308773152433, 1410.712255111885952, 224.8086590843146269 ) ) ;
#97286 = DIRECTION ( 'NONE',  ( -1.000000000000000000, 0.000000000000000000, 0.000000000000000000 ) ) ;
#97287 = AXIS2_PLACEMENT_3D ( 'NONE', #20592, #52585, #106278 ) ;
#97288 = DIRECTION ( 'NONE',  ( 0.9455185755993177343, 0.000000000000000000, -0.3255681544571540909 ) ) ;
#97289 = B_SPLINE_SURFACE_WITH_KNOTS ( 'NONE', 5, 5, ( 
 ( #51575, #49922, #92447, #25234, #25789, #81, #67836, #94665, #9551, #68948, #34209, #68393 ),
 ( #35313, #43177, #69499, #59988, #77874, #94105, #58873, #103622, #17376, #1182, #75678, #101382 ),
 ( #77329, #630, #103048, #26346, #60544, #93005, #24675, #86263, #109821, #15721, #84059, #67290 ),
 ( #16279, #50482, #84605, #19605, #61109, #62199, #53807, #10677, #2838, #70061, #89014, #97424 ),
 ( #29119, #80070, #95224, #79535, #78997, #63304, #20693, #96883, #54889, #18486, #104721, #12304 ),
 ( #52683, #20152, #86819, #10111, #46496, #54349, #70603, #28012, #36960, #96327, #28570, #45396 ),
 ( #80628, #44283, #87943, #71154, #3943, #78427, #53241, #11234, #38070, #71723, #105276, #1738 ),
 ( #35877, #104173, #62768, #88480, #27457, #3391, #44844, #61642, #45934, #72247, #37520, #11765 ),
 ( #95772, #19038, #26920, #87382, #2300, #105840, #36411, #4479, #108016, #74450, #6665, #21229 ),
 ( #56536, #13392, #82818, #39157, #65496, #73332, #66053, #108578, #6110, #107466, #57098, #99605 ),
 ( #106374, #30762, #73889, #64943, #47579, #31865, #57655, #40267, #99056, #22336, #90664, #13947 ),
 ( #40819, #48137, #91767, #31312, #82276, #5574, #39724, #22888, #100177, #15045, #91224, #63847 ),
 ( #29662, #14504, #49243, #89568, #38609, #23461, #48694, #90109, #83365, #97959, #81703, #106915 ),
 ( #55439, #12858, #47040, #81164, #72788, #30204, #64395, #98516, #21784, #55985, #5010, #110227 ),
 ( #58735, #50889, #7226, #26214, #34629, #83924, #77202, #17240, #32429, #16689, #16151, #504 ) ),
 .UNSPECIFIED., .F., .F., .F.,
 ( 6, 3, 3, 3, 6 ),
 ( 6, 3, 3, 6 ),
 ( 1.933773958289999984, 17.84603210599999912, 29.17820978809999843, 40.51038747020000130, 63.49323769619999780 ),
 ( 168.7272174100000086, 189.8181195859999946, 210.9090217629999984, 253.0908261149999987 ),
 .UNSPECIFIED. ) ;
#97290 = VERTEX_POINT ( 'NONE', #11605 ) ;
#97291 = CARTESIAN_POINT ( 'NONE',  ( 4.046802277660000335, 1505.460036802790000, 221.2327940266990254 ) ) ;
#97292 = EDGE_CURVE ( 'NONE', #107054, #79161, #22368, .T. ) ;
#97293 = CARTESIAN_POINT ( 'NONE',  ( -1.129386240404999908, 1516.613712827999962, 201.7984555248870038 ) ) ;
#97294 = CARTESIAN_POINT ( 'NONE',  ( 5.133103592700000384, 1472.975266187489979, 218.0948351415289892 ) ) ;
#97295 = EDGE_CURVE ( 'NONE', #50191, #19741, #49581, .T. ) ;
#97296 = CARTESIAN_POINT ( 'NONE',  ( 17.88377006740000397, 1429.006865431090091, 205.7968609931990045 ) ) ;
#97297 = ORIENTED_EDGE ( 'NONE', *, *, #20601, .F. ) ;
#97298 = CARTESIAN_POINT ( 'NONE',  ( -13.23542543278949957, 1410.634354704430052, 270.3664647165679753 ) ) ;
#97299 = CARTESIAN_POINT ( 'NONE',  ( -2.368833328420000051, 1427.018531676430030, 133.6118001900980232 ) ) ;
#97300 = DIRECTION ( 'NONE',  ( -9.520249230476377039E-08, -3.411690578513119204E-09, -0.9999999999999954481 ) ) ;
#97302 = ORIENTED_EDGE ( 'NONE', *, *, #22971, .T. ) ;
#97301 = CARTESIAN_POINT ( 'NONE',  ( -4.517103278725432602, 1368.953374755395998, 210.6218459616987957 ) ) ;
#97303 = EDGE_LOOP ( 'NONE', ( #10073, #99484, #62947, #3845 ) ) ;
#97304 = EDGE_CURVE ( 'NONE', #86829, #2979, #46430, .T. ) ;
#97305 = DIRECTION ( 'NONE',  ( -1.755985294532469921E-16, 1.000000000000000000, -1.338183447452831989E-16 ) ) ;
#97306 = CARTESIAN_POINT ( 'NONE',  ( -0.8168899812832949303, 1467.671549419570056, 220.1953764921350114 ) ) ;
#97307 = CARTESIAN_POINT ( 'NONE',  ( 3.750641173502857306, 1424.073545704406115, 183.6511083008927301 ) ) ;
#97308 = CARTESIAN_POINT ( 'NONE',  ( -27.32596821242635343, 1412.869984779867991, 266.6662420334005219 ) ) ;
#97309 = ADVANCED_FACE ( 'NONE', ( #50037 ), #95701, .F. ) ;
#97310 = CARTESIAN_POINT ( 'NONE',  ( -17.98740375195779606, 1415.258594619250061, 207.5661176034399773 ) ) ;
#97311 = CARTESIAN_POINT ( 'NONE',  ( 2.511983255966640183, 1439.367848956780108, 157.7248713869030325 ) ) ;
#97312 = CARTESIAN_POINT ( 'NONE',  ( -14.40866948829999927, 1423.490938386730022, 221.9456809809980200 ) ) ;
#97313 = CARTESIAN_POINT ( 'NONE',  ( 12.44325168979999852, 1415.996778985530000, 223.2102471899980003 ) ) ;
#97314 = CARTESIAN_POINT ( 'NONE',  ( 4.219439073160000220, 1446.230224797059918, 182.3842143240980249 ) ) ;
#97315 = CARTESIAN_POINT ( 'NONE',  ( -6.562635860634999929, 1517.111322026010157, 206.2508942643169974 ) ) ;
#97316 = ORIENTED_EDGE ( 'NONE', *, *, #26715, .T. ) ;
#97317 = CARTESIAN_POINT ( 'NONE',  ( 5.164931156380000507E-11, 1452.913060387330006, 179.9625354400980086 ) ) ;
#97318 = CARTESIAN_POINT ( 'NONE',  ( -22.63601521178858533, 1451.224009660701086, 219.0470436816254391 ) ) ;
#97319 = ORIENTED_EDGE ( 'NONE', *, *, #24086, .F. ) ;
#97320 = CARTESIAN_POINT ( 'NONE',  ( 10.54139892624155728, 1455.171105620551089, 226.3039058597585438 ) ) ;
#97321 = CARTESIAN_POINT ( 'NONE',  ( 25.25148443142990118, 1451.314349325280091, 137.1731793465510236 ) ) ;
#97322 = CARTESIAN_POINT ( 'NONE',  ( -4.987078442593329441, 1508.551704408389924, 211.6097810465890063 ) ) ;
#97323 = CARTESIAN_POINT ( 'NONE',  ( -22.99718798410000176, 1386.621894033409944, 202.4024127538190214 ) ) ;
#97324 = DIRECTION ( 'NONE',  ( -1.755985294532469921E-16, 1.000000000000000000, -1.338183447452831989E-16 ) ) ;
#97325 = DIRECTION ( 'NONE',  ( -0.6736849260863841948, 0.000000000000000000, 0.7390186874254148774 ) ) ;
#97326 = CARTESIAN_POINT ( 'NONE',  ( -3.313293292670107082, 1446.583016671109135, 170.5342543429541422 ) ) ;
#97327 = CARTESIAN_POINT ( 'NONE',  ( 16.34140767499999924, 1409.483715582329978, 225.5328183092979941 ) ) ;
#97328 = CARTESIAN_POINT ( 'NONE',  ( 10.17747861530000009, 1489.224014057989962, 204.9037901253090013 ) ) ;
#97329 = CARTESIAN_POINT ( 'NONE',  ( 21.69285400322056745, 1453.394215773794485, 220.8286852162956677 ) ) ;
#97330 = CARTESIAN_POINT ( 'NONE',  ( 2.500000000000000000, 1439.547542061109880, 164.8613946483260122 ) ) ;
#97331 = CARTESIAN_POINT ( 'NONE',  ( -2.288357445734999995, 1517.116049120239950, 214.9102823043970147 ) ) ;
#97332 = CARTESIAN_POINT ( 'NONE',  ( 2.708183792730093131, 1524.374142163904480, 241.9870236838057735 ) ) ;
#97333 = ORIENTED_EDGE ( 'NONE', *, *, #92582, .T. ) ;
#97334 = CARTESIAN_POINT ( 'NONE',  ( 7.722580314274999580, 1517.051704408389924, 210.6910072246569996 ) ) ;
#97335 = CARTESIAN_POINT ( 'NONE',  ( 21.13130013988323341, 1524.397344074318880, 237.4101150494052490 ) ) ;
#97336 = CARTESIAN_POINT ( 'NONE',  ( -12.98226713004480004, 1414.913060387349788, 219.9156686614909972 ) ) ;
#97337 = ADVANCED_FACE ( 'NONE', ( #53928 ), #64511, .F. ) ;
#97338 = DIRECTION ( 'NONE',  ( 1.000000000000000000, -2.735358204715540176E-15, 3.765374186129670039E-15 ) ) ;
#97339 = EDGE_CURVE ( 'NONE', #63865, #92743, #110382, .T. ) ;
#97340 = CARTESIAN_POINT ( 'NONE',  ( -40.10575600315020495, 1445.309576473759989, 136.9127853735360247 ) ) ;
#97341 = CARTESIAN_POINT ( 'NONE',  ( 11.60004869885571743, 1425.366405675970555, 138.1206266335812245 ) ) ;
#97342 = CARTESIAN_POINT ( 'NONE',  ( -19.37374569213963582, 1526.382868172863937, 183.8768763279542213 ) ) ;
#97343 = CARTESIAN_POINT ( 'NONE',  ( 11.75869035672759999, 1519.551704408389924, 227.2994842695800060 ) ) ;
#97344 = CARTESIAN_POINT ( 'NONE',  ( 11.86848022610000086, 1433.047056341809821, 150.2049543995979946 ) ) ;
#97345 = DIRECTION ( 'NONE',  ( -2.093802707073269138E-06, 0.4875922912088249683, 0.8730714504262205855 ) ) ;
#97346 = CARTESIAN_POINT ( 'NONE',  ( -9.559981065551120594, 1460.552225690790237, 210.5447656127829816 ) ) ;
#97347 = CARTESIAN_POINT ( 'NONE',  ( -109.3493290679999888, 1385.139709706009853, 297.1446333424589739 ) ) ;
#97348 = CARTESIAN_POINT ( 'NONE',  ( 10.03746411003220018, 1501.098977471080161, 203.4535166149570102 ) ) ;
#97349 = ORIENTED_EDGE ( 'NONE', *, *, #20045, .T. ) ;
#97350 = DIRECTION ( 'NONE',  ( -1.000000000000000000, 0.000000000000000000, 0.000000000000000000 ) ) ;
#97351 = VECTOR ( 'NONE', #30666, 999.9999999999998863 ) ;
#97352 = CARTESIAN_POINT ( 'NONE',  ( 11.23388613411650638, 1445.063428794548372, 150.9272215568491049 ) ) ;
#97353 = EDGE_CURVE ( 'NONE', #1550, #49802, #10236, .T. ) ;
#97354 = FACE_OUTER_BOUND ( 'NONE', #18823, .T. ) ;
#97355 = CARTESIAN_POINT ( 'NONE',  ( 7.146055568748121090, 1398.125191567241473, 198.2455685561245673 ) ) ;
#97356 = CARTESIAN_POINT ( 'NONE',  ( 1.712115011030000078, 1498.987102142929871, 236.1549197522979853 ) ) ;
#97357 = CIRCLE ( 'NONE', #49111, 1.000000000000000888 ) ;
#97358 = CARTESIAN_POINT ( 'NONE',  ( -17.04790460295919630, 1526.208281990536761, 235.6077665793768574 ) ) ;
#97359 = CARTESIAN_POINT ( 'NONE',  ( -17.25705191650000003, 1509.016679771029885, 230.6108905181980333 ) ) ;
#97360 = CARTESIAN_POINT ( 'NONE',  ( -18.70316107891150281, 1383.854929796499846, 220.2675684361349795 ) ) ;
#97361 = CARTESIAN_POINT ( 'NONE',  ( -16.11867490360164368, 1414.913060387329779, 208.6659696099576422 ) ) ;
#97362 = CARTESIAN_POINT ( 'NONE',  ( -14.45258105951289807, 1415.677402202029953, 212.7925583759839867 ) ) ;
#97363 = CARTESIAN_POINT ( 'NONE',  ( 2.562182094880000260, 1464.635166048130031, 236.5709022716980030 ) ) ;
#97365 = EDGE_LOOP ( 'NONE', ( #27079, #52380, #49176, #37672 ) ) ;
#97364 = CARTESIAN_POINT ( 'NONE',  ( 9.395113974487038888, 1451.852228830569857, 209.9056078797769942 ) ) ;
#97366 = B_SPLINE_CURVE_WITH_KNOTS ( 'NONE', 5,
 ( #75716, #58914, #16318, #58363, #110405, #7940 ),
 .UNSPECIFIED., .F., .F.,
 ( 6, 6 ),
 ( -2.000000000000000000, 0.000000000000000000 ),
 .UNSPECIFIED. ) ;
#97367 = CARTESIAN_POINT ( 'NONE',  ( -1.483649241179999967, 1450.644272461199762, 182.4983721051980012 ) ) ;
#97368 = ADVANCED_FACE ( 'NONE', ( #91346 ), #21537, .F. ) ;
#97369 = CARTESIAN_POINT ( 'NONE',  ( -5.962417602059999489, 1383.866448007470126, 218.3533362890090075 ) ) ;
#97370 = CARTESIAN_POINT ( 'NONE',  ( -20.58126087740000187, 1507.779106712530165, 190.0921675882979969 ) ) ;
#97372 = VERTEX_POINT ( 'NONE', #46618 ) ;
#97371 = CARTESIAN_POINT ( 'NONE',  ( 27.01381218759999925, 1450.681579806120226, 136.4483250053980044 ) ) ;
#97373 = CARTESIAN_POINT ( 'NONE',  ( -12.04604675982380080, 1481.197891243110007, 227.9689080549119922 ) ) ;
#97374 = VERTEX_POINT ( 'NONE', #38183 ) ;
#97375 = PRODUCT_DEFINITION_SHAPE ( 'NONE', 'NONE',  #110835 ) ;
#97376 = CARTESIAN_POINT ( 'NONE',  ( -10.45628814230000181, 1390.721297460369897, 215.7199839781590072 ) ) ;
#97377 = CARTESIAN_POINT ( 'NONE',  ( 11.89599453232379922, 1434.596263782940014, 147.6475367373340077 ) ) ;
#97378 = ADVANCED_FACE ( 'NONE', ( #98632 ), #4587, .T. ) ;
#97379 = DIRECTION ( 'NONE',  ( 0.9455185755993178454, 0.000000000000000000, -0.3255681544571537578 ) ) ;
#97380 = CARTESIAN_POINT ( 'NONE',  ( -14.73654635989563033, 1420.116477539524567, 213.6061976603614596 ) ) ;
#97381 = CARTESIAN_POINT ( 'NONE',  ( 3.347801439372898979, 1523.456924617337336, 242.0893193391914622 ) ) ;
#97382 = CARTESIAN_POINT ( 'NONE',  ( 12.49050510308880035, 1409.349238429849720, 217.3209073824620248 ) ) ;
#97383 = CIRCLE ( 'NONE', #6181, 2.000000000000001776 ) ;
#97384 = CARTESIAN_POINT ( 'NONE',  ( 18.03628730299999816, 1424.824108734929723, 224.7110847794980089 ) ) ;
#97385 = CARTESIAN_POINT ( 'NONE',  ( -106.7907400783429921, 1385.237181466299944, 297.0459356838589997 ) ) ;
#97386 = CARTESIAN_POINT ( 'NONE',  ( -18.21568074059999987, 1430.634797966130009, 192.8606760977980059 ) ) ;
#97387 = CARTESIAN_POINT ( 'NONE',  ( 11.57624701549999990, 1432.320296800590086, 151.1967064319979670 ) ) ;
#97388 = B_SPLINE_CURVE_WITH_KNOTS ( 'NONE', 5,
 ( #85484, #33427, #65556, #9357, #14569, #84937 ),
 .UNSPECIFIED., .F., .F.,
 ( 6, 6 ),
 ( 0.000000000000000000, 11.48858425020000240 ),
 .UNSPECIFIED. ) ;
#97389 = CARTESIAN_POINT ( 'NONE',  ( 10.83489300642449926, 1489.711129298920014, 207.6370862455599990 ) ) ;
#97390 = ORIENTED_EDGE ( 'NONE', *, *, #78951, .F. ) ;
#97391 = ORIENTED_EDGE ( 'NONE', *, *, #73078, .T. ) ;
#97392 = EDGE_CURVE ( 'NONE', #101083, #96593, #59915, .T. ) ;
#97393 = CARTESIAN_POINT ( 'NONE',  ( -7.203707716490680646, 1508.728101425919931, 215.8474337165719987 ) ) ;
#97395 = AXIS2_PLACEMENT_3D ( 'NONE', #12900, #38109, #7805 ) ;
#97394 = CARTESIAN_POINT ( 'NONE',  ( -2.745154014197499937, 1419.769956470485113, 137.0999999980979851 ) ) ;
#97396 = CARTESIAN_POINT ( 'NONE',  ( -3.190252885392550475, 1495.655215145649890, 197.2101252161220089 ) ) ;
#97397 = EDGE_CURVE ( 'NONE', #43603, #86830, #83478, .T. ) ;
#97398 = CARTESIAN_POINT ( 'NONE',  ( 21.90260416155314260, 1466.954533459972936, 269.4017626923731541 ) ) ;
#97399 = CARTESIAN_POINT ( 'NONE',  ( -30.51126001304308133, 1526.382868172863937, 219.8557927178091518 ) ) ;
#97400 = CARTESIAN_POINT ( 'NONE',  ( 7.491155460734093552, 1414.913060387329779, 223.8341484298593684 ) ) ;
#97401 = CARTESIAN_POINT ( 'NONE',  ( 21.91582124097350004, 1491.015010933479971, 209.7149842846540082 ) ) ;
#97402 = CARTESIAN_POINT ( 'NONE',  ( -0.8687435992890001346, 1453.579571206030096, 183.3443055433980078 ) ) ;
#97403 = CARTESIAN_POINT ( 'NONE',  ( -12.04343452997959041, 1364.919544789908969, 209.6218459617033432 ) ) ;
#97404 = FACE_OUTER_BOUND ( 'NONE', #63797, .T. ) ;
#97405 = EDGE_CURVE ( 'NONE', #17368, #8750, #42856, .T. ) ;
#97406 = CARTESIAN_POINT ( 'NONE',  ( -5.014195139944999546, 1517.120861839400050, 207.4163795216369977 ) ) ;
#97407 = DIRECTION ( 'NONE',  ( 0.003563285688556391394, -0.9999913849417920719, 0.002129093069402243805 ) ) ;
#97408 = CARTESIAN_POINT ( 'NONE',  ( 30.61611611309609415, 1526.069472839382797, 201.6871119896542268 ) ) ;
#97409 = B_SPLINE_SURFACE_WITH_KNOTS ( 'NONE', 5, 5, ( 
 ( #73076, #47866, #88772, #47316, #97163, #98260 ),
 ( #4751, #37816, #97712, #3688, #22621, #13132 ),
 ( #20984, #106657, #56824, #106117, #72003, #82001 ),
 ( #31054, #30504, #64693, #105578, #38893, #46790 ),
 ( #29393, #80919, #14247, #81440, #48436, #65235 ),
 ( #38347, #63594, #89863, #4218, #82578, #12055 ) ),
 .UNSPECIFIED., .F., .F., .F.,
 ( 6, 6 ),
 ( 6, 6 ),
 ( 113.0406221479999971, 134.6442539944619909 ),
 ( 0.3006958241500000129, 0.4689188458459999653 ),
 .UNSPECIFIED. ) ;
#97410 = CARTESIAN_POINT ( 'NONE',  ( 19.54165283311759893, 1409.595469941420106, 199.8969299576039873 ) ) ;
#97411 = FACE_OUTER_BOUND ( 'NONE', #53522, .T. ) ;
#97412 = CARTESIAN_POINT ( 'NONE',  ( -15.72154079564279705, 1469.202802763679983, 228.9466779226059714 ) ) ;
#97413 = EDGE_CURVE ( 'NONE', #91917, #76557, #6341, .T. ) ;
#97414 = ADVANCED_FACE ( 'NONE', ( #16258 ), #78717, .T. ) ;
#97415 = CARTESIAN_POINT ( 'NONE',  ( 41.65640094522370163, 1444.002002823209978, 135.7347776446760008 ) ) ;
#97416 = VERTEX_POINT ( 'NONE', #53219 ) ;
#97417 = CARTESIAN_POINT ( 'NONE',  ( 28.33103133730000067, 1431.247806717339927, 240.1819618771980061 ) ) ;
#97418 = CARTESIAN_POINT ( 'NONE',  ( -20.81017607009999892, 1469.236365769730128, 194.6575948795980082 ) ) ;
#97420 = CARTESIAN_POINT ( 'NONE',  ( -17.57263965230000125, 1409.691669017629920, 195.6049322489980113 ) ) ;
#97419 = CARTESIAN_POINT ( 'NONE',  ( -10.74627445883099952, 1425.683497583799863, 97.52444174273580302 ) ) ;
#97421 = B_SPLINE_CURVE_WITH_KNOTS ( 'NONE', 5,
 ( #23872, #13818, #73771, #48003, #5992, #107895, #65374, #91649, #31188, #74868, #108455, #31737 ),
 .UNSPECIFIED., .F., .F.,
 ( 6, 3, 3, 6 ),
 ( 0.000000000000000000, 0.4515349285676349966, 0.7455155029937545752, 1.000000000000000000 ),
 .UNSPECIFIED. ) ;
#97422 = FACE_OUTER_BOUND ( 'NONE', #30680, .T. ) ;
#97423 = B_SPLINE_CURVE_WITH_KNOTS ( 'NONE', 3,
 ( #98709, #46142, #30953, #47217, #89214, #90856, #4658, #38797, #21969, #47764, #99241, #22517, #91959, #33695, #102544, #15236, #76822, #33150, #25837, #49970, #41571, #92501, #6843, #60038, #24727, #68441, #14698, #23651, #67338, #34259, #85204, #24186, #75182, #110415, #74629, #66246, #50528, #83015, #101437, #41004 ),
 .UNSPECIFIED., .F., .F.,
 ( 4, 1, 1, 1, 1, 2, 2, 1, 1, 1, 2, 2, 1, 1, 2, 2, 1, 1, 1, 1, 2, 2, 1, 1, 1, 2, 2, 4 ),
 ( 0.000000000000000000, 0.06249999999983144039, 0.09374999999974716058, 0.1093749999997047639, 0.1171874999996835309, 0.1210937499996792149, 0.1249999999996748989, 0.1874999999995648203, 0.2187499999995081157, 0.2343749999994797772, 0.2421874999994653443, 0.2499999999994509392, 0.3749999999992617572, 0.4374999999991670552, 0.4687499999991197042, 0.4999999999990722976, 0.5624999999990122346, 0.5937499999989822586, 0.6093749999989873656, 0.6171874999989899191, 0.6210937499989912514, 0.6249999999989925836, 0.6874999999992860156, 0.7187499999994573230, 0.7343749999995197175, 0.7421874999995508038, 0.7499999999995818900, 1.000000000000000000 ),
 .UNSPECIFIED. ) ;
#97424 = CARTESIAN_POINT ( 'NONE',  ( 1.852756268550000001E-09, 1409.477339444430072, 259.9484415776979631 ) ) ;
#97425 = CARTESIAN_POINT ( 'NONE',  ( 1.209344357960000282, 1487.394827286090049, 219.9223287670990032 ) ) ;
#97426 = CARTESIAN_POINT ( 'NONE',  ( 3.373940653401940715, 1447.285893942237180, 154.8523594219587665 ) ) ;
#97427 = CARTESIAN_POINT ( 'NONE',  ( 32.74960620270000078, 1451.769474672029901, 135.1835671602979971 ) ) ;
#97428 = ORIENTED_EDGE ( 'NONE', *, *, #100623, .F. ) ;
#97429 = CARTESIAN_POINT ( 'NONE',  ( -2.500000000000000000, 1426.216228438830058, 155.9944625376979843 ) ) ;
#97430 = CARTESIAN_POINT ( 'NONE',  ( 13.24077306275803068, 1513.560745840759637, 225.9062032717914974 ) ) ;
#97431 = FACE_OUTER_BOUND ( 'NONE', #12274, .T. ) ;
#97432 = ORIENTED_EDGE ( 'NONE', *, *, #53466, .F. ) ;
#97433 = VERTEX_POINT ( 'NONE', #53789 ) ;
#97434 = B_SPLINE_CURVE_WITH_KNOTS ( 'NONE', 3,
 ( #43214, #101984, #7935, #69536, #77363, #664, #17974, #93581, #34795, #51609, #17412, #33135, #67874, #59471, #16857, #33680, #18521, #102530, #67323, #25822, #10145, #51061, #34245, #84638, #85191, #42105, #85743, #24712, #60023, #52170 ),
 .UNSPECIFIED., .F., .F.,
 ( 4, 2, 2, 2, 1, 1, 1, 1, 2, 2, 2, 2, 1, 2, 2, 1, 2, 4 ),
 ( 0.000000000000000000, 0.2499999999997336020, 0.3749999999995978217, 0.4374999999995382582, 0.4687499999995027311, 0.4843749999994849675, 0.4921874999994722000, 0.4960937499994640953, 0.4980468749994599875, 0.4999999999994559352, 0.7499999999995180522, 0.8124999999995377031, 0.8281249999995426991, 0.8320312499995468070, 0.8359374999995510258, 0.8437499999995592415, 0.8749999999996469491, 1.000000000000000000 ),
 .UNSPECIFIED. ) ;
#97435 = CIRCLE ( 'NONE', #86640, 26.99999999999999645 ) ;
#97436 = CARTESIAN_POINT ( 'NONE',  ( 9.200833838318960289, 1451.501850391510061, 210.2568363721279923 ) ) ;
#97437 = CARTESIAN_POINT ( 'NONE',  ( 5.639791218109999171, 1424.329486380210028, 193.4460986586989861 ) ) ;
#97438 = ORIENTED_EDGE ( 'NONE', *, *, #59635, .F. ) ;
#97439 = CARTESIAN_POINT ( 'NONE',  ( -1.361182826989999928, 1413.855685395729779, 185.4547579133979980 ) ) ;
#97440 = CARTESIAN_POINT ( 'NONE',  ( -5.815894185941668404, 1419.536499247897382, 194.8620236102833871 ) ) ;
#97442 = EDGE_CURVE ( 'NONE', #4434, #69179, #51399, .T. ) ;
#97441 = CIRCLE ( 'NONE', #43815, 1.999999999999999556 ) ;
#97443 = CARTESIAN_POINT ( 'NONE',  ( 0.5253559788449999601, 1450.894714552289997, 181.2879659622979887 ) ) ;
#97444 = CARTESIAN_POINT ( 'NONE',  ( -0.7153112824419999294, 1489.065501047429962, 236.4817586033979921 ) ) ;
#97445 = CARTESIAN_POINT ( 'NONE',  ( 17.19739463999658113, 1525.960063244516959, 236.2603809477409982 ) ) ;
#97446 = ORIENTED_EDGE ( 'NONE', *, *, #39098, .F. ) ;
#97447 = CARTESIAN_POINT ( 'NONE',  ( 11.63668813159999971, 1425.864839735429769, 144.1681848196979843 ) ) ;
#97448 = CARTESIAN_POINT ( 'NONE',  ( -12.65294384001009931, 1415.935475482089942, 221.7859427658239895 ) ) ;
#97449 = CARTESIAN_POINT ( 'NONE',  ( 13.73732212659999874, 1452.821288644329798, 224.4407649501980018 ) ) ;
#97450 = ORIENTED_EDGE ( 'NONE', *, *, #105493, .F. ) ;
#97451 = CARTESIAN_POINT ( 'NONE',  ( -7.721907926364999675, 1517.026025493960105, 204.1173703575669833 ) ) ;
#97452 = ORIENTED_EDGE ( 'NONE', *, *, #27805, .F. ) ;
#97453 = CARTESIAN_POINT ( 'NONE',  ( 11.84627492255189907, 1430.966456813360082, 149.8093626651640022 ) ) ;
#97454 = CARTESIAN_POINT ( 'NONE',  ( 12.53380665967529950, 1445.052233242549846, 186.0874955919830143 ) ) ;
#97455 = ORIENTED_EDGE ( 'NONE', *, *, #54235, .F. ) ;
#97456 = EDGE_LOOP ( 'NONE', ( #25985, #910 ) ) ;
#97457 = FACE_OUTER_BOUND ( 'NONE', #82617, .T. ) ;
#97458 = CARTESIAN_POINT ( 'NONE',  ( -29.65946186579084909, 1526.335487865669165, 216.9928009627314225 ) ) ;
#97459 = CARTESIAN_POINT ( 'NONE',  ( 3.714835820328249660, 1497.588999516199920, 197.6014933246789838 ) ) ;
#97460 = CARTESIAN_POINT ( 'NONE',  ( -8.267101759600800293, 1469.515716270360144, 216.2369933283739840 ) ) ;
#97461 = DIRECTION ( 'NONE',  ( 0.9455185755993178454, 0.000000000000000000, -0.3255681544571539243 ) ) ;
#97462 = CARTESIAN_POINT ( 'NONE',  ( 11.73531390670000008, 1420.449078066779975, 199.2341047989489766 ) ) ;
#97463 = CARTESIAN_POINT ( 'NONE',  ( -2.391424667983720109, 1476.089688646680088, 220.3288384573359906 ) ) ;
#97464 = CARTESIAN_POINT ( 'NONE',  ( -107.4477384240240099, 1379.886883745280102, 299.0757736425410371 ) ) ;
#97465 = LINE ( 'NONE', #13989, #12614 ) ;
#97466 = CARTESIAN_POINT ( 'NONE',  ( 0.02513987172886716220, 1410.234108419300810, 233.2181343497910575 ) ) ;
#97468 = CARTESIAN_POINT ( 'NONE',  ( -106.4065864580110059, 1391.913060387289988, 304.8084661972009712 ) ) ;
#97467 = CARTESIAN_POINT ( 'NONE',  ( -16.36114452500000027, 1503.966594772790131, 208.9878484538460270 ) ) ;
#97469 = CARTESIAN_POINT ( 'NONE',  ( -14.08142637225379978, 1379.709117121690042, 211.5303641152310092 ) ) ;
#97470 = CARTESIAN_POINT ( 'NONE',  ( -24.03340273735519972, 1507.991624071270053, 222.3151666817440173 ) ) ;
#97471 = CARTESIAN_POINT ( 'NONE',  ( -7.942827010805000754, 1514.298059036109862, 202.2691041254170159 ) ) ;
#97472 = ORIENTED_EDGE ( 'NONE', *, *, #16548, .F. ) ;
#97473 = CARTESIAN_POINT ( 'NONE',  ( 34.84383463460000030, 1427.856177373630089, 265.6112251771979800 ) ) ;
#97474 = CARTESIAN_POINT ( 'NONE',  ( 18.65451742820949832, 1507.632629731499947, 188.5326158842280222 ) ) ;
#97475 = CARTESIAN_POINT ( 'NONE',  ( -105.2149124839869927, 1384.933864520869975, 311.2011526427629633 ) ) ;
#97476 = CARTESIAN_POINT ( 'NONE',  ( -7.167383222404231979, 1508.551704408387423, 214.6352815287315252 ) ) ;
#97477 = CIRCLE ( 'NONE', #49216, 0.9999999999999940048 ) ;
#97478 = FACE_OUTER_BOUND ( 'NONE', #3995, .T. ) ;
#97479 = CARTESIAN_POINT ( 'NONE',  ( 17.72826782676450108, 1408.955359599259964, 269.5568341151930554 ) ) ;
#97480 =( BOUNDED_SURFACE ( )  B_SPLINE_SURFACE ( 3, 2, ( 
 ( #91429, #4665, #107674 ),
 ( #55644, #38804, #99247 ),
 ( #72979, #22524, #6313 ),
 ( #74635, #108770, #64043 ),
 ( #14150, #13585, #49434 ),
 ( #15242, #107117, #40460 ) ),
 .UNSPECIFIED., .F., .F., .F. ) 
 B_SPLINE_SURFACE_WITH_KNOTS ( ( 4, 2, 4 ),
 ( 3, 3 ),
 ( -2.471980953266950110E-17, 0.001312027981647300671, 0.002624055963294626061 ),
 ( 0.000000000000000000, 1.000000000000000000 ),
 .UNSPECIFIED. ) 
 GEOMETRIC_REPRESENTATION_ITEM ( )  RATIONAL_B_SPLINE_SURFACE ( (
 ( 1.000000000000000000, 0.9376006582765911146, 1.000000000000000000),
 ( 1.000000000000000000, 0.9569320108021848181, 1.000000000000000000),
 ( 1.000000000000000000, 0.9725743441619884022, 1.000000000000000000),
 ( 1.000000000000000000, 0.9942095667134637216, 1.000000000000000000),
 ( 1.000000000000000000, 1.000043666450783464, 1.000000000000000000),
 ( 1.000000000000000000, 1.000000000000000000, 1.000000000000000000) ) ) 
 REPRESENTATION_ITEM ( '' )  SURFACE ( )  );
#97482 = ORIENTED_EDGE ( 'NONE', *, *, #33518, .T. ) ;
#97481 = CARTESIAN_POINT ( 'NONE',  ( -4.149769861736410270, 1430.580313301509932, 185.9069866752190023 ) ) ;
#97483 = CARTESIAN_POINT ( 'NONE',  ( 17.36801837519999836, 1414.983771848829747, 210.5058389745279896 ) ) ;
#97484 = CARTESIAN_POINT ( 'NONE',  ( -24.27053168829999663, 1443.236894957179857, 212.3234000011480020 ) ) ;
#97485 = CARTESIAN_POINT ( 'NONE',  ( -2.233110619234230487, 1449.897286081790298, 154.3831795966705442 ) ) ;
#97486 = CARTESIAN_POINT ( 'NONE',  ( 7.097349803439506388, 1439.093602098585052, 216.1529730758497010 ) ) ;
#97487 = CARTESIAN_POINT ( 'NONE',  ( 15.20279853403500070, 1514.921193539169963, 225.0317509809670184 ) ) ;
#97488 = CARTESIAN_POINT ( 'NONE',  ( -7.303957127409999472, 1440.776932085429962, 186.0900577853979883 ) ) ;
#97489 = AXIS2_PLACEMENT_3D ( 'NONE', #110379, #42630, #16292 ) ;
#97490 = CARTESIAN_POINT ( 'NONE',  ( 27.54845678703150114, 1509.914129475679829, 222.6825216195649944 ) ) ;
#97491 = CARTESIAN_POINT ( 'NONE',  ( 8.522139007390389764, 1459.194399288350041, 203.0278343432409827 ) ) ;
#97492 = CARTESIAN_POINT ( 'NONE',  ( -0.9756374909739999879, 1431.113060387329824, 228.8047907271979966 ) ) ;
#97493 = CARTESIAN_POINT ( 'NONE',  ( 7.383547498839999612, 1417.414537312230095, 231.0421684962979896 ) ) ;
#97494 = CARTESIAN_POINT ( 'NONE',  ( -5.430946523250000268, 1476.595381090889987, 218.1965627062390354 ) ) ;
#97495 = CARTESIAN_POINT ( 'NONE',  ( -21.98490254032901703, 1525.713797967457367, 235.3026395021805683 ) ) ;
#97496 = CARTESIAN_POINT ( 'NONE',  ( -0.01265822594359850006, 1516.959716008189844, 207.4120794380770292 ) ) ;
#97497 = CARTESIAN_POINT ( 'NONE',  ( 46.05260656040000100, 1438.905840350680137, 266.6770572228979859 ) ) ;
#97498 = CARTESIAN_POINT ( 'NONE',  ( -17.45090663859999935, 1409.522459475629830, 223.7636686640979917 ) ) ;
#97499 = CARTESIAN_POINT ( 'NONE',  ( 21.87661169429999575, 1435.403821294829868, 142.1301396295980055 ) ) ;
#97500 = CARTESIAN_POINT ( 'NONE',  ( 20.17949039979999881, 1469.158434794429922, 192.3038326788980044 ) ) ;
#97501 = CARTESIAN_POINT ( 'NONE',  ( -16.03382226631890006, 1409.472973801630133, 193.0383433025830016 ) ) ;
#97502 = CARTESIAN_POINT ( 'NONE',  ( -2.765183635730000145, 1475.775321107629907, 266.9581418145979796 ) ) ;
#97503 = CARTESIAN_POINT ( 'NONE',  ( -14.28499805876190010, 1416.808594522969770, 203.2225434410350147 ) ) ;
#97504 = CARTESIAN_POINT ( 'NONE',  ( -39.97226237699269547, 1438.646033188909996, 135.6295559456019930 ) ) ;
#97505 = CARTESIAN_POINT ( 'NONE',  ( 0.2178157486290130118, 1452.982786607829894, 183.2541296479709843 ) ) ;
#97506 = CARTESIAN_POINT ( 'NONE',  ( -13.29011429918680065, 1407.447342471949923, 210.5442722391819927 ) ) ;
#97507 = CARTESIAN_POINT ( 'NONE',  ( 8.546316978770940764, 1428.346933653820088, 213.3379775298699883 ) ) ;
#97508 = CARTESIAN_POINT ( 'NONE',  ( -3.984081752360000284, 1515.551704408389924, 207.2788837304390199 ) ) ;
#97509 = EDGE_CURVE ( 'NONE', #105027, #25245, #31730, .T. ) ;
#97510 = CYLINDRICAL_SURFACE ( 'NONE', #30045, 33.13701971169416538 ) ;
#97511 = CARTESIAN_POINT ( 'NONE',  ( 4.345191827429070841, 1455.903930675749962, 218.8175630227480042 ) ) ;
#97512 = CARTESIAN_POINT ( 'NONE',  ( -35.72409870509849839, 1435.953719464810092, 134.0999999973689967 ) ) ;
#97513 = DIRECTION ( 'NONE',  ( -0.9625294240555893888, 6.236250047180620319E-07, -0.2711772627393869706 ) ) ;
#97514 = ORIENTED_EDGE ( 'NONE', *, *, #23751, .F. ) ;
#97515 = CARTESIAN_POINT ( 'NONE',  ( 6.054581389202323471, 1510.727597956443788, 216.6161816537009486 ) ) ;
#97516 = CARTESIAN_POINT ( 'NONE',  ( -3.210101824899569856, 1409.025159613220012, 223.7627473412850065 ) ) ;
#97517 = CARTESIAN_POINT ( 'NONE',  ( -11.15120484727999894, 1517.051704408389924, 198.0995572319588405 ) ) ;
#97518 = CARTESIAN_POINT ( 'NONE',  ( -2.477970950320000032, 1440.426958604040010, 157.8055609083980073 ) ) ;
#97519 = CARTESIAN_POINT ( 'NONE',  ( -16.90742456144603523, 1442.831169986190389, 162.4348202098863396 ) ) ;
#97520 = CARTESIAN_POINT ( 'NONE',  ( -31.74876339820000126, 1466.573431914830053, 268.0541753359980248 ) ) ;
#97521 = CARTESIAN_POINT ( 'NONE',  ( -13.30777107328369979, 1428.971706346040037, 222.3032313369639894 ) ) ;
#97522 = CARTESIAN_POINT ( 'NONE',  ( -17.30126322281348195, 1523.382868172863937, 237.3930845920475292 ) ) ;
#97523 = DIRECTION ( 'NONE',  ( -1.755985294532469921E-16, 1.000000000000000000, -1.338183447452831989E-16 ) ) ;
#97524 = CARTESIAN_POINT ( 'NONE',  ( 7.983219802273961996, 1511.369014876796655, 203.7222547165445690 ) ) ;
#97525 = CARTESIAN_POINT ( 'NONE',  ( -33.29420051208550291, 1384.975192605860002, 207.5272639334069993 ) ) ;
#97526 = CARTESIAN_POINT ( 'NONE',  ( -12.21562307281700122, 1490.700173189130055, 208.0633276266580083 ) ) ;
#97527 = CARTESIAN_POINT ( 'NONE',  ( 12.58432885909999932, 1415.426210663629945, 221.2617231595980059 ) ) ;
#97528 = CARTESIAN_POINT ( 'NONE',  ( -6.484578373979999810, 1434.540925522399903, 154.7070604761979951 ) ) ;
#97529 = CARTESIAN_POINT ( 'NONE',  ( 1.389373685229310817, 1526.382868172571079, 178.7050053866609858 ) ) ;
#97531 = ORIENTED_EDGE ( 'NONE', *, *, #57636, .T. ) ;
#97530 = DIRECTION ( 'NONE',  ( 0.7071067811865492381, 0.000000000000000000, -0.7071067811865457964 ) ) ;
#97532 = CARTESIAN_POINT ( 'NONE',  ( -4.026786250540000722, 1408.413060387330006, 146.1721969590979882 ) ) ;
#97534 = CARTESIAN_POINT ( 'NONE',  ( -23.49263094430000010, 1409.898020881729963, 208.4774537725740231 ) ) ;
#97533 = CIRCLE ( 'NONE', #54642, 17.27637083661241135 ) ;
#97535 = CARTESIAN_POINT ( 'NONE',  ( 26.56924837500000081, 1488.569808382929978, 207.4007344032380047 ) ) ;
#97536 = CARTESIAN_POINT ( 'NONE',  ( 2.688586027246119947, 1509.006950727750109, 238.2845013960090057 ) ) ;
#97537 = DIRECTION ( 'NONE',  ( -0.8771707348056354547, 0.03063147701716761526, 0.4792005995575221999 ) ) ;
#97538 = EDGE_CURVE ( 'NONE', #11508, #16786, #27762, .T. ) ;
#97539 = CARTESIAN_POINT ( 'NONE',  ( 23.64283040619999809, 1411.099127945830105, 211.3905525550979974 ) ) ;
#97540 = B_SPLINE_SURFACE_WITH_KNOTS ( 'NONE', 5, 5, ( 
 ( #16231, #52084, #59941, #42563, #33589, #67783 ),
 ( #101894, #25187, #28, #34161, #68347, #102453 ),
 ( #94058, #25740, #582, #17326, #51520, #68900 ),
 ( #103002, #24995, #67595, #108478, #101702, #92769 ),
 ( #39625, #24448, #6015, #100611, #14397, #75975 ),
 ( #110127, #40719, #32855, #48591, #65397, #31761 ),
 ( #23895, #91121, #49691, #92222, #41819, #7120 ),
 ( #93316, #16045, #73793, #100072, #33400, #56990 ),
 ( #5464, #107920, #59198, #82725, #58089, #50246 ) ),
 .UNSPECIFIED., .F., .F., .F.,
 ( 6, 3, 6 ),
 ( 6, 6 ),
 ( 3.064599166390000295, 5.269658684210000388, 7.474718202020000035 ),
 ( 0.000000000000000000, 2.000000000000000000 ),
 .UNSPECIFIED. ) ;
#97541 = CARTESIAN_POINT ( 'NONE',  ( -2.777747345173310123, 1456.209076296149988, 202.9659044564290014 ) ) ;
#97542 = CARTESIAN_POINT ( 'NONE',  ( -18.75153682899999907, 1469.211784502090040, 201.1821593617290205 ) ) ;
#97543 = CARTESIAN_POINT ( 'NONE',  ( -5.360046087876660259, 1422.261995185559954, 145.0057915772580088 ) ) ;
#97545 = CARTESIAN_POINT ( 'NONE',  ( -11.58399188110000111, 1381.166830487859897, 202.6872540392290318 ) ) ;
#97544 = CARTESIAN_POINT ( 'NONE',  ( -0.1681681984989999989, 1420.473120458229914, 172.2701767054979882 ) ) ;
#97546 = CARTESIAN_POINT ( 'NONE',  ( -9.129808743239919977, 1383.863787745319996, 218.5279288296370055 ) ) ;
#97547 = LINE ( 'NONE', #62898, #69904 ) ;
#97548 = EDGE_CURVE ( 'NONE', #28577, #65542, #91802, .T. ) ;
#97549 = DIRECTION ( 'NONE',  ( 0.000000000000000000, -1.000000000000000000, 0.000000000000000000 ) ) ;
#97550 = CARTESIAN_POINT ( 'NONE',  ( -1.101868389151629879, 1419.744089616479869, 184.9570230273619984 ) ) ;
#97551 = ADVANCED_FACE ( 'NONE', ( #50013 ), #8460, .T. ) ;
#97552 = CARTESIAN_POINT ( 'NONE',  ( -1.132949114555000136, 1516.693851263360102, 204.1241276937270186 ) ) ;
#97553 = DIRECTION ( 'NONE',  ( 0.000000000000000000, 0.000000000000000000, 1.000000000000000000 ) ) ;
#97554 = CARTESIAN_POINT ( 'NONE',  ( -18.75257229663529657, 1485.356831147769981, 189.3986093459970164 ) ) ;
#97555 = CARTESIAN_POINT ( 'NONE',  ( -8.952944454599998991, 1424.162919053179849, 206.7489373822789673 ) ) ;
#97556 = CARTESIAN_POINT ( 'NONE',  ( -4.278522756227959967, 1441.024006130319776, 156.7060794043559895 ) ) ;
#97558 = EDGE_LOOP ( 'NONE', ( #88320, #72187, #20742 ) ) ;
#97557 = CARTESIAN_POINT ( 'NONE',  ( -68.19307365539999921, 1379.747659725539961, 279.6816280294590342 ) ) ;
#97559 = EDGE_CURVE ( 'NONE', #77737, #2271, #1010, .T. ) ;
#97560 = ORIENTED_EDGE ( 'NONE', *, *, #82010, .T. ) ;
#97561 = CARTESIAN_POINT ( 'NONE',  ( 29.21606581500000033, 1509.871156554629806, 209.9693792701380062 ) ) ;
#97562 = ORIENTED_EDGE ( 'NONE', *, *, #55698, .F. ) ;
#97563 = CYLINDRICAL_SURFACE ( 'NONE', #860, 2.000000000000003553 ) ;
#97564 = VECTOR ( 'NONE', #100642, 1000.000000000000000 ) ;
#97565 = CARTESIAN_POINT ( 'NONE',  ( -109.6576905139999951, 1384.926051320400120, 311.3230246392589606 ) ) ;
#97567 = CARTESIAN_POINT ( 'NONE',  ( 0.8050666512040000056, 1507.647395255030006, 180.9817899904979868 ) ) ;
#97566 = CARTESIAN_POINT ( 'NONE',  ( -15.71040652243883784, 1410.149699372532723, 226.5306214444462398 ) ) ;
#97568 = CARTESIAN_POINT ( 'NONE',  ( 11.88064286090000010, 1433.444786854229960, 151.0525681022980109 ) ) ;
#97569 = CARTESIAN_POINT ( 'NONE',  ( -24.56616253283889861, 1451.897895543200093, 137.1355346205309900 ) ) ;
#97570 = CARTESIAN_POINT ( 'NONE',  ( -0.8848931312460019960, 1467.694904068390088, 220.2161335405990314 ) ) ;
#97571 = CARTESIAN_POINT ( 'NONE',  ( 4.379432440569999585, 1409.571163557129921, 231.2061471731980191 ) ) ;
#97572 = CARTESIAN_POINT ( 'NONE',  ( 10.47412083013409934, 1481.229225394920149, 212.5602164828920024 ) ) ;
#97573 = CARTESIAN_POINT ( 'NONE',  ( 2.298369469825000344, 1516.779243033999819, 212.3734572960470075 ) ) ;
#97575 = AXIS2_PLACEMENT_3D ( 'NONE', #51295, #25524, #110101 ) ;
#97574 = CARTESIAN_POINT ( 'NONE',  ( 40.01221335447130656, 1438.828034964499921, 134.0999999981109738 ) ) ;
#97576 = CARTESIAN_POINT ( 'NONE',  ( -20.02799630220000182, 1485.574563381989947, 204.1280247810589970 ) ) ;
#97577 = EDGE_LOOP ( 'NONE', ( #94137, #49445, #103322, #101558, #6405 ) ) ;
#97578 = CARTESIAN_POINT ( 'NONE',  ( 7.755379691499999062, 1459.738853293389866, 228.9106028235989925 ) ) ;
#97579 = CARTESIAN_POINT ( 'NONE',  ( 7.560886196111736623, 1492.428349930449258, 217.3049961171652740 ) ) ;
#97580 = VERTEX_POINT ( 'NONE', #94196 ) ;
#97581 = VERTEX_POINT ( 'NONE', #41609 ) ;
#97582 = ORIENTED_EDGE ( 'NONE', *, *, #27798, .F. ) ;
#97583 = CARTESIAN_POINT ( 'NONE',  ( -6.242053784335000799, 1513.743447518359972, 216.6918286318270077 ) ) ;
#97584 = CARTESIAN_POINT ( 'NONE',  ( 16.23489788457936811, 1514.585431650382588, 194.3036092076362991 ) ) ;
#97585 = CARTESIAN_POINT ( 'NONE',  ( 21.11358352923581094, 1450.944576484996105, 144.3255025187013985 ) ) ;
#97586 = CARTESIAN_POINT ( 'NONE',  ( -7.769235937790000435, 1384.905328562600062, 218.9178834932589837 ) ) ;
#97587 = CARTESIAN_POINT ( 'NONE',  ( 10.78159632189999861, 1461.896570031590045, 211.1674760275290055 ) ) ;
#97588 = EDGE_CURVE ( 'NONE', #57276, #106344, #76417, .T. ) ;
#97589 = CARTESIAN_POINT ( 'NONE',  ( -18.52965084578502086, 1445.637233098631214, 214.4783539933714849 ) ) ;
#97590 = CARTESIAN_POINT ( 'NONE',  ( -66.35921308805916397, 1379.742723719715968, 275.1101220287822002 ) ) ;
#97591 = DIRECTION ( 'NONE',  ( -0.04170409655914577435, 0.9849797009429184236, 0.1675582199135109140 ) ) ;
#97592 = CARTESIAN_POINT ( 'NONE',  ( -0.5988589654079999880, 1507.637957935130089, 231.7691613850980161 ) ) ;
#97593 = EDGE_CURVE ( 'NONE', #30075, #91018, #71845, .T. ) ;
#97594 = CARTESIAN_POINT ( 'NONE',  ( 7.951680115159998508, 1415.087745006229852, 194.0123767119980016 ) ) ;
#97595 = CARTESIAN_POINT ( 'NONE',  ( -49.72680530535440369, 1384.618443061529888, 224.8565442374369923 ) ) ;
#97596 = ORIENTED_EDGE ( 'NONE', *, *, #49480, .T. ) ;
#97597 = CARTESIAN_POINT ( 'NONE',  ( -3.269984819434999856, 1516.999105586269934, 207.4194399470370058 ) ) ;
#97598 = ORIENTED_EDGE ( 'NONE', *, *, #66866, .F. ) ;
#97599 = CARTESIAN_POINT ( 'NONE',  ( 28.01520159380029895, 1440.913060387330006, 247.6253163881469845 ) ) ;
#97600 = B_SPLINE_CURVE_WITH_KNOTS ( 'NONE', 3,
 ( #4367, #37963, #37409, #28456, #62650, #20042, #72144, #106262, #54237, #88363, #45829, #29548, #63734, #46934, #81052, #38496, #64282, #72673, #106798 ),
 .UNSPECIFIED., .F., .F.,
 ( 4, 3, 3, 3, 3, 3, 4 ),
 ( -7.611835603415659790, -7.445832134393750579, -6.293638100938689917, -5.367142758962240023, -4.666606357331840371, -3.867104339607819963, -3.122448789919999967 ),
 .UNSPECIFIED. ) ;
#97601 = CARTESIAN_POINT ( 'NONE',  ( 11.43893751517350132, 1478.788528365839966, 206.4651667696550135 ) ) ;
#97602 = ORIENTED_EDGE ( 'NONE', *, *, #14869, .T. ) ;
#97603 = CARTESIAN_POINT ( 'NONE',  ( -17.73223409949403617, 1524.152444737676660, 180.4731695944016678 ) ) ;
#97604 = CARTESIAN_POINT ( 'NONE',  ( -13.16630813000000089, 1409.372837998530031, 190.8918809504980061 ) ) ;
#97605 = CARTESIAN_POINT ( 'NONE',  ( -23.64337456402409998, 1435.765682558080016, 212.0350035351450231 ) ) ;
#97607 = CARTESIAN_POINT ( 'NONE',  ( -1.547462741870939906, 1414.913060391199906, 225.9340804956229931 ) ) ;
#97606 = CARTESIAN_POINT ( 'NONE',  ( -24.39197164660000183, 1441.205372402069997, 211.3456893288379774 ) ) ;
#97608 = CARTESIAN_POINT ( 'NONE',  ( -8.140676920415208073, 1436.358399980439799, 214.5433328127169830 ) ) ;
#97609 = CARTESIAN_POINT ( 'NONE',  ( -5.705922872222989994, 1511.346048414110101, 201.2009718814310020 ) ) ;
#97610 = CARTESIAN_POINT ( 'NONE',  ( 12.67137506719999962, 1407.308516313030168, 266.8981195266979967 ) ) ;
#97611 = FACE_OUTER_BOUND ( 'NONE', #109463, .T. ) ;
#97612 = CARTESIAN_POINT ( 'NONE',  ( -4.632636518429999128, 1507.809020188690056, 221.0048302704990135 ) ) ;
#97614 = CARTESIAN_POINT ( 'NONE',  ( 1.914156610164409855, 1431.087920293139859, 199.8421651263110164 ) ) ;
#97613 = CARTESIAN_POINT ( 'NONE',  ( 2.797472701710000287, 1464.949655032329929, 234.8291015129980224 ) ) ;
#97615 = CARTESIAN_POINT ( 'NONE',  ( 6.943602653455000606, 1516.858069504249897, 216.0629462479770098 ) ) ;
#97616 = CARTESIAN_POINT ( 'NONE',  ( 22.03465957474570658, 1522.382868172863937, 235.4136513321629991 ) ) ;
#97617 = CARTESIAN_POINT ( 'NONE',  ( 0.4346943641293429805, 1517.051704428850144, 201.3992661435559910 ) ) ;
#97618 = AXIS2_PLACEMENT_3D ( 'NONE', #49126, #82711, #6000 ) ;
#97619 = CARTESIAN_POINT ( 'NONE',  ( 14.13195592840999915, 1452.421092199690065, 222.7290593210850034 ) ) ;
#97620 = CARTESIAN_POINT ( 'NONE',  ( 6.949574947644999945, 1517.102359858469754, 212.3809477691169718 ) ) ;
#97621 = VECTOR ( 'NONE', #63446, 1000.000000000000000 ) ;
#97622 = CARTESIAN_POINT ( 'NONE',  ( -18.24515611230000189, 1416.817366564930126, 208.9598336527209881 ) ) ;
#97623 = CARTESIAN_POINT ( 'NONE',  ( -33.91369120143989591, 1451.728768194249824, 134.0999999980979851 ) ) ;
#97625 = ORIENTED_EDGE ( 'NONE', *, *, #101435, .F. ) ;
#97624 = CARTESIAN_POINT ( 'NONE',  ( -24.20882859423510070, 1435.739118765830199, 210.8967395777180229 ) ) ;
#97626 = CARTESIAN_POINT ( 'NONE',  ( -17.62880125161998990, 1524.547395018738143, 237.6137924969227413 ) ) ;
#97627 = CARTESIAN_POINT ( 'NONE',  ( 12.80873346849999983, 1461.536424719429988, 232.0427772018979908 ) ) ;
#97628 = CARTESIAN_POINT ( 'NONE',  ( -16.17568633703940151, 1459.146939663510011, 230.7169128052520080 ) ) ;
#97629 = CARTESIAN_POINT ( 'NONE',  ( -15.62922400629999942, 1415.754093022550023, 208.9578334822819841 ) ) ;
#97630 = CARTESIAN_POINT ( 'NONE',  ( -1.418980099639949977, 1507.123641610349978, 237.1495972631439884 ) ) ;
#97631 = CARTESIAN_POINT ( 'NONE',  ( 16.64885258016843039, 1526.344110814223086, 183.3327398900455592 ) ) ;
#97633 = CARTESIAN_POINT ( 'NONE',  ( 5.360183379389989788, 1422.857591872020066, 148.0592648305490115 ) ) ;
#97632 = CARTESIAN_POINT ( 'NONE',  ( -19.86788408629999836, 1444.803041715769950, 224.4210983673980024 ) ) ;
#97634 = CARTESIAN_POINT ( 'NONE',  ( 6.602631447940000342, 1463.509733493989870, 209.4768623231300069 ) ) ;
#97635 = CARTESIAN_POINT ( 'NONE',  ( -106.6524542679999854, 1380.137974075159946, 308.5605864792590296 ) ) ;
#97636 = ORIENTED_EDGE ( 'NONE', *, *, #56955, .F. ) ;
#97637 = CARTESIAN_POINT ( 'NONE',  ( -3.459156616214999591, 1516.769879638719885, 204.5118493505569859 ) ) ;
#97638 = CARTESIAN_POINT ( 'NONE',  ( 1.769677292390000156, 1406.090449095429904, 269.0444970099979969 ) ) ;
#97639 = CARTESIAN_POINT ( 'NONE',  ( -0.7576697578790009269, 1515.544658147190148, 213.2443391230790155 ) ) ;
#97640 = AXIS2_PLACEMENT_3D ( 'NONE', #39974, #66312, #14209 ) ;
#97641 = CARTESIAN_POINT ( 'NONE',  ( 31.82247306223929328, 1465.839566737470250, 269.9247011470700386 ) ) ;
#97642 = LINE ( 'NONE', #98733, #96002 ) ;
#97643 = CARTESIAN_POINT ( 'NONE',  ( 19.45791513090297542, 1498.411990192014628, 218.7312280957626456 ) ) ;
#97644 = DIRECTION ( 'NONE',  ( -0.6736849260863841948, 0.000000000000000000, 0.7390186874254148774 ) ) ;
#97645 = B_SPLINE_CURVE_WITH_KNOTS ( 'NONE', 5,
 ( #72542, #44583, #106673, #29963, #64155, #18794 ),
 .UNSPECIFIED., .F., .F.,
 ( 6, 6 ),
 ( -2.000000000000000000, 0.000000000000000000 ),
 .UNSPECIFIED. ) ;
#97646 = CARTESIAN_POINT ( 'NONE',  ( 7.137524478430058217, 1442.009334510292774, 183.6365729105961861 ) ) ;
#97647 = CARTESIAN_POINT ( 'NONE',  ( 10.62756433831671288, 1462.208184687777020, 211.9187829460415742 ) ) ;
#97648 = CARTESIAN_POINT ( 'NONE',  ( -105.6997850770000014, 1391.688872221259999, 304.2060384943581539 ) ) ;
#97649 = DIRECTION ( 'NONE',  ( -0.9786619618251627406, 0.000000000000000000, -0.2054769195713317953 ) ) ;
#97650 = ORIENTED_EDGE ( 'NONE', *, *, #32569, .F. ) ;
#97651 = CARTESIAN_POINT ( 'NONE',  ( -10.04572263220000039, 1417.623152644130187, 255.3819207682979595 ) ) ;
#97652 = B_SPLINE_CURVE_WITH_KNOTS ( 'NONE', 3,
 ( #86181, #77789, #102961, #25699, #1098, #35226 ),
 .UNSPECIFIED., .F., .F.,
 ( 4, 2, 4 ),
 ( 2.850771429603742560E-17, 0.001087661325621715322, 0.002175322651243402454 ),
 .UNSPECIFIED. ) ;
#97653 = CARTESIAN_POINT ( 'NONE',  ( 6.582297905418769801, 1467.177907444709945, 200.9815396461360137 ) ) ;
#97654 = CARTESIAN_POINT ( 'NONE',  ( -0.1075775631909999946, 1475.837061347730014, 266.9611530679979978 ) ) ;
#97655 = CARTESIAN_POINT ( 'NONE',  ( 0.0001132552782701080050, 1397.914756428169994, 209.1116890797569852 ) ) ;
#97656 = CARTESIAN_POINT ( 'NONE',  ( -12.01221612688690676, 1513.042033678214011, 192.5302509902024610 ) ) ;
#97657 = CARTESIAN_POINT ( 'NONE',  ( -4.074356902468740493, 1448.298665946849042, 185.0948666590034009 ) ) ;
#97658 = CARTESIAN_POINT ( 'NONE',  ( -30.50452582731020001, 1384.826580460149898, 228.5933960381599945 ) ) ;
#97659 = CARTESIAN_POINT ( 'NONE',  ( -105.0581544420000029, 1379.236406965169863, 304.0328518213589746 ) ) ;
#97660 = DIRECTION ( 'NONE',  ( 1.000000000000000000, -0.000000000000000000, 1.224646799147353207E-16 ) ) ;
#97661 = CARTESIAN_POINT ( 'NONE',  ( 26.79414221416690012, 1436.761946617690000, 136.7822070004859825 ) ) ;
#97662 = CARTESIAN_POINT ( 'NONE',  ( -9.355712483234770005, 1396.239769066399958, 215.0244685633099948 ) ) ;
#97663 = CARTESIAN_POINT ( 'NONE',  ( -14.79868613460000049, 1421.900788730430122, 227.7466242548979949 ) ) ;
#97664 = CARTESIAN_POINT ( 'NONE',  ( 19.58542614618488997, 1455.481092546511491, 225.8721902375976640 ) ) ;
#97665 = EDGE_CURVE ( 'NONE', #106581, #10690, #33736, .T. ) ;
#97666 = ORIENTED_EDGE ( 'NONE', *, *, #88999, .T. ) ;
#97667 = CARTESIAN_POINT ( 'NONE',  ( -11.39741020242381175, 1501.140956553491606, 208.2051223886542459 ) ) ;
#97668 = CARTESIAN_POINT ( 'NONE',  ( -15.59833272758146094, 1415.960467561331143, 208.0431140678893485 ) ) ;
#97669 = CARTESIAN_POINT ( 'NONE',  ( -3.321447364419999548, 1484.261043626330093, 183.3707343507980170 ) ) ;
#97671 = CARTESIAN_POINT ( 'NONE',  ( -13.56546627376500069, 1512.571022561229938, 193.5522729196669900 ) ) ;
#97670 = CARTESIAN_POINT ( 'NONE',  ( 11.30750857299999979, 1426.033734466129999, 121.0015455956980048 ) ) ;
#97672 = CARTESIAN_POINT ( 'NONE',  ( -5.376254996749998888E-14, 1377.913060387289988, 209.1218459616989946 ) ) ;
#97673 = CARTESIAN_POINT ( 'NONE',  ( 4.363119589138680254, 1423.854801764450031, 183.5697712894070150 ) ) ;
#97674 = CARTESIAN_POINT ( 'NONE',  ( -4.646147325060000277, 1378.399971913189802, 203.6922293430689876 ) ) ;
#97675 = CARTESIAN_POINT ( 'NONE',  ( 8.045781271640001009, 1426.290936267859934, 211.5934327219790134 ) ) ;
#97676 = CARTESIAN_POINT ( 'NONE',  ( 10.59813991459999905, 1477.524080022390081, 229.9254213492990004 ) ) ;
#97677 = CARTESIAN_POINT ( 'NONE',  ( 3.300397815039999738, 1508.450664834530016, 180.9822841743979893 ) ) ;
#97678 = CARTESIAN_POINT ( 'NONE',  ( 0.1620860067197200105, 1416.842625005220043, 190.8755133330550109 ) ) ;
#97679 = CARTESIAN_POINT ( 'NONE',  ( -42.14410030795320239, 1378.731951168329942, 233.4973399294630099 ) ) ;
#97680 = CARTESIAN_POINT ( 'NONE',  ( 8.177749334224245104, 1366.009032010753117, 210.6218459617142003 ) ) ;
#97682 = ORIENTED_EDGE ( 'NONE', *, *, #41452, .T. ) ;
#97681 = CARTESIAN_POINT ( 'NONE',  ( -16.62685139801940082, 1379.596349548939997, 212.3140244300689972 ) ) ;
#97683 = ORIENTED_EDGE ( 'NONE', *, *, #69410, .T. ) ;
#97684 = ADVANCED_FACE ( 'NONE', ( #7446 ), #90407, .T. ) ;
#97685 = CARTESIAN_POINT ( 'NONE',  ( -10.46857477760000066, 1397.317675341630093, 201.0163134539180305 ) ) ;
#97686 = CARTESIAN_POINT ( 'NONE',  ( 0.8413093506324749171, 1490.956749009019859, 236.5476227179300110 ) ) ;
#97687 = CARTESIAN_POINT ( 'NONE',  ( 1.910127611640000132E-10, 1497.713060387329961, 230.7369720342980202 ) ) ;
#97688 = CARTESIAN_POINT ( 'NONE',  ( -7.622960524865000309, 1511.191277613550028, 212.5075598512569854 ) ) ;
#97690 = CARTESIAN_POINT ( 'NONE',  ( 12.98226713004290112, 1414.913060387349788, 198.3280232619060257 ) ) ;
#97689 = CARTESIAN_POINT ( 'NONE',  ( -8.576277482710001010, 1384.765141178520025, 218.6682590137189948 ) ) ;
#97691 = CARTESIAN_POINT ( 'NONE',  ( 12.95120320960000093, 1410.293446051630099, 190.4598861209980214 ) ) ;
#97692 = CARTESIAN_POINT ( 'NONE',  ( 8.454790733525280544, 1428.363638633589972, 213.4109935021670026 ) ) ;
#97693 = ADVANCED_FACE ( 'NONE', ( #1268 ), #39237, .F. ) ;
#97694 = FACE_OUTER_BOUND ( 'NONE', #81309, .T. ) ;
#97695 = SURFACE_SIDE_STYLE ('',( #89296 ) ) ;
#97696 = CARTESIAN_POINT ( 'NONE',  ( 36.08237879343099763, 1436.861740189970078, 136.4673732261519774 ) ) ;
#97697 = CARTESIAN_POINT ( 'NONE',  ( 5.571677614479849439, 1396.107627656979957, 218.6505891727530013 ) ) ;
#97698 = CARTESIAN_POINT ( 'NONE',  ( -40.23588547079999245, 1442.699308055779966, 137.0099670915980141 ) ) ;
#97699 = CARTESIAN_POINT ( 'NONE',  ( -2.294228461334139713, 1406.102006316850066, 269.0439725548540082 ) ) ;
#97700 = LINE ( 'NONE', #19877, #103701 ) ;
#97701 = VERTEX_POINT ( 'NONE', #104269 ) ;
#97702 = CARTESIAN_POINT ( 'NONE',  ( 3.697227707439999733, 1424.334605312130179, 184.5849975447979716 ) ) ;
#97703 = CARTESIAN_POINT ( 'NONE',  ( 12.95770839519999917, 1442.886199328829889, 187.4929395404980141 ) ) ;
#97704 = ORIENTED_EDGE ( 'NONE', *, *, #86035, .F. ) ;
#97705 = ORIENTED_EDGE ( 'NONE', *, *, #66682, .T. ) ;
#97706 = CARTESIAN_POINT ( 'NONE',  ( -4.987793514269999839, 1425.174461588439954, 209.2447519049540006 ) ) ;
#97707 = CARTESIAN_POINT ( 'NONE',  ( 9.369782510130001185, 1366.497526915280105, 207.6218459616989946 ) ) ;
#97708 = CARTESIAN_POINT ( 'NONE',  ( 7.720650135305000994, 1516.977993847330026, 214.9014730243169993 ) ) ;
#97709 = CARTESIAN_POINT ( 'NONE',  ( -12.31045031087770170, 1378.376187938819839, 209.7947225889870140 ) ) ;
#97710 = AXIS2_PLACEMENT_3D ( 'NONE', #38400, #46836, #11008 ) ;
#97711 = EDGE_LOOP ( 'NONE', ( #51966, #61398, #78866, #89596, #1797 ) ) ;
#97712 = CARTESIAN_POINT ( 'NONE',  ( -2.957532206020210275, 1509.097982660189700, 179.2610898709129970 ) ) ;
#97713 = CARTESIAN_POINT ( 'NONE',  ( -71.10329879200000391, 1377.246858117049896, 279.1099741719589815 ) ) ;
#97714 = AXIS2_PLACEMENT_3D ( 'NONE', #89529, #81122, #32386 ) ;
#97715 = EDGE_CURVE ( 'NONE', #28182, #46489, #99938, .T. ) ;
#97716 = CARTESIAN_POINT ( 'NONE',  ( 0.3551208790259999803, 1416.218047894730262, 227.0926726479979720 ) ) ;
#97717 = CARTESIAN_POINT ( 'NONE',  ( -6.560742263465000335, 1517.028034847769959, 205.0881926677770082 ) ) ;
#97718 = CARTESIAN_POINT ( 'NONE',  ( -11.93029924615809989, 1489.674051635599881, 211.7541755384660007 ) ) ;
#97719 = CARTESIAN_POINT ( 'NONE',  ( -89.15684587290000707, 1384.835666735910081, 292.2581851215589950 ) ) ;
#97720 = AXIS2_PLACEMENT_3D ( 'NONE', #70767, #84342, #70219 ) ;
#97721 = CARTESIAN_POINT ( 'NONE',  ( -3.160109254029999537, 1409.527913850729874, 232.2647705438980097 ) ) ;
#97723 = ORIENTED_EDGE ( 'NONE', *, *, #83746, .F. ) ;
#97722 = CARTESIAN_POINT ( 'NONE',  ( -3.820292970859999772E-10, 1475.513060387329915, 188.4759928218979894 ) ) ;
#97724 = CARTESIAN_POINT ( 'NONE',  ( 2.370970874524633398, 1427.002265528473799, 137.0999999980980135 ) ) ;
#97725 = CARTESIAN_POINT ( 'NONE',  ( -26.88384131406899868, 1440.913060425529920, 226.2932696055459871 ) ) ;
#97726 = CARTESIAN_POINT ( 'NONE',  ( -1.332267629549999902E-15, 1384.913060387289988, 218.6218459572590120 ) ) ;
#97727 = FACE_OUTER_BOUND ( 'NONE', #23776, .T. ) ;
#97728 = CARTESIAN_POINT ( 'NONE',  ( 24.70944185802769866, 1416.032703119559756, 269.4189052401779918 ) ) ;
#97729 = CARTESIAN_POINT ( 'NONE',  ( -1.702754409475000008, 1517.014196759610059, 212.5856132281170119 ) ) ;
#97730 = CARTESIAN_POINT ( 'NONE',  ( -67.27445496530000923, 1379.746684743910009, 277.1113995282589713 ) ) ;
#97731 = B_SPLINE_CURVE_WITH_KNOTS ( 'NONE', 3,
 ( #109833, #110375, #41532, #85169, #51034, #40414, #74591, #94118 ),
 .UNSPECIFIED., .F., .F.,
 ( 4, 2, 2, 4 ),
 ( 0.0001376096082931063593, 0.003339882934058656990, 0.004941019596941432536, 0.006542156259824205913 ),
 .UNSPECIFIED. ) ;
#97732 = CARTESIAN_POINT ( 'NONE',  ( 23.62663202120000250, 1410.709074283629889, 207.9332156920780221 ) ) ;
#97733 = CARTESIAN_POINT ( 'NONE',  ( 0.01963003285704640472, 1507.326971762890707, 237.3724487458281658 ) ) ;
#97734 = CARTESIAN_POINT ( 'NONE',  ( 15.21359001291670054, 1427.479649557399853, 199.3000641055990059 ) ) ;
#97735 = CARTESIAN_POINT ( 'NONE',  ( -7.708878413334149471, 1516.528448466100144, 211.3872135947860045 ) ) ;
#97736 = CARTESIAN_POINT ( 'NONE',  ( -3.255809902135000211, 1516.837969789639828, 209.8792719553279937 ) ) ;
#97737 = ORIENTED_EDGE ( 'NONE', *, *, #28818, .T. ) ;
#97738 = CARTESIAN_POINT ( 'NONE',  ( 4.224193449673190770, 1421.807428560099879, 184.4466668902289825 ) ) ;
#97739 = CARTESIAN_POINT ( 'NONE',  ( -0.4394933405940000259, 1417.920058205030045, 233.5085631684980001 ) ) ;
#97740 = CARTESIAN_POINT ( 'NONE',  ( -81.18324780579999356, 1384.635789063720040, 304.9525423562590163 ) ) ;
#97741 = ORIENTED_EDGE ( 'NONE', *, *, #67238, .T. ) ;
#97742 = CARTESIAN_POINT ( 'NONE',  ( -29.66846558571840120, 1385.235115920719863, 227.6884932317539949 ) ) ;
#97743 = DIRECTION ( 'NONE',  ( -1.755985294532469921E-16, 1.000000000000000000, -1.338183447452831989E-16 ) ) ;
#97744 = CARTESIAN_POINT ( 'NONE',  ( 19.86721287640000000, 1507.838653413830116, 189.0155849983980261 ) ) ;
#97745 = DIRECTION ( 'NONE',  ( -0.8775825618903754233, 0.000000000000000000, -0.4794255386041978984 ) ) ;
#97746 = CARTESIAN_POINT ( 'NONE',  ( 11.13557732129999955, 1425.386704443429835, 204.8117771081390117 ) ) ;
#97747 = CARTESIAN_POINT ( 'NONE',  ( 3.043251597425320032, 1417.779699503100119, 234.3208248802520188 ) ) ;
#97749 = CARTESIAN_POINT ( 'NONE',  ( -16.45607496635827616, 1416.877115859795595, 207.9322112222681938 ) ) ;
#97748 = CARTESIAN_POINT ( 'NONE',  ( -6.941100315875000426, 1516.858069504249897, 216.0654486236869900 ) ) ;
#97750 = CARTESIAN_POINT ( 'NONE',  ( 19.08918182269999875, 1507.695925188030060, 188.5883432463980114 ) ) ;
#97751 = CARTESIAN_POINT ( 'NONE',  ( 10.17376127383159989, 1469.762723852360068, 208.1640156044039998 ) ) ;
#97752 = ORIENTED_EDGE ( 'NONE', *, *, #97548, .T. ) ;
#97753 = CARTESIAN_POINT ( 'NONE',  ( -6.554764199395000546, 1516.786099423779888, 201.4062207291269999 ) ) ;
#97754 = CARTESIAN_POINT ( 'NONE',  ( -13.58268883541719951, 1416.851343898680170, 221.9096085506480165 ) ) ;
#97755 = VERTEX_POINT ( 'NONE', #80724 ) ;
#97756 = CARTESIAN_POINT ( 'NONE',  ( 13.63295136444099853, 1492.115748128389896, 192.2627295947740151 ) ) ;
#97757 = AXIS2_PLACEMENT_3D ( 'NONE', #101069, #43405, #9247 ) ;
#97758 = CARTESIAN_POINT ( 'NONE',  ( 10.55905614399324577, 1434.900330220869137, 152.0984994257607923 ) ) ;
#97759 = CARTESIAN_POINT ( 'NONE',  ( 8.059493427214674099, 1423.943097687976206, 195.8566467428261433 ) ) ;
#97760 = CARTESIAN_POINT ( 'NONE',  ( 2.178538215579999715, 1442.258130819589951, 218.0918924510989996 ) ) ;
#97761 = CARTESIAN_POINT ( 'NONE',  ( 16.57223646264887051, 1421.748021482796958, 227.0899952749205966 ) ) ;
#97762 = CARTESIAN_POINT ( 'NONE',  ( 4.408870434958439333, 1425.824683284920184, 185.4670092970000042 ) ) ;
#97763 = CARTESIAN_POINT ( 'NONE',  ( -18.80544325660000027, 1424.672153923130054, 224.5457550954980093 ) ) ;
#97764 = CARTESIAN_POINT ( 'NONE',  ( -14.55370911430000014, 1435.825179945700029, 149.7848083361979832 ) ) ;
#97765 = CARTESIAN_POINT ( 'NONE',  ( -105.3795303980000000, 1390.980575111779899, 304.2016934099590344 ) ) ;
#97766 = CARTESIAN_POINT ( 'NONE',  ( 16.94063720780000182, 1507.935533863430010, 188.0799137801979839 ) ) ;
#97768 = CARTESIAN_POINT ( 'NONE',  ( -18.89139539159507919, 1438.542556416878369, 210.7143975199735735 ) ) ;
#97767 = CARTESIAN_POINT ( 'NONE',  ( -15.62861691365340100, 1418.244675075289933, 203.0179649770489902 ) ) ;
#97769 = CARTESIAN_POINT ( 'NONE',  ( -10.10912477582879987, 1472.430577810449904, 210.3411266470020280 ) ) ;
#97770 = VERTEX_POINT ( 'NONE', #4032 ) ;
#97771 = CARTESIAN_POINT ( 'NONE',  ( -16.68463225830000241, 1442.773887286369927, 162.0935120917980043 ) ) ;
#97772 = CARTESIAN_POINT ( 'NONE',  ( 11.71103087170000023, 1438.058396846869982, 147.7520216503980066 ) ) ;
#97773 = CARTESIAN_POINT ( 'NONE',  ( 11.31210319729820135, 1470.591574153610054, 207.8732379879190262 ) ) ;
#97774 = FACE_OUTER_BOUND ( 'NONE', #99216, .T. ) ;
#97775 = CARTESIAN_POINT ( 'NONE',  ( -16.59172940107149330, 1417.375819201424747, 206.4523686363734498 ) ) ;
#97776 = CARTESIAN_POINT ( 'NONE',  ( -2.664388089261293668, 1523.844789899201942, 242.1314412270628793 ) ) ;
#97777 = CARTESIAN_POINT ( 'NONE',  ( 17.83228018670000026, 1408.913060387329779, 213.2813548218979918 ) ) ;
#97778 = CARTESIAN_POINT ( 'NONE',  ( -0.2658540493943280514, 1507.120020986029886, 237.3289608297170048 ) ) ;
#97779 = CARTESIAN_POINT ( 'NONE',  ( 10.59812402283390043, 1477.524000194940072, 229.9254252251899970 ) ) ;
#97780 = CARTESIAN_POINT ( 'NONE',  ( -15.34230038387189943, 1415.677402202110216, 209.0149701286740083 ) ) ;
#97781 = CARTESIAN_POINT ( 'NONE',  ( -109.3135390088490055, 1383.527569083439857, 311.1030218576129869 ) ) ;
#97782 =( BOUNDED_CURVE ( )  B_SPLINE_CURVE ( 3, ( #40956, #24135, #48280, #91372 ),
 .UNSPECIFIED., .F., .F. ) 
 B_SPLINE_CURVE_WITH_KNOTS ( ( 4, 4 ),
 ( 2.356485377174994955, 3.926596519726254897 ),
 .UNSPECIFIED. ) 
 CURVE ( )  GEOMETRIC_REPRESENTATION_ITEM ( )  RATIONAL_B_SPLINE_CURVE ( ( 1.000000000000000000, 0.8048993259319946469, 0.8048993259319946469, 1.000000000000000000 ) ) 
 REPRESENTATION_ITEM ( '' )  );
#97783 = CARTESIAN_POINT ( 'NONE',  ( 5.455371915589999787, 1427.707280442089768, 215.3790498620489871 ) ) ;
#97785 = EDGE_LOOP ( 'NONE', ( #31058, #104432, #23391, #60074 ) ) ;
#97784 = CARTESIAN_POINT ( 'NONE',  ( -18.44599904095050036, 1443.433905668329999, 212.7798859627189927 ) ) ;
#97786 = CARTESIAN_POINT ( 'NONE',  ( -102.8679838510000053, 1381.036522549190067, 309.3638378892590026 ) ) ;
#97787 = CARTESIAN_POINT ( 'NONE',  ( 12.33871145880999975, 1512.142158944850053, 223.9832163156410161 ) ) ;
#97788 = ORIENTED_EDGE ( 'NONE', *, *, #86568, .F. ) ;
#97789 = ORIENTED_EDGE ( 'NONE', *, *, #23261, .T. ) ;
#97790 = CARTESIAN_POINT ( 'NONE',  ( -20.35107102299999937, 1487.435604149590063, 205.0880641165789768 ) ) ;
#97791 = CARTESIAN_POINT ( 'NONE',  ( -109.1645137389999860, 1384.901512809399946, 297.1326343689589748 ) ) ;
#97792 = CARTESIAN_POINT ( 'NONE',  ( -4.363123796622770278, 1423.854800546939941, 184.2546035468919854 ) ) ;
#97794 = CARTESIAN_POINT ( 'NONE',  ( -26.00754374419999948, 1454.033399687029942, 240.2274372898979777 ) ) ;
#97793 = CARTESIAN_POINT ( 'NONE',  ( 24.21285743589101358, 1415.977151558922287, 269.4183131582149713 ) ) ;
#97795 = CARTESIAN_POINT ( 'NONE',  ( -20.12493411150000000, 1494.494608803829806, 190.1457493620980017 ) ) ;
#97796 = CARTESIAN_POINT ( 'NONE',  ( -11.91877802890000027, 1433.473306471390060, 150.2081219906980039 ) ) ;
#97797 = CARTESIAN_POINT ( 'NONE',  ( 27.93020545470000471, 1509.888404654830083, 203.8551627510279900 ) ) ;
#97798 = CARTESIAN_POINT ( 'NONE',  ( -19.19211169099999736, 1486.006664573430044, 189.6295759001980343 ) ) ;
#97799 = VECTOR ( 'NONE', #63344, 1000.000000000000000 ) ;
#97800 = CYLINDRICAL_SURFACE ( 'NONE', #41107, 1.000000000000000888 ) ;
#97801 = DIRECTION ( 'NONE',  ( 1.755985294532464991E-16, -1.000000000000000000, 1.338183447452830017E-16 ) ) ;
#97802 = CARTESIAN_POINT ( 'NONE',  ( -18.65451756193940014, 1507.632629711779828, 229.7110761618599781 ) ) ;
#97803 = CARTESIAN_POINT ( 'NONE',  ( 1.480922050692270009, 1515.075000927530027, 213.4510274295309955 ) ) ;
#97804 = CARTESIAN_POINT ( 'NONE',  ( -9.973184873930010852, 1479.579336554859992, 215.2613112899330190 ) ) ;
#97805 = CARTESIAN_POINT ( 'NONE',  ( -8.333801363508515081, 1509.331394084260182, 237.9487518140551003 ) ) ;
#97807 = ORIENTED_EDGE ( 'NONE', *, *, #37201, .T. ) ;
#97806 = CARTESIAN_POINT ( 'NONE',  ( 1.219850571415770094E-08, 1406.911344650290175, 265.1958365716640174 ) ) ;
#97808 = ORIENTED_EDGE ( 'NONE', *, *, #83871, .T. ) ;
#97809 = CARTESIAN_POINT ( 'NONE',  ( -12.75669765699999836, 1503.496733507889985, 208.6968453557029761 ) ) ;
#97810 = CARTESIAN_POINT ( 'NONE',  ( -22.14708463899999913, 1486.361880417990051, 217.3670993146189971 ) ) ;
#97811 = CARTESIAN_POINT ( 'NONE',  ( -32.97295502609999573, 1460.269649532029916, 269.5004837624980496 ) ) ;
#97812 = CARTESIAN_POINT ( 'NONE',  ( -23.75022901606470782, 1436.081403467656173, 211.7336246957814296 ) ) ;
#97813 = CARTESIAN_POINT ( 'NONE',  ( -113.4000000000000057, 1371.894749952190068, 317.1057287443589985 ) ) ;
#97814 = CARTESIAN_POINT ( 'NONE',  ( 35.01754215041950147, 1450.340935123170084, 136.2235620930159996 ) ) ;
#97815 = CARTESIAN_POINT ( 'NONE',  ( 4.327148319165510237, 1515.152643786259887, 209.4426799714850347 ) ) ;
#97816 = CARTESIAN_POINT ( 'NONE',  ( -11.76065867670000031, 1420.498107173830022, 231.0157263700980081 ) ) ;
#97817 = CIRCLE ( 'NONE', #1285, 3.750000000000000000 ) ;
#97818 = CARTESIAN_POINT ( 'NONE',  ( -30.31052258194577931, 1523.604703353109699, 222.4930856806594193 ) ) ;
#97819 = CARTESIAN_POINT ( 'NONE',  ( -1.136808998351487521, 1484.762897349236027, 182.1973289732482044 ) ) ;
#97820 = CARTESIAN_POINT ( 'NONE',  ( 10.64129648661419658, 1361.926180408836444, 208.3718459617010978 ) ) ;
#97821 = CARTESIAN_POINT ( 'NONE',  ( -45.84226277833369778, 1436.715131148009959, 266.9824418670360160 ) ) ;
#97822 = ORIENTED_EDGE ( 'NONE', *, *, #104881, .T. ) ;
#97823 = CARTESIAN_POINT ( 'NONE',  ( -3.534759143276439808, 1493.082786438550102, 181.5750439270630068 ) ) ;
#97824 = EDGE_LOOP ( 'NONE', ( #33063, #102690, #85005, #61654, #23060, #104590 ) ) ;
#97825 = ORIENTED_EDGE ( 'NONE', *, *, #70554, .F. ) ;
#97826 = CARTESIAN_POINT ( 'NONE',  ( 5.789394662204999875, 1517.164987839469859, 210.8286437561770299 ) ) ;
#97827 = CARTESIAN_POINT ( 'NONE',  ( -9.244110535254980832, 1447.194003664420052, 212.1343190185759795 ) ) ;
#97828 = CARTESIAN_POINT ( 'NONE',  ( -20.86053628100000168, 1508.959219212030121, 190.3806355066980132 ) ) ;
#97829 = CARTESIAN_POINT ( 'NONE',  ( -15.95571536889999997, 1410.408223877029968, 191.3274944925979923 ) ) ;
#97830 = AXIS2_PLACEMENT_3D ( 'NONE', #70039, #68928, #104151 ) ;
#97831 = CARTESIAN_POINT ( 'NONE',  ( -16.68599136316429821, 1461.161685576650143, 228.2799817407029934 ) ) ;
#97832 = ORIENTED_EDGE ( 'NONE', *, *, #41943, .T. ) ;
#97833 = CARTESIAN_POINT ( 'NONE',  ( -0.7526715882979990724, 1516.710624944440042, 201.4081970979170251 ) ) ;
#97834 = CARTESIAN_POINT ( 'NONE',  ( 18.49117120320514829, 1508.844092022591212, 188.2543554909499335 ) ) ;
#97835 = CARTESIAN_POINT ( 'NONE',  ( -26.91388312470140320, 1384.548951572099895, 204.0772839077369838 ) ) ;
#97836 = ORIENTED_EDGE ( 'NONE', *, *, #21990, .T. ) ;
#97837 = CARTESIAN_POINT ( 'NONE',  ( -9.478344589416581201, 1411.163298180099900, 269.3460365866420148 ) ) ;
#97838 = CARTESIAN_POINT ( 'NONE',  ( -0.7352107454670000486, 1428.413060387330006, 91.31218443469779800 ) ) ;
#97839 = CARTESIAN_POINT ( 'NONE',  ( 17.17241001986506888, 1511.187213306747708, 238.6251415217915337 ) ) ;
#97841 = ORIENTED_EDGE ( 'NONE', *, *, #6256, .F. ) ;
#97840 = CARTESIAN_POINT ( 'NONE',  ( -9.978586514397619567, 1364.539968386201963, 210.6218459616987957 ) ) ;
#97842 = EDGE_LOOP ( 'NONE', ( #12796, #68629, #102235, #83020 ) ) ;
#97843 = CARTESIAN_POINT ( 'NONE',  ( 42.08257328447562884, 1454.145434094863049, 269.0735840997347736 ) ) ;
#97844 = EDGE_CURVE ( 'NONE', #99650, #95096, #77158, .T. ) ;
#97845 = B_SPLINE_CURVE_WITH_KNOTS ( 'NONE', 3,
 ( #94143, #17414, #51611, #667, #1217, #95808 ),
 .UNSPECIFIED., .F., .F.,
 ( 4, 2, 4 ),
 ( 1.219745808755950105E-06, 0.01184124321884439703, 0.02355706456992970321 ),
 .UNSPECIFIED. ) ;
#97846 = CARTESIAN_POINT ( 'NONE',  ( -0.6623177435430670501, 1467.634584622510147, 220.2019122221780094 ) ) ;
#97847 = CARTESIAN_POINT ( 'NONE',  ( -8.316672828268760753, 1425.055149638239982, 204.9623390585310005 ) ) ;
#97848 = CARTESIAN_POINT ( 'NONE',  ( -1.456328368119999883, 1485.358061632029830, 182.2073493714979975 ) ) ;
#97849 = AXIS2_PLACEMENT_3D ( 'NONE', #73105, #22104, #107245 ) ;
#97850 = CARTESIAN_POINT ( 'NONE',  ( -17.27558692971449972, 1507.606285623229951, 224.2552697136770234 ) ) ;
#97851 = CARTESIAN_POINT ( 'NONE',  ( -17.97429972279999788, 1430.800360081030249, 226.3842136923979922 ) ) ;
#97852 = CARTESIAN_POINT ( 'NONE',  ( 15.83383049623899730, 1474.212651018609904, 267.1442246111369627 ) ) ;
#97853 = CARTESIAN_POINT ( 'NONE',  ( 12.26979136719999985, 1416.828040475729949, 223.5793546564979977 ) ) ;
#97854 = CARTESIAN_POINT ( 'NONE',  ( 4.129912672550000607, 1446.242909026189864, 182.6856816074980259 ) ) ;
#97855 = CARTESIAN_POINT ( 'NONE',  ( 1.118903270415000151, 1517.003078582959688, 206.2405205581369785 ) ) ;
#97856 = ORIENTED_EDGE ( 'NONE', *, *, #74134, .F. ) ;
#97857 = CARTESIAN_POINT ( 'NONE',  ( -7.604289863101939773, 1426.735970264149955, 206.0920986175900111 ) ) ;
#97858 = CARTESIAN_POINT ( 'NONE',  ( 0.4403324358131759930, 1517.051704035390003, 201.6347831756999938 ) ) ;
#97859 = ORIENTED_EDGE ( 'NONE', *, *, #40161, .F. ) ;
#97860 = CARTESIAN_POINT ( 'NONE',  ( 17.87824514789634023, 1457.869968850633313, 229.1928660838007659 ) ) ;
#97861 = CARTESIAN_POINT ( 'NONE',  ( -6.025152189795589308, 1484.743689720570046, 198.8560543189699956 ) ) ;
#97862 = CARTESIAN_POINT ( 'NONE',  ( 13.56343219680000090, 1416.311719779230089, 196.3989970432979817 ) ) ;
#97863 = CARTESIAN_POINT ( 'NONE',  ( -9.175147725320000447, 1415.658347088709888, 205.8467875627789851 ) ) ;
#97864 = CARTESIAN_POINT ( 'NONE',  ( 20.10486353479999977, 1410.110232032130170, 198.1151493261979795 ) ) ;
#97865 = CARTESIAN_POINT ( 'NONE',  ( 16.68463233076019492, 1445.052233488289176, 162.0935120523188289 ) ) ;
#97866 = CARTESIAN_POINT ( 'NONE',  ( -26.28380303640000193, 1435.415400226489737, 135.3026382325979853 ) ) ;
#97867 = CARTESIAN_POINT ( 'NONE',  ( 32.38601978689629135, 1523.530870145309336, 202.1199661129109586 ) ) ;
#97868 = CARTESIAN_POINT ( 'NONE',  ( 0.7827416214407210138, 1450.881275464169903, 181.6854931341780173 ) ) ;
#97869 = CIRCLE ( 'NONE', #78218, 30.13701971169416183 ) ;
#97870 = LINE ( 'NONE', #98973, #80163 ) ;
#97871 = CARTESIAN_POINT ( 'NONE',  ( -1.123101616545000070, 1517.157901477309906, 214.9105372957470195 ) ) ;
#97872 = EDGE_LOOP ( 'NONE', ( #39907, #1233, #44137, #51863 ) ) ;
#97873 = CARTESIAN_POINT ( 'NONE',  ( 7.708979774182910027, 1516.532320736849897, 206.7210651042560130 ) ) ;
#97874 = B_SPLINE_CURVE_WITH_KNOTS ( 'NONE', 3,
 ( #58593, #69205, #75931, #102226, #51279, #102757 ),
 .UNSPECIFIED., .F., .F.,
 ( 4, 2, 4 ),
 ( -0.02784762759737050009, -0.01392846439159300086, 0.000000000000000000 ),
 .UNSPECIFIED. ) ;
#97875 = CARTESIAN_POINT ( 'NONE',  ( -3.544886644340000448, 1474.831256732490147, 198.2487847239990231 ) ) ;
#97876 = EDGE_CURVE ( 'NONE', #100109, #58839, #45252, .T. ) ;
#97877 = CARTESIAN_POINT ( 'NONE',  ( -3.134084166701379903, 1421.411054285269984, 144.1517906398860021 ) ) ;
#97878 = EDGE_CURVE ( 'NONE', #54701, #95653, #54323, .T. ) ;
#97879 = CARTESIAN_POINT ( 'NONE',  ( -39.85544913743839857, 1446.150425910739841, 136.7763567636360165 ) ) ;
#97880 = EDGE_CURVE ( 'NONE', #107968, #42578, #41340, .T. ) ;
#97881 = CARTESIAN_POINT ( 'NONE',  ( 11.60004869885203682, 1425.937227630464349, 137.5819683612840834 ) ) ;
#97882 = CARTESIAN_POINT ( 'NONE',  ( 3.002008659228135201, 1417.785699668546158, 234.2809593874903555 ) ) ;
#97883 = CARTESIAN_POINT ( 'NONE',  ( 17.92678331089475208, 1423.916767532210088, 225.7531818707438731 ) ) ;
#97884 = EDGE_CURVE ( 'NONE', #110100, #84204, #94306, .T. ) ;
#97885 = CARTESIAN_POINT ( 'NONE',  ( -12.31445988513510059, 1378.367058764619969, 209.7118765406739840 ) ) ;
#97886 = CARTESIAN_POINT ( 'NONE',  ( -34.79013702040099787, 1462.198988287599832, 269.8693405702829864 ) ) ;
#97888 = EDGE_CURVE ( 'NONE', #87268, #94097, #96077, .T. ) ;
#97887 = CARTESIAN_POINT ( 'NONE',  ( 36.66684616735739155, 1440.913060387340010, 254.0481763504310209 ) ) ;
#97889 = CARTESIAN_POINT ( 'NONE',  ( -109.1450418849999835, 1385.242479476409926, 297.1468690488589459 ) ) ;
#97890 = CARTESIAN_POINT ( 'NONE',  ( -32.36513376976815692, 1523.847233649538339, 202.1343711220893908 ) ) ;
#97891 = ORIENTED_EDGE ( 'NONE', *, *, #44859, .F. ) ;
#97892 = CARTESIAN_POINT ( 'NONE',  ( -2.487935123034410001, 1509.038615930399828, 213.6090957347729784 ) ) ;
#97893 = AXIS2_PLACEMENT_3D ( 'NONE', #57007, #109058, #73807 ) ;
#97894 = CARTESIAN_POINT ( 'NONE',  ( -19.11224328149206642, 1485.525743910654683, 189.6460228031468773 ) ) ;
#97895 = CARTESIAN_POINT ( 'NONE',  ( -1.144427402640000091, 1442.540072109689845, 200.3174140758290207 ) ) ;
#97896 = CARTESIAN_POINT ( 'NONE',  ( 1.901185863359999839, 1498.995677176629897, 235.9662232939979845 ) ) ;
#97897 = CIRCLE ( 'NONE', #56845, 1.999999999999998668 ) ;
#97898 = DIRECTION ( 'NONE',  ( 0.000000000000000000, -1.000000000000000000, 0.000000000000000000 ) ) ;
#97899 = CARTESIAN_POINT ( 'NONE',  ( -8.313149309269999065, 1507.316766614329936, 235.1568494565980245 ) ) ;
#97900 = CARTESIAN_POINT ( 'NONE',  ( -30.66717156608859796, 1383.841235968630144, 228.5150949522549979 ) ) ;
#97901 = CARTESIAN_POINT ( 'NONE',  ( -2.480175250669919951, 1429.207669930499833, 200.0830571243679969 ) ) ;
#97902 = EDGE_CURVE ( 'NONE', #15423, #99871, #58531, .T. ) ;
#97903 = CARTESIAN_POINT ( 'NONE',  ( -11.53021216923110082, 1501.524780145790146, 208.7332286060340039 ) ) ;
#97904 = FACE_OUTER_BOUND ( 'NONE', #12415, .T. ) ;
#97906 = ORIENTED_EDGE ( 'NONE', *, *, #21343, .F. ) ;
#97905 = DIRECTION ( 'NONE',  ( 0.7044160264027579110, -0.08715574274766998975, 0.7044160264027579110 ) ) ;
#97907 = CARTESIAN_POINT ( 'NONE',  ( -0.7975830076839999228, 1452.841034471829971, 183.3931114573979926 ) ) ;
#97908 = CARTESIAN_POINT ( 'NONE',  ( -18.79955029639999964, 1379.850043559990127, 215.7272756679390113 ) ) ;
#97909 = CARTESIAN_POINT ( 'NONE',  ( -3.411708654729999513, 1475.348535422589975, 198.9840501600990024 ) ) ;
#97911 = ORIENTED_EDGE ( 'NONE', *, *, #93972, .T. ) ;
#97910 = DIRECTION ( 'NONE',  ( -0.6736849260149578855, 0.000000000000000000, 0.7390186874905266823 ) ) ;
#97912 = CARTESIAN_POINT ( 'NONE',  ( -18.29179247696389865, 1466.060385685149868, 217.7541634367629797 ) ) ;
#97913 = ORIENTED_EDGE ( 'NONE', *, *, #105810, .T. ) ;
#97914 = EDGE_CURVE ( 'NONE', #1585, #70769, #3155, .T. ) ;
#97915 =( BOUNDED_CURVE ( )  B_SPLINE_CURVE ( 3, ( #4066, #108701, #15708, #48266 ),
 .UNSPECIFIED., .F., .F. ) 
 B_SPLINE_CURVE_WITH_KNOTS ( ( 4, 4 ),
 ( 1.009833105023860034, 2.131759800080520240 ),
 .UNSPECIFIED. ) 
 CURVE ( )  GEOMETRIC_REPRESENTATION_ITEM ( )  RATIONAL_B_SPLINE_CURVE ( ( 1.000000000000000000, 0.8978286673593871559, 0.8978286673593871559, 1.000000000000000000 ) ) 
 REPRESENTATION_ITEM ( '' )  );
#97916 = B_SPLINE_CURVE_WITH_KNOTS ( 'NONE', 5,
 ( #80667, #30799, #90701, #13988, #39764, #73371 ),
 .UNSPECIFIED., .F., .F.,
 ( 6, 6 ),
 ( 0.5082988451364722771, 1.000000000000000000 ),
 .UNSPECIFIED. ) ;
#97917 = CARTESIAN_POINT ( 'NONE',  ( -11.82541222281230020, 1389.477605041999823, 215.1362464586540000 ) ) ;
#97918 = CARTESIAN_POINT ( 'NONE',  ( -10.67458942334280003, 1390.939239166159950, 215.3172498179779666 ) ) ;
#97919 = CARTESIAN_POINT ( 'NONE',  ( -18.19590854888186726, 1522.862737210650039, 180.0410247165186490 ) ) ;
#97920 = ADVANCED_FACE ( 'NONE', ( #75509 ), #91730, .F. ) ;
#97921 = CARTESIAN_POINT ( 'NONE',  ( 10.29420224292342745, 1504.334860404003166, 214.4873101959476003 ) ) ;
#97922 = CARTESIAN_POINT ( 'NONE',  ( 4.329448776274299249, 1515.064792882709980, 211.4519800890089982 ) ) ;
#97923 = CARTESIAN_POINT ( 'NONE',  ( 20.41258333560000082, 1494.156730172889866, 204.1224707391089908 ) ) ;
#97924 = CIRCLE ( 'NONE', #76438, 30.60516481925333210 ) ;
#97925 = CARTESIAN_POINT ( 'NONE',  ( 6.765186941703619894, 1409.149305921059749, 195.7697136597590202 ) ) ;
#97926 = CARTESIAN_POINT ( 'NONE',  ( 18.52339265480000208, 1425.745301197430081, 224.9617099063980277 ) ) ;
#97927 = CARTESIAN_POINT ( 'NONE',  ( -97.82861174526568959, 1385.215246727240128, 295.8056424823309953 ) ) ;
#97928 = DIRECTION ( 'NONE',  ( 0.000000000000000000, 0.000000000000000000, 1.000000000000000000 ) ) ;
#97929 = CARTESIAN_POINT ( 'NONE',  ( -68.11985932390000187, 1379.748509173530010, 278.8066904925590279 ) ) ;
#97930 = CARTESIAN_POINT ( 'NONE',  ( -3.885481994197490074, 1448.980853271389833, 185.0328430115930018 ) ) ;
#97931 = ORIENTED_EDGE ( 'NONE', *, *, #10317, .T. ) ;
#97932 = VERTEX_POINT ( 'NONE', #63945 ) ;
#97933 = FACE_OUTER_BOUND ( 'NONE', #58052, .T. ) ;
#97934 = CARTESIAN_POINT ( 'NONE',  ( -12.25713978275359928, 1416.640375558050209, 194.6766261173120256 ) ) ;
#97935 = CARTESIAN_POINT ( 'NONE',  ( -1.680260975536200130, 1496.115540335259993, 196.8918274691459942 ) ) ;
#97936 = CARTESIAN_POINT ( 'NONE',  ( -5.906668414434429117E-11, 1466.311335111799963, 242.6050078029819872 ) ) ;
#97937 = CARTESIAN_POINT ( 'NONE',  ( -20.33293110796009984, 1499.214264760269998, 190.6403736919519929 ) ) ;
#97938 = CARTESIAN_POINT ( 'NONE',  ( 1.195323752479999779, 1396.139239339430105, 221.0537008139980060 ) ) ;
#97939 = CARTESIAN_POINT ( 'NONE',  ( 19.16007812963110268, 1428.477567333490015, 209.6896849280039987 ) ) ;
#97940 = CARTESIAN_POINT ( 'NONE',  ( -1.438892276100000034, 1452.191226728930133, 183.8587014809980076 ) ) ;
#97941 = CARTESIAN_POINT ( 'NONE',  ( -11.75150806997721276, 1363.816428733470957, 208.3718459617010978 ) ) ;
#97942 = CARTESIAN_POINT ( 'NONE',  ( -26.53975464933690986, 1436.733422015536462, 136.8030177142773880 ) ) ;
#97943 = CARTESIAN_POINT ( 'NONE',  ( -22.15347906188290139, 1496.414302325609924, 208.5267879710629870 ) ) ;
#97944 = CARTESIAN_POINT ( 'NONE',  ( -6.952166420425000659, 1517.213554313520035, 207.4130983078469797 ) ) ;
#97945 = AXIS2_PLACEMENT_3D ( 'NONE', #104565, #60934, #95612 ) ;
#97946 = CARTESIAN_POINT ( 'NONE',  ( 11.93966352644169859, 1433.552769406360085, 150.1888638864129746 ) ) ;
#97947 = CARTESIAN_POINT ( 'NONE',  ( -13.30603026154990154, 1434.901373284009878, 148.9434964573779894 ) ) ;
#97948 = CARTESIAN_POINT ( 'NONE',  ( -8.297448664060000922, 1384.938007622469968, 218.7034657859290121 ) ) ;
#97949 = CARTESIAN_POINT ( 'NONE',  ( 16.34466203799999917, 1409.483828562729968, 193.4811910679979974 ) ) ;
#97950 = CARTESIAN_POINT ( 'NONE',  ( -0.7967037284469989933, 1496.366648252889945, 196.7585635602989953 ) ) ;
#97951 = CARTESIAN_POINT ( 'NONE',  ( -4.461124787584389573, 1496.650352879389857, 201.9768976816139912 ) ) ;
#97952 = ORIENTED_EDGE ( 'NONE', *, *, #57594, .T. ) ;
#97953 = CARTESIAN_POINT ( 'NONE',  ( 38.77640762290000254, 1433.500815606669903, 259.1404900223979553 ) ) ;
#97954 = CARTESIAN_POINT ( 'NONE',  ( -24.71942444569999964, 1469.238022050230029, 202.0311767578679962 ) ) ;
#97956 = DIRECTION ( 'NONE',  ( 0.000000000000000000, 0.000000000000000000, 1.000000000000000000 ) ) ;
#97955 = CARTESIAN_POINT ( 'NONE',  ( -10.46183320403099870, 1425.378319878120010, 99.91631404394871652 ) ) ;
#97957 = B_SPLINE_CURVE_WITH_KNOTS ( 'NONE', 3,
 ( #55925, #21723, #90045, #4944, #13880, #5504, #46977, #106845, #39662, #91710 ),
 .UNSPECIFIED., .F., .F.,
 ( 4, 2, 2, 2, 4 ),
 ( 0.000000000000000000, 0.2500000000000000000, 0.5000000000000000000, 0.7500000000000000000, 1.000000000000000000 ),
 .UNSPECIFIED. ) ;
#97958 = CARTESIAN_POINT ( 'NONE',  ( -19.44405420005750074, 1410.830242043655289, 270.0540949853959205 ) ) ;
#97959 = CARTESIAN_POINT ( 'NONE',  ( -7.831970043950000182, 1421.243762745730010, 220.7330770330979988 ) ) ;
#97960 = CARTESIAN_POINT ( 'NONE',  ( 0.01339502592799870009, 1487.310215832789936, 219.9787594541990075 ) ) ;
#97961 = CARTESIAN_POINT ( 'NONE',  ( 2.503416217964581580, 1448.820465288596779, 154.6001883531548344 ) ) ;
#97962 = CARTESIAN_POINT ( 'NONE',  ( 27.43975379009999926, 1451.094596967429879, 136.3642754792980156 ) ) ;
#97963 = EDGE_LOOP ( 'NONE', ( #14381, #68278 ) ) ;
#97964 = CARTESIAN_POINT ( 'NONE',  ( 3.763296693692190331, 1398.025494293209931, 196.0977038891449808 ) ) ;
#97965 = CARTESIAN_POINT ( 'NONE',  ( 13.22750721609810398, 1513.553906385406208, 225.9068792231137195 ) ) ;
#97966 = CARTESIAN_POINT ( 'NONE',  ( 38.20494153861019981, 1442.993962785479880, 137.1161392804919785 ) ) ;
#97967 = ORIENTED_EDGE ( 'NONE', *, *, #75513, .T. ) ;
#97968 = VERTEX_POINT ( 'NONE', #109105 ) ;
#97969 = AXIS2_PLACEMENT_3D ( 'NONE', #28099, #27005, #62289 ) ;
#97970 = CARTESIAN_POINT ( 'NONE',  ( 9.218373049180989653, 1451.410758823449896, 210.0413447373219924 ) ) ;
#97971 = CARTESIAN_POINT ( 'NONE',  ( 5.057110678409999949, 1424.030137221399855, 193.7146012876989971 ) ) ;
#97972 = EDGE_CURVE ( 'NONE', #24298, #99485, #33109, .T. ) ;
#97973 = ORIENTED_EDGE ( 'NONE', *, *, #77539, .F. ) ;
#97974 = CARTESIAN_POINT ( 'NONE',  ( 4.668127331444700268, 1508.551704406479985, 204.7884844211849895 ) ) ;
#97975 = CARTESIAN_POINT ( 'NONE',  ( 21.04904418909999819, 1494.916427559390058, 209.1218459616989946 ) ) ;
#97976 = AXIS2_PLACEMENT_3D ( 'NONE', #83584, #24224, #58411 ) ;
#97977 = ADVANCED_FACE ( 'NONE', ( #108535 ), #37095, .T. ) ;
#97978 = CARTESIAN_POINT ( 'NONE',  ( -3.203421013219999836, 1479.771999117829864, 235.5522340181979928 ) ) ;
#97979 = CARTESIAN_POINT ( 'NONE',  ( 16.33500296837753041, 1517.151704408390060, 214.0369884316988305 ) ) ;
#97980 = VERTEX_POINT ( 'NONE', #100134 ) ;
#97981 = AXIS2_PLACEMENT_3D ( 'NONE', #22080, #32169, #90406 ) ;
#97982 = CARTESIAN_POINT ( 'NONE',  ( 46.15241393044949803, 1440.912967216340121, 268.2045458581380331 ) ) ;
#97983 = CARTESIAN_POINT ( 'NONE',  ( -12.50318290573809854, 1415.427621830080170, 221.4521480450309809 ) ) ;
#97984 = CARTESIAN_POINT ( 'NONE',  ( 0.04457229829839999546, 1420.440674599429940, 183.2993309066980032 ) ) ;
#97985 = CARTESIAN_POINT ( 'NONE',  ( -5.007588685045000432, 1516.804776704140068, 203.3466091393569855 ) ) ;
#97986 = ORIENTED_EDGE ( 'NONE', *, *, #59080, .T. ) ;
#97987 = CARTESIAN_POINT ( 'NONE',  ( 8.437259666070110242, 1482.594120399739950, 217.4026692653139889 ) ) ;
#97988 = EDGE_CURVE ( 'NONE', #80761, #6825, #67660, .T. ) ;
#97989 = CARTESIAN_POINT ( 'NONE',  ( 13.42118519619293160, 1443.449014888631837, 187.9204824381897083 ) ) ;
#97990 = VERTEX_POINT ( 'NONE', #40780 ) ;
#97991 = EDGE_LOOP ( 'NONE', ( #43201, #45445, #38577, #50533 ) ) ;
#97992 = CARTESIAN_POINT ( 'NONE',  ( -10.48469270268349796, 1480.274672445829992, 208.2228694171070345 ) ) ;
#97993 = CARTESIAN_POINT ( 'NONE',  ( -29.17014196280706173, 1526.382868172863482, 217.2191814580075970 ) ) ;
#97994 = CARTESIAN_POINT ( 'NONE',  ( 2.371290244962170224, 1497.318959729730068, 197.3528097553119949 ) ) ;
#97995 = CARTESIAN_POINT ( 'NONE',  ( -3.786808085590160022, 1468.516302267170204, 219.2555408501270051 ) ) ;
#97996 = CARTESIAN_POINT ( 'NONE',  ( 20.82408115712189911, 1452.185867449390116, 142.2070257201390007 ) ) ;
#97997 = CARTESIAN_POINT ( 'NONE',  ( 9.220875156419999996, 1420.949518439220128, 196.8516559346990107 ) ) ;
#97998 = CARTESIAN_POINT ( 'NONE',  ( -1.656993444572020024, 1475.839453786890090, 220.4462510233660169 ) ) ;
#97999 = CARTESIAN_POINT ( 'NONE',  ( -109.5833881897985265, 1382.919105250094844, 297.2490322646984851 ) ) ;
#98000 = CARTESIAN_POINT ( 'NONE',  ( -20.29127127059840063, 1509.661394863832811, 230.8411074860736960 ) ) ;
#98001 = DIRECTION ( 'NONE',  ( -0.7071067811865490160, 0.000000000000000000, 0.7071067811865460184 ) ) ;
#98003 = CARTESIAN_POINT ( 'NONE',  ( -105.6997970149250108, 1391.688863015299830, 304.2060425153250094 ) ) ;
#98002 = CARTESIAN_POINT ( 'NONE',  ( -16.23266583089999671, 1504.391494419190167, 208.8786546347319870 ) ) ;
#98004 = CARTESIAN_POINT ( 'NONE',  ( -64.37783753527037334, 1379.747207013340358, 273.6112401814819464 ) ) ;
#98005 = AXIS2_PLACEMENT_3D ( 'NONE', #4975, #107434, #30729 ) ;
#98006 = CARTESIAN_POINT ( 'NONE',  ( -24.42411529408670035, 1509.071565208550055, 222.5078051949110147 ) ) ;
#98007 = CARTESIAN_POINT ( 'NONE',  ( -7.304088287825000414, 1513.265135866609853, 201.5893727638369910 ) ) ;
#98008 = ORIENTED_EDGE ( 'NONE', *, *, #10390, .T. ) ;
#98009 = CARTESIAN_POINT ( 'NONE',  ( 27.19819524420000079, 1434.390360741930181, 248.0989693021979861 ) ) ;
#98010 = CARTESIAN_POINT ( 'NONE',  ( -3.835404308833623155, 1396.046995657106436, 202.1011854665750036 ) ) ;
#98011 = CARTESIAN_POINT ( 'NONE',  ( -87.22070388642269734, 1384.976040036309996, 307.6860165158650489 ) ) ;
#98012 = EDGE_CURVE ( 'NONE', #60698, #93813, #60366, .T. ) ;
#98013 = CARTESIAN_POINT ( 'NONE',  ( 4.114445074009999814, 1505.903523102289910, 220.4261431997990144 ) ) ;
#98014 = CARTESIAN_POINT ( 'NONE',  ( -15.30092036139999934, 1415.735729274460027, 210.9263093465289955 ) ) ;
#98016 = VERTEX_POINT ( 'NONE', #92830 ) ;
#98015 = CARTESIAN_POINT ( 'NONE',  ( -16.35827608089219964, 1420.124075138139915, 209.1664405693819901 ) ) ;
#98017 = EDGE_CURVE ( 'NONE', #50916, #96052, #1301, .T. ) ;
#98018 = CARTESIAN_POINT ( 'NONE',  ( 4.440855653409998993, 1430.031384578290044, 217.0414287054690021 ) ) ;
#98019 = CARTESIAN_POINT ( 'NONE',  ( -7.341316150999999179E-16, 1441.600846913620217, 150.7224806086979640 ) ) ;
#98020 = DIRECTION ( 'NONE',  ( 1.000000000000000000, 0.000000000000000000, 0.000000000000000000 ) ) ;
#98021 = CARTESIAN_POINT ( 'NONE',  ( -0.9085210321814130019, 1429.982231419140135, 199.7651695299570065 ) ) ;
#98022 = CARTESIAN_POINT ( 'NONE',  ( 13.59434822483500049, 1512.526319173689899, 225.1381234417670214 ) ) ;
#98023 = CARTESIAN_POINT ( 'NONE',  ( 4.116054228253682723, 1370.396681933733362, 208.4739280433301758 ) ) ;
#98024 = CARTESIAN_POINT ( 'NONE',  ( 1.548969699112269893, 1456.873934020939942, 199.3713766746409988 ) ) ;
#98025 = DIRECTION ( 'NONE',  ( 6.332794898383918850E-17, 1.000000000000000000, -8.716344404180429969E-17 ) ) ;
#98026 = CARTESIAN_POINT ( 'NONE',  ( 16.69334696330000156, 1419.771389454430164, 226.9180811344979816 ) ) ;
#98027 = EDGE_CURVE ( 'NONE', #66323, #39930, #15550, .T. ) ;
#98029 = CARTESIAN_POINT ( 'NONE',  ( -22.69876404239284184, 1522.861859112240154, 236.8953202675672287 ) ) ;
#98028 = AXIS2_PLACEMENT_3D ( 'NONE', #73045, #3108, #80344 ) ;
#98030 = CARTESIAN_POINT ( 'NONE',  ( -1.717432486395000124, 1516.836638729160086, 206.8395443540670158 ) ) ;
#98031 = CARTESIAN_POINT ( 'NONE',  ( 46.16778666300000111, 1438.897380407539913, 266.9714988366979469 ) ) ;
#98032 = CARTESIAN_POINT ( 'NONE',  ( -17.45742012540000232, 1409.522686931430144, 222.8493455500980076 ) ) ;
#98033 = CARTESIAN_POINT ( 'NONE',  ( 19.95725839569999849, 1436.009163759079911, 145.3713295913979948 ) ) ;
#98034 = CARTESIAN_POINT ( 'NONE',  ( 4.652384135149589817, 1440.963318168330034, 155.5568921565159997 ) ) ;
#98035 = EDGE_CURVE ( 'NONE', #79540, #96354, #88892, .T. ) ;
#98036 = CARTESIAN_POINT ( 'NONE',  ( -16.40119657999539982, 1409.652435746110086, 192.2255775475670134 ) ) ;
#98037 = DIRECTION ( 'NONE',  ( -1.755985294532469921E-16, 1.000000000000000000, -1.338183447452831989E-16 ) ) ;
#98038 = CARTESIAN_POINT ( 'NONE',  ( -31.33756689035240584, 1523.580203803270933, 221.9021554055879619 ) ) ;
#98039 = CARTESIAN_POINT ( 'NONE',  ( -38.70772116073620595, 1437.296229215239919, 135.0862262929739757 ) ) ;
#98040 = CARTESIAN_POINT ( 'NONE',  ( 0.2114665854462480232, 1456.524817466450031, 183.1021823691539794 ) ) ;
#98041 = CARTESIAN_POINT ( 'NONE',  ( -13.29060849360579866, 1407.754373188279942, 210.5456034691529794 ) ) ;
#98042 = CARTESIAN_POINT ( 'NONE',  ( -14.33002530880000158, 1414.913060387329779, 201.6311097326980075 ) ) ;
#98043 = CARTESIAN_POINT ( 'NONE',  ( -3.970164549730000214, 1515.569681836989957, 207.9977555470689765 ) ) ;
#98044 = CARTESIAN_POINT ( 'NONE',  ( -0.7042569225233946684, 1484.127373294593099, 198.4525884679282512 ) ) ;
#98045 = CARTESIAN_POINT ( 'NONE',  ( 12.91331072740000074, 1434.774329726679980, 147.2731663809980205 ) ) ;
#98046 = CARTESIAN_POINT ( 'NONE',  ( -38.53505232114799384, 1437.347470674169926, 134.0999999971709826 ) ) ;
#98047 = DIRECTION ( 'NONE',  ( -0.8926073982886787439, 0.4508348173337058951, 0.000000000000000000 ) ) ;
#98048 = VERTEX_POINT ( 'NONE', #53628 ) ;
#98049 = CARTESIAN_POINT ( 'NONE',  ( 1.847634023740000186, 1478.089546284990092, 198.8590795994990117 ) ) ;
#98050 = CARTESIAN_POINT ( 'NONE',  ( 40.40805859990000215, 1443.620986539019896, 137.1126368707979850 ) ) ;
#98051 = CARTESIAN_POINT ( 'NONE',  ( -10.94025997009999962, 1492.428993089990172, 207.5139326340290040 ) ) ;
#98052 = EDGE_CURVE ( 'NONE', #42640, #22416, #69245, .T. ) ;
#98053 = CARTESIAN_POINT ( 'NONE',  ( -4.602356253840000022, 1468.583955076089978, 189.7619545879989857 ) ) ;
#98054 = B_SPLINE_CURVE_WITH_KNOTS ( 'NONE', 5,
 ( #108883, #48450, #30517, #40574, #82015, #82588 ),
 .UNSPECIFIED., .F., .F.,
 ( 6, 6 ),
 ( 0.000000000000000000, 1.000000000000000000 ),
 .UNSPECIFIED. ) ;
#98055 = CARTESIAN_POINT ( 'NONE',  ( 13.36711898873540072, 1508.094956433400057, 233.0794756770270055 ) ) ;
#98056 = CARTESIAN_POINT ( 'NONE',  ( 40.50869282367309410, 1425.163924263866193, 269.1154144834585509 ) ) ;
#98057 = CARTESIAN_POINT ( 'NONE',  ( 18.19590854888146225, 1522.862737210649811, 180.0410247165184217 ) ) ;
#98058 = CARTESIAN_POINT ( 'NONE',  ( -17.84338787552398031, 1523.481610118015169, 237.8836641335898605 ) ) ;
#98059 = ADVANCED_FACE ( 'NONE', ( #35686, #78804 ), #9933, .T. ) ;
#98060 = CARTESIAN_POINT ( 'NONE',  ( -26.61732439379999704, 1507.999000608030201, 214.1432811199779849 ) ) ;
#98061 = CARTESIAN_POINT ( 'NONE',  ( -95.07784190500939303, 1384.609914070380000, 310.0516348293959936 ) ) ;
#98062 = B_SPLINE_SURFACE_WITH_KNOTS ( 'NONE', 5, 5, ( 
 ( #21289, #90722, #48751, #46550, #47634, #6167 ),
 ( #99111, #14006, #90163, #48193, #98018, #13444 ),
 ( #72303, #55496, #5066, #4533, #38667, #39213 ),
 ( #82331, #98569, #5631, #21838, #80684, #108072 ),
 ( #65550, #39782, #56036, #81763, #73391, #107526 ),
 ( #30816, #64993, #3996, #73941, #99659, #22950 ),
 ( #57155, #38121, #91280, #14560, #82874, #40321 ),
 ( #74503, #108632, #76136, #101301, #83421, #32485 ),
 ( #67202, #100759, #43093, #34128, #76683, #33556 ) ),
 .UNSPECIFIED., .F., .F., .F.,
 ( 6, 3, 6 ),
 ( 6, 6 ),
 ( 0.000000000000000000, 3.560296025780000040, 7.120592051560000080 ),
 ( 0.000000000000000000, 2.000000000000000000 ),
 .UNSPECIFIED. ) ;
#98063 = CARTESIAN_POINT ( 'NONE',  ( -38.54599120904159548, 1384.986460508979917, 211.5487390164689998 ) ) ;
#98064 = CARTESIAN_POINT ( 'NONE',  ( 17.83486663330486621, 1523.678648413191695, 180.3677388339000061 ) ) ;
#98065 = CARTESIAN_POINT ( 'NONE',  ( -4.986724123564950872, 1508.551704408389924, 206.5918190285340188 ) ) ;
#98066 = CIRCLE ( 'NONE', #8696, 1.999999999999998668 ) ;
#98067 = CARTESIAN_POINT ( 'NONE',  ( -27.02655704099999667, 1451.108971386630174, 136.3738572239980158 ) ) ;
#98068 = CARTESIAN_POINT ( 'NONE',  ( 1.191524307911312031, 1526.382868172864164, 179.0083900503168479 ) ) ;
#98070 = VERTEX_POINT ( 'NONE', #95597 ) ;
#98069 = CARTESIAN_POINT ( 'NONE',  ( -21.84020450222019605, 1523.481610426287716, 234.9798068779743403 ) ) ;
#98071 = CARTESIAN_POINT ( 'NONE',  ( -109.1308573929999852, 1384.902467940340102, 311.2647317742590189 ) ) ;
#98072 = AXIS2_PLACEMENT_3D ( 'NONE', #94003, #530, #59334 ) ;
#98073 = CARTESIAN_POINT ( 'NONE',  ( 4.063344664623878444, 1421.082680532014365, 137.4056175706463705 ) ) ;
#98074 = CARTESIAN_POINT ( 'NONE',  ( 3.005276066430000448, 1369.205039411269809, 210.6218459616989946 ) ) ;
#98075 = CARTESIAN_POINT ( 'NONE',  ( -11.90129930089999988, 1415.245980409429876, 195.5451049489979880 ) ) ;
#98076 = CARTESIAN_POINT ( 'NONE',  ( -14.03757963822240029, 1511.404482726790093, 183.4262285374240093 ) ) ;
#98077 = CARTESIAN_POINT ( 'NONE',  ( 23.17009332390000154, 1410.217324300129803, 212.3038800746780055 ) ) ;
#98078 = CARTESIAN_POINT ( 'NONE',  ( -1.974599305947250194, 1419.504832324920244, 185.8215509651549837 ) ) ;
#98079 = CARTESIAN_POINT ( 'NONE',  ( -13.21674774426140075, 1468.729004077370064, 191.9552650913620084 ) ) ;
#98080 = CARTESIAN_POINT ( 'NONE',  ( -5.513435588854999736, 1508.551704408389924, 216.1347675159770176 ) ) ;
#98082 = CARTESIAN_POINT ( 'NONE',  ( -10.57226022420000078, 1380.120851655610068, 202.6664852126289986 ) ) ;
#98081 = CARTESIAN_POINT ( 'NONE',  ( -10.98084428610000174, 1433.016922418659988, 151.7694244828979890 ) ) ;
#98083 = CARTESIAN_POINT ( 'NONE',  ( 26.02702435453459984, 1469.349391678469829, 207.6976918991759931 ) ) ;
#98084 = CARTESIAN_POINT ( 'NONE',  ( -101.5731991332999939, 1376.302340817389904, 304.2218459572590064 ) ) ;
#98085 = CARTESIAN_POINT ( 'NONE',  ( -1966.823930461590180, 11221.53578756869865, -25.46789276350280318 ) ) ;
#98086 = CARTESIAN_POINT ( 'NONE',  ( -20.64498752849999974, 1505.794066315190094, 209.1536330714710061 ) ) ;
#98087 = CARTESIAN_POINT ( 'NONE',  ( -8.910387285859998840, 1362.858511851210096, 210.6218459616991936 ) ) ;
#98088 = CARTESIAN_POINT ( 'NONE',  ( 3.254401403604999743, 1516.919782530640077, 205.0791161293069820 ) ) ;
#98089 = AXIS2_PLACEMENT_3D ( 'NONE', #12595, #55725, #20420 ) ;
#98090 = CARTESIAN_POINT ( 'NONE',  ( -4.404857644985120224, 1485.524168335080049, 183.0886271376960224 ) ) ;
#98091 = CARTESIAN_POINT ( 'NONE',  ( -12.14581532088685201, 1421.748045606286951, 210.6453319782864071 ) ) ;
#98093 = ORIENTED_EDGE ( 'NONE', *, *, #72193, .T. ) ;
#98092 = CARTESIAN_POINT ( 'NONE',  ( -67.32292340012330101, 1379.744822991889805, 278.5476412461240443 ) ) ;
#98094 = ORIENTED_EDGE ( 'NONE', *, *, #24941, .F. ) ;
#98095 = CARTESIAN_POINT ( 'NONE',  ( 27.78931436370000085, 1508.066562786630129, 211.8879754161380333 ) ) ;
#98096 = ORIENTED_EDGE ( 'NONE', *, *, #46086, .T. ) ;
#98097 = CARTESIAN_POINT ( 'NONE',  ( 7.316304296407109220, 1507.280216653023899, 182.6970439867345704 ) ) ;
#98098 = CARTESIAN_POINT ( 'NONE',  ( 1.499372387982010224, 1414.913526845469960, 192.0176458413389753 ) ) ;
#98099 =( BOUNDED_CURVE ( )  B_SPLINE_CURVE ( 3, ( #97284, #105709, #28991, #63178 ),
 .UNSPECIFIED., .F., .F. ) 
 B_SPLINE_CURVE_WITH_KNOTS ( ( 4, 4 ),
 ( 4.712388980384689674, 6.283185307179586232 ),
 .UNSPECIFIED. ) 
 CURVE ( )  GEOMETRIC_REPRESENTATION_ITEM ( )  RATIONAL_B_SPLINE_CURVE ( ( 1.000000000000000000, 0.8047378541243649375, 0.8047378541243649375, 1.000000000000000000 ) ) 
 REPRESENTATION_ITEM ( '' )  );
#98101 = CARTESIAN_POINT ( 'NONE',  ( 0.9350669245199999535, 1508.880473741730157, 179.9494619221979974 ) ) ;
#98100 = CARTESIAN_POINT ( 'NONE',  ( 15.92940539777539932, 1419.249169548590089, 191.2576731443239737 ) ) ;
#98102 = CARTESIAN_POINT ( 'NONE',  ( -1.701850495234999983, 1516.908147884120126, 210.2591426210370003 ) ) ;
#98103 = CARTESIAN_POINT ( 'NONE',  ( -24.49684469894179983, 1452.057661785150003, 136.0510194727069972 ) ) ;
#98104 = CARTESIAN_POINT ( 'NONE',  ( -105.8385759250460012, 1378.913060387480073, 304.6883937350420410 ) ) ;
#98105 = CARTESIAN_POINT ( 'NONE',  ( 4.165142600520000293, 1409.058510372029787, 229.9895894434979766 ) ) ;
#98106 = CARTESIAN_POINT ( 'NONE',  ( -20.49599333844893678, 1525.960063244516959, 184.3798832129038203 ) ) ;
#98107 = CARTESIAN_POINT ( 'NONE',  ( 0.000000000000000000, 0.000000000000000000, 0.000000000000000000 ) ) ;
#98108 = CARTESIAN_POINT ( 'NONE',  ( 39.77086280987219880, 1438.526156309450016, 134.0999999980039945 ) ) ;
#98109 = CARTESIAN_POINT ( 'NONE',  ( -7.023365448820000800, 1481.189736218790131, 206.9209398003490037 ) ) ;
#98110 = ORIENTED_EDGE ( 'NONE', *, *, #26715, .F. ) ;
#98111 = CARTESIAN_POINT ( 'NONE',  ( 2.740689650046610026, 1426.136172726640098, 188.7843778714569964 ) ) ;
#98112 = CARTESIAN_POINT ( 'NONE',  ( -1.515897882684319908, 1431.595581664609881, 200.8620100226909813 ) ) ;
#98113 = ORIENTED_EDGE ( 'NONE', *, *, #77513, .F. ) ;
#98114 = ORIENTED_EDGE ( 'NONE', *, *, #17886, .F. ) ;
#98115 = ORIENTED_EDGE ( 'NONE', *, *, #102497, .F. ) ;
#98116 = CARTESIAN_POINT ( 'NONE',  ( 12.50587472938863876, 1410.723098928997388, 228.7755205085364878 ) ) ;
#98117 = CARTESIAN_POINT ( 'NONE',  ( 32.80316127680803362, 1523.919934424249959, 217.1667916731834680 ) ) ;
#98118 = ADVANCED_FACE ( 'NONE', ( #25612 ), #27757, .F. ) ;
#98119 = CARTESIAN_POINT ( 'NONE',  ( 1.817252217737630682, 1451.599092923090211, 154.0952177214090568 ) ) ;
#98120 = CARTESIAN_POINT ( 'NONE',  ( -8.862056491009999704, 1384.892951007250076, 218.6851137842390074 ) ) ;
#98121 = CARTESIAN_POINT ( 'NONE',  ( -17.48093814192715101, 1448.293137033754647, 218.1689033131428346 ) ) ;
#98122 = CARTESIAN_POINT ( 'NONE',  ( -66.20869285293976247, 1379.742364948664090, 274.8035288233667188 ) ) ;
#98123 = CARTESIAN_POINT ( 'NONE',  ( 1.055290578150000158, 1464.343017313090058, 199.3193465885090063 ) ) ;
#98124 = CARTESIAN_POINT ( 'NONE',  ( 9817.198718245359487, 2837.742859962510011, 1424.354596153399825 ) ) ;
#98125 = CARTESIAN_POINT ( 'NONE',  ( 10.47220851269999997, 1415.931784856029935, 194.6558979389980095 ) ) ;
#98126 = CARTESIAN_POINT ( 'NONE',  ( -54.61776087596129514, 1384.642101012380181, 233.1560539664220073 ) ) ;
#98127 = VERTEX_POINT ( 'NONE', #19426 ) ;
#98128 =( BOUNDED_CURVE ( )  B_SPLINE_CURVE ( 3, ( #1025, #9950, #35150, #61485 ),
 .UNSPECIFIED., .F., .T. ) 
 B_SPLINE_CURVE_WITH_KNOTS ( ( 4, 4 ),
 ( 4.710628272208039924, 4.725173297074450218 ),
 .UNSPECIFIED. ) 
 CURVE ( )  GEOMETRIC_REPRESENTATION_ITEM ( )  RATIONAL_B_SPLINE_CURVE ( ( 1.000000000000000000, 0.9999823702653387603, 0.9999823702653387603, 1.000000000000000000 ) ) 
 REPRESENTATION_ITEM ( '' )  );
#98129 = CARTESIAN_POINT ( 'NONE',  ( -4.625693903144999730, 1517.042661899400173, 206.8353996064669786 ) ) ;
#98130 = ORIENTED_EDGE ( 'NONE', *, *, #31043, .F. ) ;
#98131 = CARTESIAN_POINT ( 'NONE',  ( 34.82393780566600583, 1440.913060387330006, 260.5799695211790095 ) ) ;
#98132 = EDGE_CURVE ( 'NONE', #61894, #44756, #60450, .T. ) ;
#98133 = CARTESIAN_POINT ( 'NONE',  ( -0.0002195400984297455574, 1452.178648969947972, 153.8655588343418117 ) ) ;
#98134 = ORIENTED_EDGE ( 'NONE', *, *, #31550, .T. ) ;
#98135 = CARTESIAN_POINT ( 'NONE',  ( -0.3153013721334770314, 1450.902049820790126, 181.2539182818010204 ) ) ;
#98136 = CARTESIAN_POINT ( 'NONE',  ( -15.37044282969999998, 1410.822167989630088, 190.9607351025979938 ) ) ;
#98137 = CARTESIAN_POINT ( 'NONE',  ( -108.7912805756727721, 1383.917190576337134, 311.1259201896712057 ) ) ;
#98138 = CARTESIAN_POINT ( 'NONE',  ( -24.41227777330000137, 1441.083062867809986, 212.0377087122379862 ) ) ;
#98139 = CARTESIAN_POINT ( 'NONE',  ( -5.033671048615249610, 1434.259900860620064, 217.3302329488490159 ) ) ;
#98140 = EDGE_CURVE ( 'NONE', #55469, #89451, #73188, .T. ) ;
#98141 = CARTESIAN_POINT ( 'NONE',  ( -21.39772323737049931, 1509.704958956720020, 229.7894127843639751 ) ) ;
#98142 = CARTESIAN_POINT ( 'NONE',  ( -3.666695921210000098, 1509.114858860330060, 179.5219325993979851 ) ) ;
#98143 = CARTESIAN_POINT ( 'NONE',  ( -13.50138217389999973, 1434.968982414120092, 147.1506466749980007 ) ) ;
#98144 = CARTESIAN_POINT ( 'NONE',  ( -21.41758936356537646, 1524.330813522192102, 184.2067724269699056 ) ) ;
#98146 = DIRECTION ( 'NONE',  ( -1.058776845917449781E-11, -0.4875922911319906516, 0.8730714504716415858 ) ) ;
#98145 = CARTESIAN_POINT ( 'NONE',  ( 10.02061939940000102, 1462.780975112430042, 234.0615248113979874 ) ) ;
#98147 = AXIS2_PLACEMENT_3D ( 'NONE', #12161, #88876, #98368 ) ;
#98148 = CARTESIAN_POINT ( 'NONE',  ( -5.777745433405000242, 1516.908489800550115, 215.6797558528670038 ) ) ;
#98149 = VECTOR ( 'NONE', #86179, 1000.000000000000000 ) ;
#98150 = B_SPLINE_CURVE_WITH_KNOTS ( 'NONE', 3,
 ( #90611, #6063, #99554, #64338, #98461, #106855 ),
 .UNSPECIFIED., .F., .F.,
 ( 4, 2, 4 ),
 ( 0.000000000000000000, 0.5000000000000000000, 1.000000000000000000 ),
 .UNSPECIFIED. ) ;
#98151 = CARTESIAN_POINT ( 'NONE',  ( -2.038646110889678287, 1525.960063244516959, 241.1857569150893994 ) ) ;
#98152 = CARTESIAN_POINT ( 'NONE',  ( -0.1363338795402929959, 1507.779362083510023, 180.7572018573229968 ) ) ;
#98153 = CIRCLE ( 'NONE', #33721, 1.000000000000005551 ) ;
#98154 = CARTESIAN_POINT ( 'NONE',  ( 19.14623459136682726, 1443.795870015896298, 213.6165435391197889 ) ) ;
#98155 = CARTESIAN_POINT ( 'NONE',  ( -7.710610441124999603, 1516.594591938570147, 212.5759658869370128 ) ) ;
#98156 = CARTESIAN_POINT ( 'NONE',  ( -21.25073931209999856, 1488.812149333029993, 209.2107079651389938 ) ) ;
#98157 = CARTESIAN_POINT ( 'NONE',  ( 5.745121365829383819, 1452.240402759911149, 190.7895842241696300 ) ) ;
#98159 = ORIENTED_EDGE ( 'NONE', *, *, #87030, .T. ) ;
#98158 = CARTESIAN_POINT ( 'NONE',  ( -109.9987473170000101, 1386.781127266330031, 297.3270903142590100 ) ) ;
#98160 = CARTESIAN_POINT ( 'NONE',  ( -8.156690520060001504, 1384.906090458550125, 199.6468865885190098 ) ) ;
#98161 = CARTESIAN_POINT ( 'NONE',  ( 24.59498549390000122, 1442.535575187109998, 213.3385281511980054 ) ) ;
#98162 = EDGE_CURVE ( 'NONE', #59669, #20723, #83881, .T. ) ;
#98163 = CARTESIAN_POINT ( 'NONE',  ( 29.74444329484895988, 1526.348417187218956, 217.2213265034476137 ) ) ;
#98164 = CARTESIAN_POINT ( 'NONE',  ( -14.48519478120000059, 1416.181292573540304, 203.8595931902989946 ) ) ;
#98165 = CARTESIAN_POINT ( 'NONE',  ( 2.671395959200000281, 1410.370854059430030, 231.6673943366980097 ) ) ;
#98166 = ADVANCED_FACE ( 'NONE', ( #108407 ), #62692, .F. ) ;
#98167 = CARTESIAN_POINT ( 'NONE',  ( -20.52383102562189876, 1473.184607215510141, 209.4975910873509974 ) ) ;
#98168 = DIRECTION ( 'NONE',  ( -0.7414773880254679206, 0.000000000000000000, 0.6709778558543715299 ) ) ;
#98169 = ADVANCED_FACE ( 'NONE', ( #9803 ), #94918, .T. ) ;
#98171 = CARTESIAN_POINT ( 'NONE',  ( 5.364000998215719740, 1424.961930034630086, 151.4178908013030309 ) ) ;
#98170 = CARTESIAN_POINT ( 'NONE',  ( -23.57099603410000199, 1444.794699592119969, 214.9951603828779980 ) ) ;
#98172 = CARTESIAN_POINT ( 'NONE',  ( -1.735729300940000108, 1484.732890180429877, 182.7347388233980041 ) ) ;
#98173 = AXIS2_PLACEMENT_3D ( 'NONE', #100591, #14375, #91096 ) ;
#98174 = ORIENTED_EDGE ( 'NONE', *, *, #76825, .T. ) ;
#98175 = CARTESIAN_POINT ( 'NONE',  ( 1.120543697654999837, 1517.073005577650065, 205.0775260448770041 ) ) ;
#98176 = CARTESIAN_POINT ( 'NONE',  ( 0.8897778044439998979, 1405.723157296330101, 267.8536995184980469 ) ) ;
#98177 = DIRECTION ( 'NONE',  ( -1.000000000000000000, 0.000000000000000000, 0.000000000000000000 ) ) ;
#98178 = EDGE_CURVE ( 'NONE', #42283, #43923, #76496, .T. ) ;
#98179 = CARTESIAN_POINT ( 'NONE',  ( 20.62267221016178453, 1427.503558244864962, 220.3768387070393260 ) ) ;
#98180 = CARTESIAN_POINT ( 'NONE',  ( -6.372167638625000130, 1511.069621805459974, 201.7253008890070021 ) ) ;
#98181 = CARTESIAN_POINT ( 'NONE',  ( 11.60004869893070278, 1424.990909871714166, 137.7500050950981176 ) ) ;
#98182 = B_SPLINE_CURVE_WITH_KNOTS ( 'NONE', 3,
 ( #6038, #108498, #15513, #48050 ),
 .UNSPECIFIED., .F., .F.,
 ( 4, 4 ),
 ( 0.000000000000000000, 1.000000000000000000 ),
 .UNSPECIFIED. ) ;
#98183 = DIRECTION ( 'NONE',  ( -0.8775825618903726477, 1.203706215242023366E-32, -0.4794255386042032829 ) ) ;
#98184 = CARTESIAN_POINT ( 'NONE',  ( -5.208772481359999595, 1458.757019672090109, 218.5248626948989852 ) ) ;
#98185 = CARTESIAN_POINT ( 'NONE',  ( -3.448830483803564828, 1518.913060387330006, 175.1594891075192209 ) ) ;
#98186 = CARTESIAN_POINT ( 'NONE',  ( 0.8745088156686119385, 1450.882521866549951, 155.0623987374809758 ) ) ;
#98187 = DIRECTION ( 'NONE',  ( 5.980589973904019347E-17, -1.000000000000000000, 1.736889445713099699E-16 ) ) ;
#98188 = CARTESIAN_POINT ( 'NONE',  ( 17.27558691658489920, 1507.606285602530079, 193.9884222186300065 ) ) ;
#98189 = CARTESIAN_POINT ( 'NONE',  ( -26.42714720800000094, 1440.913060387330006, 243.9198229517980110 ) ) ;
#98190 = EDGE_CURVE ( 'NONE', #19628, #69349, #15634, .T. ) ;
#98191 = PLANE ( 'NONE',  #28700 ) ;
#98192 = CARTESIAN_POINT ( 'NONE',  ( 3.653351625370000022, 1441.538476220570146, 168.7225134348979907 ) ) ;
#98193 = CARTESIAN_POINT ( 'NONE',  ( -0.1081014814999999990, 1476.109324709130078, 267.8540375961979407 ) ) ;
#98194 = CARTESIAN_POINT ( 'NONE',  ( -30.93305835920000035, 1451.832845973630128, 134.8030507067980182 ) ) ;
#98195 = CARTESIAN_POINT ( 'NONE',  ( -19.87223104929999806, 1484.291808912129909, 191.2808552885979907 ) ) ;
#98196 = ADVANCED_FACE ( 'NONE', ( #50706 ), #10351, .T. ) ;
#98197 = DIRECTION ( 'NONE',  ( -0.5450600352769339185, 0.8383970168982638471, 0.000000000000000000 ) ) ;
#98198 = CARTESIAN_POINT ( 'NONE',  ( -29.65001300571809750, 1384.829734561930081, 227.6949194770519966 ) ) ;
#98199 = AXIS2_PLACEMENT_3D ( 'NONE', #54656, #62515, #104473 ) ;
#98200 = FACE_OUTER_BOUND ( 'NONE', #51906, .T. ) ;
#98201 = B_SPLINE_SURFACE_WITH_KNOTS ( 'NONE', 5, 5, ( 
 ( #105519, #60781, #70295, #10907, #3082, #26584 ),
 ( #87620, #95459, #96566, #61887, #20383, #10338 ),
 ( #44511, #86495, #865, #94905, #78658, #28808 ),
 ( #2532, #62441, #79223, #54585, #45081, #1401 ),
 ( #11461, #78098, #69171, #1973, #61339, #45636 ),
 ( #97114, #19272, #103854, #96003, #19838, #88721 ),
 ( #71403, #69736, #36110, #54043, #104960, #53477 ),
 ( #36653, #46184, #104407, #12003, #27153, #9789 ),
 ( #103277, #70850, #18180, #52375, #34990, #28249 ) ),
 .UNSPECIFIED., .F., .F., .F.,
 ( 6, 3, 6 ),
 ( 6, 6 ),
 ( 0.7655572723440000615, 2.316155491860000026, 3.835724788559999876 ),
 ( 0.000000000000000000, 1.000000000000000000 ),
 .UNSPECIFIED. ) ;
#98202 = CARTESIAN_POINT ( 'NONE',  ( -105.8429516820000060, 1379.429574992919925, 301.1876983431590133 ) ) ;
#98203 = CARTESIAN_POINT ( 'NONE',  ( -20.53760542139809075, 1525.821544997590081, 184.7213720461156186 ) ) ;
#98204 = CARTESIAN_POINT ( 'NONE',  ( 24.02863916850529691, 1507.902931906480035, 195.9323055859989893 ) ) ;
#98206 = ADVANCED_FACE ( 'NONE', ( #331 ), #81450, .T. ) ;
#98205 = CARTESIAN_POINT ( 'NONE',  ( -10.21954854673889912, 1396.269934886460078, 213.3624866545780208 ) ) ;
#98207 = CARTESIAN_POINT ( 'NONE',  ( -15.20897926109999965, 1420.729871092930125, 227.0317324019979992 ) ) ;
#98208 = VECTOR ( 'NONE', #73027, 1000.000000000000000 ) ;
#98209 = CARTESIAN_POINT ( 'NONE',  ( -44.74160412339999482, 1437.880769410919811, 269.6947547460979990 ) ) ;
#98210 = ORIENTED_EDGE ( 'NONE', *, *, #46003, .T. ) ;
#98211 = CARTESIAN_POINT ( 'NONE',  ( -4.066802226674130161, 1436.717946482039906, 227.1798391186449919 ) ) ;
#98212 = CARTESIAN_POINT ( 'NONE',  ( 2.113412023180000432, 1409.489867608229815, 231.6724619568979904 ) ) ;
#98213 = CARTESIAN_POINT ( 'NONE',  ( -18.66420869458026388, 1526.382868172863937, 232.7837831374280881 ) ) ;
#98215 = CARTESIAN_POINT ( 'NONE',  ( -12.93225142166500063, 1513.362623229679912, 192.2350631226669861 ) ) ;
#98214 = CARTESIAN_POINT ( 'NONE',  ( 11.31574024959999925, 1425.558402394630093, 135.9181065939980044 ) ) ;
#98216 = DIRECTION ( 'NONE',  ( 0.000000000000000000, 1.000000000000000000, 0.000000000000000000 ) ) ;
#98217 = CARTESIAN_POINT ( 'NONE',  ( -9.972208786350000409, 1449.536236232390138, 205.8362451147190200 ) ) ;
#98218 = CARTESIAN_POINT ( 'NONE',  ( 3.452917022905000355, 1517.089216728169959, 202.1725802860869976 ) ) ;
#98219 = CARTESIAN_POINT ( 'NONE',  ( 7.445779770949999765, 1426.630704572389732, 212.5192353855690044 ) ) ;
#98220 = CARTESIAN_POINT ( 'NONE',  ( -7.276969490589999978, 1429.103926496630038, 148.8100812095979961 ) ) ;
#98221 = CARTESIAN_POINT ( 'NONE',  ( 5.784760235850000321, 1509.027726486529900, 180.8299671665979815 ) ) ;
#98222 = LINE ( 'NONE', #12023, #18529 ) ;
#98223 = CARTESIAN_POINT ( 'NONE',  ( -75.18978754212498927, 1377.263627487500116, 294.2967627425929891 ) ) ;
#98224 = CARTESIAN_POINT ( 'NONE',  ( 6.358435812117720687, 1368.427897723196111, 210.6218459616987957 ) ) ;
#98226 = VERTEX_POINT ( 'NONE', #31008 ) ;
#98225 = CARTESIAN_POINT ( 'NONE',  ( 4.987078422726499483, 1508.551704408389924, 205.6342535031670025 ) ) ;
#98227 = ORIENTED_EDGE ( 'NONE', *, *, #94158, .F. ) ;
#98228 = CARTESIAN_POINT ( 'NONE',  ( -6.240887352569999713, 1397.787773555530066, 197.7178371984979890 ) ) ;
#98229 = AXIS2_PLACEMENT_3D ( 'NONE', #98618, #4576, #83885 ) ;
#98230 = CARTESIAN_POINT ( 'NONE',  ( -113.4000000000000057, 1379.013060387289897, 304.2218459572590064 ) ) ;
#98231 = CARTESIAN_POINT ( 'NONE',  ( 1.626544742530000143, 1508.996462000230167, 238.7123361027979911 ) ) ;
#98232 = CARTESIAN_POINT ( 'NONE',  ( -13.48183417829717712, 1444.195713017638354, 169.3584165285456606 ) ) ;
#98233 = CARTESIAN_POINT ( 'NONE',  ( 14.59882275810000074, 1475.513060387329915, 225.1032622602980098 ) ) ;
#98234 = CARTESIAN_POINT ( 'NONE',  ( -7.594039287445000674, 1512.142919181319940, 211.3515775794370199 ) ) ;
#98236 = CARTESIAN_POINT ( 'NONE',  ( -1.357402501670849970, 1410.996727195599988, 185.5758023988580021 ) ) ;
#98235 = CARTESIAN_POINT ( 'NONE',  ( -8.913847076610000641, 1384.359708517599984, 218.6448320083890167 ) ) ;
#98237 = B_SPLINE_CURVE_WITH_KNOTS ( 'NONE', 3,
 ( #77230, #11133, #34656, #26244, #69951, #27358 ),
 .UNSPECIFIED., .F., .F.,
 ( 4, 2, 4 ),
 ( 0.000000000000000000, 0.5000000000000000000, 1.000000000000000000 ),
 .UNSPECIFIED. ) ;
#98238 = CARTESIAN_POINT ( 'NONE',  ( 6.075489283959999653, 1410.296875220730044, 186.7884348254980011 ) ) ;
#98239 = CARTESIAN_POINT ( 'NONE',  ( -1.954513284677499962, 1463.646611191549937, 199.5155506679120094 ) ) ;
#98240 = CARTESIAN_POINT ( 'NONE',  ( -39.72761531382059275, 1447.484040599029868, 136.5504236487229832 ) ) ;
#98241 =( NAMED_UNIT ( * ) SI_UNIT ( $, .STERADIAN. ) SOLID_ANGLE_UNIT ( ) );
#98242 = CARTESIAN_POINT ( 'NONE',  ( 10.03865112700490059, 1396.263617810830056, 213.7795285193350026 ) ) ;
#98243 = CARTESIAN_POINT ( 'NONE',  ( -27.31524396653970044, 1439.464577282379878, 137.0827076382539929 ) ) ;
#98244 = CARTESIAN_POINT ( 'NONE',  ( 11.53548580120000011, 1429.271495510729892, 150.4873605658980011 ) ) ;
#98245 = CARTESIAN_POINT ( 'NONE',  ( -18.90950359435113270, 1416.818673872099680, 208.2952427945739373 ) ) ;
#98246 = EDGE_LOOP ( 'NONE', ( #22729, #13522, #36114, #30570 ) ) ;
#98247 = FACE_OUTER_BOUND ( 'NONE', #73986, .T. ) ;
#98248 = CARTESIAN_POINT ( 'NONE',  ( 21.26060865160083679, 1525.055402519434438, 233.8824188859621813 ) ) ;
#98249 = VERTEX_POINT ( 'NONE', #84163 ) ;
#98250 = ORIENTED_EDGE ( 'NONE', *, *, #76798, .F. ) ;
#98251 = CARTESIAN_POINT ( 'NONE',  ( -19.07245837269699962, 1478.089605352000035, 228.2662948790070061 ) ) ;
#98252 = CARTESIAN_POINT ( 'NONE',  ( -17.17241001986523941, 1512.187213306747481, 179.6185504016045797 ) ) ;
#98253 = VECTOR ( 'NONE', #63499, 1000.000000000000000 ) ;
#98254 = CARTESIAN_POINT ( 'NONE',  ( -14.05029935760000015, 1452.819461534730181, 195.3943816284979960 ) ) ;
#98255 = DIRECTION ( 'NONE',  ( 0.000000000000000000, 1.000000000000000000, 0.000000000000000000 ) ) ;
#98256 = CARTESIAN_POINT ( 'NONE',  ( -1.121950782074999875, 1517.123342927159911, 214.1352753262870010 ) ) ;
#98257 = CARTESIAN_POINT ( 'NONE',  ( -14.36827873795669852, 1380.307879667200041, 209.5510879081830069 ) ) ;
#98258 = ORIENTED_EDGE ( 'NONE', *, *, #13834, .F. ) ;
#98259 = CARTESIAN_POINT ( 'NONE',  ( -11.56386820771918522, 1426.103378762827333, 138.8479550929265258 ) ) ;
#98260 = CARTESIAN_POINT ( 'NONE',  ( 0.05328461806629999908, 1509.045414532929954, 179.1219818357980103 ) ) ;
#98261 = CARTESIAN_POINT ( 'NONE',  ( -44.99452937619999915, 1380.083786706710043, 231.7591686846589880 ) ) ;
#98262 = CARTESIAN_POINT ( 'NONE',  ( 15.99522875749999962, 1414.971279908829956, 214.8034238970980141 ) ) ;
#98263 = CARTESIAN_POINT ( 'NONE',  ( 2.867803626105000170, 1516.994127245590107, 204.4971090729170271 ) ) ;
#98264 = EDGE_LOOP ( 'NONE', ( #47, #95826, #49742, #106734 ) ) ;
#98265 = CIRCLE ( 'NONE', #80377, 1.999999954277511760 ) ;
#98266 = CARTESIAN_POINT ( 'NONE',  ( -12.03651488328679875, 1489.799716091139999, 211.2608063207809721 ) ) ;
#98267 = CARTESIAN_POINT ( 'NONE',  ( -38.90097543864180807, 1429.363953125564649, 269.5912681143711325 ) ) ;
#98268 = CARTESIAN_POINT ( 'NONE',  ( 6.329634364484999942, 1512.038636172079805, 217.3289309248769996 ) ) ;
#98270 = VERTEX_POINT ( 'NONE', #83611 ) ;
#98269 = CARTESIAN_POINT ( 'NONE',  ( -30.17514886432853061, 1525.712830164893376, 196.9772668248565139 ) ) ;
#98271 = CARTESIAN_POINT ( 'NONE',  ( -0.001812510741418579775, 1450.927551375689745, 181.5184721789159994 ) ) ;
#98272 = CARTESIAN_POINT ( 'NONE',  ( -32.17164623804170276, 1440.913060389470047, 244.5574100837299909 ) ) ;
#98273 = CARTESIAN_POINT ( 'NONE',  ( -25.93734973360000140, 1384.843007074499837, 224.2459728783589981 ) ) ;
#98274 = CARTESIAN_POINT ( 'NONE',  ( -0.5431522787170589561, 1465.104810438569984, 238.0938638197280000 ) ) ;
#98275 = CARTESIAN_POINT ( 'NONE',  ( 34.45372861117999719, 1422.622881628830100, 269.5160893324709832 ) ) ;
#98276 = CARTESIAN_POINT ( 'NONE',  ( -7.322709724964999722, 1516.596789218710001, 212.3828531017969965 ) ) ;
#98277 = CARTESIAN_POINT ( 'NONE',  ( -62.13174705850000379, 1379.729651049759923, 266.3263280308589742 ) ) ;
#98278 = CARTESIAN_POINT ( 'NONE',  ( 23.21876702530000358, 1409.984068931529919, 208.2209878805410028 ) ) ;
#98279 = CARTESIAN_POINT ( 'NONE',  ( 28.97303002314067655, 1526.186458717542337, 197.4313369063826542 ) ) ;
#98280 = CARTESIAN_POINT ( 'NONE',  ( 11.24070573841260057, 1426.193493941640099, 194.9955581729190044 ) ) ;
#98281 = CARTESIAN_POINT ( 'NONE',  ( -7.719450415276570610, 1516.932212683830130, 209.1299851226509929 ) ) ;
#98282 = CARTESIAN_POINT ( 'NONE',  ( 1.127928333405000094, 1516.989863902050047, 209.1117210464550169 ) ) ;
#98283 = CARTESIAN_POINT ( 'NONE',  ( -106.5645047596862156, 1391.196592043153487, 300.3916496599600237 ) ) ;
#98284 = CARTESIAN_POINT ( 'NONE',  ( -5.218238568920000375, 1417.907702606829844, 232.1391919757979849 ) ) ;
#98285 = CARTESIAN_POINT ( 'NONE',  ( -81.17851594969998530, 1384.753895121710002, 304.9599978423589732 ) ) ;
#98286 = EDGE_LOOP ( 'NONE', ( #40752, #77788, #51271, #15092 ) ) ;
#98287 = CARTESIAN_POINT ( 'NONE',  ( -26.70710024954369999, 1385.248442757040038, 224.9715981382639995 ) ) ;
#98288 = ADVANCED_FACE ( 'NONE', ( #81956 ), #47821, .F. ) ;
#98289 = VECTOR ( 'NONE', #36532, 1000.000000000000114 ) ;
#98290 = CARTESIAN_POINT ( 'NONE',  ( -4.987078426973329925, 1508.551704408389924, 206.6339106789369851 ) ) ;
#98291 = ADVANCED_FACE ( 'NONE', ( #58433 ), #66847, .T. ) ;
#98292 = CARTESIAN_POINT ( 'NONE',  ( -9.094755087212869071, 1384.939018560090062, 199.9428094726760037 ) ) ;
#98293 = CARTESIAN_POINT ( 'NONE',  ( 4.554962005479513465, 1508.731359867455467, 206.6339108206555295 ) ) ;
#98294 = CARTESIAN_POINT ( 'NONE',  ( 3.767362825309999774, 1499.438298220989964, 230.0641493129989783 ) ) ;
#98295 = CARTESIAN_POINT ( 'NONE',  ( 12.75748638139999969, 1426.660728386520077, 203.9418282069190127 ) ) ;
#98296 = CARTESIAN_POINT ( 'NONE',  ( -1.872941326106300597, 1497.922954902849369, 197.9834655647225929 ) ) ;
#98298 = CARTESIAN_POINT ( 'NONE',  ( -15.91787331746375500, 1416.014249173312919, 209.3106600495536611 ) ) ;
#98297 = CARTESIAN_POINT ( 'NONE',  ( 0.7538707352880020807, 1516.719999691880048, 216.0603247549969979 ) ) ;
#98299 = DIRECTION ( 'NONE',  ( -0.000000000000000000, -1.000000000000000000, -0.000000000000000000 ) ) ;
#98300 = CARTESIAN_POINT ( 'NONE',  ( 10.95547293380590048, 1470.846847384059856, 209.2244093452740117 ) ) ;
#98301 = ORIENTED_EDGE ( 'NONE', *, *, #65595, .T. ) ;
#98302 = CARTESIAN_POINT ( 'NONE',  ( 5.003848121975000396, 1517.005755693489846, 201.7875176594370146 ) ) ;
#98303 = LINE ( 'NONE', #29991, #109146 ) ;
#98304 = VERTEX_POINT ( 'NONE', #92561 ) ;
#98305 = AXIS2_PLACEMENT_3D ( 'NONE', #93901, #92808, #110714 ) ;
#98306 = DIRECTION ( 'NONE',  ( -0.2020439960283723635, -0.9583089376822325756, -0.2020450534589698921 ) ) ;
#98307 = CARTESIAN_POINT ( 'NONE',  ( 10.96098658911311752, 1434.305190191134670, 151.7979222656376521 ) ) ;
#98308 = CARTESIAN_POINT ( 'NONE',  ( 8.997154110830200224, 1425.027132644833046, 195.6828247586980183 ) ) ;
#98309 = CARTESIAN_POINT ( 'NONE',  ( 0.7065304258729989684, 1442.384625720290160, 219.0605242788890052 ) ) ;
#98310 = CARTESIAN_POINT ( 'NONE',  ( -26.71962680251449740, 1509.092879738190049, 201.3937371580310014 ) ) ;
#98311 = CARTESIAN_POINT ( 'NONE',  ( -2.704615531770000025, 1447.046937273400090, 168.9986710401979906 ) ) ;
#98312 = CARTESIAN_POINT ( 'NONE',  ( -20.58707213139999936, 1427.974737749530050, 223.4007331328979831 ) ) ;
#98313 = CARTESIAN_POINT ( 'NONE',  ( 8.267083892837330694, 1487.528308034231713, 202.1104332054804047 ) ) ;
#98314 = CARTESIAN_POINT ( 'NONE',  ( -105.5650123339999880, 1390.851006877979898, 302.0524783112590512 ) ) ;
#98315 = CARTESIAN_POINT ( 'NONE',  ( 17.83984130769999865, 1445.351173051870092, 190.7420059714980027 ) ) ;
#98317 = CARTESIAN_POINT ( 'NONE',  ( -18.94313757346292348, 1438.951138393643305, 210.3999238583679130 ) ) ;
#98316 = CARTESIAN_POINT ( 'NONE',  ( -106.2614451870000067, 1391.913060386500092, 302.8078771165589842 ) ) ;
#98318 = CARTESIAN_POINT ( 'NONE',  ( 2.372478608332517336, 1522.382868172863937, 243.3440112565233449 ) ) ;
#98319 = ORIENTED_EDGE ( 'NONE', *, *, #93291, .T. ) ;
#98320 = DIRECTION ( 'NONE',  ( 0.9125304618754024322, 0.000000000000000000, -0.4090087482554191078 ) ) ;
#98321 = CARTESIAN_POINT ( 'NONE',  ( -9.454311864350000150, 1508.539839826989919, 218.7120270370789967 ) ) ;
#98322 = CARTESIAN_POINT ( 'NONE',  ( 5.513435558552499671, 1509.038615934029849, 201.6090957240569992 ) ) ;
#98323 = CARTESIAN_POINT ( 'NONE',  ( 10.30449505059999815, 1426.851415982049957, 209.1702054645420219 ) ) ;
#98324 = CARTESIAN_POINT ( 'NONE',  ( -0.9796450454589999968, 1519.913060387329779, 232.6858900125980085 ) ) ;
#98325 = VECTOR ( 'NONE', #101040, 1000.000000000000000 ) ;
#98326 = CARTESIAN_POINT ( 'NONE',  ( 2.157496122451417531, 1526.189892541619429, 240.2809797488604033 ) ) ;
#98327 = CARTESIAN_POINT ( 'NONE',  ( -2.691662542991861695, 1524.776010967675575, 241.8130992650591224 ) ) ;
#98328 = CARTESIAN_POINT ( 'NONE',  ( -13.22735232723135468, 1443.148167861271531, 186.8228418827334281 ) ) ;
#98329 = B_SPLINE_SURFACE_WITH_KNOTS ( 'NONE', 5, 5, ( 
 ( #24438, #58079, #52862, #84363, #44455, #86989 ),
 ( #94842, #27099, #70241, #92212, #41809, #58626 ),
 ( #10278, #83263, #52314, #32845, #18118, #15484 ),
 ( #78037, #75966, #61284, #67586, #101692, #109031 ),
 ( #14936, #9728, #6558, #49130, #74881, #92757 ),
 ( #16035, #1917, #104348, #43893, #32314, #1345 ),
 ( #7110, #50236, #35484, #69678, #103800, #95400 ),
 ( #27641, #41265, #61827, #66497, #23885, #49680 ),
 ( #83811, #75438, #67037, #101145, #70790, #55072 ),
 ( #62377, #53411, #97606, #38784, #63487, #88666 ),
 ( #98138, #19209, #4646, #88118, #20876, #89199 ),
 ( #19783, #4112, #28746, #106015, #53984, #104903 ),
 ( #29291, #12492, #80806, #45575, #46674, #3572 ),
 ( #62951, #97062, #38236, #72420, #2476, #10851 ),
 ( #29839, #45023, #28191, #11407, #71343, #79168 ) ),
 .UNSPECIFIED., .F., .F., .F.,
 ( 6, 3, 3, 3, 6 ),
 ( 6, 6 ),
 ( 7.637039622810000594, 10.13387562650000007, 11.38229362830000113, 12.23404602909999994, 12.63071163020000043 ),
 ( 0.000000000000000000, 2.000000000000000000 ),
 .UNSPECIFIED. ) ;
#98330 = EDGE_CURVE ( 'NONE', #65500, #105896, #51774, .T. ) ;
#98331 = CARTESIAN_POINT ( 'NONE',  ( 13.39680589851269943, 1407.451641433219947, 204.6080239228549829 ) ) ;
#98332 = CARTESIAN_POINT ( 'NONE',  ( 19.12714383624729919, 1496.834757293069970, 222.0421909404099949 ) ) ;
#98333 = CARTESIAN_POINT ( 'NONE',  ( -15.46337563405010052, 1415.677402202039957, 209.5778891453549875 ) ) ;
#98334 = B_SPLINE_CURVE_WITH_KNOTS ( 'NONE', 3,
 ( #37133, #52852, #60708, #20314, #54519, #11394, #1904, #18653, #69665, #88654, #10268, #103788, #3010, #28734, #18107, #71332, #52302, #43883, #78027, #53400, #27089, #79155, #70230, #3561, #62366, #2464, #45564, #87550, #79705, #86979, #53973, #46111, #95388, #97051, #36580, #88105, #44444, #78588, #1334, #104335, #61273, #10839, #70778 ),
 .UNSPECIFIED., .F., .F.,
 ( 4, 3, 3, 3, 3, 3, 3, 3, 3, 3, 3, 3, 3, 3, 4 ),
 ( 9.042384392956980932, 10.74863236500899966, 12.79857683260340018, 14.83630879456500118, 16.53028721917180022, 18.09003653870529860, 19.51885659866059797, 19.64978585823890000, 20.88045880726579995, 22.19108762358739995, 23.57188707978410136, 25.05204642891560241, 26.81066961526140346, 28.89555248377980234, 30.20342721250000295 ),
 .UNSPECIFIED. ) ;
#98335 = CARTESIAN_POINT ( 'NONE',  ( -9.631607308150519131, 1460.301351192619904, 209.7569760522880244 ) ) ;
#98337 = EDGE_CURVE ( 'NONE', #108462, #5353, #27157, .T. ) ;
#98336 = CARTESIAN_POINT ( 'NONE',  ( 6.697438882680000205, 1428.609913361190138, 214.7541855357489737 ) ) ;
#98339 = EDGE_LOOP ( 'NONE', ( #50702, #60185, #18712, #81158 ) ) ;
#98338 = DIRECTION ( 'NONE',  ( 1.755985294532464991E-16, -1.000000000000000000, 1.338183447452830017E-16 ) ) ;
#98340 = AXIS2_PLACEMENT_3D ( 'NONE', #72769, #78979, #71139 ) ;
#98341 = CARTESIAN_POINT ( 'NONE',  ( -102.7498137299999996, 1383.762281939259992, 311.0461218402589907 ) ) ;
#98342 = CARTESIAN_POINT ( 'NONE',  ( 12.67335156995190104, 1512.240709848930010, 224.2037181255240057 ) ) ;
#98343 = EDGE_LOOP ( 'NONE', ( #62023, #71619, #4344, #26546 ) ) ;
#98344 = ORIENTED_EDGE ( 'NONE', *, *, #89185, .T. ) ;
#98345 = FACE_OUTER_BOUND ( 'NONE', #40981, .T. ) ;
#98346 = CARTESIAN_POINT ( 'NONE',  ( -109.1643701970000109, 1384.923480540200217, 297.1325780693589991 ) ) ;
#98347 = CARTESIAN_POINT ( 'NONE',  ( -9.013032691016070075, 1381.609887807723226, 200.5860147506873545 ) ) ;
#98349 = CARTESIAN_POINT ( 'NONE',  ( -15.47923624669999931, 1465.564491350429989, 248.5133305111980064 ) ) ;
#98348 = CARTESIAN_POINT ( 'NONE',  ( 32.56932958284517099, 1421.650079385355411, 269.5000704786230585 ) ) ;
#98350 = B_SPLINE_CURVE_WITH_KNOTS ( 'NONE', 5,
 ( #66804, #25295, #25850, #94170, #58389, #93607, #24740, #51638, #75196 ),
 .UNSPECIFIED., .F., .F.,
 ( 6, 3, 6 ),
 ( -11.25975508159999983, -5.782490304330000441, 0.000000000000000000 ),
 .UNSPECIFIED. ) ;
#98351 = FACE_OUTER_BOUND ( 'NONE', #97080, .T. ) ;
#98352 = CARTESIAN_POINT ( 'NONE',  ( -11.94265424589999824, 1433.497477044639936, 149.9944001463979930 ) ) ;
#98353 = CARTESIAN_POINT ( 'NONE',  ( 20.45347777980000004, 1495.695647834889996, 214.2365953844490036 ) ) ;
#98354 = CARTESIAN_POINT ( 'NONE',  ( -19.12120586389999843, 1485.993527487529946, 189.5707249904979790 ) ) ;
#98355 = CARTESIAN_POINT ( 'NONE',  ( 5.829580275110519239, 1467.124413742679963, 217.1880984370909857 ) ) ;
#98356 = CARTESIAN_POINT ( 'NONE',  ( -25.00511632820000330, 1436.574185807339973, 137.9303955387979954 ) ) ;
#98357 = CARTESIAN_POINT ( 'NONE',  ( -0.5750010241229840391, 1515.139742041519867, 213.4493321248399980 ) ) ;
#98358 = CARTESIAN_POINT ( 'NONE',  ( 1.163729664429999966E-13, 1474.175172888730003, 270.1377426887980278 ) ) ;
#98359 = DIRECTION ( 'NONE',  ( -6.162707975952100561E-15, -1.000000000000000000, -1.094450614310000083E-14 ) ) ;
#98360 = CARTESIAN_POINT ( 'NONE',  ( 3.854212611492175977, 1362.772174771310119, 209.6218459617148824 ) ) ;
#98361 = CARTESIAN_POINT ( 'NONE',  ( -11.03244314401329795, 1509.423458058530514, 237.0196150796065808 ) ) ;
#98363 = EDGE_LOOP ( 'NONE', ( #51032, #98797, #80638, #99774, #3000 ) ) ;
#98362 = CARTESIAN_POINT ( 'NONE',  ( 7.739409189424749408E-09, 1406.348277573139967, 266.2841496100420500 ) ) ;
#98364 = ORIENTED_EDGE ( 'NONE', *, *, #44079, .F. ) ;
#98365 = CARTESIAN_POINT ( 'NONE',  ( -11.86167655160669909, 1432.027010461159989, 149.9735918577489997 ) ) ;
#98366 = CARTESIAN_POINT ( 'NONE',  ( 16.47697133779999845, 1494.872252754689953, 192.9650186975990209 ) ) ;
#98367 = CARTESIAN_POINT ( 'NONE',  ( -20.61505026740000091, 1469.732609222430028, 270.3833838275979815 ) ) ;
#98368 = DIRECTION ( 'NONE',  ( -0.9455185755993178454, 0.000000000000000000, 0.3255681544571537578 ) ) ;
#98369 = DIRECTION ( 'NONE',  ( -1.000000000000000000, 0.000000000000000000, 0.000000000000000000 ) ) ;
#98370 = CARTESIAN_POINT ( 'NONE',  ( 34.59578736694340506, 1451.704956805989923, 134.6972962829659934 ) ) ;
#98371 = VECTOR ( 'NONE', #66332, 1000.000000000000000 ) ;
#98372 = CARTESIAN_POINT ( 'NONE',  ( 0.2664901603583379464, 1451.240506610500006, 182.3742570756570274 ) ) ;
#98373 = CARTESIAN_POINT ( 'NONE',  ( 3.545373040442179935, 1484.694412436259881, 220.4261202662389962 ) ) ;
#98374 = CARTESIAN_POINT ( 'NONE',  ( -15.85075050099999849, 1459.333342989330049, 230.7228811812979927 ) ) ;
#98375 = CARTESIAN_POINT ( 'NONE',  ( -5.540249615179999587, 1457.790387395490143, 216.9137936155790101 ) ) ;
#98376 = CARTESIAN_POINT ( 'NONE',  ( 9.432497968925920517, 1361.986403221846331, 207.6218459616987673 ) ) ;
#98377 = CARTESIAN_POINT ( 'NONE',  ( -37.29566738313450003, 1420.414047975189987, 266.4270220111449703 ) ) ;
#98378 = AXIS2_PLACEMENT_3D ( 'NONE', #91100, #109021, #14379 ) ;
#98379 = VERTEX_POINT ( 'NONE', #77982 ) ;
#98380 = CARTESIAN_POINT ( 'NONE',  ( -3.548032200200450070, 1505.730471142629767, 181.0364234874799934 ) ) ;
#98381 = EDGE_LOOP ( 'NONE', ( #21673, #107810, #68914 ) ) ;
#98382 = ORIENTED_EDGE ( 'NONE', *, *, #95424, .F. ) ;
#98383 = CARTESIAN_POINT ( 'NONE',  ( -0.7350232362959980836, 1516.970035769810011, 211.4194755912870107 ) ) ;
#98384 = CARTESIAN_POINT ( 'NONE',  ( -8.908008619578920317, 1447.595509318989798, 212.1355612019459898 ) ) ;
#98386 = SURFACE_SIDE_STYLE ('',( #65367 ) ) ;
#98385 = CARTESIAN_POINT ( 'NONE',  ( -2.864326125434999870, 1516.826109302209943, 211.6149197999869784 ) ) ;
#98387 = CARTESIAN_POINT ( 'NONE',  ( -15.05796970909999999, 1440.435147221739953, 189.3328455896980245 ) ) ;
#98388 = AXIS2_PLACEMENT_3D ( 'NONE', #26321, #9528, #59413 ) ;
#98389 = CARTESIAN_POINT ( 'NONE',  ( -18.50064172359999759, 1416.067629290630066, 208.4803912601460070 ) ) ;
#98390 = VERTEX_POINT ( 'NONE', #102062 ) ;
#98391 = CARTESIAN_POINT ( 'NONE',  ( -26.03637496420000019, 1436.679440559009890, 136.9231354318980323 ) ) ;
#98392 = CARTESIAN_POINT ( 'NONE',  ( -7.330554171554999776, 1516.857992118400034, 201.7925428541169879 ) ) ;
#98393 = CARTESIAN_POINT ( 'NONE',  ( 10.10526316670000035, 1471.402127257289976, 212.2219417807989998 ) ) ;
#98394 = CARTESIAN_POINT ( 'NONE',  ( -13.08406847753679969, 1384.517833128000120, 200.3646909337909960 ) ) ;
#98395 = CARTESIAN_POINT ( 'NONE',  ( 0.06979916920619999576, 1408.910622946630156, 194.4360052257980271 ) ) ;
#98396 = CARTESIAN_POINT ( 'NONE',  ( -3.487592467065220081, 1508.551704408389924, 204.1347675093749956 ) ) ;
#98397 = CARTESIAN_POINT ( 'NONE',  ( -1.195258643130000076, 1396.139237108130146, 197.1899914320979690 ) ) ;
#98399 = VERTEX_POINT ( 'NONE', #42178 ) ;
#98398 = CARTESIAN_POINT ( 'NONE',  ( -8.791275945972083505, 1364.761074005578166, 210.6218459617142003 ) ) ;
#98400 = ORIENTED_EDGE ( 'NONE', *, *, #17950, .F. ) ;
#98401 = B_SPLINE_CURVE_WITH_KNOTS ( 'NONE', 3,
 ( #33333, #25477, #59670, #93780, #26593, #60222, #17618, #67528, #35000, #101628, #69180, #24917, #85961, #59127, #71415, #97122, #79785, #106611, #78666, #89265, #45091, #4171, #98211, #11470, #20939 ),
 .UNSPECIFIED., .F., .F.,
 ( 4, 3, 3, 3, 3, 3, 3, 3, 4 ),
 ( -3.448512466139999955, -2.538571452078679958, -1.628606578387550075, -0.7191125574035575063, -0.01266682060199997295, 0.9054669040022687021, 1.822853446759360008, 2.738681977611620244, 3.448512466139999955 ),
 .UNSPECIFIED. ) ;
#98402 = CARTESIAN_POINT ( 'NONE',  ( 45.49168718497458741, 1443.644333717846393, 268.9787543363217992 ) ) ;
#98403 = CARTESIAN_POINT ( 'NONE',  ( -2.695307629501230373, 1424.941390411620205, 191.3270642277350078 ) ) ;
#98404 = CARTESIAN_POINT ( 'NONE',  ( -14.30919783444790028, 1436.257022624779893, 150.0511997702159874 ) ) ;
#98405 = AXIS2_PLACEMENT_3D ( 'NONE', #70851, #97660, #104961 ) ;
#98406 = CARTESIAN_POINT ( 'NONE',  ( -0.5182872000439999738, 1486.281073925030114, 181.7525819957979820 ) ) ;
#98407 = CARTESIAN_POINT ( 'NONE',  ( 3.269984781304999810, 1516.999105586269934, 210.8242519552970009 ) ) ;
#98408 = CARTESIAN_POINT ( 'NONE',  ( -17.52641558221370133, 1415.034069327669840, 207.5652963658199894 ) ) ;
#98409 = DIRECTION ( 'NONE',  ( 0.9993908259982007269, 0.03489950309194383288, 3.993205903601619117E-05 ) ) ;
#98410 = CARTESIAN_POINT ( 'NONE',  ( 22.51380231507019758, 1471.707018205450140, 268.8517371266460145 ) ) ;
#98411 = CARTESIAN_POINT ( 'NONE',  ( 11.65314573679999910, 1415.128105759529944, 222.6874287277979931 ) ) ;
#98412 = CARTESIAN_POINT ( 'NONE',  ( 7.563688191785000292, 1510.983859056260144, 206.1910078925270113 ) ) ;
#98413 = CARTESIAN_POINT ( 'NONE',  ( -2.881222795715000284, 1516.891731298979948, 206.6444723262370076 ) ) ;
#98414 = EDGE_LOOP ( 'NONE', ( #44792, #29271, #108623, #103905, #105180 ) ) ;
#98415 = CARTESIAN_POINT ( 'NONE',  ( -7.709151609294999652, 1516.538881398679905, 211.6739720840869836 ) ) ;
#98416 = CARTESIAN_POINT ( 'NONE',  ( -2.935376417616495370, 1516.592453102976606, 202.2105020858446096 ) ) ;
#98417 = ORIENTED_EDGE ( 'NONE', *, *, #26966, .T. ) ;
#98419 = VECTOR ( 'NONE', #45327, 1000.000000000000114 ) ;
#98418 = CARTESIAN_POINT ( 'NONE',  ( 0.9734891864660385474, 1457.809612541702109, 228.9324353732729094 ) ) ;
#98420 = CARTESIAN_POINT ( 'NONE',  ( -2.887264227133756744, 1368.159418877311282, 210.2902280133655211 ) ) ;
#98421 = CARTESIAN_POINT ( 'NONE',  ( -4.103692849526556330, 1440.174184918509354, 185.4089468763897628 ) ) ;
#98422 = CARTESIAN_POINT ( 'NONE',  ( -14.43714569989999852, 1417.316660727240105, 204.8390003888189881 ) ) ;
#98423 = CARTESIAN_POINT ( 'NONE',  ( 20.52148985240000201, 1409.793966177029915, 200.0941763215180060 ) ) ;
#98424 = CARTESIAN_POINT ( 'NONE',  ( 28.08752589700002744, 1445.052233488288948, 160.7519773376980936 ) ) ;
#98425 = CARTESIAN_POINT ( 'NONE',  ( -26.00842845082479826, 1468.897115946460190, 210.5448491430259992 ) ) ;
#98426 = CARTESIAN_POINT ( 'NONE',  ( 32.38114538885250226, 1523.604703353109699, 202.1233279672528624 ) ) ;
#98427 = DIRECTION ( 'NONE',  ( -1.000000000000000000, 0.000000000000000000, 0.000000000000000000 ) ) ;
#98428 = CARTESIAN_POINT ( 'NONE',  ( 21.70224022220987337, 1453.376422913917168, 220.8111189556726970 ) ) ;
#98429 = CARTESIAN_POINT ( 'NONE',  ( 2.500000000000000000, 1439.624617072440060, 168.6282387789959785 ) ) ;
#98430 = CARTESIAN_POINT ( 'NONE',  ( -1.706797824074999914, 1517.164987839469859, 214.9112406324369999 ) ) ;
#98431 = EDGE_LOOP ( 'NONE', ( #110825, #35564, #69515, #95690, #68308 ) ) ;
#98432 = CARTESIAN_POINT ( 'NONE',  ( 7.711638320313230821, 1516.633846517499933, 208.0028055230160078 ) ) ;
#98433 = FACE_OUTER_BOUND ( 'NONE', #84521, .T. ) ;
#98434 = CARTESIAN_POINT ( 'NONE',  ( -18.24633262864339756, 1416.842625005220043, 208.9597599549800009 ) ) ;
#98435 = ADVANCED_FACE ( 'NONE', ( #58988 ), #27036, .F. ) ;
#98436 = CARTESIAN_POINT ( 'NONE',  ( -11.29523551895650080, 1425.738185592099853, 112.3427247082750000 ) ) ;
#98437 =( BOUNDED_CURVE ( )  B_SPLINE_CURVE ( 3, ( #50570, #35972, #8542, #52233 ),
 .UNSPECIFIED., .F., .T. ) 
 B_SPLINE_CURVE_WITH_KNOTS ( ( 4, 4 ),
 ( 4.573263261563710103, 4.591728602243319912 ),
 .UNSPECIFIED. ) 
 CURVE ( )  GEOMETRIC_REPRESENTATION_ITEM ( )  RATIONAL_B_SPLINE_CURVE ( ( 1.000000000000000000, 0.9999715861346381018, 0.9999715861346381018, 1.000000000000000000 ) ) 
 REPRESENTATION_ITEM ( '' )  );
#98438 = CARTESIAN_POINT ( 'NONE',  ( -36.32856917184830081, 1449.884418639690011, 136.2560105224960125 ) ) ;
#98439 = CARTESIAN_POINT ( 'NONE',  ( 11.60004869885203682, 1425.927668451900445, 137.5659639343614913 ) ) ;
#98440 = DIRECTION ( 'NONE',  ( 5.980589973904019347E-17, -1.000000000000000000, 1.736889445713099699E-16 ) ) ;
#98441 = VECTOR ( 'NONE', #39616, 1000.000000000000114 ) ;
#98442 = CARTESIAN_POINT ( 'NONE',  ( -2.500000000000000000, 1432.302173844710069, 157.4936352153980010 ) ) ;
#98443 = CARTESIAN_POINT ( 'NONE',  ( 0.8123333382153080651, 1456.028120524400038, 198.5934206245379983 ) ) ;
#98444 = ADVANCED_FACE ( 'NONE', ( #76889 ), #98446, .F. ) ;
#98445 = CARTESIAN_POINT ( 'NONE',  ( -1.490542806272469933, 1474.158742738300134, 270.1372991191880146 ) ) ;
#98446 = B_SPLINE_SURFACE_WITH_KNOTS ( 'NONE', 5, 5, ( 
 ( #34871, #68501, #34322, #95339, #25345, #84711 ),
 ( #59538, #76328, #24786, #10222, #8011, #198 ),
 ( #77439, #69059, #33756, #78542, #85827, #52800 ),
 ( #85261, #1856, #60656, #67953, #35428, #94214 ),
 ( #8558, #52252, #102599, #18600, #9124, #25900 ),
 ( #17489, #43291, #43836, #740, #103160, #94780 ) ),
 .UNSPECIFIED., .F., .F., .F.,
 ( 6, 6 ),
 ( 6, 6 ),
 ( 8.933709406209999315, 11.91636762130000093 ),
 ( 0.000000000000000000, 1.455044450599999983 ),
 .UNSPECIFIED. ) ;
#98447 = CARTESIAN_POINT ( 'NONE',  ( 29.56664643221430211, 1440.913060386659936, 236.9318484411240036 ) ) ;
#98448 = DIRECTION ( 'NONE',  ( -0.6736849260863839728, 0.000000000000000000, 0.7390186874254150995 ) ) ;
#98449 = CARTESIAN_POINT ( 'NONE',  ( 8.165692104976699284, 1498.965027995250011, 200.4303008461249931 ) ) ;
#98450 = VERTEX_POINT ( 'NONE', #69615 ) ;
#98451 = CARTESIAN_POINT ( 'NONE',  ( 10.65095720820150049, 1480.263004433129936, 208.4908651385430005 ) ) ;
#98452 = DIRECTION ( 'NONE',  ( 2.368020459168575969E-05, 1.033907832572708405E-06, -0.9999999997190894829 ) ) ;
#98453 = CARTESIAN_POINT ( 'NONE',  ( -4.222176722049999498, 1443.314582379889771, 199.9747765569790090 ) ) ;
#98454 = CARTESIAN_POINT ( 'NONE',  ( 2.127397458329999935, 1490.907483387130014, 235.4495606871979874 ) ) ;
#98455 = CIRCLE ( 'NONE', #100229, 2.000000000000003109 ) ;
#98456 = CARTESIAN_POINT ( 'NONE',  ( 4.500000000000000000, 1439.615672362369878, 182.7715282920979973 ) ) ;
#98457 = CARTESIAN_POINT ( 'NONE',  ( -17.84338787571961049, 1523.382868172864164, 180.3600277896300383 ) ) ;
#98458 = CARTESIAN_POINT ( 'NONE',  ( -40.29337211549999864, 1383.827701909899815, 242.2979617791790190 ) ) ;
#98459 = CARTESIAN_POINT ( 'NONE',  ( -2.472546487080370170, 1422.360492482099744, 192.6709265187130029 ) ) ;
#98460 = CARTESIAN_POINT ( 'NONE',  ( 5.800620439598599631, 1423.415524905749862, 91.01561172700489522 ) ) ;
#98461 = CARTESIAN_POINT ( 'NONE',  ( -6.141424781052139181, 1511.655929346179391, 200.3276031877419427 ) ) ;
#98462 = CARTESIAN_POINT ( 'NONE',  ( 1.657465492969999898, 1465.141359081529799, 235.6472656048979957 ) ) ;
#98464 = ORIENTED_EDGE ( 'NONE', *, *, #67162, .T. ) ;
#98463 = CARTESIAN_POINT ( 'NONE',  ( 10.56407631929999980, 1452.658139941989930, 209.7432180256290053 ) ) ;
#98465 = CARTESIAN_POINT ( 'NONE',  ( -1.213558767919999948, 1450.835243711869907, 182.4750632466980278 ) ) ;
#98466 = CARTESIAN_POINT ( 'NONE',  ( -18.10779123049999839, 1380.896120499720155, 217.9240877703190051 ) ) ;
#98467 = CARTESIAN_POINT ( 'NONE',  ( -3.501244980050000066, 1476.186593646489882, 199.3843432763690089 ) ) ;
#98469 = ORIENTED_EDGE ( 'NONE', *, *, #35983, .T. ) ;
#98468 = CARTESIAN_POINT ( 'NONE',  ( -17.19251027932519804, 1415.089118586289942, 208.5383158172610081 ) ) ;
#98470 = CARTESIAN_POINT ( 'NONE',  ( 18.99432649145670027, 1459.501291662010090, 220.3864114681610147 ) ) ;
#98471 = EDGE_LOOP ( 'NONE', ( #12310, #102861 ) ) ;
#98472 = AXIS2_PLACEMENT_3D ( 'NONE', #38184, #28133, #2419 ) ;
#98473 = CARTESIAN_POINT ( 'NONE',  ( -10.52351523589999971, 1390.477550767929870, 215.6246750091789863 ) ) ;
#98474 = CARTESIAN_POINT ( 'NONE',  ( -0.5750466322259990548, 1484.101157922590119, 201.2237824415789760 ) ) ;
#98475 = CARTESIAN_POINT ( 'NONE',  ( -10.32785587848439945, 1461.601613029019973, 211.2212836788939967 ) ) ;
#98476 = DIRECTION ( 'NONE',  ( 2.775557561562888827E-14, 0.000000000000000000, 1.000000000000000000 ) ) ;
#98477 = CARTESIAN_POINT ( 'NONE',  ( 4.789673499540000101, 1465.867933640490037, 219.0700355186390027 ) ) ;
#98478 = AXIS2_PLACEMENT_3D ( 'NONE', #30685, #63764, #55359 ) ;
#98479 = CARTESIAN_POINT ( 'NONE',  ( -113.4000000000000057, 1309.713060387289943, 304.2218459572590064 ) ) ;
#98480 = FACE_OUTER_BOUND ( 'NONE', #39298, .T. ) ;
#98481 = CARTESIAN_POINT ( 'NONE',  ( -7.966157931650249324, 1384.915561067150065, 199.4892992289589984 ) ) ;
#98482 = DIRECTION ( 'NONE',  ( -1.755985294532469921E-16, 1.000000000000000000, -1.338183447452831989E-16 ) ) ;
#98483 = CARTESIAN_POINT ( 'NONE',  ( -18.31584160739999945, 1437.055458693600031, 191.8806195066979967 ) ) ;
#98484 = CARTESIAN_POINT ( 'NONE',  ( 11.76883256610000039, 1432.286229124249985, 150.8119424997980218 ) ) ;
#98485 = CARTESIAN_POINT ( 'NONE',  ( 1.332267629549999902E-15, 1413.913060387330006, 209.1218459616989946 ) ) ;
#98486 = ORIENTED_EDGE ( 'NONE', *, *, #89234, .T. ) ;
#98487 = AXIS2_PLACEMENT_3D ( 'NONE', #41884, #76043, #68222 ) ;
#98488 = ORIENTED_EDGE ( 'NONE', *, *, #5665, .T. ) ;
#98489 = CARTESIAN_POINT ( 'NONE',  ( 18.10570579381780476, 1525.713797967456458, 238.1210409130211474 ) ) ;
#98490 = CARTESIAN_POINT ( 'NONE',  ( 17.93302110244420433, 1458.863172048540036, 228.0434772327210169 ) ) ;
#98491 = CARTESIAN_POINT ( 'NONE',  ( -12.78614179230000047, 1434.663150159289899, 149.2928482040979929 ) ) ;
#98492 = TOROIDAL_SURFACE ( 'NONE', #21589, 2.000000000000000000, 1.000000000000000000 ) ;
#98493 = DIRECTION ( 'NONE',  ( -0.7414773880254664773, 0.000000000000000000, 0.6709778558543730842 ) ) ;
#98494 = CARTESIAN_POINT ( 'NONE',  ( -20.11105721185739981, 1492.027588246229925, 190.8484634630870005 ) ) ;
#98495 = CARTESIAN_POINT ( 'NONE',  ( 7.722580314247720068, 1517.051704408590012, 209.5565402419049974 ) ) ;
#98496 = CARTESIAN_POINT ( 'NONE',  ( -109.0318845759999959, 1385.766567570789903, 311.1758076612590003 ) ) ;
#98497 = CARTESIAN_POINT ( 'NONE',  ( -0.1951232425329999798, 1486.506925057930175, 181.7766938669979879 ) ) ;
#98498 = CARTESIAN_POINT ( 'NONE',  ( -11.32094776019573956, 1366.953380474498545, 208.3718459617010978 ) ) ;
#98499 = CARTESIAN_POINT ( 'NONE',  ( -26.73069746017884185, 1436.754254116213588, 136.7839827981474912 ) ) ;
#98500 = CARTESIAN_POINT ( 'NONE',  ( -19.44259940939999964, 1468.969836806830017, 192.7096998052980155 ) ) ;
#98501 = CARTESIAN_POINT ( 'NONE',  ( 2.476170596904999854, 1516.819260244609950, 207.4047612206870213 ) ) ;
#98502 = CARTESIAN_POINT ( 'NONE',  ( -8.634542021964680458, 1448.697323880249996, 212.1401996392050080 ) ) ;
#98503 = CARTESIAN_POINT ( 'NONE',  ( 4.130957310362520118, 1408.874543812650018, 222.6735585427379931 ) ) ;
#98504 = CARTESIAN_POINT ( 'NONE',  ( -13.43623098084330003, 1434.935581815499745, 148.9651777270820219 ) ) ;
#98505 = CARTESIAN_POINT ( 'NONE',  ( -8.582794586710001283, 1385.145244622950031, 218.6615206947490151 ) ) ;
#98506 = CARTESIAN_POINT ( 'NONE',  ( 11.73563908010000034, 1425.610159190430068, 144.1657657165980027 ) ) ;
#98507 = CARTESIAN_POINT ( 'NONE',  ( 7.146076167249690414, 1424.928856607450143, 212.9496858538670097 ) ) ;
#98508 = CARTESIAN_POINT ( 'NONE',  ( -5.175842961363289696, 1496.203461988439813, 202.5536918307219878 ) ) ;
#98509 = ORIENTED_EDGE ( 'NONE', *, *, #104907, .F. ) ;
#98510 = CARTESIAN_POINT ( 'NONE',  ( 21.00608537029999923, 1420.811742010329908, 244.4374624613979847 ) ) ;
#98511 = CARTESIAN_POINT ( 'NONE',  ( -1.188407889236729575, 1416.818673806566949, 228.1243924589994947 ) ) ;
#98513 = CARTESIAN_POINT ( 'NONE',  ( -16.81341251239999934, 1409.500197688229946, 195.2116452731980019 ) ) ;
#98512 = CARTESIAN_POINT ( 'NONE',  ( -1.534027278920000015, 1494.208487614430169, 181.3504807686979916 ) ) ;
#98514 = ADVANCED_FACE ( 'NONE', ( #86378 ), #9664, .T. ) ;
#98515 = CARTESIAN_POINT ( 'NONE',  ( -0.5987183604784179769, 1507.212886163649955, 231.7504617458309895 ) ) ;
#98516 = CARTESIAN_POINT ( 'NONE',  ( -15.99459876049999885, 1425.540567386130078, 216.3101628860480048 ) ) ;
#98517 = CARTESIAN_POINT ( 'NONE',  ( -0.3150667361910010067, 1485.959260498290178, 221.0364148184989688 ) ) ;
#98518 = EDGE_CURVE ( 'NONE', #68277, #83651, #18057, .T. ) ;
#98519 = ADVANCED_FACE ( 'NONE', ( #2964 ), #72361, .T. ) ;
#98520 = CARTESIAN_POINT ( 'NONE',  ( -5.188151218920000751, 1391.908650948090099, 214.4790552262790015 ) ) ;
#98521 = CARTESIAN_POINT ( 'NONE',  ( 13.80599381087229993, 1434.979619881599774, 146.4346930152470065 ) ) ;
#98522 = ORIENTED_EDGE ( 'NONE', *, *, #69186, .F. ) ;
#98523 = CARTESIAN_POINT ( 'NONE',  ( -5.386286590926849804, 1432.308352799489967, 154.6070632664950040 ) ) ;
#98524 = CARTESIAN_POINT ( 'NONE',  ( 12.03834750937141607, 1513.050501378461377, 225.7232701713909933 ) ) ;
#98525 = CARTESIAN_POINT ( 'NONE',  ( 2.175409717514719593E-31, 1397.551704408390151, 209.1218459616989946 ) ) ;
#98526 = ORIENTED_EDGE ( 'NONE', *, *, #15165, .T. ) ;
#98527 = VERTEX_POINT ( 'NONE', #97544 ) ;
#98528 = CARTESIAN_POINT ( 'NONE',  ( -9.853100102660000914, 1384.791813251800022, 199.8713787141489888 ) ) ;
#98529 = CARTESIAN_POINT ( 'NONE',  ( 6.440198200940000284, 1422.794610071979832, 195.1019709172990133 ) ) ;
#98530 = ORIENTED_EDGE ( 'NONE', *, *, #7428, .T. ) ;
#98531 = CARTESIAN_POINT ( 'NONE',  ( 3.487587042568910167, 1508.884219106000046, 204.6305577925189993 ) ) ;
#98532 = CARTESIAN_POINT ( 'NONE',  ( 21.05584956750000103, 1495.071772848290038, 210.1533086104089989 ) ) ;
#98533 = CARTESIAN_POINT ( 'NONE',  ( -0.4270334199479999815, 1479.777432516030103, 236.1344528893980055 ) ) ;
#98534 = CARTESIAN_POINT ( 'NONE',  ( 16.53175237173092782, 1526.069472839378477, 235.9420435487000702 ) ) ;
#98535 = VERTEX_POINT ( 'NONE', #27578 ) ;
#98536 = CARTESIAN_POINT ( 'NONE',  ( 46.16775327660280226, 1441.856324383689980, 266.9713873395010069 ) ) ;
#98537 = CARTESIAN_POINT ( 'NONE',  ( -12.73643649006949907, 1414.913060387399810, 219.9105443766439976 ) ) ;
#98538 = CARTESIAN_POINT ( 'NONE',  ( 0.3152240322409999851, 1418.590776207229965, 184.6848380081979997 ) ) ;
#98539 = CARTESIAN_POINT ( 'NONE',  ( -2.488360667435000284, 1516.616791731099966, 203.3506968572170308 ) ) ;
#98540 = TOROIDAL_SURFACE ( 'NONE', #80653, 11.34254167809999991, 1.000000000000000000 ) ;
#98541 = EDGE_LOOP ( 'NONE', ( #28453, #60307, #10987, #59043 ) ) ;
#98542 = CARTESIAN_POINT ( 'NONE',  ( 11.23602576897910055, 1480.655328786240034, 212.7100351049870142 ) ) ;
#98543 = CARTESIAN_POINT ( 'NONE',  ( 9.720077016953126758, 1480.309013615846879, 204.9736173252133540 ) ) ;
#98544 = VERTEX_POINT ( 'NONE', #28691 ) ;
#98545 = ORIENTED_EDGE ( 'NONE', *, *, #90507, .T. ) ;
#98546 = CARTESIAN_POINT ( 'NONE',  ( -3.163365581163430029, 1508.551704140590118, 220.1905023666739964 ) ) ;
#98547 = CARTESIAN_POINT ( 'NONE',  ( 3.563478199850190098, 1497.907656018719990, 197.9170815786390278 ) ) ;
#98548 = CARTESIAN_POINT ( 'NONE',  ( -12.77505765355909872, 1512.281672892730057, 193.9892705280500138 ) ) ;
#98549 = CARTESIAN_POINT ( 'NONE',  ( 10.99289993254109810, 1452.529179862749970, 150.1608018894459917 ) ) ;
#98550 = CARTESIAN_POINT ( 'NONE',  ( 11.78588353789999843, 1420.143588805510035, 199.1665921514089916 ) ) ;
#98551 = CARTESIAN_POINT ( 'NONE',  ( -3.061616997868380553E-17, 1389.413060387289988, 209.1218459616989946 ) ) ;
#98552 = CARTESIAN_POINT ( 'NONE',  ( -107.9782425448296266, 1380.517964044677910, 298.4850064908227409 ) ) ;
#98553 = CARTESIAN_POINT ( 'NONE',  ( -21.39772323737049931, 1509.704958956720020, 229.7894127843639751 ) ) ;
#98554 = LINE ( 'NONE', #31352, #76785 ) ;
#98556 = CARTESIAN_POINT ( 'NONE',  ( -105.8303611032980029, 1391.403921100310072, 306.3485471784230185 ) ) ;
#98555 = CARTESIAN_POINT ( 'NONE',  ( 29.70307219812704247, 1525.408337840049853, 196.2982874201323114 ) ) ;
#98557 = CARTESIAN_POINT ( 'NONE',  ( 11.17902487211149953, 1422.624457870070046, 207.0208317409139909 ) ) ;
#98558 = VECTOR ( 'NONE', #33314, 1000.000000000000114 ) ;
#98559 = CARTESIAN_POINT ( 'NONE',  ( -24.08903237318989810, 1508.348042268949939, 222.3457766326179978 ) ) ;
#98560 = CARTESIAN_POINT ( 'NONE',  ( 7.255983564230000127, 1427.866122641229822, 147.4806042202980052 ) ) ;
#98561 = ORIENTED_EDGE ( 'NONE', *, *, #106857, .T. ) ;
#98562 = CARTESIAN_POINT ( 'NONE',  ( 19.46212511719999938, 1433.716220835580089, 224.8635561966979708 ) ) ;
#98563 = PLANE ( 'NONE',  #103496 ) ;
#98564 = CARTESIAN_POINT ( 'NONE',  ( -85.22981105258379841, 1384.980801281210006, 306.8062713692789885 ) ) ;
#98565 = CARTESIAN_POINT ( 'NONE',  ( -8.840249975039998986, 1385.811718649069917, 199.9964793815190092 ) ) ;
#98566 = DIRECTION ( 'NONE',  ( -0.08077839049150441209, -0.9967320861844480850, 0.000000000000000000 ) ) ;
#98568 = VERTEX_POINT ( 'NONE', #71285 ) ;
#98567 = CARTESIAN_POINT ( 'NONE',  ( -17.35671359422410021, 1419.675078620990007, 207.6719667936040139 ) ) ;
#98569 = CARTESIAN_POINT ( 'NONE',  ( 3.170476667209999988, 1429.217760481790037, 216.7986323648590030 ) ) ;
#98570 = VECTOR ( 'NONE', #56859, 1000.000000000000114 ) ;
#98571 = CARTESIAN_POINT ( 'NONE',  ( -2.500000000000000000, 1443.913060387330006, 150.6726614421979775 ) ) ;
#98572 = CARTESIAN_POINT ( 'NONE',  ( -14.45750876009999963, 1416.828042681729812, 221.3916373956980124 ) ) ;
#98573 = CYLINDRICAL_SURFACE ( 'NONE', #96911, 2.000000000000003553 ) ;
#98574 = EDGE_CURVE ( 'NONE', #98304, #19461, #89031, .T. ) ;
#98575 = CARTESIAN_POINT ( 'NONE',  ( 14.66019551493499939, 1513.841826332629807, 225.4222558759669823 ) ) ;
#98576 = CARTESIAN_POINT ( 'NONE',  ( 13.15726447890039985, 1414.913057819779851, 198.0251576192839877 ) ) ;
#98578 =( BOUNDED_CURVE ( )  B_SPLINE_CURVE ( 3, ( #21930, #90259, #47727, #66204 ),
 .UNSPECIFIED., .F., .T. ) 
 B_SPLINE_CURVE_WITH_KNOTS ( ( 4, 4 ),
 ( 4.168168146778059580, 5.256609830765320623 ),
 .UNSPECIFIED. ) 
 CURVE ( )  GEOMETRIC_REPRESENTATION_ITEM ( )  RATIONAL_B_SPLINE_CURVE ( ( 1.000000000000000000, 0.9036873071847475458, 0.9036873071847475458, 1.000000000000000000 ) ) 
 REPRESENTATION_ITEM ( '' )  );
#98577 = CONICAL_SURFACE ( 'NONE', #64644, 0.9999999999999962252, 1.047197551199999799 ) ;
#98579 = CARTESIAN_POINT ( 'NONE',  ( 6.454732559708139306, 1459.182081823159933, 201.6346944821260081 ) ) ;
#98580 = CARTESIAN_POINT ( 'NONE',  ( -106.5585968837300044, 1390.939245634569943, 300.3884029622149683 ) ) ;
#98581 = CARTESIAN_POINT ( 'NONE',  ( 15.89644188659999813, 1419.768287342929852, 227.4081588879980131 ) ) ;
#98582 = DIRECTION ( 'NONE',  ( -0.6736849260863841948, 0.000000000000000000, 0.7390186874254148774 ) ) ;
#98583 = CARTESIAN_POINT ( 'NONE',  ( -4.625693903144999730, 1517.042661899400173, 206.8353996064669786 ) ) ;
#98584 = CARTESIAN_POINT ( 'NONE',  ( 0.4151546846821903003, 1522.382868172863937, 242.9330574173806951 ) ) ;
#98585 = CARTESIAN_POINT ( 'NONE',  ( -17.96854058879999982, 1409.540535651430218, 222.8263146518980022 ) ) ;
#98586 = CARTESIAN_POINT ( 'NONE',  ( 1.549686116751380016, 1416.051481372750004, 190.4247184186629909 ) ) ;
#98587 = AXIS2_PLACEMENT_3D ( 'NONE', #108951, #75364, #4821 ) ;
#98588 = CARTESIAN_POINT ( 'NONE',  ( -1.120592404559999977, 1424.180376951730068, 228.4084508650980183 ) ) ;
#98589 = CARTESIAN_POINT ( 'NONE',  ( 5.385734361233229350, 1432.177428534629826, 154.6052364180729910 ) ) ;
#98590 = CARTESIAN_POINT ( 'NONE',  ( 0.008738962267850510293, 1515.558522550590169, 204.9671006875190074 ) ) ;
#98591 = FACE_OUTER_BOUND ( 'NONE', #55893, .T. ) ;
#98592 = CARTESIAN_POINT ( 'NONE',  ( -34.80965728144240501, 1436.610390194000047, 136.4824736869349806 ) ) ;
#98593 = B_SPLINE_CURVE_WITH_KNOTS ( 'NONE', 5,
 ( #995, #52496, #17735, #51937, #33446, #102857 ),
 .UNSPECIFIED., .F., .F.,
 ( 6, 6 ),
 ( 0.000000000000000000, 1.000000000000000000 ),
 .UNSPECIFIED. ) ;
#98594 = CARTESIAN_POINT ( 'NONE',  ( 0.2136699404695540094, 1455.290770098899884, 183.1551236798499929 ) ) ;
#98595 = CARTESIAN_POINT ( 'NONE',  ( -8.895217015593209098, 1407.887684287130242, 199.3644618170110050 ) ) ;
#98596 = CARTESIAN_POINT ( 'NONE',  ( -13.50674874249999924, 1414.971287085330005, 199.3316683369779980 ) ) ;
#98597 = CARTESIAN_POINT ( 'NONE',  ( -4.274335294360000148, 1515.341803653790066, 207.6472638932690131 ) ) ;
#98598 = CARTESIAN_POINT ( 'NONE',  ( -28.54117044909659739, 1509.686644087690183, 211.1713474645199824 ) ) ;
#98599 = CARTESIAN_POINT ( 'NONE',  ( 12.91307535960000052, 1434.774358524450236, 148.5017423775979921 ) ) ;
#98600 = CARTESIAN_POINT ( 'NONE',  ( -27.68327768569999847, 1435.464602415119771, 135.2595507401980228 ) ) ;
#98601 = CARTESIAN_POINT ( 'NONE',  ( -7.105427357599999217E-15, 1419.973720559130015, 171.2095165336979790 ) ) ;
#98602 = VERTEX_POINT ( 'NONE', #29237 ) ;
#98603 = CARTESIAN_POINT ( 'NONE',  ( 1.267691646300000086, 1484.678796645290049, 198.4480578130989841 ) ) ;
#98604 = CARTESIAN_POINT ( 'NONE',  ( 6.999275391030000293, 1479.249878728790009, 201.1196786008089816 ) ) ;
#98605 = CARTESIAN_POINT ( 'NONE',  ( -12.32434985131369842, 1409.343436167639766, 217.5774198073310117 ) ) ;
#98606 = CARTESIAN_POINT ( 'NONE',  ( -10.97260161140000001, 1492.335061974789824, 207.7727722944690072 ) ) ;
#98607 = EDGE_CURVE ( 'NONE', #13899, #67344, #58608, .T. ) ;
#98608 = CARTESIAN_POINT ( 'NONE',  ( 21.25167770093990072, 1489.809145040919930, 208.7427384965610031 ) ) ;
#98609 = FACE_OUTER_BOUND ( 'NONE', #73356, .T. ) ;
#98610 = CARTESIAN_POINT ( 'NONE',  ( 37.99169719898542041, 1421.960075112496497, 269.1794494414488099 ) ) ;
#98611 = CARTESIAN_POINT ( 'NONE',  ( -19.34729233231120205, 1486.470064436709890, 189.5887045964369975 ) ) ;
#98612 = CARTESIAN_POINT ( 'NONE',  ( -12.29932871299999952, 1378.340749811539808, 209.9617947631720085 ) ) ;
#98613 = CARTESIAN_POINT ( 'NONE',  ( -88.01709926131411521, 1384.622882125699789, 307.9926968129980196 ) ) ;
#98614 = CARTESIAN_POINT ( 'NONE',  ( -62.52713540591220465, 1385.073953399070206, 249.5246976450929992 ) ) ;
#98615 = CARTESIAN_POINT ( 'NONE',  ( -8.117475352257454091, 1423.842526962705506, 210.5481715165687149 ) ) ;
#98616 = CARTESIAN_POINT ( 'NONE',  ( 20.61542114510000090, 1508.364347661829925, 227.6602567121979916 ) ) ;
#98617 = CARTESIAN_POINT ( 'NONE',  ( 16.73628186595824019, 1526.382868172863937, 184.0591879540915272 ) ) ;
#98618 = CARTESIAN_POINT ( 'NONE',  ( 0.000000000000000000, 1526.382868172863937, 209.1218459616979999 ) ) ;
#98620 = ORIENTED_EDGE ( 'NONE', *, *, #29192, .F. ) ;
#98619 = CARTESIAN_POINT ( 'NONE',  ( 0.5099819841823221012, 1411.336581462000140, 185.0281086908349835 ) ) ;
#98621 = CARTESIAN_POINT ( 'NONE',  ( -109.9848792289999864, 1384.913535650479844, 311.4560967522589863 ) ) ;
#98622 = CARTESIAN_POINT ( 'NONE',  ( 10.65764281875889985, 1471.555037556759771, 211.7634253889970068 ) ) ;
#98623 = CARTESIAN_POINT ( 'NONE',  ( 3.149414619133680482, 1370.221588481574372, 210.2153961732977905 ) ) ;
#98624 = CARTESIAN_POINT ( 'NONE',  ( -0.3948765404462910023, 1418.680225851279829, 184.7139127450849969 ) ) ;
#98625 = CARTESIAN_POINT ( 'NONE',  ( 0.003118971330850000070, 1465.436580546529967, 236.3247307143980152 ) ) ;
#98626 = CARTESIAN_POINT ( 'NONE',  ( 22.17859137039999951, 1410.608979800430006, 215.6094025197479880 ) ) ;
#98627 = CARTESIAN_POINT ( 'NONE',  ( -2.425256225761660112, 1410.366585135190007, 186.4987601680199987 ) ) ;
#98628 = CARTESIAN_POINT ( 'NONE',  ( -18.71468957869999983, 1468.814975980689951, 201.1421764933589884 ) ) ;
#98629 = CARTESIAN_POINT ( 'NONE',  ( -17.97825106899999881, 1424.673537191730020, 227.3634650722979984 ) ) ;
#98631 = CARTESIAN_POINT ( 'NONE',  ( -11.34339085279999892, 1379.280816169740092, 204.1266110777590086 ) ) ;
#98630 = CARTESIAN_POINT ( 'NONE',  ( -13.73040295794826626, 1521.951704408389787, 190.6090220196199141 ) ) ;
#98632 = FACE_OUTER_BOUND ( 'NONE', #29137, .T. ) ;
#98633 = CARTESIAN_POINT ( 'NONE',  ( 0.3765318439190000199, 1477.269223033129947, 229.8244901576979942 ) ) ;
#98634 = CARTESIAN_POINT ( 'NONE',  ( 1732.234191736389675, 11221.53578756870047, 2410.535515148488230 ) ) ;
#98635 = CARTESIAN_POINT ( 'NONE',  ( -24.20883260440000129, 1435.739129888689831, 210.8967360531979978 ) ) ;
#98636 = CARTESIAN_POINT ( 'NONE',  ( 9.622136349630000751, 1363.684386430209997, 210.6218459616991936 ) ) ;
#98637 = AXIS2_PLACEMENT_3D ( 'NONE', #10921, #2545, #66574 ) ;
#98638 = CARTESIAN_POINT ( 'NONE',  ( -2.492130661305000050, 1516.778761582560037, 205.6761608547170113 ) ) ;
#98639 = CARTESIAN_POINT ( 'NONE',  ( 33.28034951413924603, 1512.187213306747481, 200.8029765415137433 ) ) ;
#98640 = ORIENTED_EDGE ( 'NONE', *, *, #5552, .F. ) ;
#98641 = CARTESIAN_POINT ( 'NONE',  ( -4.183240852922301301, 1454.059675636378415, 200.2646904393691614 ) ) ;
#98642 = CARTESIAN_POINT ( 'NONE',  ( 18.46483594369999892, 1415.628674276829770, 210.6745050120780149 ) ) ;
#98644 = ORIENTED_EDGE ( 'NONE', *, *, #99058, .T. ) ;
#98643 = CARTESIAN_POINT ( 'NONE',  ( -68.04155215168790960, 1379.746364830730045, 279.5506397144160360 ) ) ;
#98645 = ORIENTED_EDGE ( 'NONE', *, *, #88592, .T. ) ;
#98646 = CARTESIAN_POINT ( 'NONE',  ( 28.31978547999999662, 1509.874516473829999, 214.8570436738979765 ) ) ;
#98647 = VERTEX_POINT ( 'NONE', #47149 ) ;
#98648 = CARTESIAN_POINT ( 'NONE',  ( -0.2453275326669540068, 1485.933059197169996, 221.0102401867029869 ) ) ;
#98649 = EDGE_CURVE ( 'NONE', #25815, #89812, #82504, .T. ) ;
#98650 = CARTESIAN_POINT ( 'NONE',  ( -49.24962907673571522, 1524.382868172863937, 10.34030387146701813 ) ) ;
#98652 = CARTESIAN_POINT ( 'NONE',  ( 15.72108344340260011, 1409.846270172940194, 191.9446229745909989 ) ) ;
#98651 = CARTESIAN_POINT ( 'NONE',  ( 15.93782904601589934, 1419.538716697589962, 191.2487339700179803 ) ) ;
#98653 = EDGE_CURVE ( 'NONE', #26067, #63638, #19149, .T. ) ;
#98654 = CARTESIAN_POINT ( 'NONE',  ( 3.462835627365000057, 1517.038650117239968, 210.2415636864969883 ) ) ;
#98655 = ADVANCED_FACE ( 'NONE', ( #105398 ), #30512, .T. ) ;
#98656 = CIRCLE ( 'NONE', #102247, 1.000000000000005551 ) ;
#98657 = CARTESIAN_POINT ( 'NONE',  ( -25.23720171959060110, 1451.310931879150075, 137.2167829449969929 ) ) ;
#98658 = CARTESIAN_POINT ( 'NONE',  ( 33.93526097588131307, 1436.160851839354109, 136.3001501137667617 ) ) ;
#98659 = CARTESIAN_POINT ( 'NONE',  ( 15.61151356360000086, 1410.390253723229989, 227.1240187857980288 ) ) ;
#98660 = EDGE_CURVE ( 'NONE', #102140, #52122, #14625, .T. ) ;
#98661 = CARTESIAN_POINT ( 'NONE',  ( 10.65123798173899949, 1480.972066468270214, 211.8901002702700112 ) ) ;
#98662 = DIRECTION ( 'NONE',  ( 0.000000000000000000, 0.000000000000000000, 1.000000000000000000 ) ) ;
#98663 = EDGE_CURVE ( 'NONE', #86013, #37425, #39657, .T. ) ;
#98664 = CARTESIAN_POINT ( 'NONE',  ( 41.60033908837840499, 1444.718971643219902, 134.0999999983919793 ) ) ;
#98665 = DIRECTION ( 'NONE',  ( 0.000000000000000000, 0.000000000000000000, -1.000000000000000000 ) ) ;
#98666 = ORIENTED_EDGE ( 'NONE', *, *, #28861, .F. ) ;
#98667 = CARTESIAN_POINT ( 'NONE',  ( 13.90282916737450059, 1434.989572450550213, 148.6937415729140071 ) ) ;
#98668 = FACE_OUTER_BOUND ( 'NONE', #29057, .T. ) ;
#98669 = ORIENTED_EDGE ( 'NONE', *, *, #44798, .T. ) ;
#98670 = ORIENTED_EDGE ( 'NONE', *, *, #62551, .T. ) ;
#98671 = EDGE_CURVE ( 'NONE', #67655, #18109, #90223, .T. ) ;
#98672 = CARTESIAN_POINT ( 'NONE',  ( -6.259133024435000081, 1514.370494773850169, 216.8656120519870001 ) ) ;
#98673 = CARTESIAN_POINT ( 'NONE',  ( 37.66849513895419932, 1445.052233489950140, 137.0436250799990034 ) ) ;
#98674 = CARTESIAN_POINT ( 'NONE',  ( 12.46317070049899911, 1499.977136260429916, 206.8116722807479846 ) ) ;
#98675 = CARTESIAN_POINT ( 'NONE',  ( -19.38790225612389762, 1508.451864247089816, 209.8663014701650127 ) ) ;
#98676 = AXIS2_PLACEMENT_3D ( 'NONE', #32349, #66528, #33992 ) ;
#98677 = CARTESIAN_POINT ( 'NONE',  ( -13.83705309760000191, 1379.709095927359840, 208.1765788499700136 ) ) ;
#98678 = CARTESIAN_POINT ( 'NONE',  ( -68.77278092737650184, 1379.747928288920093, 280.3133413970129482 ) ) ;
#98679 = CARTESIAN_POINT ( 'NONE',  ( 9792.142915373007781, 50.28429875041810959, -1105.735996643114049 ) ) ;
#98680 = CARTESIAN_POINT ( 'NONE',  ( -1.321968956450000121, 1497.687671660330125, 231.6439708845980192 ) ) ;
#98681 = CARTESIAN_POINT ( 'NONE',  ( 6.282169504720000575, 1416.518938591829965, 191.8828167486979623 ) ) ;
#98682 = EDGE_CURVE ( 'NONE', #107607, #51438, #48997, .T. ) ;
#98683 = CARTESIAN_POINT ( 'NONE',  ( -61.94336356843140123, 1384.685152223810064, 248.2490218926199930 ) ) ;
#98684 = ORIENTED_EDGE ( 'NONE', *, *, #64219, .F. ) ;
#98685 = CIRCLE ( 'NONE', #77275, 1.999999999999999556 ) ;
#98686 = CARTESIAN_POINT ( 'NONE',  ( 9.436719802170449256, 1462.190294945330152, 206.7292107723660024 ) ) ;
#98687 = CARTESIAN_POINT ( 'NONE',  ( -4.044319925355000400, 1517.073005577650065, 208.0013022344469960 ) ) ;
#98688 = ORIENTED_EDGE ( 'NONE', *, *, #25438, .F. ) ;
#98689 = CARTESIAN_POINT ( 'NONE',  ( 7.509485228916700454E-15, 1517.551704408389924, 209.1218459616989946 ) ) ;
#98690 = CARTESIAN_POINT ( 'NONE',  ( 19.12129754759999756, 1477.356669723930054, 228.1731787199980204 ) ) ;
#98691 = VERTEX_POINT ( 'NONE', #7875 ) ;
#98692 = CARTESIAN_POINT ( 'NONE',  ( 13.15366522099999891, 1428.703228679929907, 223.0784815109979888 ) ) ;
#98693 = CARTESIAN_POINT ( 'NONE',  ( -15.82859721659999863, 1410.397881278330033, 191.2512645620979868 ) ) ;
#98694 = CARTESIAN_POINT ( 'NONE',  ( -17.63263719517827255, 1508.456413885124675, 212.4308869866120517 ) ) ;
#98695 = EDGE_CURVE ( 'NONE', #63015, #71163, #95823, .T. ) ;
#98696 = CARTESIAN_POINT ( 'NONE',  ( -9.580270985622490798, 1460.853522025070106, 207.7412804523160048 ) ) ;
#98697 = CARTESIAN_POINT ( 'NONE',  ( 22.28103957729450002, 1410.282322871559927, 206.2410114249429967 ) ) ;
#98698 = CARTESIAN_POINT ( 'NONE',  ( -5.854887960802339641, 1510.764648358910108, 201.5757148928349807 ) ) ;
#98699 = CARTESIAN_POINT ( 'NONE',  ( -2.889979094190000097, 1508.952905480530035, 179.9120178563979948 ) ) ;
#98700 = ADVANCED_FACE ( 'NONE', ( #84584 ), #40761, .F. ) ;
#98701 = CARTESIAN_POINT ( 'NONE',  ( -5.650234538444452781, 1510.510563500882199, 201.5728936304679451 ) ) ;
#98702 = CARTESIAN_POINT ( 'NONE',  ( -21.33281718256877824, 1523.429859730331145, 180.4846393450511641 ) ) ;
#98704 = DIRECTION ( 'NONE',  ( 0.7071067811870476172, 0.000000000000000000, -0.7071067811860475283 ) ) ;
#98703 = CARTESIAN_POINT ( 'NONE',  ( 15.33271527600000006, 1460.168619882530038, 230.3678631353980109 ) ) ;
#98705 = CARTESIAN_POINT ( 'NONE',  ( -6.941100315875000426, 1516.858069504249897, 216.0654486236869900 ) ) ;
#98706 = EDGE_CURVE ( 'NONE', #94134, #30502, #42043, .T. ) ;
#98707 = CARTESIAN_POINT ( 'NONE',  ( -9.467068884459999722, 1450.246902653889947, 204.4311477998990085 ) ) ;
#98708 = CARTESIAN_POINT ( 'NONE',  ( -10.35499315259030517, 1480.611330010711526, 207.1660253079129177 ) ) ;
#98709 = CARTESIAN_POINT ( 'NONE',  ( 2.759768239755020058, 1516.551696783219995, 216.8313331240459831 ) ) ;
#98710 = CARTESIAN_POINT ( 'NONE',  ( 2.878693249144999466, 1516.766397346390022, 213.1495431961470217 ) ) ;
#98711 = CARTESIAN_POINT ( 'NONE',  ( 3.644352556201880144, 1515.551704204679936, 212.3939927026280259 ) ) ;
#98712 = FACE_OUTER_BOUND ( 'NONE', #16230, .T. ) ;
#98714 = ORIENTED_EDGE ( 'NONE', *, *, #76957, .F. ) ;
#98713 = CARTESIAN_POINT ( 'NONE',  ( -5.007763590949999788, 1426.931744156050172, 207.4587325135290143 ) ) ;
#98715 = FACE_OUTER_BOUND ( 'NONE', #29502, .T. ) ;
#98716 = DIRECTION ( 'NONE',  ( 0.000000000000000000, 1.000000000000000000, 0.000000000000000000 ) ) ;
#98717 = CARTESIAN_POINT ( 'NONE',  ( -11.86130994329999844, 1432.001365804540001, 149.9732119217979971 ) ) ;
#98718 = CARTESIAN_POINT ( 'NONE',  ( -20.31208665306889927, 1487.462847046120032, 204.9267914088850091 ) ) ;
#98719 = CARTESIAN_POINT ( 'NONE',  ( -6.031237335843999681, 1442.578951278860131, 201.0497613954999849 ) ) ;
#98720 = CARTESIAN_POINT ( 'NONE',  ( 2.420926942500000401, 1415.924425175530132, 231.9930866673979892 ) ) ;
#98721 = CARTESIAN_POINT ( 'NONE',  ( 16.50400130224746675, 1525.907212628473644, 181.9890130758377609 ) ) ;
#98722 = CARTESIAN_POINT ( 'NONE',  ( 11.79002570369999958, 1447.121451514899718, 187.8029540045979786 ) ) ;
#98724 = CARTESIAN_POINT ( 'NONE',  ( 2.500000000000000000, 1419.383216040929938, 144.0854373786980034 ) ) ;
#98723 = CARTESIAN_POINT ( 'NONE',  ( -20.40381310260000092, 1444.801140792109891, 223.4425445369979855 ) ) ;
#98725 = CARTESIAN_POINT ( 'NONE',  ( -1.590912488230000088, 1484.788632896829995, 182.5874906166980054 ) ) ;
#98726 = ORIENTED_EDGE ( 'NONE', *, *, #47009, .T. ) ;
#98727 = CARTESIAN_POINT ( 'NONE',  ( -2.878693287274999957, 1516.766397346390022, 205.0941487061870134 ) ) ;
#98728 = CARTESIAN_POINT ( 'NONE',  ( 0.8891820839130000209, 1405.755862229229933, 267.5368302669979812 ) ) ;
#98729 = CARTESIAN_POINT ( 'NONE',  ( 10.95851507883410036, 1490.212960435480227, 209.1823932077190022 ) ) ;
#98730 = ADVANCED_FACE ( 'NONE', ( #68371 ), #88001, .F. ) ;
#98731 = CARTESIAN_POINT ( 'NONE',  ( 24.63111624260878685, 1440.210199689701540, 212.4614418941652900 ) ) ;
#98732 = ADVANCED_FACE ( 'NONE', ( #110342 ), #73454, .F. ) ;
#98733 = CARTESIAN_POINT ( 'NONE',  ( -3.523962701577560086, 1476.511731529740018, 220.0526012636759958 ) ) ;
#98734 = CARTESIAN_POINT ( 'NONE',  ( 11.60004869885203682, 1424.776121897636585, 137.5689991293697005 ) ) ;
#98735 = AXIS2_PLACEMENT_3D ( 'NONE', #60337, #51365, #42980 ) ;
#98736 = CARTESIAN_POINT ( 'NONE',  ( -10.07052356819160188, 1447.097068999800058, 211.4090694554620029 ) ) ;
#98737 = CARTESIAN_POINT ( 'NONE',  ( -2.498115821138040538, 1449.212599764990046, 155.3362512705470238 ) ) ;
#98738 = CYLINDRICAL_SURFACE ( 'NONE', #80702, 1.000000000000000888 ) ;
#98739 = CARTESIAN_POINT ( 'NONE',  ( -19.71995158176096652, 1486.080284922995588, 190.1322500716072454 ) ) ;
#98740 = CARTESIAN_POINT ( 'NONE',  ( -13.77282262973849924, 1415.219159639000054, 220.6941904408330117 ) ) ;
#98741 = CARTESIAN_POINT ( 'NONE',  ( -4.201107383170000098, 1515.456955069990045, 210.2333507927889968 ) ) ;
#98742 = CARTESIAN_POINT ( 'NONE',  ( 3.108624468949999707E-15, 1424.916853932230197, 224.8635561844979804 ) ) ;
#98743 = ADVANCED_FACE ( 'NONE', ( #88994 ), #65758, .F. ) ;
#98744 = CARTESIAN_POINT ( 'NONE',  ( -26.87061429964650117, 1508.006948577689855, 211.9372255802010159 ) ) ;
#98745 = FACE_OUTER_BOUND ( 'NONE', #98800, .T. ) ;
#98746 = CARTESIAN_POINT ( 'NONE',  ( -1.778002813740000132, 1476.025706879929885, 268.4824706862979724 ) ) ;
#98747 = LINE ( 'NONE', #47255, #38993 ) ;
#98748 = CARTESIAN_POINT ( 'NONE',  ( 24.02863916850529691, 1507.902931906480035, 195.9323055859989893 ) ) ;
#98749 = CARTESIAN_POINT ( 'NONE',  ( 18.10638723112739967, 1414.300371954559978, 223.0951481136329733 ) ) ;
#98750 = CARTESIAN_POINT ( 'NONE',  ( -42.07899341319999564, 1384.778030063439928, 245.8949318473310086 ) ) ;
#98751 = DIRECTION ( 'NONE',  ( -0.000000000000000000, -1.000000000000000000, -0.000000000000000000 ) ) ;
#98752 = CIRCLE ( 'NONE', #52265, 1.000000000000000888 ) ;
#98753 = CYLINDRICAL_SURFACE ( 'NONE', #57523, 2.000000000000003553 ) ;
#98754 = CARTESIAN_POINT ( 'NONE',  ( 12.16396381444949881, 1491.556051155780096, 207.3115473875270141 ) ) ;
#98755 = CARTESIAN_POINT ( 'NONE',  ( 31.31962774233649682, 1525.556090473913628, 216.7000093993642906 ) ) ;
#98756 = CARTESIAN_POINT ( 'NONE',  ( 8.510893208398943699, 1511.398734635591836, 204.1579629377903302 ) ) ;
#98757 = CARTESIAN_POINT ( 'NONE',  ( -9.885612070768521775, 1396.258273567759943, 214.0867141279609882 ) ) ;
#98758 = CARTESIAN_POINT ( 'NONE',  ( -14.63705847230000145, 1422.169902662129971, 229.4588690710980075 ) ) ;
#98759 = EDGE_CURVE ( 'NONE', #48269, #56530, #12866, .T. ) ;
#98760 = CARTESIAN_POINT ( 'NONE',  ( 19.27222582892916947, 1456.061223426223933, 225.1253623777946586 ) ) ;
#98761 = VERTEX_POINT ( 'NONE', #10087 ) ;
#98762 = CARTESIAN_POINT ( 'NONE',  ( -7.517448282616630451, 1410.548633254104288, 230.8423976230810695 ) ) ;
#98763 = CARTESIAN_POINT ( 'NONE',  ( -7.477233281890912409, 1510.784366248438573, 215.2449024152596166 ) ) ;
#98764 = CARTESIAN_POINT ( 'NONE',  ( -11.86716023049999968, 1432.353341358199941, 147.6509521729980179 ) ) ;
#98766 = CARTESIAN_POINT ( 'NONE',  ( -14.12475447096500147, 1513.169116394660023, 193.8258293473670051 ) ) ;
#98765 = CARTESIAN_POINT ( 'NONE',  ( -16.23751604409000038, 1416.676673989810070, 209.1091032500480082 ) ) ;
#98767 = CARTESIAN_POINT ( 'NONE',  ( -16.03585548469987998, 1409.473035015031883, 225.1837023168980352 ) ) ;
#98768 = EDGE_CURVE ( 'NONE', #11318, #16982, #40801, .T. ) ;
#98769 = CARTESIAN_POINT ( 'NONE',  ( -6.964608808889999558, 1453.224209856889956, 202.7117130979790147 ) ) ;
#98770 = CARTESIAN_POINT ( 'NONE',  ( 2.290886266485000267, 1517.184383877180153, 201.7830921018669983 ) ) ;
#98771 = CARTESIAN_POINT ( 'NONE',  ( 7.909027525009999948, 1426.208968979389965, 211.6952151749889879 ) ) ;
#98772 = CARTESIAN_POINT ( 'NONE',  ( -13.67845557849999949, 1504.250295190390034, 227.6838176112990197 ) ) ;
#98773 = CARTESIAN_POINT ( 'NONE',  ( 14.84895960063500020, 1511.957228877180114, 197.0446257365670135 ) ) ;
#98774 = CARTESIAN_POINT ( 'NONE',  ( -21.16165221186960110, 1418.123385324889796, 208.6155873984789935 ) ) ;
#98775 = CARTESIAN_POINT ( 'NONE',  ( -82.80618832229581017, 1377.207454081310289, 300.3238556022119496 ) ) ;
#98776 = CARTESIAN_POINT ( 'NONE',  ( 4.283227215352179762, 1367.979132611802015, 207.6218459616988241 ) ) ;
#98778 = ORIENTED_EDGE ( 'NONE', *, *, #27920, .F. ) ;
#98777 = CARTESIAN_POINT ( 'NONE',  ( 8.850386993630001697, 1454.013591409390074, 214.2286051505190017 ) ) ;
#98779 = VERTEX_POINT ( 'NONE', #91750 ) ;
#98780 = CARTESIAN_POINT ( 'NONE',  ( -12.08279855019999971, 1398.271306150530108, 203.2690269987980116 ) ) ;
#98781 = CARTESIAN_POINT ( 'NONE',  ( -21.64909456690000056, 1411.027735339629999, 216.4118746903779993 ) ) ;
#98782 = CARTESIAN_POINT ( 'NONE',  ( -1.556886619979999997, 1415.063410501429871, 226.7642036972980009 ) ) ;
#98783 = CARTESIAN_POINT ( 'NONE',  ( -13.22654679013079537, 1444.679112648444061, 169.3876301519718766 ) ) ;
#98784 = ADVANCED_FACE ( 'NONE', ( #5554 ), #56460, .F. ) ;
#98785 = DIRECTION ( 'NONE',  ( 0.000000000000000000, -1.000000000000000000, 0.000000000000000000 ) ) ;
#98786 = CARTESIAN_POINT ( 'NONE',  ( -7.621419158765000645, 1512.021995456199875, 211.6878531360469822 ) ) ;
#98788 = CARTESIAN_POINT ( 'NONE',  ( -21.53565904410000087, 1506.077647802389947, 209.2113159668039941 ) ) ;
#98787 = CARTESIAN_POINT ( 'NONE',  ( -8.251661180240001059, 1383.545955608860140, 218.5607180263089901 ) ) ;
#98789 = CARTESIAN_POINT ( 'NONE',  ( 1.567402629779999890, 1410.307036984029992, 185.3288458999980151 ) ) ;
#98790 = ADVANCED_FACE ( 'NONE', ( #64669 ), #39474, .T. ) ;
#98791 = CARTESIAN_POINT ( 'NONE',  ( -4.467442984997470390, 1464.039775823070158, 199.9285363783119749 ) ) ;
#98792 = CARTESIAN_POINT ( 'NONE',  ( -40.21925577861330225, 1446.541393603889901, 136.6959051559719853 ) ) ;
#98793 = CARTESIAN_POINT ( 'NONE',  ( 10.44466107780339925, 1396.277795989850119, 212.7871969495540156 ) ) ;
#98794 = CARTESIAN_POINT ( 'NONE',  ( 1.343523894720000111, 1416.547221147930031, 190.1769955903980076 ) ) ;
#98795 = CARTESIAN_POINT ( 'NONE',  ( 11.82328634059999928, 1429.482282172129999, 149.2137815048980087 ) ) ;
#98796 = CARTESIAN_POINT ( 'NONE',  ( 7.475494255215000550, 1511.623805160490065, 202.7254354214969965 ) ) ;
#98797 = ORIENTED_EDGE ( 'NONE', *, *, #62066, .F. ) ;
#98798 = DIRECTION ( 'NONE',  ( -4.222254822704964968E-17, -1.000000000000000000, 7.728785610902679540E-17 ) ) ;
#98799 = FACE_OUTER_BOUND ( 'NONE', #33778, .T. ) ;
#98800 = EDGE_LOOP ( 'NONE', ( #39212, #57520, #60234 ) ) ;
#98801 = VERTEX_POINT ( 'NONE', #67424 ) ;
#98802 = ADVANCED_FACE ( 'NONE', ( #75805 ), #65210, .T. ) ;
#98803 = CARTESIAN_POINT ( 'NONE',  ( -5.010776572990000233, 1425.617167130440066, 208.7696333329660092 ) ) ;
#98804 = CARTESIAN_POINT ( 'NONE',  ( -14.48621421730000058, 1460.257914811229966, 230.6628917214979992 ) ) ;
#98805 = CARTESIAN_POINT ( 'NONE',  ( -109.9823850403438712, 1385.269780471392323, 311.4448117272161198 ) ) ;
#98806 = CARTESIAN_POINT ( 'NONE',  ( -28.62766089293194227, 1526.344110814219903, 198.0439708942000721 ) ) ;
#98807 = CARTESIAN_POINT ( 'NONE',  ( 5.005071008295000290, 1516.710692850270107, 216.4473877573669824 ) ) ;
#98808 = CARTESIAN_POINT ( 'NONE',  ( -12.31216202546280059, 1378.376212517099930, 209.7634181235169706 ) ) ;
#98809 = ADVANCED_FACE ( 'NONE', ( #5848 ), #22445, .T. ) ;
#98810 = ORIENTED_EDGE ( 'NONE', *, *, #50775, .T. ) ;
#98811 = CARTESIAN_POINT ( 'NONE',  ( -18.59685951017700134, 1508.551704410880120, 210.2475276029339852 ) ) ;
#98812 = CARTESIAN_POINT ( 'NONE',  ( 2.500000000000079936, 1448.852881373850096, 156.0659984934969771 ) ) ;
#98813 = CARTESIAN_POINT ( 'NONE',  ( -42.05438492420000074, 1375.117442312619914, 227.1521432528590196 ) ) ;
#98814 = CARTESIAN_POINT ( 'NONE',  ( 0.3142747836059999744, 1415.426210663629945, 226.6044997240979910 ) ) ;
#98815 = CARTESIAN_POINT ( 'NONE',  ( 2.286446325635000054, 1517.042661899400173, 204.4961520670869959 ) ) ;
#98816 = ORIENTED_EDGE ( 'NONE', *, *, #94906, .T. ) ;
#98817 = CARTESIAN_POINT ( 'NONE',  ( -0.7402208985179988820, 1516.992029636990083, 209.8751463226419958 ) ) ;
#98818 = CARTESIAN_POINT ( 'NONE',  ( -9.154585039681560232, 1450.683066379740012, 207.9130041143549761 ) ) ;
#98819 = CARTESIAN_POINT ( 'NONE',  ( -29.83261703232589923, 1419.454359286137787, 269.4690300932230684 ) ) ;
#98820 = CARTESIAN_POINT ( 'NONE',  ( 6.338109897684999439, 1511.735270473999890, 216.7196367433270154 ) ) ;
#98822 = ORIENTED_EDGE ( 'NONE', *, *, #34627, .T. ) ;
#98821 = LINE ( 'NONE', #30515, #35118 ) ;
#98823 = ADVANCED_FACE ( 'NONE', ( #39988 ), #10787, .T. ) ;
#98824 = CARTESIAN_POINT ( 'NONE',  ( -0.01304952888453610182, 1452.849458485459763, 183.2395837122380158 ) ) ;
#98826 = B_SPLINE_CURVE_WITH_KNOTS ( 'NONE', 5,
 ( #45411, #3958, #86835, #44862, #79552, #71169 ),
 .UNSPECIFIED., .F., .F.,
 ( 6, 6 ),
 ( -2.000000000000000000, 0.000000000000000000 ),
 .UNSPECIFIED. ) ;
#98825 = CARTESIAN_POINT ( 'NONE',  ( -30.65930537466649852, 1440.913060387579890, 240.3862288817810224 ) ) ;
#98827 = CARTESIAN_POINT ( 'NONE',  ( -49.65271057950000255, 1384.118016094159884, 260.8803987871590380 ) ) ;
#98828 = CARTESIAN_POINT ( 'NONE',  ( -0.06802918170042410173, 1467.142004300180133, 235.6414935935190158 ) ) ;
#98829 = CARTESIAN_POINT ( 'NONE',  ( 39.55870798286069601, 1428.444394588759906, 270.0311279852339794 ) ) ;
#98830 = ADVANCED_FACE ( 'NONE', ( #86953 ), #78563, .F. ) ;
#98831 = CARTESIAN_POINT ( 'NONE',  ( 1.714334247185000049, 1516.699825673279975, 213.1484604498870112 ) ) ;
#98832 = CARTESIAN_POINT ( 'NONE',  ( -62.83880642449999954, 1379.741026228560031, 268.0244666111590277 ) ) ;
#98833 = CARTESIAN_POINT ( 'NONE',  ( 23.01582909600000093, 1409.742947454629984, 209.0450749743000074 ) ) ;
#98834 = FACE_OUTER_BOUND ( 'NONE', #44139, .T. ) ;
#98835 = CARTESIAN_POINT ( 'NONE',  ( -13.15726454016349933, 1414.996443537369942, 220.4820293315119955 ) ) ;
#98836 = CARTESIAN_POINT ( 'NONE',  ( -7.709419779119449423, 1516.549122391340006, 210.7997296842460173 ) ) ;
#98837 = CARTESIAN_POINT ( 'NONE',  ( -4.026614517785000125, 1516.699825673279975, 210.8361802174170236 ) ) ;
#98838 = CARTESIAN_POINT ( 'NONE',  ( 4.203924555649190431, 1421.744692650780280, 184.5805578976949732 ) ) ;
#98839 = CARTESIAN_POINT ( 'NONE',  ( 17.78793234590488481, 1523.919934424249959, 180.4102106179817042 ) ) ;
#98840 = CARTESIAN_POINT ( 'NONE',  ( -106.4193208100000021, 1384.931129459059775, 311.3263713972589812 ) ) ;
#98841 = VERTEX_POINT ( 'NONE', #102623 ) ;
#98842 = CARTESIAN_POINT ( 'NONE',  ( -33.46600142563520563, 1385.216900170149984, 232.0947013295109969 ) ) ;
#98843 = CARTESIAN_POINT ( 'NONE',  ( 18.64588645199999917, 1416.828044802730119, 209.6843146608260042 ) ) ;
#98844 = CARTESIAN_POINT ( 'NONE',  ( -0.02063504396140000002, 1416.982032014529977, 234.1905969501979996 ) ) ;
#98845 = CARTESIAN_POINT ( 'NONE',  ( -9.786977755216737407, 1519.551704408389924, 191.2793932881676540 ) ) ;
#98846 = CARTESIAN_POINT ( 'NONE',  ( 7.559673304084999934, 1510.830536680500245, 205.9482437802269885 ) ) ;
#98847 = CARTESIAN_POINT ( 'NONE',  ( 11.41335056429999995, 1426.197677042169971, 205.8024195469589870 ) ) ;
#98848 = CARTESIAN_POINT ( 'NONE',  ( -11.89463746655019882, 1434.488622496119888, 147.6463952747150188 ) ) ;
#98850 = CARTESIAN_POINT ( 'NONE',  ( -10.10004869885203682, 0.000000000000000000, 135.5999999980979851 ) ) ;
#98849 = CARTESIAN_POINT ( 'NONE',  ( 0.7533001353030019942, 1516.714320817460020, 216.4479181143769893 ) ) ;
#98851 = CARTESIAN_POINT ( 'NONE',  ( -25.91673698548662230, 1450.780993184907857, 136.7962322576231884 ) ) ;
#98852 = CARTESIAN_POINT ( 'NONE',  ( -3.350338079455601026, 1523.604703353109699, 176.1628856388066708 ) ) ;
#98853 = ORIENTED_EDGE ( 'NONE', *, *, #31658, .F. ) ;
#98854 = CARTESIAN_POINT ( 'NONE',  ( -2.485217232065000115, 1516.534320418310244, 201.4128137944169907 ) ) ;
#98855 = CARTESIAN_POINT ( 'NONE',  ( -18.64672481365220236, 1416.851343896850040, 208.5597484336410048 ) ) ;
#98856 = VERTEX_POINT ( 'NONE', #1311 ) ;
#98857 = CARTESIAN_POINT ( 'NONE',  ( 11.60004869885203682, 1426.786827912535728, 134.3786173235958472 ) ) ;
#98858 = CARTESIAN_POINT ( 'NONE',  ( 23.96634320729999956, 1447.652375259820019, 215.5884833387879951 ) ) ;
#98859 = CARTESIAN_POINT ( 'NONE',  ( 10.79317411587489950, 1461.870335762409923, 211.1042069659010281 ) ) ;
#98860 = CARTESIAN_POINT ( 'NONE',  ( 9.226840260308872388, 1425.198049312735975, 195.6167264984963765 ) ) ;
#98861 = CARTESIAN_POINT ( 'NONE',  ( 2.232433900040000196, 1443.114183221789972, 217.7415636394590024 ) ) ;
#98862 = CARTESIAN_POINT ( 'NONE',  ( 16.32344763033163559, 1421.553467051097869, 227.2347501064996891 ) ) ;
#98863 = CARTESIAN_POINT ( 'NONE',  ( 9.093901123017769095, 1470.494570018200193, 191.1297851741429952 ) ) ;
#98864 = CARTESIAN_POINT ( 'NONE',  ( -19.53791504940000223, 1426.663906195230084, 224.0751841881980226 ) ) ;
#98865 = CARTESIAN_POINT ( 'NONE',  ( -20.26467651240000123, 1485.408278981489957, 205.1073287502989899 ) ) ;
#98866 = CARTESIAN_POINT ( 'NONE',  ( -106.5486053249999969, 1387.898087395329867, 298.3709353731589999 ) ) ;
#98867 = CARTESIAN_POINT ( 'NONE',  ( 18.25078530649999919, 1498.105401280229898, 188.8231487391980181 ) ) ;
#98869 = CARTESIAN_POINT ( 'NONE',  ( -18.46874166461617151, 1436.582161157081146, 212.8784271109066992 ) ) ;
#98868 = CARTESIAN_POINT ( 'NONE',  ( -105.6997850770000014, 1391.688872221259999, 304.2060384943590066 ) ) ;
#98870 = CARTESIAN_POINT ( 'NONE',  ( -9.856202761009180691, 1472.140734045829959, 211.6206523853309704 ) ) ;
#98871 = VERTEX_POINT ( 'NONE', #35451 ) ;
#98872 = CARTESIAN_POINT ( 'NONE',  ( -105.6135012430000018, 1378.264671279439881, 303.3196108302589664 ) ) ;
#98873 = LINE ( 'NONE', #82066, #87547 ) ;
#98874 = CARTESIAN_POINT ( 'NONE',  ( -10.79902394581574221, 1424.930925960156173, 143.1565572995466198 ) ) ;
#98875 = CARTESIAN_POINT ( 'NONE',  ( 11.38728035538260208, 1470.834447203169930, 208.6597894033529883 ) ) ;
#98876 = FACE_OUTER_BOUND ( 'NONE', #79941, .T. ) ;
#98877 = CARTESIAN_POINT ( 'NONE',  ( 1.457708929429750055, 1498.159145731940043, 181.5038820770699886 ) ) ;
#98878 = CARTESIAN_POINT ( 'NONE',  ( -1.682318767883554278, 1409.475163258161501, 186.2035163977165269 ) ) ;
#98879 = CARTESIAN_POINT ( 'NONE',  ( -13.44172084558439018, 1444.321659713776171, 186.9696591558638659 ) ) ;
#98880 = CARTESIAN_POINT ( 'NONE',  ( -24.87779863397740243, 1440.202515696970067, 210.4162827866140049 ) ) ;
#98881 = CARTESIAN_POINT ( 'NONE',  ( 4.164418577872849525, 1494.305047636430118, 219.6348937993929837 ) ) ;
#98882 = DIRECTION ( 'NONE',  ( 0.000000000000000000, 1.000000000000000000, 0.000000000000000000 ) ) ;
#98883 = CARTESIAN_POINT ( 'NONE',  ( -104.5883840766809953, 1383.761025698020148, 310.9908609358749914 ) ) ;
#98884 = CARTESIAN_POINT ( 'NONE',  ( 24.93050923819999909, 1436.289048159549793, 137.8926102245979735 ) ) ;
#98885 = CARTESIAN_POINT ( 'NONE',  ( 7.605961836409999677, 1428.548125308290082, 214.1230708307590191 ) ) ;
#98887 = ORIENTED_EDGE ( 'NONE', *, *, #23580, .F. ) ;
#98886 = CARTESIAN_POINT ( 'NONE',  ( -18.78579970166540036, 1443.967530420280127, 210.3883505492739801 ) ) ;
#98888 = CARTESIAN_POINT ( 'NONE',  ( -109.9987472910000008, 1380.124979902150017, 307.5701647321589576 ) ) ;
#98889 = CARTESIAN_POINT ( 'NONE',  ( 13.64573737686789912, 1512.804203059180054, 224.4338647574110155 ) ) ;
#98890 = VERTEX_POINT ( 'NONE', #103762 ) ;
#98891 = VERTEX_POINT ( 'NONE', #1879 ) ;
#98892 = CARTESIAN_POINT ( 'NONE',  ( -11.42085373749999988, 1500.664288093890036, 209.5050427136080202 ) ) ;
#98893 = CARTESIAN_POINT ( 'NONE',  ( 6.198157297588786641, 1516.723276579750518, 204.8982196523435846 ) ) ;
#98894 = CARTESIAN_POINT ( 'NONE',  ( -8.164798220873796808, 1383.354011203070968, 199.7069691412050076 ) ) ;
#98896 = CARTESIAN_POINT ( 'NONE',  ( -28.66942461689999888, 1455.243640874929952, 248.2467662535980253 ) ) ;
#98895 = CARTESIAN_POINT ( 'NONE',  ( 25.36271876829972172, 1416.586431751986311, 269.4273607397962564 ) ) ;
#98897 = CARTESIAN_POINT ( 'NONE',  ( -20.28483480839999942, 1503.699721672330043, 189.5804053314980138 ) ) ;
#98898 = CARTESIAN_POINT ( 'NONE',  ( -11.90306278269999929, 1433.319533555049929, 150.0454030812979909 ) ) ;
#98899 = CARTESIAN_POINT ( 'NONE',  ( 0.000000000000000000, 1512.051704408390151, 209.1218459616989946 ) ) ;
#98900 = CARTESIAN_POINT ( 'NONE',  ( 11.61600128336219839, 1426.776741275609993, 135.5201114608300088 ) ) ;
#98901 = CARTESIAN_POINT ( 'NONE',  ( 9.207476614228639278, 1464.697200489039915, 212.6097977664159941 ) ) ;
#98902 = CARTESIAN_POINT ( 'NONE',  ( -25.38336389990000086, 1437.595645302209959, 137.6395686390980018 ) ) ;
#98903 = CARTESIAN_POINT ( 'NONE',  ( 1.251490820293549966, 1515.089511802750167, 213.4506474497650004 ) ) ;
#98904 = CARTESIAN_POINT ( 'NONE',  ( 8.510960778390000314, 1440.269029158009971, 153.6986480022980004 ) ) ;
#98905 = CARTESIAN_POINT ( 'NONE',  ( -7.933021179928469557, 1478.422619274720091, 217.6197839746220097 ) ) ;
#98906 = CARTESIAN_POINT ( 'NONE',  ( 3.426613460960548085, 1360.656565846677722, 210.6218459616987957 ) ) ;
#98907 = CARTESIAN_POINT ( 'NONE',  ( -5.847473420468886296, 1509.246610639426535, 238.5602555325059484 ) ) ;
#98909 = ORIENTED_EDGE ( 'NONE', *, *, #86424, .T. ) ;
#98908 = CARTESIAN_POINT ( 'NONE',  ( 1.301951668218010061E-10, 1411.335116748880182, 255.3083647514700090 ) ) ;
#98910 = EDGE_LOOP ( 'NONE', ( #103073, #92220, #101806, #33582, #89, #11424, #44174, #90280 ) ) ;
#98911 = CARTESIAN_POINT ( 'NONE',  ( -11.56701740770000164, 1505.460402719889998, 207.8473594444390073 ) ) ;
#98912 = CARTESIAN_POINT ( 'NONE',  ( -21.46116573947509920, 1504.834610015079988, 215.7390694031070097 ) ) ;
#98913 = CARTESIAN_POINT ( 'NONE',  ( -34.31228247859999669, 1461.759392064230042, 270.3000846135980169 ) ) ;
#98914 = CARTESIAN_POINT ( 'NONE',  ( -1.547930050009999947, 1416.311719782429918, 227.9539241407980228 ) ) ;
#98915 = CARTESIAN_POINT ( 'NONE',  ( -123.7110048619999958, 1378.528619065190014, 304.2218459572590064 ) ) ;
#98916 = CARTESIAN_POINT ( 'NONE',  ( 29.79881796581619469, 1526.748660780343698, 221.5803863269301246 ) ) ;
#98917 = EDGE_CURVE ( 'NONE', #64661, #2574, #9690, .T. ) ;
#98918 = FACE_OUTER_BOUND ( 'NONE', #34507, .T. ) ;
#98919 = EDGE_CURVE ( 'NONE', #108026, #64960, #97897, .T. ) ;
#98920 = CARTESIAN_POINT ( 'NONE',  ( 3.394586470828380165, 1484.752177860970050, 220.4731790445629827 ) ) ;
#98921 = DIRECTION ( 'NONE',  ( -5.980589973904019347E-17, 1.000000000000000000, -1.736889445713099699E-16 ) ) ;
#98922 = CARTESIAN_POINT ( 'NONE',  ( -5.729479221760000129, 1458.872054288590107, 217.7597387405890288 ) ) ;
#98923 = CARTESIAN_POINT ( 'NONE',  ( 11.45468757771786450, 1366.970939356060853, 209.6218459617033432 ) ) ;
#98924 = CARTESIAN_POINT ( 'NONE',  ( -37.53908224095089707, 1420.183636347619995, 266.9518714729799740 ) ) ;
#98925 = ORIENTED_EDGE ( 'NONE', *, *, #41926, .F. ) ;
#98926 = CARTESIAN_POINT ( 'NONE',  ( -3.539686542936679725, 1497.693967252670063, 181.3788000397719884 ) ) ;
#98927 = ORIENTED_EDGE ( 'NONE', *, *, #6044, .T. ) ;
#98928 = EDGE_LOOP ( 'NONE', ( #110112, #59705 ) ) ;
#98929 = CARTESIAN_POINT ( 'NONE',  ( 2.881548424445000034, 1516.909589401870107, 211.4054166033970148 ) ) ;
#98930 = CARTESIAN_POINT ( 'NONE',  ( 33.46233750170772225, 1444.994950788469168, 154.5794059528860203 ) ) ;
#98931 = CARTESIAN_POINT ( 'NONE',  ( -5.771797464315000070, 1516.647618671360078, 211.9976960644470125 ) ) ;
#98932 = CARTESIAN_POINT ( 'NONE',  ( -14.43318959600000007, 1455.449656469629872, 188.2552579046979986 ) ) ;
#98933 = EDGE_CURVE ( 'NONE', #86983, #53037, #53259, .T. ) ;
#98934 = CARTESIAN_POINT ( 'NONE',  ( -11.60004869885203682, 1428.983126981193436, 134.0999999980979851 ) ) ;
#98935 = VERTEX_POINT ( 'NONE', #67979 ) ;
#98936 = CARTESIAN_POINT ( 'NONE',  ( -26.62406874550000069, 1435.731906908609972, 136.2240211947980129 ) ) ;
#98937 = CARTESIAN_POINT ( 'NONE',  ( 2.290886266485000267, 1517.184383877180153, 201.7830921018669983 ) ) ;
#98938 = CARTESIAN_POINT ( 'NONE',  ( 20.71343476517512272, 1512.187213306747481, 179.9059455038194528 ) ) ;
#98939 = CARTESIAN_POINT ( 'NONE',  ( 1.317974831259093316, 1508.993303073226343, 238.7438154217258557 ) ) ;
#98940 = CARTESIAN_POINT ( 'NONE',  ( -44.13013983209490476, 1435.750459799680129, 270.2165836708290385 ) ) ;
#98941 = CARTESIAN_POINT ( 'NONE',  ( -6.338192872240000497, 1481.865655818189907, 205.0401094726289841 ) ) ;
#98942 = CARTESIAN_POINT ( 'NONE',  ( -1.233242815080000110, 1396.496402683329961, 196.6588694784980191 ) ) ;
#98944 = ORIENTED_EDGE ( 'NONE', *, *, #39882, .F. ) ;
#98943 = CARTESIAN_POINT ( 'NONE',  ( -8.790915045283584917, 1365.067705246386822, 210.6218459617142003 ) ) ;
#98945 = ORIENTED_EDGE ( 'NONE', *, *, #52190, .T. ) ;
#98946 = CIRCLE ( 'NONE', #79310, 2.000000000000001776 ) ;
#98947 = CARTESIAN_POINT ( 'NONE',  ( 2.897647365308007039, 1475.048391750445489, 269.6500680714580653 ) ) ;
#98948 = CARTESIAN_POINT ( 'NONE',  ( 2.976200793056689609, 1426.218032820240069, 191.3194850719970077 ) ) ;
#98949 = CARTESIAN_POINT ( 'NONE',  ( -14.36669942202730077, 1436.256511924010056, 150.0155719173559987 ) ) ;
#98950 = CARTESIAN_POINT ( 'NONE',  ( -1.267179638100000227, 1485.071352279529947, 182.1863245234980013 ) ) ;
#98951 = EDGE_CURVE ( 'NONE', #19921, #80510, #27602, .T. ) ;
#98952 = CARTESIAN_POINT ( 'NONE',  ( 1.717139084115000047, 1516.949031626070109, 210.2396860569670025 ) ) ;
#98953 = CARTESIAN_POINT ( 'NONE',  ( 9.146299198640271300, 1461.861878385089767, 205.8341600298289791 ) ) ;
#98954 = CARTESIAN_POINT ( 'NONE',  ( -18.69112752649999720, 1430.796159002630020, 225.2456904468979815 ) ) ;
#98955 = CARTESIAN_POINT ( 'NONE',  ( 6.624757470297610418, 1440.385568604370064, 215.0349520669070102 ) ) ;
#98956 = CARTESIAN_POINT ( 'NONE',  ( 11.90129930089999988, 1415.245980409429876, 222.6985869743980118 ) ) ;
#98957 = CARTESIAN_POINT ( 'NONE',  ( -4.221362096953909848, 1441.596168439879875, 170.5366494805969921 ) ) ;
#98958 = CARTESIAN_POINT ( 'NONE',  ( -3.462948834675000143, 1516.956048353049937, 206.8373194734570006 ) ) ;
#98959 = EDGE_CURVE ( 'NONE', #9890, #85608, #70205, .T. ) ;
#98960 = ORIENTED_EDGE ( 'NONE', *, *, #49480, .F. ) ;
#98961 = CARTESIAN_POINT ( 'NONE',  ( -42.60628464300700102, 1443.705283383359983, 135.3761640576199738 ) ) ;
#98962 = CARTESIAN_POINT ( 'NONE',  ( -22.71570642892181624, 1451.001388305250430, 218.7895664819020283 ) ) ;
#98963 = EDGE_LOOP ( 'NONE', ( #63775, #2153, #35363, #13343, #56003 ) ) ;
#98964 = CARTESIAN_POINT ( 'NONE',  ( 18.07930019939639621, 1457.670260863833164, 229.7183053949007956 ) ) ;
#98965 = CARTESIAN_POINT ( 'NONE',  ( 25.15410452086170068, 1451.315323596600138, 137.3483238205280088 ) ) ;
#98966 = CARTESIAN_POINT ( 'NONE',  ( 13.91384509699999938, 1415.996778984329922, 196.5752437455980157 ) ) ;
#98967 = CARTESIAN_POINT ( 'NONE',  ( -16.53125420670000167, 1418.541487540729804, 202.7561987471289910 ) ) ;
#98968 = CARTESIAN_POINT ( 'NONE',  ( 19.29764154210000271, 1410.948454093429746, 195.8526098399979958 ) ) ;
#98969 = DIRECTION ( 'NONE',  ( -0.9942586961433752535, 0.000000000000000000, 0.1070030146457353060 ) ) ;
#98970 = CARTESIAN_POINT ( 'NONE',  ( 10.79528401680000016, 1489.628194867089860, 207.4012257089289903 ) ) ;
#98971 = CARTESIAN_POINT ( 'NONE',  ( -13.80541478530910027, 1434.979604282769969, 148.5370187744020143 ) ) ;
#98972 = CARTESIAN_POINT ( 'NONE',  ( 24.59103204445768043, 1443.271088975028761, 213.0685705457873382 ) ) ;
#98973 = CARTESIAN_POINT ( 'NONE',  ( -18.28985832939522993, 1517.151704408390060, 198.5293912879491529 ) ) ;
#98974 = CARTESIAN_POINT ( 'NONE',  ( 3.262264650305000124, 1516.633288330999903, 215.6694029015669969 ) ) ;
#98975 = ORIENTED_EDGE ( 'NONE', *, *, #95240, .T. ) ;
#98976 = CARTESIAN_POINT ( 'NONE',  ( 7.709204607498650219, 1516.540906774789846, 207.3459979817129977 ) ) ;
#98977 = CARTESIAN_POINT ( 'NONE',  ( -39.29615804430000026, 1457.459686057429963, 269.7910478776980199 ) ) ;
#98978 = CARTESIAN_POINT ( 'NONE',  ( 16.68463225900990210, 1445.052233488270076, 162.0935120915889911 ) ) ;
#98979 = CARTESIAN_POINT ( 'NONE',  ( -5.850883015700239831, 1422.777641411109926, 112.2634153026260009 ) ) ;
#98980 = CARTESIAN_POINT ( 'NONE',  ( -2.990731931200000471, 1475.888290570790105, 219.4132863883990296 ) ) ;
#98981 = CARTESIAN_POINT ( 'NONE',  ( 11.60004869885203682, 1426.432599161485996, 138.7994597023310916 ) ) ;
#98982 = CARTESIAN_POINT ( 'NONE',  ( 2.077066168525637302, 1417.353822717204594, 233.2012438648220893 ) ) ;
#98983 = CARTESIAN_POINT ( 'NONE',  ( 17.89881597930054014, 1423.835250522596425, 225.8299768472458311 ) ) ;
#98984 = LINE ( 'NONE', #4933, #70089 ) ;
#98985 = DIRECTION ( 'NONE',  ( 5.980589973904019347E-17, -1.000000000000000000, 1.736889445713099699E-16 ) ) ;
#98986 = CARTESIAN_POINT ( 'NONE',  ( 35.19864010958440304, 1440.913060386249981, 251.3230737458970054 ) ) ;
#98987 = CARTESIAN_POINT ( 'NONE',  ( -109.8956297860000006, 1384.931289663850066, 297.0283806398589945 ) ) ;
#98988 = CARTESIAN_POINT ( 'NONE',  ( -32.38114538885259464, 1523.604703353109699, 202.1233279672532888 ) ) ;
#98989 = ORIENTED_EDGE ( 'NONE', *, *, #17252, .T. ) ;
#98990 = ORIENTED_EDGE ( 'NONE', *, *, #60466, .F. ) ;
#98991 = CARTESIAN_POINT ( 'NONE',  ( 10.68058308266429890, 1480.421846638939996, 209.0069263140630085 ) ) ;
#98992 = CARTESIAN_POINT ( 'NONE',  ( -19.09472837541543555, 1485.512501651969160, 189.6337084803414541 ) ) ;
#98993 = CARTESIAN_POINT ( 'NONE',  ( -2.705330512559999789, 1443.650354199390222, 199.8402550512289793 ) ) ;
#98994 = CARTESIAN_POINT ( 'NONE',  ( -3.415238448984999842, 1511.775527460079957, 212.5370843810869985 ) ) ;
#98995 = CARTESIAN_POINT ( 'NONE',  ( 0.02089822245711980137, 1507.111760766699945, 237.3522839811660106 ) ) ;
#98996 = DIRECTION ( 'NONE',  ( 0.9532327469067780612, 0.2978772346122090520, -0.05115157206129060385 ) ) ;
#98997 = CARTESIAN_POINT ( 'NONE',  ( 2.154110967345579830, 1508.551704408389924, 219.6365568787950338 ) ) ;
#98998 = CARTESIAN_POINT ( 'NONE',  ( -50.19710983959630113, 1383.811588252980073, 261.7494256533389603 ) ) ;
#98999 = CARTESIAN_POINT ( 'NONE',  ( -5.139225489064998875, 1511.037966505499980, 201.4363886582769965 ) ) ;
#99000 = CARTESIAN_POINT ( 'NONE',  ( -12.61640430610000152, 1416.837080253930026, 194.9197996555979842 ) ) ;
#99001 = CARTESIAN_POINT ( 'NONE',  ( -11.58641202078170096, 1501.658531164619944, 208.7684197680320040 ) ) ;
#99002 = CARTESIAN_POINT ( 'NONE',  ( 1.348363903870000158, 1466.040058020430024, 235.1849732789979726 ) ) ;
#99005 = ORIENTED_EDGE ( 'NONE', *, *, #39902, .F. ) ;
#99004 = LINE ( 'NONE', #29072, #8566 ) ;
#99003 = B_SPLINE_CURVE_WITH_KNOTS ( 'NONE', 3,
 ( #57640, #92304, #25644, #42459, #67690, #33488, #32947, #23981, #59292, #58175, #40805, #93409, #74984, #8297, #16674, #8846, #41918, #15574, #43029, #83907, #67137, #92858, #41371, #34060, #58723 ),
 .UNSPECIFIED., .F., .F.,
 ( 4, 3, 3, 3, 3, 3, 3, 3, 4 ),
 ( 0.000000000000000000, 1.234047661610760072, 2.425972046132570448, 3.560296027315850154, 4.348419011639929721, 5.612354531546630554, 6.366473291553310432, 7.034225416716780366, 7.120592051560000080 ),
 .UNSPECIFIED. ) ;
#99006 = CARTESIAN_POINT ( 'NONE',  ( -0.8000066638249999640, 1450.880929917359936, 181.7283017618979954 ) ) ;
#99007 = CARTESIAN_POINT ( 'NONE',  ( -38.90243383290000168, 1381.518824974109975, 213.3883314898789934 ) ) ;
#99008 = CARTESIAN_POINT ( 'NONE',  ( 4.604592056516840337, 1508.551704408389924, 205.3031616744609948 ) ) ;
#99010 = ORIENTED_EDGE ( 'NONE', *, *, #37063, .T. ) ;
#99009 = CARTESIAN_POINT ( 'NONE',  ( -31.31962989722713786, 1525.556089352344770, 216.7000087461251212 ) ) ;
#99011 = CARTESIAN_POINT ( 'NONE',  ( 20.56231333760889868, 1477.111373227550075, 217.7195205697740050 ) ) ;
#99012 = ORIENTED_EDGE ( 'NONE', *, *, #54901, .T. ) ;
#99013 = CARTESIAN_POINT ( 'NONE',  ( -9.214005947760000481, 1389.265557518159994, 217.4246417548390014 ) ) ;
#99014 = CARTESIAN_POINT ( 'NONE',  ( -2.958097658349249759, 1515.068899390480283, 204.7924306805940091 ) ) ;
#99015 = DIRECTION ( 'NONE',  ( -0.3282391760791589785, 0.000000000000000000, -0.9445946449598763284 ) ) ;
#99016 = CIRCLE ( 'NONE', #50761, 2.000000000000059064 ) ;
#99017 = CARTESIAN_POINT ( 'NONE',  ( -17.71193100849139768, 1522.051704408389924, 221.5709757781449980 ) ) ;
#99018 = B_SPLINE_CURVE_WITH_KNOTS ( 'NONE', 3,
 ( #27254, #28358, #1516, #972, #62556, #35649, #103384, #77659, #18281, #35097, #19948, #52475 ),
 .UNSPECIFIED., .F., .F.,
 ( 4, 2, 2, 2, 2, 4 ),
 ( 0.000000000000000000, 0.0007194225121792270335, 0.001079133768269161528, 0.001438845024359096348, 0.002158267536538997864, 0.002877690048718900030 ),
 .UNSPECIFIED. ) ;
#99019 = CARTESIAN_POINT ( 'NONE',  ( -104.7943799579999933, 1379.906422268759798, 301.8989113051590039 ) ) ;
#99020 = LINE ( 'NONE', #81124, #103651 ) ;
#99021 = CARTESIAN_POINT ( 'NONE',  ( 19.59040869416958941, 1509.614908582205999, 186.9437411615208475 ) ) ;
#99022 = CARTESIAN_POINT ( 'NONE',  ( 12.66229353878289920, 1409.355237421249967, 201.1910009548570031 ) ) ;
#99023 = CARTESIAN_POINT ( 'NONE',  ( 0.6328050152959999730, 1408.935158425530062, 186.1228243921979981 ) ) ;
#99024 = CARTESIAN_POINT ( 'NONE',  ( 1.959361663749999982, 1419.250139722030099, 185.0399661677979850 ) ) ;
#99025 = CARTESIAN_POINT ( 'NONE',  ( -18.87607639370000001, 1452.025551963729868, 192.2339656219979815 ) ) ;
#99026 = CARTESIAN_POINT ( 'NONE',  ( -68.62428177750000202, 1379.748209670530059, 279.8484656398590005 ) ) ;
#99027 = CIRCLE ( 'NONE', #72293, 1.000000000000000888 ) ;
#99028 = DIRECTION ( 'NONE',  ( 0.2420316379589268763, -4.446049060781863124E-17, 0.9702683578407156340 ) ) ;
#99029 = ORIENTED_EDGE ( 'NONE', *, *, #2899, .F. ) ;
#99030 = ORIENTED_EDGE ( 'NONE', *, *, #108128, .T. ) ;
#99031 = CARTESIAN_POINT ( 'NONE',  ( -109.1642343328397260, 1384.919851393370436, 297.1325477198193425 ) ) ;
#99032 = CARTESIAN_POINT ( 'NONE',  ( 18.12943984651419882, 1457.942338673419954, 228.1937571059060019 ) ) ;
#99033 = CARTESIAN_POINT ( 'NONE',  ( -12.89823998259999982, 1434.736470928759900, 149.6930873346979922 ) ) ;
#99034 = CARTESIAN_POINT ( 'NONE',  ( 12.73828631345009832, 1420.788157922979963, 202.0023175873409969 ) ) ;
#99035 = CARTESIAN_POINT ( 'NONE',  ( -20.40237847379039948, 1501.463721599679957, 190.5751277017120060 ) ) ;
#99036 = FACE_BOUND ( 'NONE', #16171, .T. ) ;
#99037 = CARTESIAN_POINT ( 'NONE',  ( -109.2142229400000133, 1387.165659784040145, 310.9727364242590397 ) ) ;
#99038 = CARTESIAN_POINT ( 'NONE',  ( -7.580298022105069755, 1511.034527886640262, 215.0658449916730035 ) ) ;
#99039 = CARTESIAN_POINT ( 'NONE',  ( -10.68489437346363857, 1363.121218440984649, 210.6218459617030021 ) ) ;
#99040 = DIRECTION ( 'NONE',  ( 0.4794255386042096112, 0.000000000000000000, -0.8775825618903690950 ) ) ;
#99041 = CARTESIAN_POINT ( 'NONE',  ( -21.03123196750000190, 1507.789098030329797, 192.1781278414979965 ) ) ;
#99042 = CARTESIAN_POINT ( 'NONE',  ( 1.119592181715000079, 1516.958737650239982, 207.9859471464170326 ) ) ;
#99043 = CARTESIAN_POINT ( 'NONE',  ( -10.16501911979129957, 1447.237709317130111, 211.0287244977210150 ) ) ;
#99044 = CARTESIAN_POINT ( 'NONE',  ( 1.369523653644170169, 1408.899450504319930, 223.4949184458459968 ) ) ;
#99045 = CARTESIAN_POINT ( 'NONE',  ( -13.27386107244829994, 1434.917007507699964, 149.3091083363100040 ) ) ;
#99046 = CARTESIAN_POINT ( 'NONE',  ( -8.589998329009999267, 1385.225457215250117, 218.6546645165990128 ) ) ;
#99047 = CARTESIAN_POINT ( 'NONE',  ( 0.3641805758275279969, 1424.317995888269934, 227.5054904079770211 ) ) ;
#99048 = CARTESIAN_POINT ( 'NONE',  ( 7.216878188901039159, 1424.962458274039818, 212.8178266198389963 ) ) ;
#99049 = ORIENTED_EDGE ( 'NONE', *, *, #59577, .F. ) ;
#99050 = EDGE_CURVE ( 'NONE', #23316, #82812, #85427, .T. ) ;
#99051 = CARTESIAN_POINT ( 'NONE',  ( 31.44036153859999771, 1425.375771343829911, 254.7811647136979900 ) ) ;
#99052 = CARTESIAN_POINT ( 'NONE',  ( -1.546949757679999760, 1416.828040475729949, 228.0209010782980101 ) ) ;
#99054 = CARTESIAN_POINT ( 'NONE',  ( -15.21196350663329966, 1512.378201925209851, 222.0999656735410213 ) ) ;
#99053 = CARTESIAN_POINT ( 'NONE',  ( -11.65129296574880158, 1491.369970010279985, 206.7844079078949733 ) ) ;
#99055 = CARTESIAN_POINT ( 'NONE',  ( -5.513435595168334480, 1508.783371651738207, 216.5758637223831329 ) ) ;
#99056 = CARTESIAN_POINT ( 'NONE',  ( -12.77010823640000048, 1420.349902697730158, 231.7712046106979926 ) ) ;
#99057 = CARTESIAN_POINT ( 'NONE',  ( -29.70214828285509867, 1509.984309146039777, 208.0179991509364470 ) ) ;
#99058 = EDGE_CURVE ( 'NONE', #21837, #24662, #46163, .T. ) ;
#99059 = CARTESIAN_POINT ( 'NONE',  ( -17.05409589288600003, 1452.317518235730176, 146.2609911881839651 ) ) ;
#99060 = CARTESIAN_POINT ( 'NONE',  ( -18.96298731639999602, 1416.825532216530064, 208.0004950568580000 ) ) ;
#99061 = ORIENTED_EDGE ( 'NONE', *, *, #85403, .F. ) ;
#99062 = CARTESIAN_POINT ( 'NONE',  ( -108.1236415588580115, 1378.913060387289988, 299.8223284637080610 ) ) ;
#99063 = CARTESIAN_POINT ( 'NONE',  ( -3.180365954794715400, 1370.226539215816501, 210.2066197577219100 ) ) ;
#99064 = CARTESIAN_POINT ( 'NONE',  ( 14.30536690592939841, 1421.516539548159926, 228.9956906566140162 ) ) ;
#99065 = ORIENTED_EDGE ( 'NONE', *, *, #32198, .T. ) ;
#99066 = VERTEX_POINT ( 'NONE', #102086 ) ;
#99067 = CARTESIAN_POINT ( 'NONE',  ( 9.695032739815491851, 1452.327451679549995, 210.0352081693090156 ) ) ;
#99068 = CARTESIAN_POINT ( 'NONE',  ( 6.577796586379999866, 1424.576947660639917, 193.8008614473990008 ) ) ;
#99069 = ORIENTED_EDGE ( 'NONE', *, *, #56834, .T. ) ;
#99070 = CARTESIAN_POINT ( 'NONE',  ( 4.987081042841619904, 1508.551704408389924, 205.1632167381339968 ) ) ;
#99071 = LINE ( 'NONE', #90124, #15163 ) ;
#99072 = DIRECTION ( 'NONE',  ( 0.02546698206423540778, -0.0008893270957687149847, -0.9996752682355689590 ) ) ;
#99073 = CARTESIAN_POINT ( 'NONE',  ( 5.519893427111519202, 1440.499866072189889, 154.7645221071819890 ) ) ;
#99074 = ORIENTED_EDGE ( 'NONE', *, *, #32367, .F. ) ;
#99075 = CARTESIAN_POINT ( 'NONE',  ( 45.82909222224540002, 1446.182179057269877, 267.6052008258039905 ) ) ;
#99076 = CARTESIAN_POINT ( 'NONE',  ( -13.15726442270000085, 1416.851343897030119, 221.9096085505980227 ) ) ;
#99077 = CARTESIAN_POINT ( 'NONE',  ( -7.973546373919998764, 1425.245985973290090, 205.1887633420689667 ) ) ;
#99078 =( BOUNDED_CURVE ( )  B_SPLINE_CURVE ( 3, ( #82916, #73982, #99701, #40359 ),
 .UNSPECIFIED., .F., .F. ) 
 B_SPLINE_CURVE_WITH_KNOTS ( ( 4, 4 ),
 ( 2.436781329611982017, 3.141592653589793116 ),
 .UNSPECIFIED. ) 
 CURVE ( )  GEOMETRIC_REPRESENTATION_ITEM ( )  RATIONAL_B_SPLINE_CURVE ( ( 1.000000000000000000, 0.9590300661663084814, 0.9590300661663084814, 1.000000000000000000 ) ) 
 REPRESENTATION_ITEM ( '' )  );
#99079 = CARTESIAN_POINT ( 'NONE',  ( 4.611879685325000366, 1516.858533673840157, 204.4999481076869756 ) ) ;
#99080 = EDGE_CURVE ( 'NONE', #43475, #22743, #94369, .T. ) ;
#99081 = ORIENTED_EDGE ( 'NONE', *, *, #7673, .F. ) ;
#99082 = LINE ( 'NONE', #3969, #40127 ) ;
#99083 = CARTESIAN_POINT ( 'NONE',  ( 13.51514909825042565, 1443.972136820036440, 188.0277010184605899 ) ) ;
#99084 = EDGE_LOOP ( 'NONE', ( #41466, #8470, #99005, #3497 ) ) ;
#99085 = ORIENTED_EDGE ( 'NONE', *, *, #34595, .F. ) ;
#99086 = CARTESIAN_POINT ( 'NONE',  ( 2.911802205207963734, 1507.562757914708527, 220.4805861716940001 ) ) ;
#99087 = DIRECTION ( 'NONE',  ( -1.238073365138532047E-30, 1.000000000000000000, -6.123233995736639079E-17 ) ) ;
#99088 = CARTESIAN_POINT ( 'NONE',  ( -4.324698967714178721, 1424.665291916374827, 185.8068982220774217 ) ) ;
#99089 = CARTESIAN_POINT ( 'NONE',  ( 10.06559049306389930, 1452.561562221930217, 150.5716378858789994 ) ) ;
#99090 = CARTESIAN_POINT ( 'NONE',  ( -1.726328313212220289E-05, 1407.650947845630071, 270.1377426662980383 ) ) ;
#99091 = CARTESIAN_POINT ( 'NONE',  ( 33.91369968912619726, 1451.728767897860052, 134.7155302171979940 ) ) ;
#99092 = CARTESIAN_POINT ( 'NONE',  ( -109.1299347229319210, 1382.116777868800455, 297.5434349749086778 ) ) ;
#99093 = CARTESIAN_POINT ( 'NONE',  ( -10.97860844464990038, 1432.885878357189995, 151.7696306460070161 ) ) ;
#99094 = VECTOR ( 'NONE', #73896, 1000.000000000000000 ) ;
#99095 = DIRECTION ( 'NONE',  ( 0.000000000000000000, 0.000000000000000000, -1.000000000000000000 ) ) ;
#99097 = CARTESIAN_POINT ( 'NONE',  ( -106.5186017514349999, 1391.553736368970021, 307.6918517192190166 ) ) ;
#99096 = CARTESIAN_POINT ( 'NONE',  ( -16.66101146819999812, 1410.867390116229899, 191.7375337716979971 ) ) ;
#99098 = CARTESIAN_POINT ( 'NONE',  ( 10.67506506432800073, 1424.493056960179956, 206.5997893278160120 ) ) ;
#99099 = CARTESIAN_POINT ( 'NONE',  ( -24.23681317631879750, 1508.759042070240184, 222.4186787974370247 ) ) ;
#99100 = CARTESIAN_POINT ( 'NONE',  ( 9.634835741540001663, 1430.981823154709900, 148.7079730222979776 ) ) ;
#99101 = ORIENTED_EDGE ( 'NONE', *, *, #37770, .F. ) ;
#99102 = CARTESIAN_POINT ( 'NONE',  ( 20.41675352909999930, 1438.655740921959932, 219.6133833292979887 ) ) ;
#99103 = AXIS2_PLACEMENT_3D ( 'NONE', #80594, #71122, #105243 ) ;
#99104 = CARTESIAN_POINT ( 'NONE',  ( -0.2232534084008130082, 1424.263167169779990, 227.7533338486369985 ) ) ;
#99105 = CARTESIAN_POINT ( 'NONE',  ( -79.55893548068129917, 1384.995123410919859, 303.5731928006850353 ) ) ;
#99106 = B_SPLINE_SURFACE_WITH_KNOTS ( 'NONE', 5, 4, ( 
 ( #68105, #3663, #10936, #28281, #37792 ),
 ( #106632, #73049, #20960, #45666, #12583 ),
 ( #70878, #104989, #19867, #62476, #54616 ),
 ( #30479, #21502, #64112, #28840, #98233 ),
 ( #97687, #2561, #71980, #107190, #89287 ),
 ( #46764, #46212, #4191, #80894, #79252 ) ),
 .UNSPECIFIED., .F., .F., .F.,
 ( 6, 6 ),
 ( 5, 5 ),
 ( 0.000000000000000000, 111.1101480259999903 ),
 ( 25.81581217359999769, 39.03307591160000101 ),
 .UNSPECIFIED. ) ;
#99107 = CARTESIAN_POINT ( 'NONE',  ( -8.998777790820000178, 1385.475401132710203, 199.9682204879490257 ) ) ;
#99108 = CARTESIAN_POINT ( 'NONE',  ( 10.17360721298319959, 1426.903618366670116, 209.4281458372120142 ) ) ;
#99110 = ORIENTED_EDGE ( 'NONE', *, *, #63930, .F. ) ;
#99109 = CARTESIAN_POINT ( 'NONE',  ( -15.83960918336639878, 1420.111814593369900, 210.7068784591650115 ) ) ;
#99111 = CARTESIAN_POINT ( 'NONE',  ( 3.661554943190000078, 1428.528251320389927, 216.5381528549790175 ) ) ;
#99112 = CARTESIAN_POINT ( 'NONE',  ( -7.544733521240000407, 1384.899971913130003, 219.0877090842990071 ) ) ;
#99113 = CARTESIAN_POINT ( 'NONE',  ( -14.20190154360000179, 1416.831305866930279, 221.7380342762980092 ) ) ;
#99114 = CARTESIAN_POINT ( 'NONE',  ( 11.28251112829999947, 1433.921144945409878, 151.5399218156979941 ) ) ;
#99115 = CARTESIAN_POINT ( 'NONE',  ( -11.60004869885203682, 1425.894669202444675, 137.5118601406020673 ) ) ;
#99116 = CARTESIAN_POINT ( 'NONE',  ( 12.48769551257159982, 1414.971717244360207, 197.6617324145900056 ) ) ;
#99117 = CARTESIAN_POINT ( 'NONE',  ( 1.779422250252779891, 1456.357346840630044, 198.6855212002049882 ) ) ;
#99118 = CARTESIAN_POINT ( 'NONE',  ( 7.479166282266099586, 1423.852740058520112, 195.4333272129960051 ) ) ;
#99119 = CARTESIAN_POINT ( 'NONE',  ( 13.65755722549999973, 1419.762562827630063, 228.6500612441979854 ) ) ;
#99120 = CARTESIAN_POINT ( 'NONE',  ( -31.55060375016910257, 1525.712835404586031, 201.2105082957782543 ) ) ;
#99121 = CYLINDRICAL_SURFACE ( 'NONE', #52063, 4.000000000000003553 ) ;
#99122 = CYLINDRICAL_SURFACE ( 'NONE', #98305, 1.999999999999999556 ) ;
#99123 = CARTESIAN_POINT ( 'NONE',  ( -0.5639001407619999018, 1420.522959561429843, 227.9306795899979932 ) ) ;
#99124 = CARTESIAN_POINT ( 'NONE',  ( -26.97127426239999792, 1450.931412349030097, 136.4066425356980119 ) ) ;
#99125 = CARTESIAN_POINT ( 'NONE',  ( 21.54890432409654011, 1524.816846803860471, 183.6629423615462429 ) ) ;
#99126 = CARTESIAN_POINT ( 'NONE',  ( 12.61566547299999996, 1416.819759814730105, 223.3235036042979971 ) ) ;
#99127 = FACE_OUTER_BOUND ( 'NONE', #43687, .T. ) ;
#99128 = LINE ( 'NONE', #82896, #52776 ) ;
#99129 = CARTESIAN_POINT ( 'NONE',  ( -7.803087493140000497, 1414.971262582530017, 223.9800507790980362 ) ) ;
#99130 = TOROIDAL_SURFACE ( 'NONE', #79510, 12.73448142120000171, 1.000000000000000000 ) ;
#99131 = CARTESIAN_POINT ( 'NONE',  ( 0.2091846300955290117, 1457.806774526239906, 183.0471825358959848 ) ) ;
#99132 = B_SPLINE_CURVE_WITH_KNOTS ( 'NONE', 3,
 ( #101684, #59721, #61396, #50226 ),
 .UNSPECIFIED., .F., .F.,
 ( 4, 4 ),
 ( 0.000000000000000000, 1.000000000000000000 ),
 .UNSPECIFIED. ) ;
#99133 = CARTESIAN_POINT ( 'NONE',  ( -8.860300303135609568, 1407.578384618130031, 199.4146916745189912 ) ) ;
#99134 = CARTESIAN_POINT ( 'NONE',  ( -12.85971948620000127, 1415.932840167130053, 196.7491045163979777 ) ) ;
#99135 = CARTESIAN_POINT ( 'NONE',  ( -28.30972139877570015, 1509.473640034179880, 210.9653718159219977 ) ) ;
#99136 = CARTESIAN_POINT ( 'NONE',  ( 12.40421625309999953, 1434.420021183800145, 148.5016035624979907 ) ) ;
#99137 = CARTESIAN_POINT ( 'NONE',  ( -28.14146986589999955, 1435.479030298939961, 135.6828298310979903 ) ) ;
#99138 = CARTESIAN_POINT ( 'NONE',  ( 8.709291548640001324, 1441.011683078770147, 186.3963333776979709 ) ) ;
#99139 = ORIENTED_EDGE ( 'NONE', *, *, #31923, .F. ) ;
#99140 = CARTESIAN_POINT ( 'NONE',  ( -16.92737834736502833, 1525.317349363549965, 181.4495812669162831 ) ) ;
#99141 = CARTESIAN_POINT ( 'NONE',  ( -2.919110404717550011, 1368.384062535930070, 207.8228080779019820 ) ) ;
#99142 = CARTESIAN_POINT ( 'NONE',  ( -103.7837470130642856, 1380.040681755203195, 305.7727476933569051 ) ) ;
#99143 = CARTESIAN_POINT ( 'NONE',  ( 5.923682464646780943, 1517.051704408389924, 194.3813127491490036 ) ) ;
#99144 = CARTESIAN_POINT ( 'NONE',  ( -0.8597107442289990686, 1463.363299246390170, 202.2013017290789776 ) ) ;
#99145 = DIRECTION ( 'NONE',  ( 0.000000000000000000, 1.000000000000000000, 0.000000000000000000 ) ) ;
#99146 = CARTESIAN_POINT ( 'NONE',  ( 31.88106177436622701, 1416.458733636820853, 269.3181919498966295 ) ) ;
#99147 = CARTESIAN_POINT ( 'NONE',  ( -17.29882006758053592, 1523.542365884048650, 237.3908737315615269 ) ) ;
#99148 = CARTESIAN_POINT ( 'NONE',  ( 20.15452300067990166, 1507.845791525220193, 189.3412703910400126 ) ) ;
#99149 = CARTESIAN_POINT ( 'NONE',  ( -4.219439073160000220, 1441.595895977600094, 177.0328731553979935 ) ) ;
#99150 = CARTESIAN_POINT ( 'NONE',  ( -57.51883745420190053, 1385.049604656559950, 238.7888358578429973 ) ) ;
#99151 = CARTESIAN_POINT ( 'NONE',  ( -12.25211328800230071, 1490.425571931200011, 208.9817620660529940 ) ) ;
#99152 = CARTESIAN_POINT ( 'NONE',  ( -27.79585007420000053, 1451.789558028530109, 135.7670632556980195 ) ) ;
#99153 = CARTESIAN_POINT ( 'NONE',  ( 41.66134420550000073, 1443.796851579070108, 135.6885409488979803 ) ) ;
#99154 = CARTESIAN_POINT ( 'NONE',  ( -15.86684091882549907, 1409.475427479080281, 225.4728633087160006 ) ) ;
#99156 = VERTEX_POINT ( 'NONE', #70751 ) ;
#99155 = CARTESIAN_POINT ( 'NONE',  ( 0.4983054691675419257, 1414.932839379760026, 184.8741889412040393 ) ) ;
#99157 = CARTESIAN_POINT ( 'NONE',  ( -109.3073322039999908, 1384.904126850409966, 311.2647055142589920 ) ) ;
#99158 = CARTESIAN_POINT ( 'NONE',  ( 9.861354742171270615, 1470.940182288200049, 211.9688742596949851 ) ) ;
#99159 = CARTESIAN_POINT ( 'NONE',  ( -22.11218108847071306, 1411.043597553445352, 214.4701686222656178 ) ) ;
#99160 = CARTESIAN_POINT ( 'NONE',  ( -109.9871902949999907, 1384.855229205870046, 311.4556902802589775 ) ) ;
#99161 = CARTESIAN_POINT ( 'NONE',  ( -0.09623828610459078670, 1420.380023493850103, 183.2616177384549871 ) ) ;
#99162 = CARTESIAN_POINT ( 'NONE',  ( 1.108178853160000088, 1466.523263909929938, 235.2969450623980094 ) ) ;
#99163 = CARTESIAN_POINT ( 'NONE',  ( 22.66638050679999949, 1410.625956981130230, 214.3745493218679883 ) ) ;
#99164 = DIRECTION ( 'NONE',  ( -0.07035059757514136591, -0.9966174162490445410, -0.04247963100003462888 ) ) ;
#99165 = CARTESIAN_POINT ( 'NONE',  ( -16.59693199761399995, 1464.025901459640181, 220.5208652158270013 ) ) ;
#99166 = CARTESIAN_POINT ( 'NONE',  ( -17.67465541829999864, 1423.538376080030048, 226.2965632852980207 ) ) ;
#99168 = CARTESIAN_POINT ( 'NONE',  ( 9.638115859575000499, 1517.051704408389924, 214.4931927712770232 ) ) ;
#99167 = CARTESIAN_POINT ( 'NONE',  ( 3.862828020359158732, 1497.382717227735611, 197.2227926766582300 ) ) ;
#99169 = CARTESIAN_POINT ( 'NONE',  ( 27.41515664521250173, 1488.740012672480134, 209.4249987372610065 ) ) ;
#99170 = CARTESIAN_POINT ( 'NONE',  ( -106.4559248862600214, 1358.631207110789319, 305.9949594761371827 ) ) ;
#99171 = FACE_OUTER_BOUND ( 'NONE', #78904, .T. ) ;
#99172 = CARTESIAN_POINT ( 'NONE',  ( -0.9621744844780000250, 1415.477225457230134, 233.2860938207980155 ) ) ;
#99173 = AXIS2_PLACEMENT_3D ( 'NONE', #78175, #61968, #70929 ) ;
#99174 = CARTESIAN_POINT ( 'NONE',  ( -5.099447121353800405, 1375.125474032349985, 203.4873467743369986 ) ) ;
#99175 = CARTESIAN_POINT ( 'NONE',  ( -3.460101890015000237, 1516.812923327049930, 205.0932153474469715 ) ) ;
#99176 = CARTESIAN_POINT ( 'NONE',  ( -11.36618588219640102, 1485.531419837760041, 185.0615275845599967 ) ) ;
#99177 = ORIENTED_EDGE ( 'NONE', *, *, #26089, .T. ) ;
#99178 = VECTOR ( 'NONE', #81214, 1000.000000000000000 ) ;
#99179 = CARTESIAN_POINT ( 'NONE',  ( -32.38114538885245963, 1523.604703353109699, 216.1203639561433647 ) ) ;
#99180 = CARTESIAN_POINT ( 'NONE',  ( -4.242759794694189956, 1441.416754616080198, 162.3033463234470162 ) ) ;
#99181 = AXIS2_PLACEMENT_3D ( 'NONE', #98994, #48633, #66545 ) ;
#99183 = ORIENTED_EDGE ( 'NONE', *, *, #83786, .T. ) ;
#99182 = CARTESIAN_POINT ( 'NONE',  ( -68.44821854895280921, 1379.747450488880077, 280.0214965132619795 ) ) ;
#99184 = ORIENTED_EDGE ( 'NONE', *, *, #74895, .F. ) ;
#99185 = CARTESIAN_POINT ( 'NONE',  ( -11.01457153678066980, 1378.540399413372143, 214.6712006714588199 ) ) ;
#99186 = ORIENTED_EDGE ( 'NONE', *, *, #9671, .F. ) ;
#99187 = CARTESIAN_POINT ( 'NONE',  ( -1.583985751884120052, 1486.289433825739934, 220.9322661043319727 ) ) ;
#99188 = CARTESIAN_POINT ( 'NONE',  ( 11.51819234920000135, 1500.360414606190034, 206.3631727204690094 ) ) ;
#99190 = CARTESIAN_POINT ( 'NONE',  ( 1.446896864630000001, 1507.663901920830085, 181.0890709196980026 ) ) ;
#99189 = CARTESIAN_POINT ( 'NONE',  ( -10.82182428428866672, 1424.917064109405146, 144.5864024659527729 ) ) ;
#99191 = CARTESIAN_POINT ( 'NONE',  ( -7.713648872314999849, 1516.710624944440042, 209.8745175203999906 ) ) ;
#99192 = CARTESIAN_POINT ( 'NONE',  ( -24.86261486476140092, 1452.044834405480060, 135.5980773263869992 ) ) ;
#99193 = CARTESIAN_POINT ( 'NONE',  ( -11.73709356449999852, 1426.695943566229971, 144.1748013792980032 ) ) ;
#99194 = CARTESIAN_POINT ( 'NONE',  ( 3.556995324409999881, 1476.475065048189890, 198.0947962222990100 ) ) ;
#99195 = CARTESIAN_POINT ( 'NONE',  ( 11.55223054067229960, 1480.217571523739934, 211.4788428327300380 ) ) ;
#99196 = DIRECTION ( 'NONE',  ( 1.000000000000000000, 0.000000000000000000, 0.000000000000000000 ) ) ;
#99197 = PRODUCT_DEFINITION_SHAPE ( 'NONE', 'NONE',  #110836 ) ;
#99198 = LINE ( 'NONE', #49925, #64156 ) ;
#99199 = CARTESIAN_POINT ( 'NONE',  ( -39.65801192383619167, 1440.831642379499954, 136.8099676560480020 ) ) ;
#99200 = CARTESIAN_POINT ( 'NONE',  ( -17.55008888309999904, 1487.029577685089862, 194.9701234138989889 ) ) ;
#99201 = CARTESIAN_POINT ( 'NONE',  ( -1.955843867788469970, 1431.363043548789847, 200.9645343544800085 ) ) ;
#99202 = ORIENTED_EDGE ( 'NONE', *, *, #20631, .F. ) ;
#99203 = EDGE_LOOP ( 'NONE', ( #57494, #50721, #86523, #75015 ) ) ;
#99204 = CARTESIAN_POINT ( 'NONE',  ( 10.66111875780481633, 1410.659669277416242, 229.5690789417564019 ) ) ;
#99205 = CARTESIAN_POINT ( 'NONE',  ( 16.30010422171099904, 1514.508970265533890, 194.3992361457187599 ) ) ;
#99206 = CARTESIAN_POINT ( 'NONE',  ( 0.04542731285949999642, 1451.694725257930031, 183.0340308383979959 ) ) ;
#99207 = CARTESIAN_POINT ( 'NONE',  ( -3.311547598719999819, 1485.996598843729998, 182.1826784800979908 ) ) ;
#99208 = CARTESIAN_POINT ( 'NONE',  ( -2.500000000000199840, 1439.253552895449957, 159.5302512421249901 ) ) ;
#99209 = CARTESIAN_POINT ( 'NONE',  ( -3.347801439296148818, 1523.382868172864164, 242.0893193391992497 ) ) ;
#99210 = CARTESIAN_POINT ( 'NONE',  ( -67.63660556605692875, 1379.745626871633021, 277.6924153040722558 ) ) ;
#99211 = CARTESIAN_POINT ( 'NONE',  ( -5.100957845159999948, 1482.122785942490054, 228.9672709512990139 ) ) ;
#99212 = CIRCLE ( 'NONE', #81318, 1.999999999999999556 ) ;
#99213 = CARTESIAN_POINT ( 'NONE',  ( 28.28208337139999884, 1508.151294399930066, 209.1094497554269935 ) ) ;
#99214 = CARTESIAN_POINT ( 'NONE',  ( 12.51099981729999833, 1416.825784011830137, 196.0986189375979905 ) ) ;
#99215 = CARTESIAN_POINT ( 'NONE',  ( -75.71374782820129212, 1384.771513434549888, 276.6754848879950259 ) ) ;
#99216 = EDGE_LOOP ( 'NONE', ( #68551, #55468, #26930, #57145 ) ) ;
#99217 = CARTESIAN_POINT ( 'NONE',  ( 3.260357128764999946, 1517.133889586189980, 201.3971135232069969 ) ) ;
#99218 = CARTESIAN_POINT ( 'NONE',  ( 4.610079833424999940, 1516.713079096360161, 207.9883289669969884 ) ) ;
#99219 = ORIENTED_EDGE ( 'NONE', *, *, #80073, .T. ) ;
#99220 = CARTESIAN_POINT ( 'NONE',  ( 11.03427950888080211, 1414.913526845469960, 222.2765582366960189 ) ) ;
#99221 = CARTESIAN_POINT ( 'NONE',  ( -0.0002585518234266428279, 1452.563254695420028, 153.5184766442947080 ) ) ;
#99222 = EDGE_LOOP ( 'NONE', ( #62630, #51581, #23805, #43143 ) ) ;
#99223 = CARTESIAN_POINT ( 'NONE',  ( -17.22845782853304542, 1525.848196786131211, 181.7617168241399952 ) ) ;
#99224 = CARTESIAN_POINT ( 'NONE',  ( -15.04452981080000029, 1409.438426944829871, 191.9174468092980135 ) ) ;
#99225 = CARTESIAN_POINT ( 'NONE',  ( -14.01398736212220086, 1379.590348564800024, 211.9184487047760115 ) ) ;
#99226 = CARTESIAN_POINT ( 'NONE',  ( -16.99050533527280038, 1420.323706995179919, 203.8408272025779979 ) ) ;
#99227 = CARTESIAN_POINT ( 'NONE',  ( -8.672201264859550562, 1436.845892416930155, 213.7190775223999992 ) ) ;
#99228 = DIRECTION ( 'NONE',  ( 0.6205445805634681733, -0.7071067811868638753, -0.3390050494208928233 ) ) ;
#99229 = CARTESIAN_POINT ( 'NONE',  ( -2.197413446379999691, 1507.220826626529970, 180.8381795196980022 ) ) ;
#99230 = CARTESIAN_POINT ( 'NONE',  ( -6.288919133997779021, 1510.947107049704073, 201.6929532012474340 ) ) ;
#99232 = EDGE_CURVE ( 'NONE', #36566, #36154, #24949, .T. ) ;
#99231 = CARTESIAN_POINT ( 'NONE',  ( -22.14913372576182127, 1525.402221411349728, 182.5746398196750988 ) ) ;
#99234 = CARTESIAN_POINT ( 'NONE',  ( -11.60004869884504686, 1423.657758649147581, 137.0691908906612753 ) ) ;
#99233 = CARTESIAN_POINT ( 'NONE',  ( 11.86013743380000030, 1462.256145969930003, 232.2216276054980142 ) ) ;
#99235 = B_SPLINE_CURVE_WITH_KNOTS ( 'NONE', 2,
 ( #87418, #27498, #10714, #95263, #1779 ),
 .UNSPECIFIED., .F., .F.,
 ( 3, 2, 3 ),
 ( 0.000000000000000000, 0.5000000000000000000, 1.000000000000000000 ),
 .UNSPECIFIED. ) ;
#99236 = CARTESIAN_POINT ( 'NONE',  ( -0.1562295872588534418, 1410.302064320732597, 233.2305516458151828 ) ) ;
#99237 = B_SPLINE_SURFACE_WITH_KNOTS ( 'NONE', 5, 5, ( 
 ( #68178, #100628, #102285, #109061, #25566, #51338, #32344, #66524, #41294 ),
 ( #75468, #109602, #101170, #53019, #87154, #18273, #2626, #52466, #37310 ),
 ( #105062, #61984, #88262, #19375, #53578, #87725, #1507, #95005, #79316 ),
 ( #86596, #77651, #11003, #63103, #45175, #2072, #36203, #11555, #43507 ),
 ( #35638, #36752, #78757, #70944, #70387, #62546, #9888, #45732, #44056 ),
 ( #78196, #104504, #965, #69832, #28351, #97200, #28908, #20473, #103949 ) ),
 .UNSPECIFIED., .F., .F., .F.,
 ( 6, 6 ),
 ( 6, 3, 6 ),
 ( 0.4666582265029999843, 2.797885342349890170 ),
 ( -1.082959988738329909E-05, 1.000000000000000000, 2.000000000000000000 ),
 .UNSPECIFIED. ) ;
#99238 = CARTESIAN_POINT ( 'NONE',  ( 3.261007131564999995, 1516.596789218710001, 216.4445556570670135 ) ) ;
#99239 = FACE_OUTER_BOUND ( 'NONE', #86807, .T. ) ;
#99240 = CARTESIAN_POINT ( 'NONE',  ( -0.1052129130517930056, 1508.249961362639851, 180.4882525773680015 ) ) ;
#99241 = CARTESIAN_POINT ( 'NONE',  ( 2.255244433210603638, 1516.528169492436291, 216.8307170402573831 ) ) ;
#99242 = CARTESIAN_POINT ( 'NONE',  ( 1.134357970594999987, 1516.744381837270112, 213.1504571913470159 ) ) ;
#99243 = CARTESIAN_POINT ( 'NONE',  ( 4.259777688362279768, 1515.374151772610048, 212.0586625277509825 ) ) ;
#99244 = CARTESIAN_POINT ( 'NONE',  ( -2.171184902437989894, 1483.765132005870100, 198.6683033559409921 ) ) ;
#99246 = EDGE_LOOP ( 'NONE', ( #89595, #104447, #90964, #56947, #28277 ) ) ;
#99245 = CARTESIAN_POINT ( 'NONE',  ( 3.487587102937319994, 1509.038630944639863, 213.6090953401219963 ) ) ;
#99247 = CARTESIAN_POINT ( 'NONE',  ( -2.390047989678332208, 1526.069472839386663, 177.7067300826772964 ) ) ;
#99248 = CARTESIAN_POINT ( 'NONE',  ( 1.909107468240000216, 1507.666028269690059, 220.7249166300989884 ) ) ;
#99249 = CARTESIAN_POINT ( 'NONE',  ( -11.30047077689999924, 1432.243567658440043, 151.5215873816980263 ) ) ;
#99250 = CARTESIAN_POINT ( 'NONE',  ( 4.208240993269999564, 1434.939300248989866, 227.0651965576989824 ) ) ;
#99251 = B_SPLINE_CURVE_WITH_KNOTS ( 'NONE', 5,
 ( #31432, #81829, #39289, #82404, #73463, #74008, #56655, #25082, #33482, #98086, #107594, #108139 ),
 .UNSPECIFIED., .F., .F.,
 ( 6, 3, 3, 6 ),
 ( -18.25602225929999989, -13.68355489660000046, -9.538385084389998880, -6.066676742310001202 ),
 .UNSPECIFIED. ) ;
#99252 = CARTESIAN_POINT ( 'NONE',  ( -8.519718778234439682, 1440.842058268650135, 204.6679085666960134 ) ) ;
#99253 = CARTESIAN_POINT ( 'NONE',  ( 6.413908346207559674, 1429.087432367279916, 154.6253934533610277 ) ) ;
#99254 = CARTESIAN_POINT ( 'NONE',  ( 11.81780673814840021, 1517.151704408390060, 195.5270144474869767 ) ) ;
#99255 = CARTESIAN_POINT ( 'NONE',  ( -9.119413322219999785, 1439.059527644790023, 208.3668177869740248 ) ) ;
#99257 = CARTESIAN_POINT ( 'NONE',  ( -21.10083498417930059, 1505.340688622180096, 209.5899059317720230 ) ) ;
#99256 = CARTESIAN_POINT ( 'NONE',  ( -18.79847754549999905, 1457.450606964430108, 227.1476812467979869 ) ) ;
#99258 = CARTESIAN_POINT ( 'NONE',  ( -1.783662796859999844, 1484.717543678729953, 182.7833423215980133 ) ) ;
#99259 = ORIENTED_EDGE ( 'NONE', *, *, #83400, .T. ) ;
#99260 = CARTESIAN_POINT ( 'NONE',  ( -6.560742263465000335, 1517.028034847769959, 205.0881926677770082 ) ) ;
#99261 = CARTESIAN_POINT ( 'NONE',  ( 9.884505093230000483, 1406.768685218130031, 266.9235441556980390 ) ) ;
#99262 = FACE_OUTER_BOUND ( 'NONE', #21653, .T. ) ;
#99263 = CARTESIAN_POINT ( 'NONE',  ( 20.10957645199999888, 1410.870268510630012, 197.6120402619980041 ) ) ;
#99264 = ADVANCED_FACE ( 'NONE', ( #20838 ), #45695, .F. ) ;
#99265 = CARTESIAN_POINT ( 'NONE',  ( 24.58038383556951700, 1439.418613111171453, 212.5155431820280683 ) ) ;
#99266 = EDGE_CURVE ( 'NONE', #54755, #110792, #12099, .T. ) ;
#99267 = CARTESIAN_POINT ( 'NONE',  ( 10.37019963556298841, 1423.186367574259748, 137.2231398063942436 ) ) ;
#99268 = EDGE_CURVE ( 'NONE', #80633, #104047, #22165, .T. ) ;
#99269 = CARTESIAN_POINT ( 'NONE',  ( 4.363122647530000009, 1421.075575420230052, 170.1076616725979989 ) ) ;
#99270 = CARTESIAN_POINT ( 'NONE',  ( -1.981093173629999926, 1450.324655959600022, 155.6080925165979920 ) ) ;
#99271 = CARTESIAN_POINT ( 'NONE',  ( -7.211414364699999524, 1427.415731310709816, 205.0259060341190320 ) ) ;
#99272 = ADVANCED_FACE ( 'NONE', ( #56669 ), #58893, .T. ) ;
#99273 = CARTESIAN_POINT ( 'NONE',  ( -19.84490639471488649, 1485.616324373336283, 190.5157334858500633 ) ) ;
#99274 = ADVANCED_FACE ( 'NONE', ( #63301 ), #108328, .T. ) ;
#99275 = CARTESIAN_POINT ( 'NONE',  ( -1.951848414609999915, 1509.046756045790062, 220.7383877411990056 ) ) ;
#99276 = CARTESIAN_POINT ( 'NONE',  ( -3.970093244310000102, 1515.569676282289947, 210.2462954219890037 ) ) ;
#99277 = CARTESIAN_POINT ( 'NONE',  ( 8.881784197000000993E-16, 1412.362567936729874, 265.6112251771979800 ) ) ;
#99278 = CARTESIAN_POINT ( 'NONE',  ( 3.330134165755000097, 1515.051704408389924, 204.7920544413669859 ) ) ;
#99279 = CARTESIAN_POINT ( 'NONE',  ( 4.222563055010000177, 1441.596179668460081, 170.5493975461980085 ) ) ;
#99280 = CARTESIAN_POINT ( 'NONE',  ( -2.112521956910000220, 1476.073962097629874, 267.8521519262979496 ) ) ;
#99281 = CARTESIAN_POINT ( 'NONE',  ( -10.73514658959810752, 1424.973046406437561, 139.1354236156141724 ) ) ;
#99282 = CARTESIAN_POINT ( 'NONE',  ( -5.360152366205530150, 1422.242722016050038, 144.1549655170190078 ) ) ;
#99283 = CARTESIAN_POINT ( 'NONE',  ( -11.67151907566795366, 1486.510180171227375, 184.2271218764052776 ) ) ;
#99284 = CARTESIAN_POINT ( 'NONE',  ( -31.70262514495150086, 1384.822076339110254, 229.9359219034049886 ) ) ;
#99285 = CARTESIAN_POINT ( 'NONE',  ( -106.4316804820100089, 1391.913060387289988, 303.6209942796789960 ) ) ;
#99286 = CARTESIAN_POINT ( 'NONE',  ( -21.13622131300000007, 1506.830164498290060, 213.5433617895989755 ) ) ;
#99287 = CARTESIAN_POINT ( 'NONE',  ( -105.6089689389999933, 1379.039522535980041, 302.3092273913590020 ) ) ;
#99288 = CARTESIAN_POINT ( 'NONE',  ( -20.49599333844887639, 1525.960063244516959, 184.3798832129037351 ) ) ;
#99289 = CARTESIAN_POINT ( 'NONE',  ( 7.943217798846315958, 1511.827406192408489, 205.9421500790769528 ) ) ;
#99290 = VECTOR ( 'NONE', #109077, 1000.000000000000000 ) ;
#99291 = CARTESIAN_POINT ( 'NONE',  ( -22.68024642580000005, 1410.626440472329932, 203.9056876081779990 ) ) ;
#99292 = EDGE_CURVE ( 'NONE', #508, #8596, #67631, .T. ) ;
#99293 = CARTESIAN_POINT ( 'NONE',  ( -15.03439673157799916, 1422.460132116142177, 229.1221540998959938 ) ) ;
#99294 = CARTESIAN_POINT ( 'NONE',  ( 31.81407709660769001, 1522.382868172863937, 196.2902540610627682 ) ) ;
#99295 = ORIENTED_EDGE ( 'NONE', *, *, #88439, .F. ) ;
#99296 = CARTESIAN_POINT ( 'NONE',  ( -6.821020807950000098, 1472.286670839089766, 210.4001276167389847 ) ) ;
#99298 = EDGE_CURVE ( 'NONE', #47608, #3729, #42470, .T. ) ;
#99297 = CARTESIAN_POINT ( 'NONE',  ( -7.550704986171106192, 1510.491946833609973, 214.7158011863163836 ) ) ;
#99299 = CARTESIAN_POINT ( 'NONE',  ( 18.94655734006379788, 1455.761339616339910, 200.3458083268320138 ) ) ;
#99301 = CARTESIAN_POINT ( 'NONE',  ( -12.86192383983290100, 1379.355455732259998, 211.5054726329910011 ) ) ;
#99300 = CARTESIAN_POINT ( 'NONE',  ( 11.37055338930000126, 1425.522980547530096, 139.6335801328979755 ) ) ;
#99302 = CARTESIAN_POINT ( 'NONE',  ( 16.52275002910640112, 1525.042412244750039, 237.2696364103756252 ) ) ;
#99303 = ADVANCED_FACE ( 'NONE', ( #94518 ), #77200, .F. ) ;
#99304 = CARTESIAN_POINT ( 'NONE',  ( 40.08574870070000173, 1445.562093085849938, 136.8698620028980031 ) ) ;
#99305 = CARTESIAN_POINT ( 'NONE',  ( 2.483949940595000516, 1517.156142772249950, 202.1710124019969896 ) ) ;
#99306 = CARTESIAN_POINT ( 'NONE',  ( 7.792129069010000464, 1426.255977840449987, 211.8493891909589877 ) ) ;
#99307 = CARTESIAN_POINT ( 'NONE',  ( -13.28956057169999916, 1415.163755984229965, 220.9230430223980193 ) ) ;
#99308 = CARTESIAN_POINT ( 'NONE',  ( 16.48353617723500264, 1512.679339245399888, 197.4676877011670229 ) ) ;
#99309 = CARTESIAN_POINT ( 'NONE',  ( -18.19590854888185305, 1512.187213306747481, 180.0410247165186490 ) ) ;
#99310 = CARTESIAN_POINT ( 'NONE',  ( 6.490272193332720122E-14, 1378.020218211860083, 211.7927966155920103 ) ) ;
#99311 = ADVANCED_FACE ( 'NONE', ( #105149 ), #65800, .T. ) ;
#99312 = CARTESIAN_POINT ( 'NONE',  ( 7.975220293214148271, 1366.176009064089612, 210.6218459617142003 ) ) ;
#99313 = B_SPLINE_CURVE_WITH_KNOTS ( 'NONE', 5,
 ( #4716, #48953, #66858, #47281, #32679, #24264 ),
 .UNSPECIFIED., .F., .F.,
 ( 6, 6 ),
 ( 0.000000000000000000, 1.000000000000000000 ),
 .UNSPECIFIED. ) ;
#99315 = ORIENTED_EDGE ( 'NONE', *, *, #94120, .T. ) ;
#99314 = CARTESIAN_POINT ( 'NONE',  ( 9.480877448319999345, 1453.580774491189914, 212.8767779103989994 ) ) ;
#99316 = EDGE_LOOP ( 'NONE', ( #4607, #87387, #80599 ) ) ;
#99317 = CARTESIAN_POINT ( 'NONE',  ( -13.96458935331429174, 1446.023135734114703, 188.4738057646961806 ) ) ;
#99318 = CARTESIAN_POINT ( 'NONE',  ( -22.02326011579999943, 1411.040515729830076, 214.9716949974079796 ) ) ;
#99319 = CARTESIAN_POINT ( 'NONE',  ( 2.087781203659999640, 1508.813655593830163, 237.6275677719980024 ) ) ;
#99320 = CARTESIAN_POINT ( 'NONE',  ( -12.99573497267853739, 1444.878364782870221, 169.4220454143612073 ) ) ;
#99321 = CARTESIAN_POINT ( 'NONE',  ( -24.90417444750000087, 1509.109214294029925, 197.4104332050980304 ) ) ;
#99322 = CARTESIAN_POINT ( 'NONE',  ( 2.958096254149829907, 1515.068899375750107, 204.7924306969019881 ) ) ;
#99324 = CARTESIAN_POINT ( 'NONE',  ( 17.46592908230000063, 1416.259332967430055, 226.1411364642979720 ) ) ;
#99323 = CARTESIAN_POINT ( 'NONE',  ( 3.297786611580000304, 1446.227577985589960, 199.9593576464789919 ) ) ;
#99325 = CARTESIAN_POINT ( 'NONE',  ( 2.498440639099999583, 1429.771114423330118, 184.7212983517980263 ) ) ;
#99326 = CARTESIAN_POINT ( 'NONE',  ( -4.151903202082950273, 1464.101420083999983, 199.7805968759980146 ) ) ;
#99327 = CARTESIAN_POINT ( 'NONE',  ( -41.45642610774959991, 1445.626696643309970, 135.8732978911219789 ) ) ;
#99328 = CARTESIAN_POINT ( 'NONE',  ( 9.141780084607901813, 1396.232298419879726, 202.9009529963200009 ) ) ;
#99329 = CARTESIAN_POINT ( 'NONE',  ( 33.91375399455670703, 1437.010669090869897, 136.5612025278969952 ) ) ;
#99330 = CARTESIAN_POINT ( 'NONE',  ( 11.73709356400000026, 1426.695943121429991, 144.1748013713979901 ) ) ;
#99331 = CARTESIAN_POINT ( 'NONE',  ( 8.979367357839899810, 1509.226626805293563, 181.2302862350315991 ) ) ;
#99332 = ORIENTED_EDGE ( 'NONE', *, *, #48004, .T. ) ;
#99333 = CARTESIAN_POINT ( 'NONE',  ( 3.791089716489999706, 1424.059099777229903, 184.0089410633980265 ) ) ;
#99334 = CARTESIAN_POINT ( 'NONE',  ( 1.737175160616053260, 1450.466040294496452, 181.7986353519378326 ) ) ;
#99335 = ORIENTED_EDGE ( 'NONE', *, *, #95331, .T. ) ;
#99336 = ORIENTED_EDGE ( 'NONE', *, *, #70910, .T. ) ;
#99337 = FACE_OUTER_BOUND ( 'NONE', #18474, .T. ) ;
#99338 = CARTESIAN_POINT ( 'NONE',  ( 6.358435812139999754, 1368.427897723179740, 207.6218459616989946 ) ) ;
#99339 = CARTESIAN_POINT ( 'NONE',  ( -109.6623370671470781, 1386.518664481797941, 311.2475360254030079 ) ) ;
#99340 = CARTESIAN_POINT ( 'NONE',  ( 13.06509470220000146, 1434.822844257089855, 195.5376774312979933 ) ) ;
#99341 = CARTESIAN_POINT ( 'NONE',  ( -4.615017365965000451, 1516.987478262539980, 215.6816440265270103 ) ) ;
#99342 = CARTESIAN_POINT ( 'NONE',  ( -12.64090277919120098, 1379.240988027499952, 208.6656503568100050 ) ) ;
#99343 = ORIENTED_EDGE ( 'NONE', *, *, #15204, .T. ) ;
#99344 = CARTESIAN_POINT ( 'NONE',  ( -11.65393960900000003, 1502.937255890489951, 208.0196683168489926 ) ) ;
#99345 = CARTESIAN_POINT ( 'NONE',  ( 2.500000000000000000, 1448.894380902750072, 155.6080914261119972 ) ) ;
#99346 = CARTESIAN_POINT ( 'NONE',  ( -44.99452937809999753, 1375.083786706710043, 231.7591686826590092 ) ) ;
#99347 = VECTOR ( 'NONE', #90373, 1000.000000000000114 ) ;
#99348 = CARTESIAN_POINT ( 'NONE',  ( 16.32914645889999861, 1414.913060387329779, 212.3586363723179886 ) ) ;
#99349 = CARTESIAN_POINT ( 'NONE',  ( 3.447264348965000558, 1516.858765657450249, 205.6607986404769974 ) ) ;
#99350 = ORIENTED_EDGE ( 'NONE', *, *, #50862, .F. ) ;
#99351 = CARTESIAN_POINT ( 'NONE',  ( 2.297629621054999571, 1516.970035769810011, 209.8568691683980205 ) ) ;
#99352 = CARTESIAN_POINT ( 'NONE',  ( -19.89462864549999921, 1508.347918161529833, 229.2892912506979997 ) ) ;
#99353 = B_SPLINE_SURFACE_WITH_KNOTS ( 'NONE', 2, 5, ( 
 ( #21607, #72597, #29471, #64206, #30016, #3208 ),
 ( #46859, #37890, #72073, #56347, #38422, #37336 ),
 ( #28939, #89389, #12679, #47395, #80445, #4294 ) ),
 .UNSPECIFIED., .F., .F., .F.,
 ( 3, 3 ),
 ( 6, 6 ),
 ( 1.399803019399999959, 2.016961153140000018 ),
 ( 0.000000000000000000, 1.000000000000000000 ),
 .UNSPECIFIED. ) ;
#99354 = CARTESIAN_POINT ( 'NONE',  ( -16.18025473180839668, 1412.759566377935926, 269.3698341425424587 ) ) ;
#99355 = CARTESIAN_POINT ( 'NONE',  ( 6.252266454184999489, 1511.741868877540128, 217.9101624594169948 ) ) ;
#99357 = ORIENTED_EDGE ( 'NONE', *, *, #366, .F. ) ;
#99356 = CARTESIAN_POINT ( 'NONE',  ( 1.600048698852036821, 1411.254281879943164, 135.5999999980979851 ) ) ;
#99358 = CARTESIAN_POINT ( 'NONE',  ( 2.500000000000000000, 1419.623475504530006, 147.1347451145979903 ) ) ;
#99359 = CARTESIAN_POINT ( 'NONE',  ( -33.37279912171400298, 1440.913060389960037, 247.4612066733249947 ) ) ;
#99360 = CARTESIAN_POINT ( 'NONE',  ( -54.20202940400000102, 1384.105748123020021, 270.3343205631590536 ) ) ;
#99362 = EDGE_CURVE ( 'NONE', #100441, #19417, #19275, .T. ) ;
#99361 = CARTESIAN_POINT ( 'NONE',  ( -0.2518430497564930204, 1466.381564116799836, 235.6808877654009962 ) ) ;
#99363 = ADVANCED_FACE ( 'NONE', ( #88895 ), #61512, .F. ) ;
#99364 = CARTESIAN_POINT ( 'NONE',  ( 6.238299656213650124, 1410.363799256209859, 269.8684970340120231 ) ) ;
#99365 = CARTESIAN_POINT ( 'NONE',  ( 2.877744946244999991, 1516.723920667490120, 213.7309102736070088 ) ) ;
#99366 = CARTESIAN_POINT ( 'NONE',  ( -51.85551458690000004, 1379.702026082089787, 243.6795232500590203 ) ) ;
#99367 = CARTESIAN_POINT ( 'NONE',  ( 23.92887862800000320, 1410.398442247130106, 209.4513301797530005 ) ) ;
#99368 = CARTESIAN_POINT ( 'NONE',  ( -20.54038862950000066, 1509.293030658830048, 188.7525476221979943 ) ) ;
#99369 = DIRECTION ( 'NONE',  ( 0.7414773880254711402, 0.000000000000000000, 0.6709778558543678662 ) ) ;
#99371 = CARTESIAN_POINT ( 'NONE',  ( -7.709465792554129671, 1516.550879573519751, 210.7818539985390203 ) ) ;
#99370 = CIRCLE ( 'NONE', #40396, 1.999999999999998668 ) ;
#99372 = CARTESIAN_POINT ( 'NONE',  ( -2.863787893864999656, 1516.788317650260069, 210.8382387120070121 ) ) ;
#99373 = CARTESIAN_POINT ( 'NONE',  ( 0.3641805758275279969, 1424.317995888269934, 227.5054904079770211 ) ) ;
#99374 = CARTESIAN_POINT ( 'NONE',  ( 0.07204396340539999388, 1420.438790373129905, 183.3235068346980086 ) ) ;
#99375 = CARTESIAN_POINT ( 'NONE',  ( 10.71453348701945885, 1425.002631316717952, 137.0999999980979283 ) ) ;
#99377 = EDGE_LOOP ( 'NONE', ( #95764, #110094, #80651, #78794 ) ) ;
#99376 = CARTESIAN_POINT ( 'NONE',  ( -26.06393844649999991, 1386.902048729640001, 224.0886486646589901 ) ) ;
#99378 = CARTESIAN_POINT ( 'NONE',  ( -41.85805827384730549, 1385.171263413119959, 245.4604812281340287 ) ) ;
#99379 = EDGE_CURVE ( 'NONE', #71213, #96354, #90908, .T. ) ;
#99380 = CARTESIAN_POINT ( 'NONE',  ( 18.95816156469999925, 1416.822692809329965, 210.4639564331680219 ) ) ;
#99381 = CARTESIAN_POINT ( 'NONE',  ( -4.366757940789628201, 1370.449312398489383, 209.4870077725456667 ) ) ;
#99382 = AXIS2_PLACEMENT_3D ( 'NONE', #4520, #40308, #56575 ) ;
#99383 = DIRECTION ( 'NONE',  ( 0.000000000000000000, -1.000000000000000000, 6.123233995736769734E-17 ) ) ;
#99384 = CARTESIAN_POINT ( 'NONE',  ( -5.506656393879999278, 1440.093542876940091, 154.7592574253979762 ) ) ;
#99385 = CARTESIAN_POINT ( 'NONE',  ( 11.13078225340000138, 1425.146663512289933, 203.3901361119889941 ) ) ;
#99386 = CARTESIAN_POINT ( 'NONE',  ( -1.116803387759635502, 1498.149304908504519, 197.8710347455017313 ) ) ;
#99388 = CARTESIAN_POINT ( 'NONE',  ( -173.8335085727391913, 1524.382868172863937, 317.3879012941878273 ) ) ;
#99387 = CARTESIAN_POINT ( 'NONE',  ( -3.259729335964999919, 1517.119374999550018, 216.4589997383470177 ) ) ;
#99389 = CARTESIAN_POINT ( 'NONE',  ( -0.4151546846821903003, 1511.187213306747708, 242.9330574173806951 ) ) ;
#99390 = CARTESIAN_POINT ( 'NONE',  ( -0.6219649468940665615, 1515.589553500699594, 205.1020666507063481 ) ) ;
#99391 = ORIENTED_EDGE ( 'NONE', *, *, #8283, .F. ) ;
#99392 = CARTESIAN_POINT ( 'NONE',  ( -2.291676311554999845, 1516.534976163889951, 201.8006522243570089 ) ) ;
#99393 = VERTEX_POINT ( 'NONE', #35733 ) ;
#99394 = CARTESIAN_POINT ( 'NONE',  ( 28.32265144099999787, 1509.673549454430031, 207.2611521168180104 ) ) ;
#99395 = ADVANCED_FACE ( 'NONE', ( #36281 ), #104592, .T. ) ;
#99396 = CARTESIAN_POINT ( 'NONE',  ( 21.00628566139999975, 1454.076385129430037, 222.0485915842979807 ) ) ;
#99397 =( BOUNDED_CURVE ( )  B_SPLINE_CURVE ( 3, ( #106605, #56214, #82521, #64084 ),
 .UNSPECIFIED., .F., .F. ) 
 B_SPLINE_CURVE_WITH_KNOTS ( ( 4, 4 ),
 ( 1.227519483377339959, 1.249431231073490078 ),
 .UNSPECIFIED. ) 
 CURVE ( )  GEOMETRIC_REPRESENTATION_ITEM ( )  RATIONAL_B_SPLINE_CURVE ( ( 1.000000000000000000, 0.9999599900096145522, 0.9999599900096145522, 1.000000000000000000 ) ) 
 REPRESENTATION_ITEM ( '' )  );
#99398 = CARTESIAN_POINT ( 'NONE',  ( 7.878720380360996423, 1438.230628562198945, 153.7443670316927182 ) ) ;
#99399 = CARTESIAN_POINT ( 'NONE',  ( 8.652278223286959502, 1511.434805660039956, 203.7377894773300113 ) ) ;
#99400 = CARTESIAN_POINT ( 'NONE',  ( 2.106115005279999952, 1442.705724707790068, 217.8803785435890177 ) ) ;
#99401 = CARTESIAN_POINT ( 'NONE',  ( -26.80674662115270124, 1509.211243910479880, 201.3592588738389964 ) ) ;
#99402 = B_SPLINE_CURVE_WITH_KNOTS ( 'NONE', 3,
 ( #98857, #89363, #54137, #12656, #97203, #96670, #47914, #46835, #106166, #89905, #88813, #80963, #37313, #64744, #64184, #73119 ),
 .UNSPECIFIED., .F., .F.,
 ( 4, 2, 2, 2, 2, 2, 2, 4 ),
 ( 3.254750701746227874E-09, 6.242996095738161545E-05, 0.0001248566671640615031, 0.0002497100795776726776, 0.0004994169044049760709, 0.0009988305540596259004, 0.001997657853369099248, 0.003995312451988130079 ),
 .UNSPECIFIED. ) ;
#99403 = CARTESIAN_POINT ( 'NONE',  ( -3.667959980290000033, 1446.440575669779946, 162.7182840746979764 ) ) ;
#99404 = CARTESIAN_POINT ( 'NONE',  ( -18.76055448960000049, 1425.655531962830082, 225.4079628041980072 ) ) ;
#99405 = DIRECTION ( 'NONE',  ( 3.828568698926946970E-16, 0.000000000000000000, -1.000000000000000000 ) ) ;
#99406 = CARTESIAN_POINT ( 'NONE',  ( -107.1300166679999961, 1387.670188495179900, 298.1786851041590012 ) ) ;
#99407 = CARTESIAN_POINT ( 'NONE',  ( 18.54207614579999941, 1507.885690588130046, 188.5212023680979883 ) ) ;
#99408 = CARTESIAN_POINT ( 'NONE',  ( -34.76957446138440844, 1458.023740881216781, 269.5283794133094943 ) ) ;
#99409 = VERTEX_POINT ( 'NONE', #62637 ) ;
#99410 = CARTESIAN_POINT ( 'NONE',  ( -105.5086717259999887, 1378.552684895010088, 304.0447740192590231 ) ) ;
#99411 = PLANE ( 'NONE',  #63943 ) ;
#99412 = ADVANCED_FACE ( 'NONE', ( #28997 ), #11100, .F. ) ;
#99413 = CARTESIAN_POINT ( 'NONE',  ( 9.912692182420000719, 1426.220680563049882, 209.0669814966779825 ) ) ;
#99414 = DIRECTION ( 'NONE',  ( -1.836970198721029688E-16, -1.000000000000000000, -1.314768175368352060E-31 ) ) ;
#99415 = CARTESIAN_POINT ( 'NONE',  ( -1.137831637353148961, 1408.952794343696041, 186.7671043909383570 ) ) ;
#99416 = B_SPLINE_CURVE_WITH_KNOTS ( 'NONE', 3,
 ( #35879, #1740, #70063, #26922, #95774, #53243, #68395, #19040, #95226, #34762, #18489, #103050, #68950, #86821, #78999, #44846, #104724, #28014, #94107, #10113, #44285, #87384, #27459, #62201, #10679, #2302, #53809, #36413, #70605, #96329, #26348, #77876, #79537, #102501, #60546, #43722, #19607 ),
 .UNSPECIFIED., .F., .F.,
 ( 4, 3, 3, 3, 3, 3, 3, 3, 3, 3, 3, 3, 4 ),
 ( -1.999999848934280067, -1.897891338336010092, -1.728761199251590108, -1.557452154569009872, -1.384905005406759981, -1.210695233754919942, -1.035838574448660010, -0.8607549794867428439, -0.6858798840580180300, -0.5121999522673421623, -0.3398111951967790478, -0.1690102479686510506, -5.799765116165644940E-06 ),
 .UNSPECIFIED. ) ;
#99417 = CARTESIAN_POINT ( 'NONE',  ( -13.40117755332782856, 1443.408819078402530, 187.0327686018816280 ) ) ;
#99418 = CARTESIAN_POINT ( 'NONE',  ( -3.827327205999999649, 1409.546157813730133, 121.6099336315979969 ) ) ;
#99419 = FACE_OUTER_BOUND ( 'NONE', #88641, .T. ) ;
#99420 = EDGE_CURVE ( 'NONE', #31602, #8790, #101484, .T. ) ;
#99421 = CARTESIAN_POINT ( 'NONE',  ( -2.052509464423307950, 1415.610420790406124, 233.0191148808001458 ) ) ;
#99422 = AXIS2_PLACEMENT_3D ( 'NONE', #52987, #54105, #87119 ) ;
#99423 = CARTESIAN_POINT ( 'NONE',  ( -15.84432591830269743, 1419.853212859319910, 210.7451195136700051 ) ) ;
#99424 = CARTESIAN_POINT ( 'NONE',  ( 24.40297774660000485, 1435.533511806519982, 137.4233649837979954 ) ) ;
#99425 = CARTESIAN_POINT ( 'NONE',  ( -13.25973371150704416, 1443.185291380165609, 169.3834991182581007 ) ) ;
#99427 = ORIENTED_EDGE ( 'NONE', *, *, #20132, .T. ) ;
#99426 = CARTESIAN_POINT ( 'NONE',  ( -14.30199729709999978, 1410.347835160429895, 226.8241708172980111 ) ) ;
#99428 = CARTESIAN_POINT ( 'NONE',  ( -96.27487712110000473, 1383.766385264410019, 310.4021576922589816 ) ) ;
#99429 = CARTESIAN_POINT ( 'NONE',  ( -16.53242905777631222, 1526.073429442291854, 235.9344201561504804 ) ) ;
#99430 = ORIENTED_EDGE ( 'NONE', *, *, #102147, .T. ) ;
#99431 = ORIENTED_EDGE ( 'NONE', *, *, #85906, .T. ) ;
#99432 = CARTESIAN_POINT ( 'NONE',  ( -11.41402577200000223, 1500.969831348989828, 208.5831151415709996 ) ) ;
#99433 = CARTESIAN_POINT ( 'NONE',  ( -19.38211899475871647, 1526.344110814221267, 232.9251177427894390 ) ) ;
#99435 = CARTESIAN_POINT ( 'NONE',  ( -27.24390625670000077, 1454.605078679430108, 244.3119003928979964 ) ) ;
#99434 = CARTESIAN_POINT ( 'NONE',  ( 2.358876809229999871, 1455.879957205790106, 218.6867517008690243 ) ) ;
#99436 = CARTESIAN_POINT ( 'NONE',  ( 8.927028317280980119, 1436.767930426870180, 210.5805728413830025 ) ) ;
#99437 = EDGE_CURVE ( 'NONE', #57683, #89981, #105109, .T. ) ;
#99438 = CARTESIAN_POINT ( 'NONE',  ( -11.51652132750000135, 1433.525180497049860, 151.2587270096979921 ) ) ;
#99439 = CARTESIAN_POINT ( 'NONE',  ( 14.38276615817169635, 1509.537722092532931, 235.4493228184925897 ) ) ;
#99440 = CARTESIAN_POINT ( 'NONE',  ( -4.994775864380000208, 1391.713558696990049, 203.8075142969990168 ) ) ;
#99441 = CARTESIAN_POINT ( 'NONE',  ( 9.581777264995830379, 1464.075427050579947, 211.2528481700169891 ) ) ;
#99442 = FACE_OUTER_BOUND ( 'NONE', #31322, .T. ) ;
#99444 = EDGE_CURVE ( 'NONE', #100441, #82285, #78322, .T. ) ;
#99443 = CARTESIAN_POINT ( 'NONE',  ( 1.407451548163070054, 1515.079400017670196, 213.4509122356359967 ) ) ;
#99445 = CARTESIAN_POINT ( 'NONE',  ( -4.102794113347690619, 1453.855854241320003, 199.4852768663029963 ) ) ;
#99446 = CARTESIAN_POINT ( 'NONE',  ( 451.6689809271080094, 1435.140433208369814, 155.5900787298459704 ) ) ;
#99447 = CARTESIAN_POINT ( 'NONE',  ( 1.592937850129041877, 1362.438491279120626, 209.6218459617148824 ) ) ;
#99448 = CARTESIAN_POINT ( 'NONE',  ( -16.65108875018284706, 1509.615391758380611, 234.1414537928058337 ) ) ;
#99449 = AXIS2_PLACEMENT_3D ( 'NONE', #54946, #29175, #63365 ) ;
#99451 = ORIENTED_EDGE ( 'NONE', *, *, #70106, .F. ) ;
#99450 = CARTESIAN_POINT ( 'NONE',  ( -7.915285451137539677E-10, 1412.889808523510055, 251.0689582627720426 ) ) ;
#99452 = ORIENTED_EDGE ( 'NONE', *, *, #88424, .T. ) ;
#99453 = CARTESIAN_POINT ( 'NONE',  ( -11.85932238006850170, 1431.862983400520079, 149.9619179884730045 ) ) ;
#99454 = CARTESIAN_POINT ( 'NONE',  ( 24.13249860440000205, 1497.226937179990045, 206.7234963521489988 ) ) ;
#99455 = CARTESIAN_POINT ( 'NONE',  ( -5.184304023010000151, 1471.561735541330108, 269.8675879627980407 ) ) ;
#99456 = CARTESIAN_POINT ( 'NONE',  ( 12.89273669479999995, 1508.859229393329997, 233.8778408584979900 ) ) ;
#99457 = CARTESIAN_POINT ( 'NONE',  ( -106.3844429930778972, 1376.302340817388313, 316.0486468239590181 ) ) ;
#99458 = CARTESIAN_POINT ( 'NONE',  ( -13.97684781309999913, 1452.404795722730114, 223.0329335630979983 ) ) ;
#99459 = CARTESIAN_POINT ( 'NONE',  ( 0.3742949575629109793, 1450.903878863470027, 181.4136564121010053 ) ) ;
#99460 = CARTESIAN_POINT ( 'NONE',  ( -8.857648614099998596, 1384.596810254769935, 199.9412065693690010 ) ) ;
#99461 = CARTESIAN_POINT ( 'NONE',  ( 9.986161364699151832, 1468.785215375359940, 208.2634456866570076 ) ) ;
#99462 = CARTESIAN_POINT ( 'NONE',  ( -2.330134126090000368, 1515.064792882589927, 204.7923971856590128 ) ) ;
#99463 = CARTESIAN_POINT ( 'NONE',  ( 10.34804584725118737, 1366.870369466032798, 207.6218459616987673 ) ) ;
#99464 = CARTESIAN_POINT ( 'NONE',  ( -27.39518923616549984, 1412.781094389850068, 268.7457036271840138 ) ) ;
#99465 = VERTEX_POINT ( 'NONE', #43403 ) ;
#99466 = CARTESIAN_POINT ( 'NONE',  ( -3.535949085321830498, 1494.186315171800061, 181.5280936908750107 ) ) ;
#99467 = VERTEX_POINT ( 'NONE', #84820 ) ;
#99468 = ORIENTED_EDGE ( 'NONE', *, *, #106382, .T. ) ;
#99469 = CARTESIAN_POINT ( 'NONE',  ( 4.626591867355000609, 1517.096587378560116, 210.8266407735670214 ) ) ;
#99470 = FACE_OUTER_BOUND ( 'NONE', #76659, .T. ) ;
#99471 = CARTESIAN_POINT ( 'NONE',  ( 41.65675406397859604, 1443.992462633329978, 135.6790809494980010 ) ) ;
#99473 = CARTESIAN_POINT ( 'NONE',  ( -17.64860873675443287, 1419.496838671263504, 207.1709281612535563 ) ) ;
#99472 = CARTESIAN_POINT ( 'NONE',  ( -4.997573825325000385, 1516.742629295279812, 212.5803724681170195 ) ) ;
#99474 = CARTESIAN_POINT ( 'NONE',  ( -15.19110828580000039, 1440.435427132970062, 189.4075412060980170 ) ) ;
#99475 = CARTESIAN_POINT ( 'NONE',  ( -2.447859506707243060, 1449.353156360412186, 183.0517911818036794 ) ) ;
#99476 = VERTEX_POINT ( 'NONE', #34438 ) ;
#99477 = CARTESIAN_POINT ( 'NONE',  ( -5.005700239535000762, 1516.732530461250008, 202.1838802717869896 ) ) ;
#99478 = CARTESIAN_POINT ( 'NONE',  ( 9.788141037149998169, 1471.003676308989952, 212.2094846091489728 ) ) ;
#99479 = CARTESIAN_POINT ( 'NONE',  ( -19.40145187611040001, 1384.532064108600025, 201.5288265737380016 ) ) ;
#99480 = CARTESIAN_POINT ( 'NONE',  ( -42.54898869008160034, 1440.913047336420050, 270.0692026506110324 ) ) ;
#99481 = CARTESIAN_POINT ( 'NONE',  ( -15.72751745975079984, 1517.051704408389924, 211.3620530696679793 ) ) ;
#99482 = CARTESIAN_POINT ( 'NONE',  ( -4.606808002230000199, 1396.134576369729984, 198.3574891071980062 ) ) ;
#99484 = ORIENTED_EDGE ( 'NONE', *, *, #69870, .T. ) ;
#99483 = CARTESIAN_POINT ( 'NONE',  ( -7.988512957371035839, 1364.858218297605163, 209.6218459617148824 ) ) ;
#99485 = VERTEX_POINT ( 'NONE', #59109 ) ;
#99486 = CARTESIAN_POINT ( 'NONE',  ( -1.793335950739999962, 1419.496365638530051, 185.6406336190979971 ) ) ;
#99487 = CARTESIAN_POINT ( 'NONE',  ( 3.746090737668994031, 1425.475261178803976, 185.1844613459034576 ) ) ;
#99488 = CARTESIAN_POINT ( 'NONE',  ( -14.25613302710000063, 1464.413060387330006, 194.1747703853979772 ) ) ;
#99489 = ADVANCED_FACE ( 'NONE', ( #35536 ), #7920, .T. ) ;
#99490 = CARTESIAN_POINT ( 'NONE',  ( 18.65451742820949832, 1507.632629731499947, 188.5326158842280222 ) ) ;
#99491 = CYLINDRICAL_SURFACE ( 'NONE', #65097, 2.000000000000003109 ) ;
#99492 = CARTESIAN_POINT ( 'NONE',  ( -1.117840124865000062, 1516.949031626070109, 210.8389850543470061 ) ) ;
#99493 = CARTESIAN_POINT ( 'NONE',  ( -68.77190080519999071, 1379.747925807450201, 280.3125203366930123 ) ) ;
#99494 = CARTESIAN_POINT ( 'NONE',  ( 5.492221782479999703, 1439.600215925499924, 154.7521915351979942 ) ) ;
#99495 = CARTESIAN_POINT ( 'NONE',  ( 0.9598037665343115421, 1421.307034539813685, 193.7451072252824247 ) ) ;
#99496 = CARTESIAN_POINT ( 'NONE',  ( 5.819172478703739770, 1440.531633204680020, 216.0087162162849665 ) ) ;
#99497 = CARTESIAN_POINT ( 'NONE',  ( 18.80463393750000023, 1425.801073282529842, 225.6039001781980176 ) ) ;
#99498 = CARTESIAN_POINT ( 'NONE',  ( 7.703229018584999643, 1511.126521646420088, 203.6801735634869885 ) ) ;
#99499 = CARTESIAN_POINT ( 'NONE',  ( 3.445201488374999954, 1516.743010792419909, 207.4064848398570291 ) ) ;
#99500 = ORIENTED_EDGE ( 'NONE', *, *, #45337, .F. ) ;
#99501 = CARTESIAN_POINT ( 'NONE',  ( -40.71747596589660390, 1438.773003664010048, 134.7398499747960159 ) ) ;
#99502 = CARTESIAN_POINT ( 'NONE',  ( -11.74015320060000001, 1428.979986575930070, 144.1938086916980239 ) ) ;
#99503 = DIRECTION ( 'NONE',  ( -6.123233995736769734E-17, -1.000000000000000000, -1.124819836996399911E-32 ) ) ;
#99504 = EDGE_LOOP ( 'NONE', ( #81216, #65343, #49547, #28059 ) ) ;
#99505 = CARTESIAN_POINT ( 'NONE',  ( 7.012921545474999796, 1508.551704408389924, 209.1218459511669892 ) ) ;
#99506 = EDGE_CURVE ( 'NONE', #23328, #22416, #21002, .T. ) ;
#99507 = CARTESIAN_POINT ( 'NONE',  ( 23.84493162013280099, 1452.080376998370184, 136.9869860125139951 ) ) ;
#99508 = CARTESIAN_POINT ( 'NONE',  ( 13.88473851270000026, 1415.296882296330068, 197.4370144994979910 ) ) ;
#99509 = DIRECTION ( 'NONE',  ( 1.224646799147350002E-16, -1.836970198721029688E-16, -1.000000000000000000 ) ) ;
#99510 = CARTESIAN_POINT ( 'NONE',  ( 26.69873419689999849, 1451.980699541129979, 134.9231770738980174 ) ) ;
#99511 = CARTESIAN_POINT ( 'NONE',  ( -26.79413315976150045, 1435.433175095809929, 135.2874648155150226 ) ) ;
#99512 = CARTESIAN_POINT ( 'NONE',  ( -14.07887498544812743, 1379.617235141234687, 211.6859004506403323 ) ) ;
#99513 = CARTESIAN_POINT ( 'NONE',  ( 33.23571934791672788, 1512.187213306747481, 219.4842663281462478 ) ) ;
#99514 = DIRECTION ( 'NONE',  ( 0.000000000000000000, -1.000000000000000000, 0.000000000000000000 ) ) ;
#99515 = CARTESIAN_POINT ( 'NONE',  ( 2.500000000000000000, 1439.509563800350179, 163.9071484463910053 ) ) ;
#99516 = CARTESIAN_POINT ( 'NONE',  ( -16.19086242769280304, 1409.478452467050147, 225.0103265570539861 ) ) ;
#99517 = CARTESIAN_POINT ( 'NONE',  ( 7.718763505904999711, 1516.905946377369901, 216.0642002436470079 ) ) ;
#99518 = ORIENTED_EDGE ( 'NONE', *, *, #75563, .F. ) ;
#99519 = CARTESIAN_POINT ( 'NONE',  ( 7.713327774496799627, 1516.698364169800016, 208.2833887839009890 ) ) ;
#99520 = CARTESIAN_POINT ( 'NONE',  ( -2.339369569539999638, 1474.134115800729887, 270.1366117264980176 ) ) ;
#99521 = CARTESIAN_POINT ( 'NONE',  ( -3.090243552160000018, 1448.623823917879918, 184.7128630361980015 ) ) ;
#99522 = TOROIDAL_SURFACE ( 'NONE', #95959, 10.10241613150000006, 2.000000000000000000 ) ;
#99523 = B_SPLINE_CURVE_WITH_KNOTS ( 'NONE', 3,
 ( #53072, #70441, #36808, #70999, #28409, #62607, #96722, #54188, #56371, #5402, #39561, #105681, #4318, #55835, #55284, #91052, #107312, #56922, #46886, #37362, #98357, #20531, #28965, #63690, #38449, #21080, #90502, #89414, #80470, #47420, #12702, #81011, #13780, #72621, #97254, #29497, #106753, #54736, #30042, #63155, #64794, #38990, #64234, #81543, #31147, #107858, #47961, #82104, #73735, #65335, #98903, #21629, #106215, #46341, #99443, #97803, #3786, #22720, #45786, #88865, #79921 ),
 .UNSPECIFIED., .F., .F.,
 ( 4, 3, 3, 3, 3, 3, 3, 3, 3, 3, 3, 3, 3, 3, 3, 3, 3, 3, 3, 3, 4 ),
 ( 2.324858856890000158, 2.629298819987540003, 2.933834190021629595, 3.016888080810000261, 3.323211181039090079, 3.630193766034540026, 3.937176351030000188, 4.233214320285879850, 4.526002641956389461, 4.813615658896620353, 4.970096098099999971, 5.257590953083679963, 5.548112191535929938, 5.843468099036670083, 6.019659498159999345, 6.321166958453420470, 6.626011430626180143, 6.935803168058399137, 7.053491825919998348, 7.364378125606098280, 7.657659707949999728 ),
 .UNSPECIFIED. ) ;
#99524 = CARTESIAN_POINT ( 'NONE',  ( 0.2178157486290130118, 1452.982786607829894, 183.2541296479709843 ) ) ;
#99525 = CARTESIAN_POINT ( 'NONE',  ( 1.326883316820000269, 1474.953498172789978, 220.4794457010989959 ) ) ;
#99526 = CARTESIAN_POINT ( 'NONE',  ( 30.83123567651259833, 1510.067171565570106, 207.3056169179679671 ) ) ;
#99527 = CARTESIAN_POINT ( 'NONE',  ( 11.60004869885203682, 1426.461398603654288, 139.0972022331852145 ) ) ;
#99528 = DIRECTION ( 'NONE',  ( 0.000000000000000000, 0.000000000000000000, -1.000000000000000000 ) ) ;
#99529 = CARTESIAN_POINT ( 'NONE',  ( -2.500000000000000000, 1421.745358796729988, 151.9633565684980283 ) ) ;
#99531 = EDGE_CURVE ( 'NONE', #103262, #5409, #29967, .T. ) ;
#99530 = CARTESIAN_POINT ( 'NONE',  ( 0.6680169871064080001, 1455.976695232599923, 198.5860125881739862 ) ) ;
#99532 = CARTESIAN_POINT ( 'NONE',  ( -4.790712462651379169E-07, 1408.860257374809862, 223.5938187205209999 ) ) ;
#99533 = CARTESIAN_POINT ( 'NONE',  ( 29.92073223143840011, 1440.913060386099914, 238.0971241985569975 ) ) ;
#99535 = CARTESIAN_POINT ( 'NONE',  ( -3.441085789689999785, 1476.342819426989990, 219.6507253252989926 ) ) ;
#99534 = CARTESIAN_POINT ( 'NONE',  ( -10.49702031989500028, 1471.002758439979971, 210.3192899704120293 ) ) ;
#99536 = CARTESIAN_POINT ( 'NONE',  ( 0.7998021860399979754, 1481.092795404789968, 229.6971392698989973 ) ) ;
#99537 = ORIENTED_EDGE ( 'NONE', *, *, #7129, .T. ) ;
#99538 = ADVANCED_FACE ( 'NONE', ( #64075 ), #49661, .T. ) ;
#99539 = ORIENTED_EDGE ( 'NONE', *, *, #42452, .F. ) ;
#99540 = CARTESIAN_POINT ( 'NONE',  ( -2.487935123034410001, 1508.783371655767951, 213.6678281891418578 ) ) ;
#99541 = ADVANCED_FACE ( 'NONE', ( #70291 ), #24880, .T. ) ;
#99542 = CARTESIAN_POINT ( 'NONE',  ( 17.38482601099109814, 1410.884446382940041, 192.4603632472940262 ) ) ;
#99543 = CARTESIAN_POINT ( 'NONE',  ( -4.014584143420000473, 1443.145720380289958, 200.3327953268290287 ) ) ;
#99544 = CARTESIAN_POINT ( 'NONE',  ( 11.72073075646250118, 1501.840823038659892, 211.4460601384429879 ) ) ;
#99545 = CARTESIAN_POINT ( 'NONE',  ( 2.279486850145009846, 1508.935250638985735, 237.8394454178328488 ) ) ;
#99546 = CARTESIAN_POINT ( 'NONE',  ( 18.18137293399999876, 1507.546748832030062, 186.5307135875980009 ) ) ;
#99547 = EDGE_CURVE ( 'NONE', #91877, #93336, #89021, .T. ) ;
#99548 = CARTESIAN_POINT ( 'NONE',  ( 15.09682228229999978, 1409.610690924630035, 192.0685155598980032 ) ) ;
#99549 = CARTESIAN_POINT ( 'NONE',  ( -5.430576729993609852, 1440.816380553300178, 154.8042786586000261 ) ) ;
#99550 = CARTESIAN_POINT ( 'NONE',  ( -39.50122532003389608, 1383.828917900590113, 240.9233743668259820 ) ) ;
#99551 = CARTESIAN_POINT ( 'NONE',  ( -4.824495029074999941, 1511.382391139620040, 200.6581036276869838 ) ) ;
#99552 = CARTESIAN_POINT ( 'NONE',  ( -12.78755494719999852, 1416.844618642330033, 195.3259368849979865 ) ) ;
#99553 = B_SPLINE_CURVE_WITH_KNOTS ( 'NONE', 5,
 ( #32092, #101471, #93089, #83582, #110450, #50005 ),
 .UNSPECIFIED., .F., .F.,
 ( 6, 6 ),
 ( 0.000000000000000000, 1.000000000000000000 ),
 .UNSPECIFIED. ) ;
#99554 = CARTESIAN_POINT ( 'NONE',  ( -5.716900218388740740, 1511.491070486171338, 200.3735384854518315 ) ) ;
#99555 = CARTESIAN_POINT ( 'NONE',  ( 2.502826361999999971, 1464.606218255329850, 236.1230330374980042 ) ) ;
#99557 = ORIENTED_EDGE ( 'NONE', *, *, #53463, .T. ) ;
#99556 = CARTESIAN_POINT ( 'NONE',  ( -3.094819227209999912, 1457.827881835389917, 218.9172905669589966 ) ) ;
#99558 = CARTESIAN_POINT ( 'NONE',  ( -0.8228443623879999613, 1450.943455458130074, 182.1014883083980180 ) ) ;
#99559 = CARTESIAN_POINT ( 'NONE',  ( -27.25467149600000027, 1380.910011778850276, 222.6012197218589677 ) ) ;
#99560 = CARTESIAN_POINT ( 'NONE',  ( -3.592139376770000059, 1475.286963719890082, 199.0484973181989972 ) ) ;
#99562 = ORIENTED_EDGE ( 'NONE', *, *, #26080, .T. ) ;
#99561 = CARTESIAN_POINT ( 'NONE',  ( -18.05542472024740164, 1416.825783990419950, 209.4840485447890046 ) ) ;
#99563 = ORIENTED_EDGE ( 'NONE', *, *, #44571, .F. ) ;
#99564 = FACE_OUTER_BOUND ( 'NONE', #17528, .T. ) ;
#99565 = CARTESIAN_POINT ( 'NONE',  ( 35.75324696180250328, 1437.345929592409902, 136.5360666854240037 ) ) ;
#99566 = CARTESIAN_POINT ( 'NONE',  ( -1.073240929390329958E-18, 1414.661898229710005, 209.1218459616989946 ) ) ;
#99567 = CARTESIAN_POINT ( 'NONE',  ( -37.65047686723229958, 1442.773887284729881, 137.1096749952629921 ) ) ;
#99568 = CARTESIAN_POINT ( 'NONE',  ( -103.9362963259999901, 1380.106856784760112, 301.6745611782590117 ) ) ;
#99569 = CARTESIAN_POINT ( 'NONE',  ( 3.395043742270000386, 1466.412111213989874, 219.6384586637989855 ) ) ;
#99570 = DIRECTION ( 'NONE',  ( -0.9417419115949053898, -0.3363363969979660806, 9.559255346349054600E-15 ) ) ;
#99571 = CARTESIAN_POINT ( 'NONE',  ( 7.948017842360480145, 1409.190611286300282, 196.4401314888699801 ) ) ;
#99572 = CARTESIAN_POINT ( 'NONE',  ( 18.12086373898799962, 1425.009007305328169, 225.3873405099579941 ) ) ;
#99573 = FACE_OUTER_BOUND ( 'NONE', #106795, .T. ) ;
#99574 = ADVANCED_FACE ( 'NONE', ( #63539 ), #10903, .F. ) ;
#99575 = DIRECTION ( 'NONE',  ( 0.000000000000000000, 1.000000000000000000, 0.000000000000000000 ) ) ;
#99576 = FACE_OUTER_BOUND ( 'NONE', #46398, .T. ) ;
#99577 = TOROIDAL_SURFACE ( 'NONE', #79946, 32.13701971169416538, 1.000000000000000000 ) ;
#99578 = CARTESIAN_POINT ( 'NONE',  ( -3.884405768773259826, 1449.583267633219975, 185.0056059189860207 ) ) ;
#99579 = ORIENTED_EDGE ( 'NONE', *, *, #14706, .T. ) ;
#99580 = EDGE_CURVE ( 'NONE', #109851, #56546, #72913, .T. ) ;
#99581 = CARTESIAN_POINT ( 'NONE',  ( 18.19590854887586318, 1522.644714754857659, 238.2026672068722064 ) ) ;
#99582 = DIRECTION ( 'NONE',  ( -1.000000000000000000, 0.000000000000000000, 0.000000000000000000 ) ) ;
#99583 = CARTESIAN_POINT ( 'NONE',  ( -12.82272891259999881, 1434.845015028379976, 150.1638710903980041 ) ) ;
#99584 = DIRECTION ( 'NONE',  ( -0.000000000000000000, -1.000000000000000000, -0.000000000000000000 ) ) ;
#99585 = CARTESIAN_POINT ( 'NONE',  ( -20.27149120612340027, 1497.224176212940165, 190.6980538895379880 ) ) ;
#99586 = CARTESIAN_POINT ( 'NONE',  ( -14.65245208429999835, 1420.119839420520066, 213.8659312793989784 ) ) ;
#99587 = CARTESIAN_POINT ( 'NONE',  ( -109.6649067579999866, 1386.049555229090174, 311.2750003182590035 ) ) ;
#99588 = CARTESIAN_POINT ( 'NONE',  ( -8.771942286537230515, 1511.501325589009866, 214.9071201462460010 ) ) ;
#99589 = CARTESIAN_POINT ( 'NONE',  ( -9.692061980449199865, 1363.802329763672105, 210.6218459616991936 ) ) ;
#99590 = CARTESIAN_POINT ( 'NONE',  ( -46.14542121321060364, 1440.248490524040108, 268.2047085544609786 ) ) ;
#99591 = CARTESIAN_POINT ( 'NONE',  ( 13.42361184146170139, 1508.223676004419985, 233.2139651083469971 ) ) ;
#99592 = CARTESIAN_POINT ( 'NONE',  ( -19.99752153760000084, 1488.350075126529873, 191.5586291822979774 ) ) ;
#99593 = CARTESIAN_POINT ( 'NONE',  ( -3.269984819434999856, 1516.999105586269934, 207.4194399470370058 ) ) ;
#99594 = CARTESIAN_POINT ( 'NONE',  ( 4.214930602837739571, 1408.999354465240231, 222.9586692084779997 ) ) ;
#99595 = AXIS2_PLACEMENT_3D ( 'NONE', #2614, #106687, #63627 ) ;
#99596 = CARTESIAN_POINT ( 'NONE',  ( 29.33952678944442027, 1526.382868172864164, 201.1028049641010114 ) ) ;
#99597 = CARTESIAN_POINT ( 'NONE',  ( -14.47191459792289869, 1379.648775954749908, 208.1784578746709826 ) ) ;
#99598 = CARTESIAN_POINT ( 'NONE',  ( 7.462159244181010287, 1425.241657824579988, 212.3244533792270090 ) ) ;
#99599 = VERTEX_POINT ( 'NONE', #20925 ) ;
#99600 = CARTESIAN_POINT ( 'NONE',  ( 14.70061896029999993, 1417.388462482229897, 244.5173668933980196 ) ) ;
#99601 = CARTESIAN_POINT ( 'NONE',  ( -7.500000000000000888, 1392.213060387289943, 209.1218459616989946 ) ) ;
#99603 = CARTESIAN_POINT ( 'NONE',  ( -14.92433373228269922, 1512.160613316490071, 221.5430094126030269 ) ) ;
#99602 = CARTESIAN_POINT ( 'NONE',  ( -3.518337011159999861, 1478.170661589230122, 182.2087550695979985 ) ) ;
#99604 = CARTESIAN_POINT ( 'NONE',  ( 1.514918641329773497, 1508.378724870832229, 180.6682338045059169 ) ) ;
#99605 = CARTESIAN_POINT ( 'NONE',  ( 1.436583437199999868E-09, 1416.682256489629935, 238.2947547783980156 ) ) ;
#99606 = CARTESIAN_POINT ( 'NONE',  ( -29.63440978849957474, 1509.974483337211041, 207.3636310854570866 ) ) ;
#99607 = CARTESIAN_POINT ( 'NONE',  ( -18.16938274068190040, 1452.278571560799946, 145.2377407453319904 ) ) ;
#99608 = CARTESIAN_POINT ( 'NONE',  ( 27.85266659460000227, 1451.078832383830104, 136.3466686027980188 ) ) ;
#99609 = EDGE_LOOP ( 'NONE', ( #27631, #75940, #82565, #60990 ) ) ;
#99610 = CARTESIAN_POINT ( 'NONE',  ( -2.500000000000000000, 1420.232870451130111, 149.2693594355980053 ) ) ;
#99611 = DIRECTION ( 'NONE',  ( 0.000000000000000000, 1.000000000000000000, 0.000000000000000000 ) ) ;
#99612 = CARTESIAN_POINT ( 'NONE',  ( 16.65265346172540006, 1423.208279008830004, 227.6530141284199829 ) ) ;
#99613 = CARTESIAN_POINT ( 'NONE',  ( 10.94062157769999999, 1501.627468090889806, 205.7261589474190373 ) ) ;
#99614 = ORIENTED_EDGE ( 'NONE', *, *, #28932, .T. ) ;
#99615 = ORIENTED_EDGE ( 'NONE', *, *, #83871, .F. ) ;
#99616 = CARTESIAN_POINT ( 'NONE',  ( -53.47023167649999920, 1385.031515079650262, 230.7490043923590122 ) ) ;
#99617 = CARTESIAN_POINT ( 'NONE',  ( -24.12531086176590378, 1410.986997877699878, 208.8764144295159895 ) ) ;
#99618 = CARTESIAN_POINT ( 'NONE',  ( 19.66678637246580053, 1522.051704408389924, 202.3500283489900085 ) ) ;
#99619 = DIRECTION ( 'NONE',  ( -0.09060005235378243427, 0.000000000000000000, 0.9958873583460591261 ) ) ;
#99620 = VECTOR ( 'NONE', #106298, 1000.000000000000000 ) ;
#99621 = FACE_OUTER_BOUND ( 'NONE', #47406, .T. ) ;
#99622 = CARTESIAN_POINT ( 'NONE',  ( -9.872048858160001217, 1498.343720009429944, 234.1146122690979894 ) ) ;
#99623 = CARTESIAN_POINT ( 'NONE',  ( -1.775935834183570261, 1421.047323150906550, 184.1901391204128799 ) ) ;
#99624 = CARTESIAN_POINT ( 'NONE',  ( 43.21760421406469987, 1452.663687658380013, 268.8371515474040052 ) ) ;
#99625 = CARTESIAN_POINT ( 'NONE',  ( -12.81744069099319994, 1415.938742849230039, 221.7277189786869940 ) ) ;
#99626 = CARTESIAN_POINT ( 'NONE',  ( -7.753833341240000898, 1425.741319864559955, 203.8098606200590268 ) ) ;
#99627 = CARTESIAN_POINT ( 'NONE',  ( 5.773668814845000163, 1516.734985836460055, 205.0832084693769843 ) ) ;
#99628 = ORIENTED_EDGE ( 'NONE', *, *, #55531, .F. ) ;
#99629 = CARTESIAN_POINT ( 'NONE',  ( 11.52063869959389919, 1480.272724040029971, 211.6366542486999833 ) ) ;
#99630 = CARTESIAN_POINT ( 'NONE',  ( 20.05746556670000302, 1473.529709444389937, 207.1912480031890027 ) ) ;
#99631 = CARTESIAN_POINT ( 'NONE',  ( 12.89353391096544676, 1442.888115666797830, 187.0162393882783078 ) ) ;
#99632 = ORIENTED_EDGE ( 'NONE', *, *, #52901, .T. ) ;
#99633 = VERTEX_POINT ( 'NONE', #89251 ) ;
#99634 = CARTESIAN_POINT ( 'NONE',  ( 2.413234528062761619, 1507.615208040094103, 220.6132374451732971 ) ) ;
#99635 = DIRECTION ( 'NONE',  ( -1.836970198721029688E-16, -1.000000000000000000, -8.835242138475329394E-33 ) ) ;
#99636 = CARTESIAN_POINT ( 'NONE',  ( -10.93170597650880005, 1470.132936137649949, 212.2373671120849963 ) ) ;
#99637 = CARTESIAN_POINT ( 'NONE',  ( 9.464504535678571528, 1503.363322680939973, 217.6559705080630067 ) ) ;
#99638 = CARTESIAN_POINT ( 'NONE',  ( -1.718340007434250173E-05, 1407.928426573429988, 270.2927087787980440 ) ) ;
#99639 = CARTESIAN_POINT ( 'NONE',  ( -2.993158061556190130, 1476.307674819270005, 220.1965791242180046 ) ) ;
#99640 = CARTESIAN_POINT ( 'NONE',  ( 10.98083629090000102, 1433.016921068679949, 151.7694307944979926 ) ) ;
#99641 = CARTESIAN_POINT ( 'NONE',  ( 10.02421119480000122, 1480.534221758890226, 205.8829018067289951 ) ) ;
#99642 = PLANE ( 'NONE',  #66102 ) ;
#99644 = CARTESIAN_POINT ( 'NONE',  ( -105.6427474625459979, 1391.452704347849931, 305.6364936059279671 ) ) ;
#99643 = CARTESIAN_POINT ( 'NONE',  ( -16.75267927776890176, 1413.684132339210009, 191.6587516336579995 ) ) ;
#99645 = VECTOR ( 'NONE', #3879, 1000.000000000000000 ) ;
#99646 = CARTESIAN_POINT ( 'NONE',  ( 10.72411309857909778, 1423.704347997469995, 206.7356728586999850 ) ) ;
#99647 = B_SPLINE_CURVE_WITH_KNOTS ( 'NONE', 3,
 ( #52073, #86762, #69998, #10051, #45341, #18982, #43664, #19548, #54295, #86206, #79481, #53179, #9498, #2788, #36908, #1125 ),
 .UNSPECIFIED., .F., .F.,
 ( 4, 3, 3, 3, 3, 4 ),
 ( -7.332849288699999413, -7.184230839218289866, -6.152654883699300470, -5.122512162619800691, -4.092878776982500355, -3.012888606410000669 ),
 .UNSPECIFIED. ) ;
#99648 = CARTESIAN_POINT ( 'NONE',  ( -24.66395196768430154, 1509.340428037599850, 222.6198678659309849 ) ) ;
#99649 = CARTESIAN_POINT ( 'NONE',  ( -7.692900486654999703, 1514.487275757750012, 203.3032714771670157 ) ) ;
#99650 = VERTEX_POINT ( 'NONE', #104955 ) ;
#99651 = CARTESIAN_POINT ( 'NONE',  ( 19.00000000000000000, 1438.871025162500018, 209.1218459616979999 ) ) ;
#99652 = CARTESIAN_POINT ( 'NONE',  ( -0.2626388801599250367, 1424.255108689230156, 227.7923674788299877 ) ) ;
#99653 = AXIS2_PLACEMENT_3D ( 'NONE', #72901, #108692, #90225 ) ;
#99654 = CARTESIAN_POINT ( 'NONE',  ( -94.85908788526670321, 1384.958307967540122, 310.0174651394229386 ) ) ;
#99655 = CARTESIAN_POINT ( 'NONE',  ( -8.851511101499999867, 1386.548753862859940, 200.1620584707990247 ) ) ;
#99656 = CARTESIAN_POINT ( 'NONE',  ( 11.26956004432950031, 1427.671205884309984, 209.9218968568520154 ) ) ;
#99658 = VERTEX_POINT ( 'NONE', #46179 ) ;
#99657 = CARTESIAN_POINT ( 'NONE',  ( 12.00882698043040087, 1426.066405874380052, 202.8181785508519965 ) ) ;
#99659 = CARTESIAN_POINT ( 'NONE',  ( 2.354338606519999821, 1430.802573520589931, 217.9074022094590077 ) ) ;
#99660 = DIRECTION ( 'NONE',  ( 0.000000000000000000, 1.000000000000000000, 0.000000000000000000 ) ) ;
#99661 = CARTESIAN_POINT ( 'NONE',  ( -14.35469252290000064, 1416.832348304330026, 221.5787001177979789 ) ) ;
#99663 = EDGE_CURVE ( 'NONE', #100437, #5014, #41038, .T. ) ;
#99662 = FACE_OUTER_BOUND ( 'NONE', #55574, .T. ) ;
#99664 = CARTESIAN_POINT ( 'NONE',  ( 36.06124927020000115, 1445.049634744800187, 262.6648722463980334 ) ) ;
#99665 = CARTESIAN_POINT ( 'NONE',  ( 32.37018134260397062, 1511.187213306747708, 200.1723992780595438 ) ) ;
#99666 = CARTESIAN_POINT ( 'NONE',  ( -16.82407893874610139, 1420.448463740390025, 203.3157013238160289 ) ) ;
#99667 = CARTESIAN_POINT ( 'NONE',  ( -5.812333085687390266, 1457.439411062993941, 216.6809223546719068 ) ) ;
#99668 = CARTESIAN_POINT ( 'NONE',  ( -109.3076880190397020, 1387.423153082153476, 297.4241389203062909 ) ) ;
#99669 = CARTESIAN_POINT ( 'NONE',  ( 7.421564111899999538, 1419.755070490029993, 231.1403862899979913 ) ) ;
#99670 = CARTESIAN_POINT ( 'NONE',  ( 0.000000000000000000, 1512.413060387330006, 209.1218459616979999 ) ) ;
#99671 = FACE_OUTER_BOUND ( 'NONE', #11758, .T. ) ;
#99672 = DIRECTION ( 'NONE',  ( 0.000000000000000000, 1.000000000000000000, 0.000000000000000000 ) ) ;
#99673 = CARTESIAN_POINT ( 'NONE',  ( -7.571527303769999939, 1491.603552466590145, 211.0272147816089898 ) ) ;
#99674 = CARTESIAN_POINT ( 'NONE',  ( 18.81609481059999922, 1456.479165729590022, 204.5196734937790097 ) ) ;
#99675 = CARTESIAN_POINT ( 'NONE',  ( 21.76694865736958562, 1524.152444737676205, 183.4045613090604832 ) ) ;
#99676 = EDGE_CURVE ( 'NONE', #20182, #62097, #52960, .T. ) ;
#99677 = CARTESIAN_POINT ( 'NONE',  ( -0.7331377667929990238, 1515.470556211590065, 204.9034494321989825 ) ) ;
#99678 = CARTESIAN_POINT ( 'NONE',  ( 12.71887460719259977, 1426.545466713459973, 203.1631513952430055 ) ) ;
#99679 = DIRECTION ( 'NONE',  ( 0.6709778558543718630, 0.000000000000000000, -0.7414773880254675875 ) ) ;
#99680 = CARTESIAN_POINT ( 'NONE',  ( -5.681577072609999668, 1414.971279908829956, 225.1170751815979827 ) ) ;
#99681 = CARTESIAN_POINT ( 'NONE',  ( 0.2155153167960190130, 1454.260632470949986, 183.1993150321829944 ) ) ;
#99683 = VERTEX_POINT ( 'NONE', #56761 ) ;
#99682 = CARTESIAN_POINT ( 'NONE',  ( -13.31542525870250060, 1407.755358688280012, 207.9544151864530193 ) ) ;
#99684 = DIRECTION ( 'NONE',  ( 0.000000000000000000, 1.000000000000000000, 0.000000000000000000 ) ) ;
#99685 = EDGE_CURVE ( 'NONE', #104141, #85887, #103331, .T. ) ;
#99686 = CARTESIAN_POINT ( 'NONE',  ( -28.22512692420650282, 1509.373780534800062, 210.8894252387570134 ) ) ;
#99687 = CARTESIAN_POINT ( 'NONE',  ( 12.91294366230000179, 1434.774374641290024, 149.1897813115979829 ) ) ;
#99688 = CARTESIAN_POINT ( 'NONE',  ( -34.51820589334170108, 1435.725758536279955, 134.0999999979759707 ) ) ;
#99689 = CARTESIAN_POINT ( 'NONE',  ( 12.24119640919999874, 1442.732430062529829, 186.9125350121979920 ) ) ;
#99690 = VERTEX_POINT ( 'NONE', #92541 ) ;
#99691 = CARTESIAN_POINT ( 'NONE',  ( -17.12660205615338427, 1524.374578187333100, 180.9416429095477099 ) ) ;
#99692 = DIRECTION ( 'NONE',  ( -1.755985294532469921E-16, 1.000000000000000000, -1.338183447452831989E-16 ) ) ;
#99693 = CARTESIAN_POINT ( 'NONE',  ( 39.08053441540000250, 1436.812233320949872, 136.3561087622979926 ) ) ;
#99694 = CARTESIAN_POINT ( 'NONE',  ( -11.43172008590000033, 1490.909894833790077, 209.1362624142179811 ) ) ;
#99695 = CARTESIAN_POINT ( 'NONE',  ( -5.013264356492538099, 1375.413060387289761, 214.7179447576738482 ) ) ;
#99696 = CARTESIAN_POINT ( 'NONE',  ( 16.69548807383920064, 1509.501171630579847, 233.4225513957580063 ) ) ;
#99697 = AXIS2_PLACEMENT_3D ( 'NONE', #103418, #77690, #44097 ) ;
#99698 = CARTESIAN_POINT ( 'NONE',  ( 42.02056136452171842, 1427.554426610052360, 269.0752184054053373 ) ) ;
#99699 = CARTESIAN_POINT ( 'NONE',  ( -17.29393938232439965, 1523.621879633028811, 237.3864571009502242 ) ) ;
#99700 = CARTESIAN_POINT ( 'NONE',  ( -12.28572795910000082, 1378.826156777889992, 210.3262432577790264 ) ) ;
#99701 = CARTESIAN_POINT ( 'NONE',  ( -22.03465957474588066, 1522.862737210650039, 182.8300405912331428 ) ) ;
#99702 = CARTESIAN_POINT ( 'NONE',  ( -66.59252740955220418, 1385.094901321110001, 258.5833803216879687 ) ) ;
#99703 = CARTESIAN_POINT ( 'NONE',  ( -12.06665071716309967, 1491.071228040269943, 206.9060804303800012 ) ) ;
#99704 = CARTESIAN_POINT ( 'NONE',  ( 21.33070998320000200, 1509.431296620630064, 227.6602567435979836 ) ) ;
#99705 = ORIENTED_EDGE ( 'NONE', *, *, #11077, .T. ) ;
#99706 = CARTESIAN_POINT ( 'NONE',  ( -28.32839677941640133, 1508.625224776620144, 208.8290590941180085 ) ) ;
#99707 = CARTESIAN_POINT ( 'NONE',  ( -16.03670630470179859, 1410.715819712529992, 226.6960494820459928 ) ) ;
#99709 = ORIENTED_EDGE ( 'NONE', *, *, #65857, .T. ) ;
#99708 = CARTESIAN_POINT ( 'NONE',  ( -21.83550407203883736, 1523.678648413191695, 234.9693198511253627 ) ) ;
#99710 = CARTESIAN_POINT ( 'NONE',  ( -109.1310914430000167, 1384.891515483489911, 311.2646936322590250 ) ) ;
#99711 = CARTESIAN_POINT ( 'NONE',  ( 10.40693933779219904, 1471.062888143880173, 210.9539924980650198 ) ) ;
#99712 = ADVANCED_FACE ( 'NONE', ( #31540 ), #64627, .F. ) ;
#99713 = CARTESIAN_POINT ( 'NONE',  ( 17.77217598520769926, 1430.610759356409972, 213.2442890844889973 ) ) ;
#99714 = CARTESIAN_POINT ( 'NONE',  ( -109.1321484620000035, 1384.869787276959869, 311.2644936502589985 ) ) ;
#99715 = CARTESIAN_POINT ( 'NONE',  ( -0.1030177700933130047, 1419.835433905890113, 184.1455088873570105 ) ) ;
#99716 = CARTESIAN_POINT ( 'NONE',  ( 1.089618986890000141, 1466.173027012529928, 235.3909690008979965 ) ) ;
#99717 = CARTESIAN_POINT ( 'NONE',  ( 23.18583117279999684, 1410.644154559629897, 212.8685298154279906 ) ) ;
#99718 = CARTESIAN_POINT ( 'NONE',  ( -2.191379157991490079, 1412.648780287710224, 186.2800507015870153 ) ) ;
#99719 = CARTESIAN_POINT ( 'NONE',  ( -16.56403879315699967, 1464.818678847870160, 220.6315892174129942 ) ) ;
#99720 = CARTESIAN_POINT ( 'NONE',  ( -17.45904667960000012, 1423.446827278330147, 226.6221925633979879 ) ) ;
#99722 = CARTESIAN_POINT ( 'NONE',  ( -3.087788399999999989, 1439.686999668429962, 185.1123624746980170 ) ) ;
#99721 = CARTESIAN_POINT ( 'NONE',  ( -3.112702537996912433, 1511.889608914253358, 201.1973302697319070 ) ) ;
#99723 = CARTESIAN_POINT ( 'NONE',  ( 20.21728935790000037, 1475.862786327189951, 209.1218459616989946 ) ) ;
#99724 = CARTESIAN_POINT ( 'NONE',  ( -113.4000000000000057, 1366.350733876289951, 293.4380634648589989 ) ) ;
#99725 = CARTESIAN_POINT ( 'NONE',  ( -3.268503196014072465, 1371.061470524529796, 208.3718459617010978 ) ) ;
#99726 = CARTESIAN_POINT ( 'NONE',  ( -23.53568538760000095, 1430.818610655530165, 211.5316886895479911 ) ) ;
#99727 = AXIS2_PLACEMENT_3D ( 'NONE', #19695, #2933, #63397 ) ;
#99728 = CARTESIAN_POINT ( 'NONE',  ( 1.748848150599999984, 1360.440694539930064, 210.6218459616991936 ) ) ;
#99729 = CARTESIAN_POINT ( 'NONE',  ( -7.724423432224999608, 1517.122088787240045, 205.6676733166769964 ) ) ;
#99730 = CARTESIAN_POINT ( 'NONE',  ( -3.427607156821979917, 1485.816111524730104, 182.6024182081450249 ) ) ;
#99731 = ORIENTED_EDGE ( 'NONE', *, *, #84985, .F. ) ;
#99732 = CARTESIAN_POINT ( 'NONE',  ( -109.1655177890000061, 1384.872414444939977, 297.1329087538589420 ) ) ;
#99733 = PLANE ( 'NONE',  #35801 ) ;
#99736 = ORIENTED_EDGE ( 'NONE', *, *, #86544, .T. ) ;
#99735 = CARTESIAN_POINT ( 'NONE',  ( -68.71636368279999374, 1379.747847531599973, 280.3054625287589943 ) ) ;
#99734 = AXIS2_PLACEMENT_3D ( 'NONE', #104034, #45263, #1596 ) ;
#99737 = EDGE_LOOP ( 'NONE', ( #16980, #82417, #66704, #94654 ) ) ;
#99738 = CARTESIAN_POINT ( 'NONE',  ( -11.05880225982243381, 1378.497832814331559, 214.5800325812288918 ) ) ;
#99739 = ORIENTED_EDGE ( 'NONE', *, *, #106127, .F. ) ;
#99740 = VECTOR ( 'NONE', #1332, 999.9999999999998863 ) ;
#99741 = CARTESIAN_POINT ( 'NONE',  ( -2.037005282023119701, 1486.400766935479851, 220.8722278604369933 ) ) ;
#99742 = CARTESIAN_POINT ( 'NONE',  ( 11.43369621480000120, 1502.212434881789932, 208.0469179695890034 ) ) ;
#99744 = CARTESIAN_POINT ( 'NONE',  ( 15.93516857634840278, 1410.115694288839904, 191.7361898460559928 ) ) ;
#99743 = CARTESIAN_POINT ( 'NONE',  ( 0.7352107454670000486, 1428.413060387330006, 91.31218443469779800 ) ) ;
#99745 = CARTESIAN_POINT ( 'NONE',  ( 7.727327114725000001, 1517.232977404109988, 210.8318586907270173 ) ) ;
#99746 =( BOUNDED_CURVE ( )  B_SPLINE_CURVE ( 3, ( #68268, #41933, #76089, #25658 ),
 .UNSPECIFIED., .F., .T. ) 
 B_SPLINE_CURVE_WITH_KNOTS ( ( 4, 4 ),
 ( 4.149749351278939180, 5.275028794336680704 ),
 .UNSPECIFIED. ) 
 CURVE ( )  GEOMETRIC_REPRESENTATION_ITEM ( )  RATIONAL_B_SPLINE_CURVE ( ( 1.000000000000000000, 0.8972333180728662150, 0.8972333180728662150, 1.000000000000000000 ) ) 
 REPRESENTATION_ITEM ( '' )  );
#99747 = CARTESIAN_POINT ( 'NONE',  ( 40.22912568530000499, 1442.658719917350027, 137.0054168744979961 ) ) ;
#99748 = CARTESIAN_POINT ( 'NONE',  ( -106.9640595847560007, 1378.913060387289988, 307.1352131009099935 ) ) ;
#99749 = CARTESIAN_POINT ( 'NONE',  ( 3.552713678799999608E-15, 1507.551704408389924, 209.1218459616989946 ) ) ;
#99750 = CARTESIAN_POINT ( 'NONE',  ( 14.61595079141635622, 1462.229544524060429, 230.2230838894210478 ) ) ;
#99751 = APPLICATION_PROTOCOL_DEFINITION ( 'draft international standard', 'automotive_design', 1998, #9133 ) ;
#99752 = LINE ( 'NONE', #65635, #55202 ) ;
#99753 = DIRECTION ( 'NONE',  ( 0.9993902469235412811, 0.03489947644508400310, -0.001077449749359510062 ) ) ;
#99754 = CARTESIAN_POINT ( 'NONE',  ( -21.47380076839990082, 1487.892778387440103, 202.0847333328300124 ) ) ;
#99755 = DIRECTION ( 'NONE',  ( -1.000000000000000000, 0.000000000000000000, 0.000000000000000000 ) ) ;
#99756 = ORIENTED_EDGE ( 'NONE', *, *, #36336, .F. ) ;
#99757 = ORIENTED_EDGE ( 'NONE', *, *, #33639, .T. ) ;
#99758 = CARTESIAN_POINT ( 'NONE',  ( -6.470331913555000369, 1513.423632355040127, 216.5900188188570041 ) ) ;
#99759 = CARTESIAN_POINT ( 'NONE',  ( 18.07041998555298434, 1523.313115944345327, 238.0891100728146625 ) ) ;
#99760 = CARTESIAN_POINT ( 'NONE',  ( 0.002706352938670000211, 1450.912965879100057, 181.8859610906980038 ) ) ;
#99761 = VECTOR ( 'NONE', #19688, 1000.000000000000114 ) ;
#99762 = CARTESIAN_POINT ( 'NONE',  ( -21.11937805367519871, 1508.452816383899972, 209.9028812253390015 ) ) ;
#99763 = CARTESIAN_POINT ( 'NONE',  ( -2.500000000000000000, 1439.114301494319989, 157.7261950941980331 ) ) ;
#99764 = CARTESIAN_POINT ( 'NONE',  ( -13.17512049819999831, 1379.550058867589996, 208.3055830647739697 ) ) ;
#99765 = CARTESIAN_POINT ( 'NONE',  ( 36.37832868398670172, 1451.642701156830071, 135.3769930297369797 ) ) ;
#99766 = CARTESIAN_POINT ( 'NONE',  ( -2.031883754679999932, 1464.998375783689880, 198.3053765207990011 ) ) ;
#99767 = CARTESIAN_POINT ( 'NONE',  ( 26.68042020029999861, 1438.488799039590049, 136.9899190847980037 ) ) ;
#99768 = CARTESIAN_POINT ( 'NONE',  ( 7.490736227920000267, 1414.913060387329779, 194.7918206520979822 ) ) ;
#99769 = B_SPLINE_CURVE_WITH_KNOTS ( 'NONE', 3,
 ( #75771, #43279, #85249, #77425 ),
 .UNSPECIFIED., .F., .F.,
 ( 4, 4 ),
 ( 0.000000000000000000, 1.000000000000000000 ),
 .UNSPECIFIED. ) ;
#99770 = CARTESIAN_POINT ( 'NONE',  ( -72.30335119138749178, 1384.751552219569930, 270.5210238762560380 ) ) ;
#99771 = VERTEX_POINT ( 'NONE', #6887 ) ;
#99772 = CARTESIAN_POINT ( 'NONE',  ( 0.7391219670640019057, 1517.130100026000036, 202.1721425974470208 ) ) ;
#99773 = CARTESIAN_POINT ( 'NONE',  ( -2.881325412095000260, 1517.003078582959688, 208.0029426616869728 ) ) ;
#99774 = ORIENTED_EDGE ( 'NONE', *, *, #30123, .T. ) ;
#99775 = CARTESIAN_POINT ( 'NONE',  ( 34.26305872384260454, 1440.913060387330006, 259.7236778358719675 ) ) ;
#99776 = CARTESIAN_POINT ( 'NONE',  ( -0.0001975589939290832919, 1452.328857962840857, 153.7571063932752224 ) ) ;
#99777 = ORIENTED_EDGE ( 'NONE', *, *, #90389, .F. ) ;
#99778 = CARTESIAN_POINT ( 'NONE',  ( -113.4235965852909089, 1389.413060387289988, 305.2215675190763591 ) ) ;
#99779 = CARTESIAN_POINT ( 'NONE',  ( -15.51104348340000172, 1410.386807788529950, 191.0641050774980272 ) ) ;
#99780 = CARTESIAN_POINT ( 'NONE',  ( -6.790918657024139549, 1517.051704408389924, 184.0243675267330161 ) ) ;
#99781 = CARTESIAN_POINT ( 'NONE',  ( -10.92255993703960115, 1462.741395054350278, 207.3771677357329963 ) ) ;
#99782 = CARTESIAN_POINT ( 'NONE',  ( -4.316841735459999718, 1421.954789602430083, 184.7991042349980262 ) ) ;
#99783 = CARTESIAN_POINT ( 'NONE',  ( 10.96015508933500016, 1514.690994518219895, 225.0317485278669949 ) ) ;
#99785 = B_SPLINE_CURVE_WITH_KNOTS ( 'NONE', 5,
 ( #2232, #36900, #28506, #62705, #2780, #47519, #29063, #36348, #63248 ),
 .UNSPECIFIED., .F., .F.,
 ( 6, 3, 6 ),
 ( 0.000000000000000000, 0.9874393323384224042, 1.000000000000000000 ),
 .UNSPECIFIED. ) ;
#99784 = CARTESIAN_POINT ( 'NONE',  ( -19.05930086066416962, 1517.151704408390060, 223.0490131529958262 ) ) ;
#99786 = CARTESIAN_POINT ( 'NONE',  ( -5.773315255633579390, 1510.559702728003685, 201.5815081783346727 ) ) ;
#99787 = CARTESIAN_POINT ( 'NONE',  ( -21.13130013988163114, 1524.397344074317971, 180.8335768739890455 ) ) ;
#99789 = CARTESIAN_POINT ( 'NONE',  ( -10.10004869885101009, 1422.222932908415260, 137.0999999980978714 ) ) ;
#99788 = CARTESIAN_POINT ( 'NONE',  ( 17.22921662220000272, 1459.838650815730034, 228.5711330225980191 ) ) ;
#99790 = CARTESIAN_POINT ( 'NONE',  ( -4.618315814097702976, 1422.106628702972557, 184.6512326330956171 ) ) ;
#99791 = CIRCLE ( 'NONE', #51526, 2.000000000000001776 ) ;
#99792 = CARTESIAN_POINT ( 'NONE',  ( -7.329930051325000306, 1516.881930554049859, 216.8399805996670011 ) ) ;
#99793 = ORIENTED_EDGE ( 'NONE', *, *, #104995, .T. ) ;
#99794 = DIRECTION ( 'NONE',  ( -0.6736849260863841948, 0.000000000000000000, 0.7390186874254148774 ) ) ;
#99795 = CARTESIAN_POINT ( 'NONE',  ( 5.213129316145000303, 1514.517422889960017, 200.4652853224170030 ) ) ;
#99796 = CARTESIAN_POINT ( 'NONE',  ( 16.73897281474028631, 1449.350004377781488, 218.9967825959608092 ) ) ;
#99797 = CARTESIAN_POINT ( 'NONE',  ( -1.119717754394999876, 1517.038650117239968, 212.5846815975970117 ) ) ;
#99798 = CARTESIAN_POINT ( 'NONE',  ( 18.52446843400000276, 1509.559949079429998, 186.5302684548980210 ) ) ;
#99799 = CARTESIAN_POINT ( 'NONE',  ( -2.022453434156979757, 1483.801003577689926, 198.6380168107399982 ) ) ;
#99801 = ORIENTED_EDGE ( 'NONE', *, *, #89858, .F. ) ;
#99800 = CARTESIAN_POINT ( 'NONE',  ( 4.429741920660830168, 1508.551704408389924, 213.9240898912200066 ) ) ;
#99802 = CARTESIAN_POINT ( 'NONE',  ( -18.65451756193940014, 1507.632629711779828, 229.7110761618599781 ) ) ;
#99803 = CARTESIAN_POINT ( 'NONE',  ( 24.59498549419999947, 1440.913060393719888, 213.3385281389280124 ) ) ;
#99804 = CARTESIAN_POINT ( 'NONE',  ( -11.86483741480000198, 1432.251307157519932, 150.3967669623980044 ) ) ;
#99805 = CARTESIAN_POINT ( 'NONE',  ( -0.4895834631420010186, 1430.089577145089834, 214.7663758875890210 ) ) ;
#99806 = CARTESIAN_POINT ( 'NONE',  ( -4.360112039636049985, 1441.644505157019921, 201.4346413363180091 ) ) ;
#99807 = CARTESIAN_POINT ( 'NONE',  ( 6.330596736919809508, 1422.104800651550022, 147.4057713054710064 ) ) ;
#99808 = CARTESIAN_POINT ( 'NONE',  ( 16.85976061912560908, 1525.821544997590536, 182.0492613858611719 ) ) ;
#99809 = VECTOR ( 'NONE', #41019, 1000.000000000000000 ) ;
#99810 = CARTESIAN_POINT ( 'NONE',  ( -8.588225070092541102, 1439.751992671629978, 226.1486124413150094 ) ) ;
#99812 = CARTESIAN_POINT ( 'NONE',  ( -10.64685008816380041, 1482.274716053820157, 206.1670479490190360 ) ) ;
#99811 = CARTESIAN_POINT ( 'NONE',  ( -20.25856915909999856, 1457.444690063829967, 224.8321900254979937 ) ) ;
#99813 = CARTESIAN_POINT ( 'NONE',  ( 19.26216268010000121, 1457.979299265790132, 211.9620131672190269 ) ) ;
#99814 = ORIENTED_EDGE ( 'NONE', *, *, #71695, .F. ) ;
#99816 = AXIS2_PLACEMENT_3D ( 'NONE', #5929, #91585, #33312 ) ;
#99815 = CARTESIAN_POINT ( 'NONE',  ( 3.446329775655000205, 1516.812046502680005, 206.2422037788969931 ) ) ;
#99817 = CARTESIAN_POINT ( 'NONE',  ( 3.401339724939999698, 1406.599585306829795, 269.4945997090979972 ) ) ;
#99818 = CARTESIAN_POINT ( 'NONE',  ( -0.1600491160670000079, 1410.295025987830059, 185.0245251824980244 ) ) ;
#99819 = VECTOR ( 'NONE', #16886, 1000.000000000000000 ) ;
#99820 = CARTESIAN_POINT ( 'NONE',  ( 18.23351301940000369, 1410.878721802529981, 193.8722903718979751 ) ) ;
#99821 = EDGE_CURVE ( 'NONE', #7253, #23788, #90879, .T. ) ;
#99822 = CARTESIAN_POINT ( 'NONE',  ( 24.18941653212194254, 1436.492649024060938, 213.3767979003249025 ) ) ;
#99823 = DIRECTION ( 'NONE',  ( 0.000000000000000000, 0.000000000000000000, 1.000000000000000000 ) ) ;
#99824 = CARTESIAN_POINT ( 'NONE',  ( -0.5697989934069560558, 1450.893162568020216, 155.6080925154190027 ) ) ;
#99825 = TOROIDAL_SURFACE ( 'NONE', #37270, 32.13701971169416538, 1.000000000000000000 ) ;
#99826 = CARTESIAN_POINT ( 'NONE',  ( -6.574341282982393508, 1439.975808622007889, 203.3270148206125612 ) ) ;
#99827 = CARTESIAN_POINT ( 'NONE',  ( -1.177008307996480152, 1450.813907466269711, 155.0627524578040095 ) ) ;
#99828 = CARTESIAN_POINT ( 'NONE',  ( -12.41051836359999960, 1445.069699529200079, 185.9600399849980192 ) ) ;
#99829 = EDGE_CURVE ( 'NONE', #38215, #104547, #67641, .T. ) ;
#99830 = CARTESIAN_POINT ( 'NONE',  ( -19.88955515405384133, 1484.852955906364514, 190.9985515883152516 ) ) ;
#99831 = CARTESIAN_POINT ( 'NONE',  ( -14.13596061218840028, 1415.658863692520072, 221.0621937284620060 ) ) ;
#99832 = CARTESIAN_POINT ( 'NONE',  ( -10.94721987830000032, 1499.473939016889972, 212.6801052600889932 ) ) ;
#99833 = CARTESIAN_POINT ( 'NONE',  ( -9.100166781252440273, 1409.230845213859993, 197.2463952335830015 ) ) ;
#99834 = CARTESIAN_POINT ( 'NONE',  ( -26.96340810044629777, 1508.002441355999736, 211.5727766284590246 ) ) ;
#99835 = CARTESIAN_POINT ( 'NONE',  ( 2.500000000000000000, 1438.975727077510101, 156.0986697955979992 ) ) ;
#99836 = CARTESIAN_POINT ( 'NONE',  ( -2.776721148250000049, 1475.989443049229976, 268.4805436461979866 ) ) ;
#99838 = AXIS2_PLACEMENT_3D ( 'NONE', #46223, #106103, #89844 ) ;
#99837 = CARTESIAN_POINT ( 'NONE',  ( -4.226172892403809556, 1446.259735967549886, 166.0433939504960108 ) ) ;
#99839 = CARTESIAN_POINT ( 'NONE',  ( 8.723134474349999223, 1451.781317889190177, 212.2855316608589931 ) ) ;
#99840 = CARTESIAN_POINT ( 'NONE',  ( 1.484142863822459857, 1526.349689584397083, 239.9035297921357142 ) ) ;
#99841 = CARTESIAN_POINT ( 'NONE',  ( -42.50846000140169423, 1384.776023261829778, 246.7016633287670118 ) ) ;
#99842 = CARTESIAN_POINT ( 'NONE',  ( -10.61999372029469946, 1462.990852176999852, 206.0510140530389833 ) ) ;
#99843 = CARTESIAN_POINT ( 'NONE',  ( -17.71193101166619854, 1517.051704408389924, 221.5709757775249784 ) ) ;
#99844 = CARTESIAN_POINT ( 'NONE',  ( -105.4748898929999967, 1378.947219630530071, 303.4796662018589473 ) ) ;
#99845 = DIRECTION ( 'NONE',  ( -0.000000000000000000, -1.000000000000000000, -0.000000000000000000 ) ) ;
#99846 = CARTESIAN_POINT ( 'NONE',  ( 8.184191755800993562, 1511.478973222094055, 205.1565754550810254 ) ) ;
#99847 = CARTESIAN_POINT ( 'NONE',  ( -19.70672637799999904, 1410.962757928930159, 197.6880275815980212 ) ) ;
#99848 = CARTESIAN_POINT ( 'NONE',  ( -4.633397096295920115, 1377.913060387289988, 213.8868415672910146 ) ) ;
#99849 = CYLINDRICAL_SURFACE ( 'NONE', #80140, 1.999999999999999556 ) ;
#99850 = ORIENTED_EDGE ( 'NONE', *, *, #102365, .F. ) ;
#99851 = CARTESIAN_POINT ( 'NONE',  ( -6.872280032289999063, 1472.400811630890075, 210.0671059703809931 ) ) ;
#99852 = DIRECTION ( 'NONE',  ( 1.755985294532469921E-16, -1.000000000000000000, 1.338183447452831989E-16 ) ) ;
#99853 = CARTESIAN_POINT ( 'NONE',  ( -18.47518245109339929, 1466.235720590640085, 200.8822878488529966 ) ) ;
#99855 = DIRECTION ( 'NONE',  ( 1.836970198721029688E-16, 1.000000000000000000, 0.000000000000000000 ) ) ;
#99854 = CARTESIAN_POINT ( 'NONE',  ( 11.08531958919999916, 1425.204049180429820, 139.6337526468980172 ) ) ;
#99856 = DIRECTION ( 'NONE',  ( -0.6736849260863839728, 0.000000000000000000, 0.7390186874254150995 ) ) ;
#99857 = DIRECTION ( 'NONE',  ( -1.000000000000000000, 0.000000000000000000, 0.000000000000000000 ) ) ;
#99858 = CARTESIAN_POINT ( 'NONE',  ( 39.86302261571789529, 1446.848482913750104, 136.6554637131669949 ) ) ;
#99859 = CARTESIAN_POINT ( 'NONE',  ( 4.615017327834999961, 1516.987478262539980, 202.5620478758069964 ) ) ;
#99860 = CARTESIAN_POINT ( 'NONE',  ( 7.586419159530000123, 1426.023150451340143, 212.1170382088889994 ) ) ;
#99861 = CARTESIAN_POINT ( 'NONE',  ( -12.73682884018698758, 1398.290620877891797, 211.7349528390541593 ) ) ;
#99862 = CARTESIAN_POINT ( 'NONE',  ( 15.85140261003499873, 1511.863761374039996, 197.3804798592670124 ) ) ;
#99863 = CARTESIAN_POINT ( 'NONE',  ( -15.80819117724120026, 1420.947422077100100, 203.3790723405460028 ) ) ;
#99864 = CARTESIAN_POINT ( 'NONE',  ( -18.09482676940919887, 1377.903424712840206, 213.0196949892159921 ) ) ;
#99865 = CARTESIAN_POINT ( 'NONE',  ( 20.81497463947879822, 1509.689032670049983, 230.4046146822830110 ) ) ;
#99867 = ORIENTED_EDGE ( 'NONE', *, *, #35083, .T. ) ;
#99866 = CARTESIAN_POINT ( 'NONE',  ( -36.41835043334280186, 1379.641566369280099, 223.8136772429340056 ) ) ;
#99868 = ORIENTED_EDGE ( 'NONE', *, *, #67162, .F. ) ;
#99869 = CARTESIAN_POINT ( 'NONE',  ( -2.328768353080000075, 1395.994382770230231, 220.1364017053979865 ) ) ;
#99870 = CARTESIAN_POINT ( 'NONE',  ( -21.63131569299999768, 1410.588498113729884, 216.4024978495980065 ) ) ;
#99871 = VERTEX_POINT ( 'NONE', #92001 ) ;
#99872 = CARTESIAN_POINT ( 'NONE',  ( -13.33598659858382618, 1444.533481128697531, 169.3750784523817003 ) ) ;
#99873 = CARTESIAN_POINT ( 'NONE',  ( 21.89171915302359039, 1509.706674751428181, 229.1511294852978438 ) ) ;
#99874 = DIRECTION ( 'NONE',  ( 0.000000000000000000, 0.000000000000000000, -1.000000000000000000 ) ) ;
#99876 = CARTESIAN_POINT ( 'NONE',  ( -13.74978541103059904, 1508.254514242250025, 184.1447064633670152 ) ) ;
#99875 = CARTESIAN_POINT ( 'NONE',  ( -8.861333410889999485, 1384.870662623869976, 218.6848950059889773 ) ) ;
#99877 = CARTESIAN_POINT ( 'NONE',  ( 1.415376035039999758, 1449.240524800240109, 183.6130213356980221 ) ) ;
#99878 = CARTESIAN_POINT ( 'NONE',  ( -4.669740627984789505, 1464.328320229509927, 199.6059302412689931 ) ) ;
#99879 = CARTESIAN_POINT ( 'NONE',  ( -17.13142892129999950, 1417.632139391989995, 207.5091448026290095 ) ) ;
#99880 = SURFACE_STYLE_USAGE ( .BOTH. , #66333 ) ;
#99881 = B_SPLINE_SURFACE_WITH_KNOTS ( 'NONE', 5, 5, ( 
 ( #82808, #41375, #66041, #30188, #100165, #14492, #40256, #15577, #64382 ),
 ( #6655, #91211, #100702, #109137, #21771, #55972, #75540, #65485, #92307 ),
 ( #40809, #74987, #99594, #98503, #90096, #39713, #90652, #32419, #13379 ),
 ( #6101, #74438, #48123, #23449, #81691, #83911, #39142, #107455, #30750 ),
 ( #64931, #57644, #99044, #22322, #13936, #82262, #73877, #108005, #93124 ),
 ( #84718, #60104, #41071, #85267, #24792, #83617, #42184, #50043, #51141 ) ),
 .UNSPECIFIED., .F., .F., .F.,
 ( 6, 6 ),
 ( 6, 3, 6 ),
 ( 0.000000000000000000, 9.931187219381479636 ),
 ( 0.000000000000000000, 1.000000000000000000, 2.000000002426730372 ),
 .UNSPECIFIED. ) ;
#99882 = CARTESIAN_POINT ( 'NONE',  ( 5.771317186272449717, 1396.114599253079859, 199.7147697363969883 ) ) ;
#99883 = CARTESIAN_POINT ( 'NONE',  ( 1.237038659510000027, 1415.048591087029763, 191.5546371455980079 ) ) ;
#99884 = CARTESIAN_POINT ( 'NONE',  ( 11.78240326789999948, 1427.379900601830059, 147.2810486092980113 ) ) ;
#99885 = CARTESIAN_POINT ( 'NONE',  ( 2.409586283469999923, 1426.663880916129983, 144.1938086916980239 ) ) ;
#99886 = ORIENTED_EDGE ( 'NONE', *, *, #64539, .F. ) ;
#99887 = CARTESIAN_POINT ( 'NONE',  ( 13.12526434545569920, 1435.132197141100050, 150.0848052037160016 ) ) ;
#99888 = CARTESIAN_POINT ( 'NONE',  ( 0.000000000000000000, 1391.913060387289988, 209.1218459616989946 ) ) ;
#99889 = ORIENTED_EDGE ( 'NONE', *, *, #499, .T. ) ;
#99890 = ORIENTED_EDGE ( 'NONE', *, *, #16453, .F. ) ;
#99891 = CARTESIAN_POINT ( 'NONE',  ( -18.49177796861540202, 1468.166699000810013, 228.2165253284340167 ) ) ;
#99892 = CARTESIAN_POINT ( 'NONE',  ( -2.799250156989999905, 1466.496106898330027, 235.0820921407980109 ) ) ;
#99893 = CIRCLE ( 'NONE', #33716, 32.13701971169416538 ) ;
#99894 = CARTESIAN_POINT ( 'NONE',  ( -108.2218672464631197, 1388.808672301278648, 310.1868769870816323 ) ) ;
#99895 = CARTESIAN_POINT ( 'NONE',  ( 0.01171160595180150039, 1516.939568781210028, 215.6786969668069958 ) ) ;
#99896 = CARTESIAN_POINT ( 'NONE',  ( -13.74255644588489922, 1380.321565345840099, 209.5209940965139879 ) ) ;
#99897 = AXIS2_PLACEMENT_3D ( 'NONE', #34628, #78860, #53108 ) ;
#99898 = ORIENTED_EDGE ( 'NONE', *, *, #39908, .T. ) ;
#99899 = CARTESIAN_POINT ( 'NONE',  ( -12.50356189400000062, 1503.103369310989819, 208.6063100965829733 ) ) ;
#99900 = CARTESIAN_POINT ( 'NONE',  ( 2.500000000000000000, 1448.271836152329797, 165.0530739316030235 ) ) ;
#99901 = CARTESIAN_POINT ( 'NONE',  ( -57.85314987360000316, 1374.895658628189949, 259.2190729278590311 ) ) ;
#99902 = AXIS2_PLACEMENT_3D ( 'NONE', #58783, #100754, #94570 ) ;
#99903 = EDGE_CURVE ( 'NONE', #97183, #81284, #98747, .T. ) ;
#99904 = ORIENTED_EDGE ( 'NONE', *, *, #96617, .T. ) ;
#99905 = CARTESIAN_POINT ( 'NONE',  ( -3.267603553834999897, 1516.858171774179937, 205.8687047948669999 ) ) ;
#99906 = ORIENTED_EDGE ( 'NONE', *, *, #83792, .T. ) ;
#99907 = CARTESIAN_POINT ( 'NONE',  ( 3.455495833855000143, 1516.939877939420057, 209.1085718841020196 ) ) ;
#99908 = CARTESIAN_POINT ( 'NONE',  ( -20.84366584300000014, 1509.634592552130016, 230.0407975123980009 ) ) ;
#99909 = ADVANCED_FACE ( 'NONE', ( #39398 ), #15018, .F. ) ;
#99911 = ADVANCED_FACE ( 'NONE', ( #100403 ), #34823, .F. ) ;
#99910 = CARTESIAN_POINT ( 'NONE',  ( -29.91807324427193748, 1419.517122880768056, 269.4699333455887995 ) ) ;
#99912 = CARTESIAN_POINT ( 'NONE',  ( 6.262845557134999908, 1511.198876514819858, 216.5713750547470227 ) ) ;
#99914 = ORIENTED_EDGE ( 'NONE', *, *, #85030, .F. ) ;
#99913 = CARTESIAN_POINT ( 'NONE',  ( 0.007886336566007640797, 1415.935475482089942, 227.0236970807289936 ) ) ;
#99915 = CARTESIAN_POINT ( 'NONE',  ( 24.57126086520000285, 1440.930726575820017, 213.1726801958579927 ) ) ;
#99916 = CARTESIAN_POINT ( 'NONE',  ( -32.83528556352659677, 1440.913060389920020, 246.2013707445869954 ) ) ;
#99917 = CARTESIAN_POINT ( 'NONE',  ( -67.04611378480001349, 1384.669946114650202, 292.1828053715589704 ) ) ;
#99918 = CARTESIAN_POINT ( 'NONE',  ( -0.2727009628635130301, 1465.116480817439879, 238.1272600893040021 ) ) ;
#99919 = STYLED_ITEM ( 'NONE', ( #52705 ), #84353 ) ;
#99920 = CARTESIAN_POINT ( 'NONE',  ( 15.21920960200000117, 1410.493944514729947, 270.4035064526980250 ) ) ;
#99921 = CARTESIAN_POINT ( 'NONE',  ( -2.479246885834999858, 1516.983612918759945, 213.1658362778269691 ) ) ;
#99922 = CARTESIAN_POINT ( 'NONE',  ( 23.73706522670000041, 1410.130559204529845, 209.1801705544619949 ) ) ;
#99923 = CARTESIAN_POINT ( 'NONE',  ( 29.36670733768142227, 1526.000688113686692, 197.3383209345576006 ) ) ;
#99924 = CARTESIAN_POINT ( 'NONE',  ( -3.467940587273969921, 1495.562067866610050, 197.2905559816869925 ) ) ;
#99925 = CARTESIAN_POINT ( 'NONE',  ( -7.709535243742100086, 1516.553531807379841, 210.7548730175080038 ) ) ;
#99927 = B_SPLINE_CURVE_WITH_KNOTS ( 'NONE', 5,
 ( #56667, #90803, #98097, #47166, #55578, #14084, #38742, #57782, #40395 ),
 .UNSPECIFIED., .F., .F.,
 ( 6, 3, 6 ),
 ( 0.000000000000000000, 0.3780778814934559473, 1.000000000000000000 ),
 .UNSPECIFIED. ) ;
#99926 = CARTESIAN_POINT ( 'NONE',  ( -6.548200625775000283, 1516.632821972880038, 210.2524534341069966 ) ) ;
#99928 = CARTESIAN_POINT ( 'NONE',  ( -3.381815025240311634, 1447.294493428453052, 154.8487956087455473 ) ) ;
#99929 = DIRECTION ( 'NONE',  ( -0.9942586961433742543, 0.000000000000000000, 0.1070030146457445069 ) ) ;
#99930 = CARTESIAN_POINT ( 'NONE',  ( -10.11438356259093041, 1486.011445013448338, 183.8897573256294322 ) ) ;
#99932 = EDGE_LOOP ( 'NONE', ( #104023, #24955, #72438 ) ) ;
#99931 = CARTESIAN_POINT ( 'NONE',  ( -22.00954832700000097, 1389.608130893230054, 205.5395550013790285 ) ) ;
#99933 = CARTESIAN_POINT ( 'NONE',  ( -42.90628611040540363, 1385.165074035010093, 247.4351966983790021 ) ) ;
#99934 = CARTESIAN_POINT ( 'NONE',  ( 18.90749324119999741, 1416.833018152629847, 210.0260543018609951 ) ) ;
#99935 = DIRECTION ( 'NONE',  ( 0.9455185755993178454, 0.000000000000000000, -0.3255681544571537578 ) ) ;
#99936 = EDGE_CURVE ( 'NONE', #104782, #109848, #59699, .T. ) ;
#99937 = CARTESIAN_POINT ( 'NONE',  ( -8.878956589741459737, 1509.223142555890036, 236.7286733813189983 ) ) ;
#99938 = B_SPLINE_CURVE_WITH_KNOTS ( 'NONE', 5,
 ( #95318, #28667, #36513, #61741, #38160, #62872, #96424, #62297, #12404 ),
 .UNSPECIFIED., .F., .F.,
 ( 6, 3, 6 ),
 ( -157.9539410499999974, -142.4618993580000108, -78.28065404276159711 ),
 .UNSPECIFIED. ) ;
#99939 = LINE ( 'NONE', #40046, #9795 ) ;
#99940 = CARTESIAN_POINT ( 'NONE',  ( 12.54060419009999983, 1427.026833031130082, 206.2830509747190035 ) ) ;
#99941 = CARTESIAN_POINT ( 'NONE',  ( -1.637258856660000150, 1483.893433971690001, 198.5669146070989939 ) ) ;
#99943 = CARTESIAN_POINT ( 'NONE',  ( -7.769040032840000443, 1384.899909079960025, 218.9179066534690037 ) ) ;
#99942 = CARTESIAN_POINT ( 'NONE',  ( -5.003848160104999998, 1517.005755693489846, 216.4561742428970206 ) ) ;
#99944 = CARTESIAN_POINT ( 'NONE',  ( 8.884590929279953642, 1458.997830320633511, 202.8087306969714518 ) ) ;
#99945 = CARTESIAN_POINT ( 'NONE',  ( -3.347801439296141712, 1523.382868172864164, 176.1543725841967500 ) ) ;
#99946 = ORIENTED_EDGE ( 'NONE', *, *, #35723, .T. ) ;
#99947 = CARTESIAN_POINT ( 'NONE',  ( 2.871580388595000422, 1517.129577905929864, 202.1716309988170224 ) ) ;
#99948 = CARTESIAN_POINT ( 'NONE',  ( -16.28235098596499952, 1514.570049710740022, 223.9522021028669769 ) ) ;
#99949 = FACE_OUTER_BOUND ( 'NONE', #64107, .T. ) ;
#99950 = VECTOR ( 'NONE', #15673, 1000.000000000000000 ) ;
#99951 = CARTESIAN_POINT ( 'NONE',  ( 19.81774543710000103, 1455.367724597530014, 224.1005748771979995 ) ) ;
#99952 = CARTESIAN_POINT ( 'NONE',  ( 10.92804747355420147, 1461.442164761259846, 210.0201248578009938 ) ) ;
#99953 = CARTESIAN_POINT ( 'NONE',  ( 7.591975344036550055, 1510.802068165409992, 203.6262312139739947 ) ) ;
#99954 = CARTESIAN_POINT ( 'NONE',  ( -0.9256615464240010027, 1443.221293306289908, 218.6972998774490122 ) ) ;
#99955 = CARTESIAN_POINT ( 'NONE',  ( 15.42145445766184686, 1420.877149889689235, 227.7429447766757846 ) ) ;
#99956 = AXIS2_PLACEMENT_3D ( 'NONE', #98230, #89833, #9409 ) ;
#99957 = CARTESIAN_POINT ( 'NONE',  ( 39.97998863047710216, 1445.784950460129949, 136.8350985949439860 ) ) ;
#99958 = CARTESIAN_POINT ( 'NONE',  ( -20.09064370129999944, 1427.417574131329957, 223.6716081326979975 ) ) ;
#99959 = AXIS2_PLACEMENT_3D ( 'NONE', #17672, #77076, #33382 ) ;
#99960 = CARTESIAN_POINT ( 'NONE',  ( -20.60448988230000111, 1484.737042837089803, 209.1218459616989946 ) ) ;
#99961 = CARTESIAN_POINT ( 'NONE',  ( -108.1807521070000035, 1387.239101882400064, 297.7772244688590035 ) ) ;
#99962 = ADVANCED_FACE ( 'NONE', ( #8507, #49983 ), #33710, .F. ) ;
#99963 = CARTESIAN_POINT ( 'NONE',  ( 19.58740883549999978, 1488.302744340930076, 189.9643116126979976 ) ) ;
#99964 = CARTESIAN_POINT ( 'NONE',  ( -0.01757669524774119890, 1409.855414155669905, 233.2048809017120163 ) ) ;
#99965 = CARTESIAN_POINT ( 'NONE',  ( -35.03848265734369960, 1457.732937364906093, 269.5320884425483428 ) ) ;
#99966 = ORIENTED_EDGE ( 'NONE', *, *, #22687, .T. ) ;
#99967 = CARTESIAN_POINT ( 'NONE',  ( 0.000000000000000000, 1512.187213306747481, 209.1218459616979999 ) ) ;
#99968 = CARTESIAN_POINT ( 'NONE',  ( -19.60062230800302885, 1409.993166476541774, 269.5268391383848439 ) ) ;
#99969 = CARTESIAN_POINT ( 'NONE',  ( 32.39779788405888894, 1524.816846803860926, 201.1912884557872303 ) ) ;
#99970 = CARTESIAN_POINT ( 'NONE',  ( -10.60236678890000128, 1431.113060387329824, 224.6557647168980338 ) ) ;
#99971 = B_SPLINE_CURVE_WITH_KNOTS ( 'NONE', 3,
 ( #48669, #40241, #25074, #84454, #84987, #100149 ),
 .UNSPECIFIED., .F., .F.,
 ( 4, 2, 4 ),
 ( 1.000000006357030081E-06, 0.7542730840691190819, 1.502771284927904238 ),
 .UNSPECIFIED. ) ;
#99972 = CARTESIAN_POINT ( 'NONE',  ( 11.60004869885203327, 1428.043774929915571, 134.2198016428816914 ) ) ;
#99973 = CARTESIAN_POINT ( 'NONE',  ( -12.92817269062425467, 1442.906901620904819, 186.4515505936974762 ) ) ;
#99974 = DIRECTION ( 'NONE',  ( -0.8564730265368828421, -0.5161917810414574648, 0.000000000000000000 ) ) ;
#99975 = CARTESIAN_POINT ( 'NONE',  ( -3.465081665767479890, 1515.493283046529996, 213.0346231893849733 ) ) ;
#99976 = CIRCLE ( 'NONE', #41000, 30.13701971169416183 ) ;
#99977 = CARTESIAN_POINT ( 'NONE',  ( -2.773560967585325887, 1415.718487882860018, 232.8280475519434560 ) ) ;
#99978 = CARTESIAN_POINT ( 'NONE',  ( -14.98124668174299856, 1415.677402202029953, 207.3353217124920036 ) ) ;
#99979 = CIRCLE ( 'NONE', #21310, 3.750000000000000000 ) ;
#99980 = CARTESIAN_POINT ( 'NONE',  ( 23.85742997590000414, 1435.349283830410059, 137.3962418501980380 ) ) ;
#99981 = CARTESIAN_POINT ( 'NONE',  ( -12.17813008270000097, 1438.571549855089870, 224.0393728361989929 ) ) ;
#99984 = EDGE_LOOP ( 'NONE', ( #74889, #46524, #68762, #3915, #85024 ) ) ;
#99983 = CARTESIAN_POINT ( 'NONE',  ( -13.55937074789999919, 1409.552479676130133, 226.6517356775979977 ) ) ;
#99982 = B_SPLINE_CURVE_WITH_KNOTS ( 'NONE', 5,
 ( #55609, #47193, #99213, #81319, #4633, #38771, #72945, #107083, #64562 ),
 .UNSPECIFIED., .F., .F.,
 ( 6, 3, 6 ),
 ( 0.000000000000000000, 0.4153918097741242099, 1.000000000000000000 ),
 .UNSPECIFIED. ) ;
#99985 = CARTESIAN_POINT ( 'NONE',  ( 0.1496009369300290159, 1415.938742849230039, 191.1448484385929873 ) ) ;
#99986 = CARTESIAN_POINT ( 'NONE',  ( -0.5979851740210000433, 1408.933942489730043, 231.6757385099979842 ) ) ;
#99987 = EDGE_LOOP ( 'NONE', ( #72267, #69744, #90668, #30883 ) ) ;
#99988 = EDGE_LOOP ( 'NONE', ( #40002, #45143, #86321, #92071, #107499, #45872 ) ) ;
#99989 = CARTESIAN_POINT ( 'NONE',  ( 18.09157779502649888, 1416.524489948229984, 209.0416182593249914 ) ) ;
#99990 = CARTESIAN_POINT ( 'NONE',  ( -20.21716934224603079, 1526.104292489135332, 233.6939662645372380 ) ) ;
#99992 = CARTESIAN_POINT ( 'NONE',  ( -26.35776619319999980, 1444.383684710270018, 225.2710189609979921 ) ) ;
#99991 = CARTESIAN_POINT ( 'NONE',  ( 3.209129091579999926, 1455.228273979189908, 218.1432107165790057 ) ) ;
#99993 = B_SPLINE_CURVE_WITH_KNOTS ( 'NONE', 3,
 ( #39190, #66639, #57131, #30238, #91258, #91800, #14538, #100740, #64973, #23494, #24024, #31899, #65529, #58224, #98548, #22366, #48727, #6142, #108049, #92347, #82309, #48171, #81194, #5607, #40853, #32464, #40300, #21817, #74483, #15620, #107505, #90696, #108610, #100212, #57686, #15079, #13983, #31345, #39760, #49273, #83401, #6698, #75028, #4512, #47613, #109179, #38644, #13423, #81737, #5045, #85595, #67733, #94007, #50381, #9460 ),
 .UNSPECIFIED., .F., .F.,
 ( 4, 3, 3, 3, 3, 3, 3, 3, 3, 3, 3, 3, 3, 3, 3, 3, 3, 3, 4 ),
 ( 9.902195898180000455, 10.17210527305359946, 10.45530577770680125, 10.70141353110000004, 11.00396970308290001, 11.32322756685609910, 11.52456852350000105, 11.84989040654409997, 12.16242387770059885, 12.38020728900000123, 12.74551463658920092, 13.12275145097450135, 13.53252099856520019, 13.95359103768650044, 14.40783883234479923, 14.91487510226109947, 15.44821056776079971, 15.94145638524880049, 16.40090783169999966 ),
 .UNSPECIFIED. ) ;
#99994 = CARTESIAN_POINT ( 'NONE',  ( -3.026951662149999667, 1443.662240191790033, 218.7413276925990147 ) ) ;
#99995 = CARTESIAN_POINT ( 'NONE',  ( -11.87691384789999915, 1433.083180736939994, 150.0777257821980015 ) ) ;
#99996 = ADVANCED_FACE ( 'NONE', ( #103115 ), #74379, .T. ) ;
#99997 = CARTESIAN_POINT ( 'NONE',  ( 4.208240993269999564, 1434.939300248989866, 227.0651965576989824 ) ) ;
#99998 = AXIS2_PLACEMENT_3D ( 'NONE', #33960, #93312, #35613 ) ;
#99999 = CARTESIAN_POINT ( 'NONE',  ( 25.37391927814179837, 1441.218297505840155, 209.5413194381530104 ) ) ;
#100000 = ADVANCED_FACE ( 'NONE', ( #69010 ), #42601, .F. ) ;
#100001 = CARTESIAN_POINT ( 'NONE',  ( -27.50325879720000444, 1440.422393616930094, 137.1890872278979998 ) ) ;
#100002 = CARTESIAN_POINT ( 'NONE',  ( -24.17043414239999777, 1438.260851936789777, 211.4235143265279930 ) ) ;
#100003 = FACE_BOUND ( 'NONE', #7660, .T. ) ;
#100004 = CARTESIAN_POINT ( 'NONE',  ( -11.60387536552270049, 1481.105535834539978, 211.4044418330699955 ) ) ;
#100005 = CARTESIAN_POINT ( 'NONE',  ( 7.699968550499718845, 1364.464658747520616, 209.6218459617148824 ) ) ;
#100006 = CARTESIAN_POINT ( 'NONE',  ( -11.47024688358358091, 1509.438411113718075, 236.8433996648743687 ) ) ;
#100008 = ORIENTED_EDGE ( 'NONE', *, *, #58396, .T. ) ;
#100007 = CARTESIAN_POINT ( 'NONE',  ( -2.240280033315860162E-09, 1413.999988936019918, 247.7072834788440048 ) ) ;
#100009 = VERTEX_POINT ( 'NONE', #77391 ) ;
#100010 = CARTESIAN_POINT ( 'NONE',  ( -11.76110721155049887, 1426.914523167039988, 145.8371853733709997 ) ) ;
#100011 = CARTESIAN_POINT ( 'NONE',  ( 13.91046082419999941, 1500.295402486089870, 227.7266705026989939 ) ) ;
#100012 = CARTESIAN_POINT ( 'NONE',  ( -3.565775599929999817, 1474.072336424830155, 270.1349117941979898 ) ) ;
#100013 = CARTESIAN_POINT ( 'NONE',  ( 0.1263686949653684832, 1473.473085869263741, 219.3472977631268463 ) ) ;
#100014 = CARTESIAN_POINT ( 'NONE',  ( -125.6580589596999999, 1375.179104070690073, 304.2218459572590064 ) ) ;
#100015 = CARTESIAN_POINT ( 'NONE',  ( -5.013435694540000043, 1375.426148861440197, 214.7180213005390215 ) ) ;
#100016 = CARTESIAN_POINT ( 'NONE',  ( 0.2085018806018199833, 1452.672090412190073, 183.2418198939489855 ) ) ;
#100017 = CARTESIAN_POINT ( 'NONE',  ( 19.58650745723603137, 1456.033696075030775, 227.9567582387556683 ) ) ;
#100018 = B_SPLINE_CURVE_WITH_KNOTS ( 'NONE', 3,
 ( #17695, #84386, #85464, #103369, #75461, #101714, #50258, #59208, #94419, #83830, #86040, #101163, #93873, #43500, #24457, #58645, #102278, #60871, #16054, #77644, #7674, #93327 ),
 .UNSPECIFIED., .F., .F.,
 ( 4, 3, 3, 3, 3, 3, 3, 4 ),
 ( 0.000000000000000000, 1.239833439119680136, 2.490079122229909903, 3.560295889715780149, 4.472241803407629668, 5.624444489460710628, 6.402815887447280474, 7.120592051560000080 ),
 .UNSPECIFIED. ) ;
#100019 = CARTESIAN_POINT ( 'NONE',  ( 9.967358615308720360, 1468.722972651999953, 208.0937358601780147 ) ) ;
#100020 = CARTESIAN_POINT ( 'NONE',  ( -4.882000055239999803, 1457.939062349089909, 217.4853468547690056 ) ) ;
#100021 = CARTESIAN_POINT ( 'NONE',  ( 11.10947396198625370, 1365.784518360480661, 210.6218459617030021 ) ) ;
#100022 = CARTESIAN_POINT ( 'NONE',  ( -39.78916335803459958, 1422.796236866350000, 266.8817143848179967 ) ) ;
#100023 = ORIENTED_EDGE ( 'NONE', *, *, #33566, .F. ) ;
#100024 = CARTESIAN_POINT ( 'NONE',  ( -4.329200639848730603, 1515.074268821609849, 210.6179437698939978 ) ) ;
#100025 = B_SPLINE_SURFACE_WITH_KNOTS ( 'NONE', 5, 5, ( 
 ( #64195, #46304, #4806, #80432, #55243, #72061 ),
 ( #72586, #30004, #13191, #55801, #89917, #47379 ),
 ( #22134, #81504, #64758, #62393, #45588, #94855 ),
 ( #34938, #18677, #69691, #97075, #79181, #45036 ),
 ( #53427, #18130, #71359, #105472, #1928, #813 ),
 ( #103811, #28759, #52328, #88678, #11956, #86451 ),
 ( #20340, #19795, #1357, #95413, #104358, #9741 ),
 ( #78049, #35499, #61295, #52873, #60734, #36066 ),
 ( #79729, #2488, #10864, #36605, #54545, #28204 ) ),
 .UNSPECIFIED., .F., .F., .F.,
 ( 6, 3, 6 ),
 ( 6, 6 ),
 ( 1.123296626329999937, 3.227739016200000144, 6.189459079109999706 ),
 ( 0.000000000000000000, 2.000000000000000000 ),
 .UNSPECIFIED. ) ;
#100026 = EDGE_LOOP ( 'NONE', ( #81839, #64530, #61072 ) ) ;
#100027 = VERTEX_POINT ( 'NONE', #84666 ) ;
#100028 = CARTESIAN_POINT ( 'NONE',  ( 3.268235720634999897, 1516.890356958860139, 211.9874346545169885 ) ) ;
#100029 = CARTESIAN_POINT ( 'NONE',  ( 38.71370889343818078, 1443.913060387330916, 136.9324510732293732 ) ) ;
#100030 = CARTESIAN_POINT ( 'NONE',  ( -2.500000000000000000, 1439.615672362210034, 183.5288080682979910 ) ) ;
#100031 = EDGE_CURVE ( 'NONE', #53370, #110657, #55187, .T. ) ;
#100033 = CARTESIAN_POINT ( 'NONE',  ( -2.801317293797483288, 1440.706042130769220, 170.5311005417991623 ) ) ;
#100032 = CARTESIAN_POINT ( 'NONE',  ( 7.724423394095000894, 1517.122088787240045, 212.5760185856570104 ) ) ;
#100034 = CARTESIAN_POINT ( 'NONE',  ( -14.65731754589999802, 1440.434325343710043, 189.1109637770979930 ) ) ;
#100035 = CIRCLE ( 'NONE', #3523, 2.000000000000003553 ) ;
#100036 = CARTESIAN_POINT ( 'NONE',  ( -11.60004869885203682, 1428.983126981193436, 137.0999999980979851 ) ) ;
#100037 = B_SPLINE_SURFACE_WITH_KNOTS ( 'NONE', 5, 5, ( 
 ( #47795, #99828, #107698, #31530, #66278, #29877, #39388, #57324, #6337 ),
 ( #5800, #30982, #82498, #39941, #73565, #74111, #108241, #81371, #100394 ),
 ( #64066, #15266, #91990, #33727, #49458, #67920, #41034, #101469, #102028 ),
 ( #66819, #75211, #25866, #33179, #41600, #67370, #166, #84136, #15798 ),
 ( #43257, #92530, #76856, #708, #50556, #42700, #34288, #109364, #6878 ),
 ( #51654, #25312, #58954, #59511, #24219, #103130, #75754, #26430, #24756 ),
 ( #102572, #9091, #83580, #7435, #60069, #32642, #100920, #109900, #58405 ),
 ( #50001, #93085, #16358, #76297, #68469, #94186, #85231, #84683, #7981 ),
 ( #16901, #17455, #42147, #110448, #93622, #85794, #51106, #8523, #77404 ),
 ( #34838, #69027, #2383, #18025, #36501, #9629, #70144, #70697, #19120 ),
 ( #43799, #105364, #1823, #10192, #35958, #79626, #52763, #95308, #103702 ),
 ( #37603, #2930, #87469, #53323, #86899, #77950, #62284, #44366, #27001 ),
 ( #104808, #27549, #28096, #61191, #71805, #78512, #105924, #104258, #18568 ),
 ( #88569, #94746, #61731, #28655, #60625, #52218, #95854, #69584, #96414 ),
 ( #10761, #1256, #44931, #45483, #62859, #53895, #79078, #19691, #88030 ) ),
 .UNSPECIFIED., .F., .F., .F.,
 ( 6, 3, 3, 3, 6 ),
 ( 6, 3, 6 ),
 ( 3.076410786119999852, 5.721725431660000361, 7.579817615749999682, 10.83727443650000133, 12.56788425660000108 ),
 ( 0.000000000000000000, 1.000000000000000000, 2.000000000000000000 ),
 .UNSPECIFIED. ) ;
#100038 = ORIENTED_EDGE ( 'NONE', *, *, #77429, .F. ) ;
#100039 = CARTESIAN_POINT ( 'NONE',  ( -26.02813552489999793, 1435.406381042510020, 135.3446223067979872 ) ) ;
#100040 = EDGE_CURVE ( 'NONE', #78889, #59125, #98350, .T. ) ;
#100041 = EDGE_CURVE ( 'NONE', #69919, #104433, #92514, .T. ) ;
#100042 = CARTESIAN_POINT ( 'NONE',  ( 1.708747624254999931, 1517.213554313520035, 202.1696795498070003 ) ) ;
#100043 = VECTOR ( 'NONE', #96694, 1000.000000000000000 ) ;
#100044 = B_SPLINE_SURFACE_WITH_KNOTS ( 'NONE', 4, 5, ( 
 ( #60855, #44032, #16040, #75970, #43485, #94980 ),
 ( #51885, #84903, #50241, #42362, #68693, #26094 ),
 ( #84368, #59733, #8195, #69809, #76516, #101697 ),
 ( #110667, #93852, #17123, #86021, #8747, #77088 ),
 ( #18248, #52444, #94403, #60284, #34515, #102797 ) ),
 .UNSPECIFIED., .F., .F., .F.,
 ( 5, 5 ),
 ( 6, 6 ),
 ( 6.591324572230000456, 20.28790020619999979 ),
 ( 0.000000000000000000, 2.000000000000000000 ),
 .UNSPECIFIED. ) ;
#100045 = CARTESIAN_POINT ( 'NONE',  ( 9.549000335789999738, 1470.075890097690035, 212.3436668229989834 ) ) ;
#100046 = CARTESIAN_POINT ( 'NONE',  ( -22.03947762662830101, 1384.537944471270066, 202.2607269266779895 ) ) ;
#100047 = CARTESIAN_POINT ( 'NONE',  ( -38.22512636920640006, 1426.932643485439939, 269.5724048218409621 ) ) ;
#100048 = CARTESIAN_POINT ( 'NONE',  ( -6.918225190410000280, 1481.313522052990038, 206.5729027308990169 ) ) ;
#100049 = CARTESIAN_POINT ( 'NONE',  ( -3.502932684640000183, 1396.096286483429822, 197.9227087040979995 ) ) ;
#100050 = CIRCLE ( 'NONE', #12464, 0.9999999999999935607 ) ;
#100052 = ORIENTED_EDGE ( 'NONE', *, *, #11972, .F. ) ;
#100051 = CARTESIAN_POINT ( 'NONE',  ( 15.95383384960000228, 1506.798305107329952, 193.5571554442980187 ) ) ;
#100053 = ORIENTED_EDGE ( 'NONE', *, *, #31533, .F. ) ;
#100054 = CARTESIAN_POINT ( 'NONE',  ( 0.3740406684259999781, 1452.976565745030030, 183.2744760548980025 ) ) ;
#100055 = LINE ( 'NONE', #73780, #20562 ) ;
#100056 = ADVANCED_FACE ( 'NONE', ( #51091 ), #91340, .F. ) ;
#100057 = CARTESIAN_POINT ( 'NONE',  ( -0.3900471094334390099, 1425.462776352800120, 191.1056874147849953 ) ) ;
#100058 = CARTESIAN_POINT ( 'NONE',  ( -14.48051094013809958, 1436.252343529019981, 149.9435809378360318 ) ) ;
#100059 = CARTESIAN_POINT ( 'NONE',  ( -0.03672266410218510274, 1409.548389820189868, 185.2684399885600044 ) ) ;
#100061 = CARTESIAN_POINT ( 'NONE',  ( 0.7579843820170020230, 1516.883361325900069, 211.4083188566570186 ) ) ;
#100060 = VECTOR ( 'NONE', #37443, 1000.000000000000000 ) ;
#100062 = EDGE_CURVE ( 'NONE', #103670, #63089, #35414, .T. ) ;
#100063 = FACE_OUTER_BOUND ( 'NONE', #99504, .T. ) ;
#100064 = CARTESIAN_POINT ( 'NONE',  ( 5.426920751279999955, 1436.492768174659886, 154.6973185947979914 ) ) ;
#100065 = CARTESIAN_POINT ( 'NONE',  ( -109.1322461037039915, 1384.978503018139918, 313.2642998889880346 ) ) ;
#100066 = CARTESIAN_POINT ( 'NONE',  ( 4.164920226616133370, 1440.953747641006203, 156.0413096252420644 ) ) ;
#100067 = CARTESIAN_POINT ( 'NONE',  ( 11.79002767249999906, 1447.121451531979801, 187.8029512936980154 ) ) ;
#100068 =( BOUNDED_CURVE ( )  B_SPLINE_CURVE ( 3, ( #86729, #17837, #6842, #60445 ),
 .UNSPECIFIED., .F., .T. ) 
 B_SPLINE_CURVE_WITH_KNOTS ( ( 4, 4 ),
 ( 0.9240765055798439986, 2.217571029433250018 ),
 .UNSPECIFIED. ) 
 CURVE ( )  GEOMETRIC_REPRESENTATION_ITEM ( )  RATIONAL_B_SPLINE_CURVE ( ( 1.000000000000000000, 0.8653653976934794212, 0.8653653976934794212, 1.000000000000000000 ) ) 
 REPRESENTATION_ITEM ( '' )  );
#100069 = CARTESIAN_POINT ( 'NONE',  ( -0.7579263249019989601, 1516.927039499179955, 207.4176752179770347 ) ) ;
#100070 = EDGE_LOOP ( 'NONE', ( #37727, #66341 ) ) ;
#100071 = CARTESIAN_POINT ( 'NONE',  ( 19.53786426059039982, 1512.187213306747481, 236.7197124308265188 ) ) ;
#100073 = EDGE_CURVE ( 'NONE', #71004, #97290, #19613, .T. ) ;
#100072 = CARTESIAN_POINT ( 'NONE',  ( -10.42886454120000117, 1471.797594669490081, 207.2580361199489687 ) ) ;
#100074 = CARTESIAN_POINT ( 'NONE',  ( -8.744990863649999113, 1385.315572773260101, 218.5566709142290165 ) ) ;
#100075 = ORIENTED_EDGE ( 'NONE', *, *, #41271, .T. ) ;
#100076 = DIRECTION ( 'NONE',  ( 0.000000000000000000, -6.123233995736769734E-17, -1.000000000000000000 ) ) ;
#100077 = CARTESIAN_POINT ( 'NONE',  ( -3.272667022753710242, 1519.551704408389924, 189.0363362235078171 ) ) ;
#100078 = CARTESIAN_POINT ( 'NONE',  ( 13.15726448919999925, 1414.996444518330009, 197.7616626325980178 ) ) ;
#100079 = ADVANCED_FACE ( 'NONE', ( #82887 ), #40837, .T. ) ;
#100080 = CARTESIAN_POINT ( 'NONE',  ( -3.549608351769999892, 1507.276797637930031, 180.9704965309979912 ) ) ;
#100081 = DIRECTION ( 'NONE',  ( 0.7382608262429739554, 0.6622882068469760908, -0.1278486742459950254 ) ) ;
#100082 = CARTESIAN_POINT ( 'NONE',  ( 2.838432861149654318, 1451.798331723987985, 183.8400387955967403 ) ) ;
#100083 = CARTESIAN_POINT ( 'NONE',  ( 7.174675627540000100, 1488.418531450889986, 199.9219973391489873 ) ) ;
#100084 = EDGE_CURVE ( 'NONE', #67251, #103179, #35688, .T. ) ;
#100085 = CARTESIAN_POINT ( 'NONE',  ( 7.512750208045280154, 1509.038615934079871, 214.6352815289239970 ) ) ;
#100086 = CARTESIAN_POINT ( 'NONE',  ( 4.282037523864819839, 1440.980613445030031, 156.2001673258700123 ) ) ;
#100087 = AXIS2_PLACEMENT_3D ( 'NONE', #15283, #50574, #8548 ) ;
#100088 = CARTESIAN_POINT ( 'NONE',  ( -11.96661585360000046, 1440.449248668989867, 150.8629738177980073 ) ) ;
#100089 = CARTESIAN_POINT ( 'NONE',  ( -22.69876404240119072, 1501.977400791986611, 181.3483716558183119 ) ) ;
#100090 = CARTESIAN_POINT ( 'NONE',  ( -3.452917061035000401, 1517.089216728169959, 216.0711116162470091 ) ) ;
#100091 = VERTEX_POINT ( 'NONE', #68324 ) ;
#100092 = CARTESIAN_POINT ( 'NONE',  ( -17.57477352489999944, 1417.955521924099912, 206.8173651875889902 ) ) ;
#100093 = CARTESIAN_POINT ( 'NONE',  ( -8.181958980964999739, 1517.051704408389924, 206.0868810637969943 ) ) ;
#100094 = ADVANCED_FACE ( 'NONE', ( #92937 ), #41901, .F. ) ;
#100096 = CARTESIAN_POINT ( 'NONE',  ( -16.68447695228019967, 1508.551704408389924, 212.9946650234450090 ) ) ;
#100095 = ADVANCED_BREP_SHAPE_REPRESENTATION ( '', ( #7937, #21632 ), #107481 ) ;
#100097 = CARTESIAN_POINT ( 'NONE',  ( -8.902413453548941646, 1424.022967874639789, 122.9079028789289936 ) ) ;
#100098 = CARTESIAN_POINT ( 'NONE',  ( -2.182683425780000075, 1475.185842043989851, 219.3315818484989848 ) ) ;
#100099 = CARTESIAN_POINT ( 'NONE',  ( 21.60894078433416610, 1521.951704408389787, 218.5714488934191309 ) ) ;
#100100 = CARTESIAN_POINT ( 'NONE',  ( 11.44617005173907209, 1425.796920914145858, 139.1405512805114597 ) ) ;
#100101 = CARTESIAN_POINT ( 'NONE',  ( -3.751676929405963978, 1508.135276464469143, 220.7189868887600142 ) ) ;
#100102 = CARTESIAN_POINT ( 'NONE',  ( -1.743193279576590093, 1464.853942634930036, 183.6101355626199734 ) ) ;
#100103 = CARTESIAN_POINT ( 'NONE',  ( -109.1637285801670032, 1385.118900514759844, 297.1380744252289787 ) ) ;
#100104 = CARTESIAN_POINT ( 'NONE',  ( -2.379883222516000230E-07, 1408.913060379049739, 223.8563942630169947 ) ) ;
#100105 = CARTESIAN_POINT ( 'NONE',  ( 33.18315033877439646, 1440.913060383530137, 247.0235257256299803 ) ) ;
#100107 = CARTESIAN_POINT ( 'NONE',  ( -15.75336812958823884, 1414.913060387329779, 213.0330643493421121 ) ) ;
#100106 = CARTESIAN_POINT ( 'NONE',  ( -10.00567527226339948, 1472.275973908610013, 211.0029054612709842 ) ) ;
#100108 = CARTESIAN_POINT ( 'NONE',  ( 12.97616279770000070, 1422.953780371429957, 222.3281805362979924 ) ) ;
#100109 = VERTEX_POINT ( 'NONE', #10602 ) ;
#100110 = VERTEX_POINT ( 'NONE', #87309 ) ;
#100111 = CARTESIAN_POINT ( 'NONE',  ( 4.253777714910000007, 1442.471859903390168, 216.9083338397390150 ) ) ;
#100112 = CARTESIAN_POINT ( 'NONE',  ( -19.67371442948930849, 1485.252007959948060, 190.3247210294366596 ) ) ;
#100113 = CARTESIAN_POINT ( 'NONE',  ( -27.68516856759999811, 1508.595246549830108, 210.6013668364779789 ) ) ;
#100114 = LINE ( 'NONE', #100648, #54567 ) ;
#100115 = CARTESIAN_POINT ( 'NONE',  ( 11.19147557906589974, 1422.145537183640045, 210.4506353095700035 ) ) ;
#100116 = ADVANCED_FACE ( 'NONE', ( #54283 ), #11701, .F. ) ;
#100117 = CARTESIAN_POINT ( 'NONE',  ( -3.500000000000000000, 1421.663060387330006, 172.2701767054979882 ) ) ;
#100118 = CARTESIAN_POINT ( 'NONE',  ( -51.20695252170450118, 1383.809936270029993, 263.8239077099820520 ) ) ;
#100119 = DIRECTION ( 'NONE',  ( 0.9125304618753903307, 0.000000000000000000, -0.4090087482554460863 ) ) ;
#100120 = CARTESIAN_POINT ( 'NONE',  ( -15.44132444299999918, 1507.624369720630057, 192.1037569956980064 ) ) ;
#100121 = EDGE_CURVE ( 'NONE', #36366, #24304, #47586, .T. ) ;
#100122 = CARTESIAN_POINT ( 'NONE',  ( -12.73491014300939916, 1502.691142067039891, 209.0150589030249932 ) ) ;
#100123 = CARTESIAN_POINT ( 'NONE',  ( 10.46256578778500135, 1491.122137232039904, 212.5076585947759895 ) ) ;
#100125 = ORIENTED_EDGE ( 'NONE', *, *, #106394, .T. ) ;
#100124 = CARTESIAN_POINT ( 'NONE',  ( 0.7870490817069989431, 1454.950702146390086, 218.5222641204089769 ) ) ;
#100126 = CARTESIAN_POINT ( 'NONE',  ( 33.72300830903717639, 1524.397344074318198, 219.5868698111207777 ) ) ;
#100127 = AXIS2_PLACEMENT_3D ( 'NONE', #74191, #108871, #100466 ) ;
#100128 = CARTESIAN_POINT ( 'NONE',  ( -22.99522306489999579, 1384.540050732020063, 202.4077213122689898 ) ) ;
#100129 = CARTESIAN_POINT ( 'NONE',  ( 2.564245648567370139, 1508.551704408389924, 204.1347675678190114 ) ) ;
#100130 = ORIENTED_EDGE ( 'NONE', *, *, #2859, .T. ) ;
#100131 = ORIENTED_EDGE ( 'NONE', *, *, #70945, .T. ) ;
#100132 = CARTESIAN_POINT ( 'NONE',  ( -8.517264636099429964, 1385.713703502809949, 218.6243582954489852 ) ) ;
#100133 = CARTESIAN_POINT ( 'NONE',  ( -2.329920892870120053, 1515.492270357739926, 204.9835198739350233 ) ) ;
#100135 = CARTESIAN_POINT ( 'NONE',  ( 2.470168521978402421, 1523.481610426287716, 175.3649660270905599 ) ) ;
#100134 = CARTESIAN_POINT ( 'NONE',  ( -14.93718008229999938, 1416.181292664740113, 212.9156384192889959 ) ) ;
#100136 = CARTESIAN_POINT ( 'NONE',  ( -3.541011004710050258, 1495.537215548379891, 197.3123223667620323 ) ) ;
#100137 = CARTESIAN_POINT ( 'NONE',  ( -105.9813432219999925, 1380.125633722419934, 300.4093128206589540 ) ) ;
#100138 = EDGE_CURVE ( 'NONE', #78944, #110307, #54356, .T. ) ;
#100139 = CARTESIAN_POINT ( 'NONE',  ( 4.487574688360000508, 1465.989648107290122, 219.2141235446990208 ) ) ;
#100140 = CARTESIAN_POINT ( 'NONE',  ( -12.19041342026659969, 1508.551704408389924, 217.1207088137099959 ) ) ;
#100141 = CARTESIAN_POINT ( 'NONE',  ( 5.217757123237790395, 1409.095268481059975, 195.0806377026630116 ) ) ;
#100142 = CARTESIAN_POINT ( 'NONE',  ( 18.12190093680000302, 1425.048267533830085, 225.2390196191980181 ) ) ;
#100143 = CARTESIAN_POINT ( 'NONE',  ( 4.071927273580000062, 1420.049653579930009, 185.6171871639980111 ) ) ;
#100144 = CARTESIAN_POINT ( 'NONE',  ( 4.462819848452499905, 1432.645271588519790, 201.4082248412790079 ) ) ;
#100145 = CARTESIAN_POINT ( 'NONE',  ( -4.228686410976469467, 1441.557731059559956, 165.0907915641419947 ) ) ;
#100146 = AXIS2_PLACEMENT_3D ( 'NONE', #30178, #14481, #98493 ) ;
#100147 = DIRECTION ( 'NONE',  ( -0.03489949627507600571, 0.9993908270340192690, 7.149496293836860302E-08 ) ) ;
#100148 = EDGE_LOOP ( 'NONE', ( #94510, #80834, #52075, #34946 ) ) ;
#100149 = CARTESIAN_POINT ( 'NONE',  ( 14.38276615817169635, 1509.537722092532931, 235.4493228184925897 ) ) ;
#100150 = CARTESIAN_POINT ( 'NONE',  ( 17.94043310207709752, 1458.161672853299933, 228.3106580608940135 ) ) ;
#100151 = CARTESIAN_POINT ( 'NONE',  ( -12.16672036689999814, 1434.609987438209828, 150.8335117639980183 ) ) ;
#100152 = EDGE_CURVE ( 'NONE', #68424, #104636, #8896, .T. ) ;
#100153 = CARTESIAN_POINT ( 'NONE',  ( -7.271832385515029613E-10, 1467.401133680060184, 246.3384324245209882 ) ) ;
#100154 = CARTESIAN_POINT ( 'NONE',  ( -20.49879694356830129, 1504.586794500839915, 190.4844630885789911 ) ) ;
#100155 = CARTESIAN_POINT ( 'NONE',  ( -15.68596832889999959, 1420.312328904400147, 210.6114427239490112 ) ) ;
#100156 = CARTESIAN_POINT ( 'NONE',  ( -108.7028354350000114, 1386.982920307299764, 310.7828582002589428 ) ) ;
#100157 = CARTESIAN_POINT ( 'NONE',  ( -8.275210849650859402, 1511.570327478370018, 214.9577656342009959 ) ) ;
#100158 = CARTESIAN_POINT ( 'NONE',  ( -11.37099373375535727, 1362.708999033907048, 209.6218459617033432 ) ) ;
#100159 = LINE ( 'NONE', #49775, #62665 ) ;
#100160 = CARTESIAN_POINT ( 'NONE',  ( -2.562340869413346489, 1517.051704408389924, 196.2891841806521711 ) ) ;
#100161 = ADVANCED_FACE ( 'NONE', ( #2777 ), #5028, .F. ) ;
#100162 = CARTESIAN_POINT ( 'NONE',  ( -20.26037020649999576, 1488.374911902629947, 192.5828114397980073 ) ) ;
#100163 = CARTESIAN_POINT ( 'NONE',  ( 2.286472886424999906, 1516.883361325900069, 208.3638615500849767 ) ) ;
#100164 = CIRCLE ( 'NONE', #30464, 1.999999999999999556 ) ;
#100165 = CARTESIAN_POINT ( 'NONE',  ( 6.448255092998069316, 1408.606950371990024, 221.0175999112360046 ) ) ;
#100166 = FACE_OUTER_BOUND ( 'NONE', #16596, .T. ) ;
#100167 = B_SPLINE_SURFACE_WITH_KNOTS ( 'NONE', 5, 1, ( 
 ( #96783, #19499 ),
 ( #53701, #11664 ),
 ( #52577, #86712 ),
 ( #95668, #20054 ),
 ( #10004, #45840 ),
 ( #3291, #37423 ),
 ( #71620, #105740 ),
 ( #53132, #87269 ),
 ( #78312, #29024 ) ),
 .UNSPECIFIED., .F., .F., .F.,
 ( 6, 3, 6 ),
 ( 2, 2 ),
 ( 0.000000000000000000, 3.503639760140000003, 6.986073851990000527 ),
 ( 0.000000000000000000, 14.00000000000000000 ),
 .UNSPECIFIED. ) ;
#100168 = CARTESIAN_POINT ( 'NONE',  ( 3.586377583332121866, 1515.071394844002270, 205.0391410476011913 ) ) ;
#100169 = CARTESIAN_POINT ( 'NONE',  ( 7.495056103950230586, 1425.330532392250007, 212.2567483120330110 ) ) ;
#100170 = EDGE_LOOP ( 'NONE', ( #34004, #40530, #28293 ) ) ;
#100171 = CARTESIAN_POINT ( 'NONE',  ( 25.63688228349999676, 1437.526525769599857, 221.5010247020979932 ) ) ;
#100172 = CARTESIAN_POINT ( 'NONE',  ( -27.00673398009999815, 1508.127684928829922, 203.3798472705879874 ) ) ;
#100174 = CARTESIAN_POINT ( 'NONE',  ( 22.52609212299890018, 1509.699688857919909, 227.3081665486540146 ) ) ;
#100173 = CARTESIAN_POINT ( 'NONE',  ( 1.478882416969999891, 1478.166263375429935, 182.3756109040980107 ) ) ;
#100175 = CYLINDRICAL_SURFACE ( 'NONE', #44465, 2.000000000000003553 ) ;
#100176 = TOROIDAL_SURFACE ( 'NONE', #89398, 1.000000000000000000, 1.000000000000000000 ) ;
#100177 = CARTESIAN_POINT ( 'NONE',  ( -12.00843801870000149, 1421.605076870430139, 225.2224014919979993 ) ) ;
#100178 = CARTESIAN_POINT ( 'NONE',  ( -4.635184277964138566, 1377.964720639146435, 214.2196526210096579 ) ) ;
#100179 = EDGE_CURVE ( 'NONE', #20284, #102300, #80906, .T. ) ;
#100180 = CARTESIAN_POINT ( 'NONE',  ( -9.354210145178099012, 1452.586404171080176, 150.8537525510609782 ) ) ;
#100181 = CARTESIAN_POINT ( 'NONE',  ( 29.26107752939999784, 1451.736821630529903, 135.7240151124980230 ) ) ;
#100182 = ORIENTED_EDGE ( 'NONE', *, *, #19926, .T. ) ;
#100183 = CARTESIAN_POINT ( 'NONE',  ( -5.361476397494260304, 1423.659291631490078, 149.6373755565670081 ) ) ;
#100184 = DIRECTION ( 'NONE',  ( 0.4090087482554316534, -0.000000000000000000, 0.9125304618753967700 ) ) ;
#100185 = CARTESIAN_POINT ( 'NONE',  ( 16.53448445007540357, 1423.354062263319975, 228.9298141595320146 ) ) ;
#100186 = CARTESIAN_POINT ( 'NONE',  ( 17.17007368304201975, 1414.941152333512946, 210.4884745552690504 ) ) ;
#100187 = ORIENTED_EDGE ( 'NONE', *, *, #57143, .T. ) ;
#100188 = VERTEX_POINT ( 'NONE', #89505 ) ;
#100189 = CARTESIAN_POINT ( 'NONE',  ( -75.49308973149999247, 1385.139059930169878, 276.6890413075590232 ) ) ;
#100190 = CARTESIAN_POINT ( 'NONE',  ( -23.24847510427670016, 1409.840678955939893, 209.5428208297719834 ) ) ;
#100191 = ADVANCED_FACE ( 'NONE', ( #5502 ), #109560, .T. ) ;
#100192 = ORIENTED_EDGE ( 'NONE', *, *, #45332, .T. ) ;
#100193 = CARTESIAN_POINT ( 'NONE',  ( 4.487358438102120317, 1509.034524880150002, 205.3201215594939981 ) ) ;
#100194 = CARTESIAN_POINT ( 'NONE',  ( -105.1200804420000026, 1379.260731124600170, 305.2465900763589843 ) ) ;
#100195 = EDGE_CURVE ( 'NONE', #3770, #78370, #30137, .T. ) ;
#100196 = CARTESIAN_POINT ( 'NONE',  ( -23.81755502456005047, 1436.557569478829009, 140.3494998115120325 ) ) ;
#100197 = CARTESIAN_POINT ( 'NONE',  ( -19.24674285640000093, 1410.873837133030065, 222.4867807485979938 ) ) ;
#100198 = CARTESIAN_POINT ( 'NONE',  ( 44.66341284919820254, 1448.409646889560008, 266.2171260073000099 ) ) ;
#100199 = CARTESIAN_POINT ( 'NONE',  ( -4.987078454533489413, 1508.551704408389924, 205.6342615457560044 ) ) ;
#100200 = CARTESIAN_POINT ( 'NONE',  ( 0.02539148181239999844, 1420.205191554729936, 183.8956754969979954 ) ) ;
#100201 = CARTESIAN_POINT ( 'NONE',  ( -3.460101890015000237, 1516.812923327049930, 205.0932153474469715 ) ) ;
#100202 = ORIENTED_EDGE ( 'NONE', *, *, #81477, .F. ) ;
#100203 = CARTESIAN_POINT ( 'NONE',  ( 10.63195896838979948, 1481.229057553459825, 214.2444091096009799 ) ) ;
#100204 = CARTESIAN_POINT ( 'NONE',  ( 15.13257540405220070, 1512.281672892730057, 196.3467883166729848 ) ) ;
#100205 = VECTOR ( 'NONE', #87835, 1000.000000000000114 ) ;
#100206 = CARTESIAN_POINT ( 'NONE',  ( 12.76981295728383081, 1442.833559347544679, 186.8056601929062595 ) ) ;
#100207 = ORIENTED_EDGE ( 'NONE', *, *, #15978, .T. ) ;
#100209 = B_SPLINE_CURVE_WITH_KNOTS ( 'NONE', 3,
 ( #89088, #12375, #14428, #48625, #53308, #79064, #87450, #31244, #19673, #29187, #10744, #2369, #71225, #53879, #82756, #4006 ),
 .UNSPECIFIED., .F., .F.,
 ( 4, 3, 3, 3, 3, 4 ),
 ( -7.611835606329999671, -7.348446743584259977, -6.291169182585940156, -5.234779306343579464, -4.178565810992130203, -3.122448789919999967 ),
 .UNSPECIFIED. ) ;
#100208 = CARTESIAN_POINT ( 'NONE',  ( -10.50709737680259970, 1479.857933738049951, 209.4405100821019801 ) ) ;
#100210 = CARTESIAN_POINT ( 'NONE',  ( 5.989683923130864507, 1434.842958979083505, 203.0326939871309548 ) ) ;
#100211 = B_SPLINE_SURFACE_WITH_KNOTS ( 'NONE', 5, 5, ( 
 ( #103635, #62213, #53254, #43734, #26932, #77886 ),
 ( #44858, #61121, #95784, #18500, #85170, #52696 ),
 ( #19051, #1752, #68407, #35890, #36423, #8456 ),
 ( #70073, #104736, #27469, #28025, #61658, #102511 ),
 ( #87394, #10689, #79010, #3954, #63317, #71734 ),
 ( #98529, #13403, #2850, #55997, #29130, #99068 ),
 ( #64954, #54362, #80084, #55452, #11776, #87956 ),
 ( #80640, #89027, #21796, #5022, #71166, #97437 ),
 ( #3402, #45945, #36974, #105851, #97971, #53819 ) ),
 .UNSPECIFIED., .F., .F., .F.,
 ( 6, 3, 6 ),
 ( 6, 6 ),
 ( 25.28925225189999892, 28.57063311849999820, 31.85201398510000104 ),
 ( 0.000000000000000000, 2.000000000000000000 ),
 .UNSPECIFIED. ) ;
#100212 = CARTESIAN_POINT ( 'NONE',  ( -13.70533116771989945, 1512.850289815999986, 193.8128379569050139 ) ) ;
#100213 = CARTESIAN_POINT ( 'NONE',  ( 5.716743777814420113, 1452.713427295639804, 151.9346595207390180 ) ) ;
#100214 = CIRCLE ( 'NONE', #43000, 4.820754716980014010 ) ;
#100215 = CARTESIAN_POINT ( 'NONE',  ( 7.457597788700000230, 1422.876260087079800, 195.6364883457989947 ) ) ;
#100216 = EDGE_CURVE ( 'NONE', #42670, #76843, #13703, .T. ) ;
#100217 = CARTESIAN_POINT ( 'NONE',  ( 16.19086104229999989, 1409.478457713630178, 193.2334207647979838 ) ) ;
#100218 = CARTESIAN_POINT ( 'NONE',  ( -10.14960351718960041, 1492.786034375650161, 202.1826628221230067 ) ) ;
#100219 = CARTESIAN_POINT ( 'NONE',  ( 10.87765004282280046, 1478.880950294009835, 205.9430073526910121 ) ) ;
#100220 = CARTESIAN_POINT ( 'NONE',  ( 2.127093723893670241, 1408.987340136950024, 186.9630477151469847 ) ) ;
#100222 = CARTESIAN_POINT ( 'NONE',  ( -18.27190865341688308, 1423.986030104572819, 225.3810334195744076 ) ) ;
#100221 = CARTESIAN_POINT ( 'NONE',  ( -12.95358049610739926, 1434.757105051030067, 149.1854028063150110 ) ) ;
#100223 = CARTESIAN_POINT ( 'NONE',  ( 11.36690311099069994, 1426.240274596359995, 206.5033745847870250 ) ) ;
#100224 = CARTESIAN_POINT ( 'NONE',  ( -11.59204932530000143, 1378.005205810240113, 213.3426278446090123 ) ) ;
#100225 = EDGE_CURVE ( 'NONE', #100706, #11098, #64858, .T. ) ;
#100226 = LINE ( 'NONE', #23506, #32053 ) ;
#100227 = ORIENTED_EDGE ( 'NONE', *, *, #38524, .F. ) ;
#100228 = CARTESIAN_POINT ( 'NONE',  ( 8.800012970690000103, 1429.116251061429921, 209.1218459616979999 ) ) ;
#100229 = AXIS2_PLACEMENT_3D ( 'NONE', #92195, #15468, #30438 ) ;
#100230 = DIRECTION ( 'NONE',  ( 3.828568698926946970E-16, 0.000000000000000000, -1.000000000000000000 ) ) ;
#100231 = LINE ( 'NONE', #15635, #101727 ) ;
#100232 = CARTESIAN_POINT ( 'NONE',  ( -9.105351999590000744, 1386.405645367540046, 200.2123243072389869 ) ) ;
#100233 = CARTESIAN_POINT ( 'NONE',  ( 9.228811086073759995, 1424.916317554060015, 209.5472453667709942 ) ) ;
#100234 = CARTESIAN_POINT ( 'NONE',  ( 11.22642611442629956, 1422.531523140060017, 203.3570491252529848 ) ) ;
#100235 = CARTESIAN_POINT ( 'NONE',  ( 13.23453334633730094, 1423.606062042400026, 221.8416081335510057 ) ) ;
#100236 = CARTESIAN_POINT ( 'NONE',  ( 16.50400130224771544, 1525.907212628473644, 236.2546788475581820 ) ) ;
#100237 = CARTESIAN_POINT ( 'NONE',  ( -13.79555465660000024, 1416.822694272029821, 221.9085256446979884 ) ) ;
#100238 = PLANE ( 'NONE',  #93295 ) ;
#100239 = CARTESIAN_POINT ( 'NONE',  ( 6.438546668759999925, 1470.874276671130019, 268.3665355201979992 ) ) ;
#100240 = B_SPLINE_CURVE_WITH_KNOTS ( 'NONE', 5,
 ( #80137, #54419, #2367, #45466, #21298, #88014 ),
 .UNSPECIFIED., .F., .F.,
 ( 6, 6 ),
 ( -21.89489252110000095, -4.528383794635178816 ),
 .UNSPECIFIED. ) ;
#100241 = DIRECTION ( 'NONE',  ( -0.9455185755993178454, 0.000000000000000000, 0.3255681544571537578 ) ) ;
#100242 = VECTOR ( 'NONE', #101194, 1000.000000000000114 ) ;
#100243 = CARTESIAN_POINT ( 'NONE',  ( -16.99050533527280038, 1420.323706995179919, 203.8408272025779979 ) ) ;
#100244 = CARTESIAN_POINT ( 'NONE',  ( -108.6316274086125020, 1388.459345456638630, 297.9094210424456151 ) ) ;
#100245 = DIRECTION ( 'NONE',  ( 1.000000000000000000, 0.000000000000000000, 0.000000000000000000 ) ) ;
#100246 = CARTESIAN_POINT ( 'NONE',  ( -17.66088505599999792, 1486.101186812730020, 188.1926570484980346 ) ) ;
#100247 = CIRCLE ( 'NONE', #1967, 3.500000000000003109 ) ;
#100248 = CARTESIAN_POINT ( 'NONE',  ( 3.096410888356740276, 1474.521509624629743, 220.1161525996240016 ) ) ;
#100249 = CARTESIAN_POINT ( 'NONE',  ( -16.93199317389999692, 1409.669516225829966, 225.4753726314980042 ) ) ;
#100250 = CARTESIAN_POINT ( 'NONE',  ( -1.121059198139999991, 1418.672904462529914, 228.1661418348980135 ) ) ;
#100251 = CARTESIAN_POINT ( 'NONE',  ( -2.157956873969999911, 1474.488379276790056, 216.3412529684890160 ) ) ;
#100252 = CARTESIAN_POINT ( 'NONE',  ( 21.63718167644599433, 1524.600389084706649, 183.5694068101082621 ) ) ;
#100253 = CARTESIAN_POINT ( 'NONE',  ( 1.842962231260000028, 1515.372048949689997, 204.8601094097890041 ) ) ;
#100254 = CARTESIAN_POINT ( 'NONE',  ( 12.73074594762250022, 1426.578829893890088, 203.3886192763110330 ) ) ;
#100255 = CARTESIAN_POINT ( 'NONE',  ( 14.43085700395960025, 1426.807556820840091, 195.4949582478319883 ) ) ;
#100256 = CARTESIAN_POINT ( 'NONE',  ( -12.51099981729999833, 1416.825784011830137, 222.1450729858979969 ) ) ;
#100257 = CARTESIAN_POINT ( 'NONE',  ( 0.1746847925749699937, 1477.583909127160041, 182.1981708306240080 ) ) ;
#100259 = EDGE_LOOP ( 'NONE', ( #68761, #18111, #103064, #90260 ) ) ;
#100258 = CARTESIAN_POINT ( 'NONE',  ( 0.05087725381669139929, 1408.368774909579997, 222.6640242875809861 ) ) ;
#100260 = CARTESIAN_POINT ( 'NONE',  ( -28.06188869160000010, 1444.994950788469851, 168.7697867250980153 ) ) ;
#100261 = CONICAL_SURFACE ( 'NONE', #91305, 6.911399307709998219, 0.04363323129990067523 ) ;
#100262 = B_SPLINE_CURVE_WITH_KNOTS ( 'NONE', 3,
 ( #81149, #38056, #56521, #31299, #72234, #30747, #80612, #81688, #108002, #90648, #21211, #38592 ),
 .UNSPECIFIED., .F., .F.,
 ( 4, 2, 2, 2, 2, 4 ),
 ( 0.000000000000000000, 0.0007194225121803531943, 0.001079133768270215156, 0.001438845024360077118, 0.002158267536539286262, 0.002877690048718495406 ),
 .UNSPECIFIED. ) ;
#100263 = CARTESIAN_POINT ( 'NONE',  ( -28.39832174097189821, 1509.566674240429847, 211.0445668619889830 ) ) ;
#100264 = CARTESIAN_POINT ( 'NONE',  ( 11.87515583119999896, 1433.007142645810063, 149.4775923092979895 ) ) ;
#100265 = CARTESIAN_POINT ( 'NONE',  ( -41.66188030070000536, 1443.705283505669740, 134.0999999982089719 ) ) ;
#100266 = DIRECTION ( 'NONE',  ( -0.3363363969981477131, -0.6659120918162938496, 0.6659120918162938496 ) ) ;
#100267 = ORIENTED_EDGE ( 'NONE', *, *, #23852, .T. ) ;
#100268 = CARTESIAN_POINT ( 'NONE',  ( -17.42134197181179545, 1525.253996226947947, 181.0775359434758229 ) ) ;
#100269 = FACE_OUTER_BOUND ( 'NONE', #93459, .T. ) ;
#100270 = CARTESIAN_POINT ( 'NONE',  ( -107.4425579992611830, 1382.651356145541286, 310.5015941399482244 ) ) ;
#100271 = CARTESIAN_POINT ( 'NONE',  ( -11.24222018449999894, 1491.652723530989988, 206.9322330278289712 ) ) ;
#100272 = CARTESIAN_POINT ( 'NONE',  ( 19.21579935105259906, 1443.315311240889969, 208.7528447609300031 ) ) ;
#100273 = CARTESIAN_POINT ( 'NONE',  ( 29.17712929358009077, 1414.632439072223178, 269.3720782604887631 ) ) ;
#100274 = DIRECTION ( 'NONE',  ( 4.440892098500626162E-15, 0.000000000000000000, 1.000000000000000000 ) ) ;
#100275 = CARTESIAN_POINT ( 'NONE',  ( -12.54840892090000004, 1379.545626517140136, 210.2256536815890229 ) ) ;
#100276 = CARTESIAN_POINT ( 'NONE',  ( 32.38845791999494850, 1523.456872492435195, 202.1182848005511801 ) ) ;
#100277 = CARTESIAN_POINT ( 'NONE',  ( -60.62137868135909713, 1385.064398150979741, 245.3311423290439848 ) ) ;
#100278 = CARTESIAN_POINT ( 'NONE',  ( -20.37381179411450560, 1524.397344074318880, 237.9604625470747123 ) ) ;
#100279 = CARTESIAN_POINT ( 'NONE',  ( 11.05034677255730102, 1426.485892148770290, 207.3310236586839892 ) ) ;
#100280 = ORIENTED_EDGE ( 'NONE', *, *, #92850, .F. ) ;
#100281 = CARTESIAN_POINT ( 'NONE',  ( -29.54414221549020070, 1509.931130578880129, 208.5939597344579965 ) ) ;
#100282 = CARTESIAN_POINT ( 'NONE',  ( -16.03779784396279950, 1410.573261502639753, 226.6730129231060289 ) ) ;
#100284 = ORIENTED_EDGE ( 'NONE', *, *, #27065, .F. ) ;
#100283 = CARTESIAN_POINT ( 'NONE',  ( -113.4000000000000057, 1305.913060387289988, 309.7218459572590064 ) ) ;
#100285 = CARTESIAN_POINT ( 'NONE',  ( 4.551482758439999721, 1472.189735705889916, 218.2242021444390048 ) ) ;
#100286 = CARTESIAN_POINT ( 'NONE',  ( 40.27306231122417302, 1443.623772255950371, 137.1176861334613477 ) ) ;
#100287 = CARTESIAN_POINT ( 'NONE',  ( 18.02736213689669853, 1430.307743537649912, 211.8462674276539985 ) ) ;
#100288 = CARTESIAN_POINT ( 'NONE',  ( -109.6584366050000057, 1384.889060011860010, 311.3230549062590171 ) ) ;
#100289 = CARTESIAN_POINT ( 'NONE',  ( -0.07605448290418309609, 1420.080655933570142, 183.8600900220690164 ) ) ;
#100290 = CARTESIAN_POINT ( 'NONE',  ( 22.10980528540000023, 1409.685151801829761, 213.0533367086480041 ) ) ;
#100291 = DIRECTION ( 'NONE',  ( -1.000000000000000000, 0.000000000000000000, 0.000000000000000000 ) ) ;
#100292 = CARTESIAN_POINT ( 'NONE',  ( -17.50943625649999902, 1423.244172935829965, 226.4867715792979936 ) ) ;
#100293 = CARTESIAN_POINT ( 'NONE',  ( -4.330155983108352480, 1511.419855273161829, 200.8197880651785852 ) ) ;
#100294 = CARTESIAN_POINT ( 'NONE',  ( 7.590404545110000178, 1448.844191051889993, 202.5505402568389854 ) ) ;
#100295 = CARTESIAN_POINT ( 'NONE',  ( -121.5779650366748399, 1311.832804576490162, 299.7542032958752998 ) ) ;
#100296 = CARTESIAN_POINT ( 'NONE',  ( 15.28420222189999933, 1497.713060387329961, 225.7900586086979899 ) ) ;
#100297 = CARTESIAN_POINT ( 'NONE',  ( -0.04684193791649880062, 1455.943453576789807, 198.9381708170990066 ) ) ;
#100298 = CARTESIAN_POINT ( 'NONE',  ( 7.710610402995000001, 1516.594591938570147, 205.6677260153969939 ) ) ;
#100299 = CARTESIAN_POINT ( 'NONE',  ( -12.78907454407420019, 1485.543771368729949, 185.6852311013239785 ) ) ;
#100300 = ORIENTED_EDGE ( 'NONE', *, *, #17506, .T. ) ;
#100301 = CARTESIAN_POINT ( 'NONE',  ( -1.861669630580974566, 1464.694416944532804, 199.0202437191204581 ) ) ;
#100302 = CARTESIAN_POINT ( 'NONE',  ( 9.327651199099038948, 1434.415569083649871, 206.2244204008570136 ) ) ;
#100304 = VERTEX_POINT ( 'NONE', #20622 ) ;
#100303 = CARTESIAN_POINT ( 'NONE',  ( -68.62161786750179715, 1379.747591873680221, 280.2379983867550095 ) ) ;
#100305 = ORIENTED_EDGE ( 'NONE', *, *, #33706, .F. ) ;
#100306 = CARTESIAN_POINT ( 'NONE',  ( -8.779627249246892973, 1381.198063572799583, 217.8823406631832142 ) ) ;
#100307 = ORIENTED_EDGE ( 'NONE', *, *, #78685, .F. ) ;
#100308 = CARTESIAN_POINT ( 'NONE',  ( -3.218646267206591638, 1456.153438597946661, 200.2079057308925485 ) ) ;
#100309 = CARTESIAN_POINT ( 'NONE',  ( -22.95381948389999849, 1410.909818712429797, 204.6459351782779947 ) ) ;
#100311 = CARTESIAN_POINT ( 'NONE',  ( 15.92282521243189919, 1409.477284117250065, 192.7841990163499872 ) ) ;
#100310 = CARTESIAN_POINT ( 'NONE',  ( -9.064548087047670677, 1441.200071124479791, 153.7187301749719950 ) ) ;
#100312 = CARTESIAN_POINT ( 'NONE',  ( -6.548200625775000283, 1516.632821972880038, 210.2524534341069966 ) ) ;
#100313 = CARTESIAN_POINT ( 'NONE',  ( 40.71426153566390127, 1443.112331678010150, 137.0418675333559975 ) ) ;
#100314 = CARTESIAN_POINT ( 'NONE',  ( -107.4534871969369902, 1378.913060387289988, 307.7877216430330236 ) ) ;
#100315 = CARTESIAN_POINT ( 'NONE',  ( -14.48037769471150149, 1379.715043008649900, 208.2752642513599994 ) ) ;
#100317 = ADVANCED_FACE ( 'NONE', ( #38542 ), #101782, .T. ) ;
#100316 = CARTESIAN_POINT ( 'NONE',  ( 5.852294824033087650, 1466.142654960249729, 233.6444853126671148 ) ) ;
#100318 = CARTESIAN_POINT ( 'NONE',  ( 37.10988369666650044, 1450.944967383590210, 134.0999999986949831 ) ) ;
#100319 = CIRCLE ( 'NONE', #9125, 2.500000000000002220 ) ;
#100320 = CARTESIAN_POINT ( 'NONE',  ( -24.02854066789229748, 1507.902906607559999, 222.3115874531950169 ) ) ;
#100321 = VERTEX_POINT ( 'NONE', #94888 ) ;
#100322 = CARTESIAN_POINT ( 'NONE',  ( 16.50821004073419829, 1494.476738410949793, 193.0249950623970108 ) ) ;
#100323 = CARTESIAN_POINT ( 'NONE',  ( -8.486023334060130097, 1522.051704408389924, 211.0297173932031569 ) ) ;
#100324 = VERTEX_POINT ( 'NONE', #86478 ) ;
#100325 = ORIENTED_EDGE ( 'NONE', *, *, #64461, .F. ) ;
#100326 = CARTESIAN_POINT ( 'NONE',  ( 0.1517714129250010147, 1432.859101342389977, 203.3442573752690237 ) ) ;
#100327 = CARTESIAN_POINT ( 'NONE',  ( 10.43262181653840059, 1453.107031927230082, 211.0136350519360064 ) ) ;
#100328 = CIRCLE ( 'NONE', #87879, 33.13701971169416538 ) ;
#100329 = CARTESIAN_POINT ( 'NONE',  ( 0.1468926284139999983, 1452.343333621129887, 183.2733069738979736 ) ) ;
#100330 = CARTESIAN_POINT ( 'NONE',  ( -3.071983047080000251, 1484.702655605429982, 183.3182174088979934 ) ) ;
#100331 = CARTESIAN_POINT ( 'NONE',  ( 8.775825618903720482, 1379.913060387289988, 213.9161013477410336 ) ) ;
#100332 = CARTESIAN_POINT ( 'NONE',  ( -4.678976733710140223, 1508.551704408389924, 213.1801812299080154 ) ) ;
#100333 = CARTESIAN_POINT ( 'NONE',  ( -12.31888632829999963, 1377.996605653940151, 209.2056224726200071 ) ) ;
#100334 = ADVANCED_FACE ( 'NONE', ( #52905 ), #108511, .T. ) ;
#100335 = CARTESIAN_POINT ( 'NONE',  ( -19.84369564248747864, 1485.788751164898940, 214.8618253020684392 ) ) ;
#100336 = CARTESIAN_POINT ( 'NONE',  ( 29.99674465255694500, 1524.860077346005028, 222.2674750195774322 ) ) ;
#100337 = CARTESIAN_POINT ( 'NONE',  ( -10.58542156100000042, 1391.805874643410107, 214.6478040594989807 ) ) ;
#100338 = CARTESIAN_POINT ( 'NONE',  ( -77.54941825186959647, 1384.781592401509897, 279.6170682065900337 ) ) ;
#100339 = VERTEX_POINT ( 'NONE', #102704 ) ;
#100340 = CARTESIAN_POINT ( 'NONE',  ( -4.617490504904999682, 1516.685667699390024, 201.7969310139470167 ) ) ;
#100341 = CARTESIAN_POINT ( 'NONE',  ( -2.879318455905000018, 1516.995911393979895, 208.3865093923290033 ) ) ;
#100342 = ORIENTED_EDGE ( 'NONE', *, *, #34408, .T. ) ;
#100343 = CARTESIAN_POINT ( 'NONE',  ( 37.01368886828679905, 1440.913060387330006, 263.6769638602469854 ) ) ;
#100344 = CIRCLE ( 'NONE', #89545, 1.999999999999998668 ) ;
#100345 = CARTESIAN_POINT ( 'NONE',  ( -0.0007967155919044118005, 1451.919253836483904, 154.0005622324263470 ) ) ;
#100346 = VERTEX_POINT ( 'NONE', #87036 ) ;
#100347 = CARTESIAN_POINT ( 'NONE',  ( -13.57591587749999995, 1415.063410501429871, 220.4959916660980070 ) ) ;
#100348 = CARTESIAN_POINT ( 'NONE',  ( -11.85318840119790096, 1432.336023631749867, 150.2214164863760004 ) ) ;
#100349 = CARTESIAN_POINT ( 'NONE',  ( -17.33260530524039211, 1508.455897782298734, 212.8473335983153731 ) ) ;
#100350 = CARTESIAN_POINT ( 'NONE',  ( 17.38482601099109814, 1410.884446382940041, 192.4603632472940262 ) ) ;
#100351 = CARTESIAN_POINT ( 'NONE',  ( 21.58361403490490105, 1409.738374864039997, 206.3476434096999981 ) ) ;
#100352 = CARTESIAN_POINT ( 'NONE',  ( 10.03483494456899905, 1469.241669691499965, 207.4251379534379964 ) ) ;
#100353 = CARTESIAN_POINT ( 'NONE',  ( -8.374556587419998976, 1473.433882946689891, 202.3872411742389943 ) ) ;
#100354 = CARTESIAN_POINT ( 'NONE',  ( -11.87936887709999922, 1433.311451768779989, 148.5636887028979913 ) ) ;
#100355 = CARTESIAN_POINT ( 'NONE',  ( 26.30822731440100171, 1495.554174878970116, 206.2282085093290220 ) ) ;
#100357 = CARTESIAN_POINT ( 'NONE',  ( -1.674817372199999932, 1416.913060387330006, 226.0542104739980118 ) ) ;
#100356 = CARTESIAN_POINT ( 'NONE',  ( 17.41280886879999912, 1458.364526861729928, 230.6041451782980118 ) ) ;
#100358 = CARTESIAN_POINT ( 'NONE',  ( 4.613723315850000479E-06, 1474.175172091230024, 270.1377426632980132 ) ) ;
#100359 = EDGE_CURVE ( 'NONE', #87290, #61133, #16800, .T. ) ;
#100360 = CARTESIAN_POINT ( 'NONE',  ( -4.035536263215000474, 1517.086065052259983, 216.8453260496270047 ) ) ;
#100361 = ORIENTED_EDGE ( 'NONE', *, *, #18756, .F. ) ;
#100362 = AXIS2_PLACEMENT_3D ( 'NONE', #66419, #64772, #107288 ) ;
#100363 = DIRECTION ( 'NONE',  ( -0.000000000000000000, -1.000000000000000000, -0.000000000000000000 ) ) ;
#100364 = CARTESIAN_POINT ( 'NONE',  ( -0.1584504759644470018, 1507.222331208859941, 180.8948199759900035 ) ) ;
#100365 = DIRECTION ( 'NONE',  ( 1.755985294532469921E-16, -1.000000000000000000, 1.338183447452831989E-16 ) ) ;
#100366 = CARTESIAN_POINT ( 'NONE',  ( 6.560742225334999844, 1517.028034847769959, 213.1554992345569701 ) ) ;
#100367 = CARTESIAN_POINT ( 'NONE',  ( 18.56679396470000043, 1509.561427119029759, 187.1464481793979928 ) ) ;
#100368 = EDGE_CURVE ( 'NONE', #47286, #79230, #47964, .T. ) ;
#100369 = CARTESIAN_POINT ( 'NONE',  ( -10.85852386199281661, 1424.794007418467800, 138.1924915073045099 ) ) ;
#100371 = ORIENTED_EDGE ( 'NONE', *, *, #30388, .F. ) ;
#100370 = CARTESIAN_POINT ( 'NONE',  ( 3.910140106688379635, 1508.551704408389924, 213.9552835937910231 ) ) ;
#100372 = CARTESIAN_POINT ( 'NONE',  ( -10.10004869885203682, -0.000000000000000000, 137.0999999980979851 ) ) ;
#100373 = CARTESIAN_POINT ( 'NONE',  ( 2.645105003909999919, 1508.551704408389924, 219.5149751571990180 ) ) ;
#100374 = CARTESIAN_POINT ( 'NONE',  ( -11.57324738139999987, 1432.089115936239978, 151.1932558213979974 ) ) ;
#100375 = CARTESIAN_POINT ( 'NONE',  ( 0.06577164741639930645, 1429.775327166390070, 214.7293411062190103 ) ) ;
#100376 = CARTESIAN_POINT ( 'NONE',  ( -5.051788235653639880, 1442.712519720660111, 200.9272651379969830 ) ) ;
#100377 = CARTESIAN_POINT ( 'NONE',  ( 27.02695150585199357, 1451.203551446300708, 136.2753212570038102 ) ) ;
#100378 = DIRECTION ( 'NONE',  ( 1.000000000000000000, 0.000000000000000000, 0.000000000000000000 ) ) ;
#100379 = CARTESIAN_POINT ( 'NONE',  ( -4.682239257119849896, 1438.893378829450057, 227.1256970199729892 ) ) ;
#100381 = CARTESIAN_POINT ( 'NONE',  ( -13.54690246880000082, 1502.950168964990098, 209.0732237156209976 ) ) ;
#100380 = CARTESIAN_POINT ( 'NONE',  ( -24.01773571409999875, 1482.721384371930071, 219.5181103496979915 ) ) ;
#100382 = DIRECTION ( 'NONE',  ( 0.7074300732877097930, -0.02470400237317429276, 0.7063514731880239372 ) ) ;
#100383 = ORIENTED_EDGE ( 'NONE', *, *, #61791, .F. ) ;
#100384 = CARTESIAN_POINT ( 'NONE',  ( -7.336844680545000053, 1517.106845464700200, 205.6683011064770312 ) ) ;
#100385 = CARTESIAN_POINT ( 'NONE',  ( 6.194088323349999925, 1406.153407140329819, 267.2191889491979850 ) ) ;
#100386 = CARTESIAN_POINT ( 'NONE',  ( 38.60856580501570079, 1443.613625263020140, 137.1750438873210101 ) ) ;
#100387 = CARTESIAN_POINT ( 'NONE',  ( 10.81257864043729988, 1489.663435189140046, 207.4999579193730028 ) ) ;
#100388 = CARTESIAN_POINT ( 'NONE',  ( 23.82579336797228819, 1434.875857586895791, 214.2505971287225748 ) ) ;
#100389 = CARTESIAN_POINT ( 'NONE',  ( -10.53528427685149005, 1390.796569291690957, 215.5647122002405638 ) ) ;
#100390 = DIRECTION ( 'NONE',  ( 0.000000000000000000, 1.000000000000000000, 0.000000000000000000 ) ) ;
#100391 = AXIS2_PLACEMENT_3D ( 'NONE', #42494, #91245, #50371 ) ;
#100392 = CARTESIAN_POINT ( 'NONE',  ( -29.99620953741480278, 1526.382868172863937, 219.7462484079463252 ) ) ;
#100393 = CARTESIAN_POINT ( 'NONE',  ( -15.72388564909999964, 1416.853542096379897, 206.7724104149789923 ) ) ;
#100394 = CARTESIAN_POINT ( 'NONE',  ( -12.51069050239999925, 1447.046592316670058, 187.7237828829979946 ) ) ;
#100395 = CARTESIAN_POINT ( 'NONE',  ( -19.75952018396922227, 1485.979955017908424, 190.2281124034579136 ) ) ;
#100396 = LINE ( 'NONE', #41602, #107360 ) ;
#100397 = CARTESIAN_POINT ( 'NONE',  ( -11.25637333110000071, 1500.624827943590162, 211.0037259975690063 ) ) ;
#100398 = CARTESIAN_POINT ( 'NONE',  ( -17.24149055319999846, 1434.891998881070094, 209.1218459616979999 ) ) ;
#100399 = DIRECTION ( 'NONE',  ( -3.469446951953611033E-15, 0.000000000000000000, 1.000000000000000000 ) ) ;
#100400 = CARTESIAN_POINT ( 'NONE',  ( 2.500000001330000110, 1439.558446910639987, 156.0470066727980054 ) ) ;
#100401 = AXIS2_PLACEMENT_3D ( 'NONE', #63021, #80330, #38853 ) ;
#100402 = CARTESIAN_POINT ( 'NONE',  ( -6.205390840879999814, 1475.766608774730003, 267.5209476633980330 ) ) ;
#100403 = FACE_OUTER_BOUND ( 'NONE', #19662, .T. ) ;
#100404 = CARTESIAN_POINT ( 'NONE',  ( -13.22747438852011292, 1513.553889449568032, 192.3368110773319586 ) ) ;
#100405 = CARTESIAN_POINT ( 'NONE',  ( -11.92971211075766291, 1486.509503358195616, 184.3501215366537167 ) ) ;
#100406 = CARTESIAN_POINT ( 'NONE',  ( -45.18590935617369553, 1384.763297676119919, 251.9116518250590389 ) ) ;
#100407 = CARTESIAN_POINT ( 'NONE',  ( -106.9011555262299993, 1391.913060387289988, 301.9300221985360508 ) ) ;
#100408 = DIRECTION ( 'NONE',  ( 0.000000000000000000, 0.000000000000000000, -1.000000000000000000 ) ) ;
#100409 = CARTESIAN_POINT ( 'NONE',  ( -24.42951531446290048, 1444.777949477279890, 211.0705837658230166 ) ) ;
#100410 = CARTESIAN_POINT ( 'NONE',  ( 31.30542346655888863, 1525.651286436460396, 216.2805831001146259 ) ) ;
#100411 = CARTESIAN_POINT ( 'NONE',  ( 7.910095025013141878, 1511.948749218533067, 206.0626124326618651 ) ) ;
#100412 = CARTESIAN_POINT ( 'NONE',  ( -22.01686062879999994, 1410.177021064929932, 202.7226449493980169 ) ) ;
#100413 =( BOUNDED_CURVE ( )  B_SPLINE_CURVE ( 3, ( #97607, #20877, #46675, #74478 ),
 .UNSPECIFIED., .F., .F. ) 
 B_SPLINE_CURVE_WITH_KNOTS ( ( 4, 4 ),
 ( 4.409610696067515434, 5.070003797870570317 ),
 .UNSPECIFIED. ) 
 CURVE ( )  GEOMETRIC_REPRESENTATION_ITEM ( )  RATIONAL_B_SPLINE_CURVE ( ( 1.000000000000000000, 0.9639857562037046357, 0.9639857562037046357, 1.000000000000000000 ) ) 
 REPRESENTATION_ITEM ( '' )  );
#100414 = B_SPLINE_CURVE_WITH_KNOTS ( 'NONE', 5,
 ( #64340, #106858, #72732, #3890, #37468, #4428 ),
 .UNSPECIFIED., .F., .F.,
 ( 6, 6 ),
 ( 0.000000000000000000, 1.000000000000000000 ),
 .UNSPECIFIED. ) ;
#100415 = AXIS2_PLACEMENT_3D ( 'NONE', #24869, #31087, #6992 ) ;
#100416 = CARTESIAN_POINT ( 'NONE',  ( 5.145309177750649887, 1422.426130283250131, 194.5914460530619863 ) ) ;
#100417 = CARTESIAN_POINT ( 'NONE',  ( 11.26929293258100095, 1478.652642090589779, 205.8599246912870058 ) ) ;
#100418 = EDGE_LOOP ( 'NONE', ( #27333, #4302, #24916, #76491, #17101, #23610, #4091, #98319 ) ) ;
#100419 = CARTESIAN_POINT ( 'NONE',  ( -10.30418465418137153, 1410.643618912880129, 229.4321436142978996 ) ) ;
#100420 = CARTESIAN_POINT ( 'NONE',  ( 21.05711716160284652, 1526.748660780343698, 184.6313866553783498 ) ) ;
#100421 = CARTESIAN_POINT ( 'NONE',  ( -8.627754864100788623, 1437.492696373060198, 228.3379673427390060 ) ) ;
#100423 = CARTESIAN_POINT ( 'NONE',  ( 13.89659397336691171, 1452.767297056081361, 223.5433327310063873 ) ) ;
#100422 = CARTESIAN_POINT ( 'NONE',  ( 11.14405623819999924, 1425.166915822629790, 143.4624449666980297 ) ) ;
#100424 = CARTESIAN_POINT ( 'NONE',  ( 17.50735355147223160, 1524.972613296789177, 237.3782595154142996 ) ) ;
#100425 = FACE_OUTER_BOUND ( 'NONE', #98431, .T. ) ;
#100426 = CARTESIAN_POINT ( 'NONE',  ( -8.405631201569999433, 1451.156562209089998, 203.4069089233589978 ) ) ;
#100427 = CARTESIAN_POINT ( 'NONE',  ( 7.328049280255000575, 1516.809497469189864, 202.5664528150769854 ) ) ;
#100428 = CARTESIAN_POINT ( 'NONE',  ( 11.86606288651399588, 1432.348820292879054, 150.6996693143473465 ) ) ;
#100429 = CARTESIAN_POINT ( 'NONE',  ( -4.823778297959999684, 1426.859560269130043, 144.1938086916980239 ) ) ;
#100430 = CARTESIAN_POINT ( 'NONE',  ( 15.71561344153500350, 1514.030803186779849, 194.0252525622669850 ) ) ;
#100431 = CARTESIAN_POINT ( 'NONE',  ( -19.79017267473430053, 1418.757295473250224, 207.3023242580109979 ) ) ;
#100432 = CARTESIAN_POINT ( 'NONE',  ( 7.628773448410000491, 1416.913060387330006, 216.7506196533479965 ) ) ;
#100433 = VECTOR ( 'NONE', #56306, 1000.000000000000227 ) ;
#100434 = CARTESIAN_POINT ( 'NONE',  ( 22.51756696979500205, 1509.699391153020088, 227.9212068633959802 ) ) ;
#100436 = ORIENTED_EDGE ( 'NONE', *, *, #90427, .F. ) ;
#100435 = CARTESIAN_POINT ( 'NONE',  ( -59.67093331630000108, 1379.746016655649782, 264.7494437565589465 ) ) ;
#100437 = VERTEX_POINT ( 'NONE', #109080 ) ;
#100438 = CARTESIAN_POINT ( 'NONE',  ( 11.41627450834240065, 1434.253991202039970, 151.4464532660140037 ) ) ;
#100439 = CARTESIAN_POINT ( 'NONE',  ( -5.420556941769999248, 1397.452469479530009, 221.3623452826979872 ) ) ;
#100440 = CARTESIAN_POINT ( 'NONE',  ( -19.73686209359999921, 1410.963192513930153, 221.4818400716980307 ) ) ;
#100441 = VERTEX_POINT ( 'NONE', #32361 ) ;
#100442 = CARTESIAN_POINT ( 'NONE',  ( -13.14780857342640807, 1444.759452443107193, 169.3987409578616052 ) ) ;
#100443 = CARTESIAN_POINT ( 'NONE',  ( 22.00282045326062175, 1509.704813241454076, 228.9760804587602649 ) ) ;
#100444 = CARTESIAN_POINT ( 'NONE',  ( -7.883416877324999739, 1512.215430505229961, 212.0555133921270112 ) ) ;
#100446 = CARTESIAN_POINT ( 'NONE',  ( -13.71395690008879953, 1507.898280399110035, 184.2319266679010070 ) ) ;
#100445 = CARTESIAN_POINT ( 'NONE',  ( 0.6279484944370010702, 1443.757946321590225, 200.1921173854589995 ) ) ;
#100447 = CARTESIAN_POINT ( 'NONE',  ( 2.108249574319999819, 1468.706075860329975, 182.9191506125980027 ) ) ;
#100448 = CARTESIAN_POINT ( 'NONE',  ( -9.839465017559998472, 1415.426091369230107, 193.9823038429979931 ) ) ;
#100449 = CARTESIAN_POINT ( 'NONE',  ( -17.44368141866249999, 1417.861416191989974, 207.0172452560950092 ) ) ;
#100450 = CARTESIAN_POINT ( 'NONE',  ( 10.91120509363300073, 1396.294088065360029, 210.9837282830089862 ) ) ;
#100451 = CARTESIAN_POINT ( 'NONE',  ( 1.393184507720000020, 1415.579607678529783, 190.6507824856979880 ) ) ;
#100452 = CARTESIAN_POINT ( 'NONE',  ( 11.83689489290000019, 1430.337612590129993, 149.6288192558980086 ) ) ;
#100453 = CARTESIAN_POINT ( 'NONE',  ( 5.639308305133535093, 1426.925666188799596, 144.1938086916980524 ) ) ;
#100454 = ORIENTED_EDGE ( 'NONE', *, *, #48064, .F. ) ;
#100455 = CARTESIAN_POINT ( 'NONE',  ( 13.24048663314659890, 1434.881627497140016, 149.0998486302219987 ) ) ;
#100456 = ORIENTED_EDGE ( 'NONE', *, *, #60045, .T. ) ;
#100457 = ORIENTED_EDGE ( 'NONE', *, *, #4861, .T. ) ;
#100458 = CARTESIAN_POINT ( 'NONE',  ( 13.45896606823204600, 1444.273004732949403, 169.3617971741905421 ) ) ;
#100459 = CARTESIAN_POINT ( 'NONE',  ( -8.404281262359999616, 1463.438804155129901, 234.4303259422979977 ) ) ;
#100460 = CARTESIAN_POINT ( 'NONE',  ( -13.36764582699999870, 1434.818091166239810, 195.6891582639979958 ) ) ;
#100461 = CARTESIAN_POINT ( 'NONE',  ( 1.709358663124999955, 1516.542957540330008, 216.0554336257470140 ) ) ;
#100462 = CARTESIAN_POINT ( 'NONE',  ( -8.389626007570329946, 1511.399590460235004, 213.7199506810841569 ) ) ;
#100463 =( GEOMETRIC_REPRESENTATION_CONTEXT ( 3 ) GLOBAL_UNCERTAINTY_ASSIGNED_CONTEXT ( ( #43514 ) ) GLOBAL_UNIT_ASSIGNED_CONTEXT ( ( #45546, #4082, #38207 ) ) REPRESENTATION_CONTEXT ( 'NONE', 'WORKASPACE' ) );
#100464 = VERTEX_POINT ( 'NONE', #100645 ) ;
#100465 = CARTESIAN_POINT ( 'NONE',  ( -11.46285876299999984, 1503.757027581689954, 207.6153421870490092 ) ) ;
#100466 = DIRECTION ( 'NONE',  ( -0.6736849260863841948, 0.000000000000000000, 0.7390186874254148774 ) ) ;
#100467 = CARTESIAN_POINT ( 'NONE',  ( -19.31603552230000176, 1376.225470561590100, 208.2524156231209815 ) ) ;
#100468 = EDGE_CURVE ( 'NONE', #98544, #105125, #51550, .T. ) ;
#100469 = ORIENTED_EDGE ( 'NONE', *, *, #58439, .T. ) ;
#100470 = CARTESIAN_POINT ( 'NONE',  ( -4.042417815834999928, 1516.904492006980036, 205.6736390534169914 ) ) ;
#100471 = ORIENTED_EDGE ( 'NONE', *, *, #39179, .F. ) ;
#100472 = CARTESIAN_POINT ( 'NONE',  ( 4.623892060624999800, 1517.066898074209803, 209.8584071487349831 ) ) ;
#100473 = CARTESIAN_POINT ( 'NONE',  ( -20.99960920810000076, 1509.542875960729816, 229.5003925517980008 ) ) ;
#100474 = EDGE_CURVE ( 'NONE', #36031, #65500, #14035, .T. ) ;
#100475 = CARTESIAN_POINT ( 'NONE',  ( -17.16049493890136546, 1413.067501001438586, 269.3744597087676311 ) ) ;
#100476 = CARTESIAN_POINT ( 'NONE',  ( 6.911190382705000523, 1512.677556571470177, 217.1831025208769859 ) ) ;
#100478 = ORIENTED_EDGE ( 'NONE', *, *, #24780, .T. ) ;
#100477 = CARTESIAN_POINT ( 'NONE',  ( -0.2241001114496510016, 1414.913060387399810, 225.2212286822969816 ) ) ;
#100479 = CARTESIAN_POINT ( 'NONE',  ( 2.500000000000000000, 1422.854123512330034, 153.3880924786980131 ) ) ;
#100480 = CARTESIAN_POINT ( 'NONE',  ( -27.68018901532030185, 1440.913060394170088, 229.8355793643949880 ) ) ;
#100481 = CARTESIAN_POINT ( 'NONE',  ( -59.38610754540000158, 1383.797318715759957, 279.8430129459590034 ) ) ;
#100482 = CARTESIAN_POINT ( 'NONE',  ( -0.1457467676193440198, 1465.435012609549858, 236.3215832813700104 ) ) ;
#100483 = VECTOR ( 'NONE', #7618, 999.9999999999998863 ) ;
#100484 = CARTESIAN_POINT ( 'NONE',  ( 10.92641736269999875, 1408.882512851029787, 270.2707055153979923 ) ) ;
#100485 = CARTESIAN_POINT ( 'NONE',  ( 5.784638319815000429, 1516.939574742129935, 213.7356083271170064 ) ) ;
#100486 = CARTESIAN_POINT ( 'NONE',  ( 22.71325450959999870, 1409.706218420429877, 209.2588089802279967 ) ) ;
#100487 = CARTESIAN_POINT ( 'NONE',  ( -5.100957845159999948, 1482.122785942490054, 228.9672709512990139 ) ) ;
#100488 = CARTESIAN_POINT ( 'NONE',  ( 17.59477483717979851, 1428.744049018530177, 204.6105714838779761 ) ) ;
#100489 = CARTESIAN_POINT ( 'NONE',  ( 6.032864527508810859, 1508.551565390810083, 216.2881064761960204 ) ) ;
#100490 = CARTESIAN_POINT ( 'NONE',  ( -3.253301419385000504, 1516.790374942449944, 210.2573062871869922 ) ) ;
#100491 = CARTESIAN_POINT ( 'NONE',  ( -21.91520783698913633, 1524.538768545233779, 233.6709662800621459 ) ) ;
#100492 = CARTESIAN_POINT ( 'NONE',  ( -5.311724842150000292, 1500.891271500089942, 229.7588813323989996 ) ) ;
#100493 = CARTESIAN_POINT ( 'NONE',  ( -11.66377130828579389, 1486.022747640305397, 184.5416405436658351 ) ) ;
#100495 = VERTEX_POINT ( 'NONE', #11446 ) ;
#100494 = CARTESIAN_POINT ( 'NONE',  ( -67.04318418450000649, 1385.033547286170005, 292.1847026260589928 ) ) ;
#100497 = CIRCLE ( 'NONE', #104014, 1.000000000000000000 ) ;
#100496 = CARTESIAN_POINT ( 'NONE',  ( -48.92494107440639795, 1385.128557567969892, 259.5107056320019865 ) ) ;
#100498 = DIRECTION ( 'NONE',  ( 0.000000000000000000, -1.036208156316811829E-12, 1.000000000000000000 ) ) ;
#100499 = DIRECTION ( 'NONE',  ( -0.9942586961433764747, 0.000000000000000000, -0.1070030146457237041 ) ) ;
#100500 = B_SPLINE_CURVE_WITH_KNOTS ( 'NONE', 3,
 ( #687, #34817, #69004, #103108, #26409, #32623, #100898, #24195, #58382, #15775, #27521, #52741 ),
 .UNSPECIFIED., .F., .F.,
 ( 4, 2, 2, 2, 2, 4 ),
 ( -0.1123552058535770004, -0.09789079797561310581, -0.08345975750668109538, -0.05408602645508549939, -0.02844277172862970382, 0.000000000000000000 ),
 .UNSPECIFIED. ) ;
#100501 = CARTESIAN_POINT ( 'NONE',  ( -0.1651761191785623695, 1494.443534717202510, 220.2719660499762995 ) ) ;
#100502 = CARTESIAN_POINT ( 'NONE',  ( 4.955161316548390538, 1484.956798682839917, 218.7828042351830220 ) ) ;
#100503 = CARTESIAN_POINT ( 'NONE',  ( -23.51884061340000187, 1448.078341978100070, 217.4024159431679664 ) ) ;
#100504 = CARTESIAN_POINT ( 'NONE',  ( -2.072561274125446218, 1497.860486493681265, 198.0224543596587807 ) ) ;
#100506 = CARTESIAN_POINT ( 'NONE',  ( -8.297843675610002023, 1384.899870833489786, 218.7036046430589806 ) ) ;
#100505 = CARTESIAN_POINT ( 'NONE',  ( -2.872836660654999985, 1517.158319634930194, 216.8472181024670249 ) ) ;
#100507 = CARTESIAN_POINT ( 'NONE',  ( 5.291552342926635788, 1457.527819839196582, 199.7187649193072332 ) ) ;
#100508 = CARTESIAN_POINT ( 'NONE',  ( 29.78220350812350858, 1524.382868172863937, 221.7347658002326227 ) ) ;
#100509 = EDGE_LOOP ( 'NONE', ( #22822, #77844, #25495, #104123 ) ) ;
#100510 = CARTESIAN_POINT ( 'NONE',  ( 7.328049280255000575, 1516.809497469189864, 202.5664528150769854 ) ) ;
#100511 = CARTESIAN_POINT ( 'NONE',  ( -16.62677417856500028, 1512.592133792520144, 221.2813269351669874 ) ) ;
#100512 = CONICAL_SURFACE ( 'NONE', #97016, 6.911399307709998219, 0.04363323129990067523 ) ;
#100513 = CARTESIAN_POINT ( 'NONE',  ( 15.14035858829999981, 1484.828642735030144, 223.7275130474980074 ) ) ;
#100514 = CARTESIAN_POINT ( 'NONE',  ( 22.91083410329999737, 1450.813759947410063, 218.3463015468979904 ) ) ;
#100515 = CARTESIAN_POINT ( 'NONE',  ( 10.91194618042609932, 1461.517685402190182, 210.2175723062259749 ) ) ;
#100516 = CARTESIAN_POINT ( 'NONE',  ( -5.516138227071085254, 1462.433753707725145, 201.0655331976316802 ) ) ;
#100517 = CARTESIAN_POINT ( 'NONE',  ( -1.259107554299999876, 1443.335980107890009, 218.6644318344589806 ) ) ;
#100518 = CARTESIAN_POINT ( 'NONE',  ( 15.20205009985922828, 1420.720005487666640, 227.8617693338353547 ) ) ;
#100519 = CARTESIAN_POINT ( 'NONE',  ( -106.5585968837300044, 1390.939245634569943, 300.3884029622149683 ) ) ;
#100520 = CARTESIAN_POINT ( 'NONE',  ( -21.29751270369999716, 1429.161938467929986, 221.7940764617979994 ) ) ;
#100521 = CARTESIAN_POINT ( 'NONE',  ( 8.784378609766859469, 1487.811415144687999, 202.7137191972914536 ) ) ;
#100522 = CARTESIAN_POINT ( 'NONE',  ( -106.7184954779999941, 1387.980454484629945, 298.4661214286589939 ) ) ;
#100523 = CARTESIAN_POINT ( 'NONE',  ( -15.75701339500000131, 1413.316754371529896, 226.8028676289979728 ) ) ;
#100524 = CARTESIAN_POINT ( 'NONE',  ( -105.8054920000000010, 1391.680210928180031, 302.6861668426589631 ) ) ;
#100525 = CARTESIAN_POINT ( 'NONE',  ( -14.55555340835505618, 1469.534367028784800, 269.3628596919716642 ) ) ;
#100526 = ORIENTED_EDGE ( 'NONE', *, *, #43179, .T. ) ;
#100527 = FACE_OUTER_BOUND ( 'NONE', #84910, .T. ) ;
#100528 = CARTESIAN_POINT ( 'NONE',  ( -42.22973048505161131, 1427.945894564693617, 269.0695617814723164 ) ) ;
#100529 = CARTESIAN_POINT ( 'NONE',  ( -4.333389548141039604, 1508.551704407329908, 213.7899627404379999 ) ) ;
#100530 = CARTESIAN_POINT ( 'NONE',  ( -4.871322248929999432, 1483.548475176390184, 199.6254626716689984 ) ) ;
#100531 = CARTESIAN_POINT ( 'NONE',  ( -14.77861346903486073, 1452.029250706874791, 222.9956542297432804 ) ) ;
#100532 = CARTESIAN_POINT ( 'NONE',  ( -13.45936570671707422, 1444.272002885449183, 187.0016728524507528 ) ) ;
#100533 = CARTESIAN_POINT ( 'NONE',  ( -8.590080337109450070, 1437.218647809359709, 210.0977144842290159 ) ) ;
#100534 = CARTESIAN_POINT ( 'NONE',  ( 3.076459279043819883, 1495.499563246870139, 221.1031227505570200 ) ) ;
#100535 = CARTESIAN_POINT ( 'NONE',  ( -2.293473560577727444, 1415.644794225288933, 232.9564924084930908 ) ) ;
#100536 = CARTESIAN_POINT ( 'NONE',  ( -33.93019615848960768, 1522.382868172863937, 197.6607374646001176 ) ) ;
#100537 = CARTESIAN_POINT ( 'NONE',  ( -9.615660731045778675, 1460.249980679099963, 209.9216382747220280 ) ) ;
#100538 = CARTESIAN_POINT ( 'NONE',  ( -13.14373765855973453, 1443.062906526838788, 169.3993406322344981 ) ) ;
#100540 = ORIENTED_EDGE ( 'NONE', *, *, #18889, .T. ) ;
#100539 = CARTESIAN_POINT ( 'NONE',  ( -13.04207716350000013, 1409.368499757629934, 225.9431851714979871 ) ) ;
#100541 = B_SPLINE_CURVE_WITH_KNOTS ( 'NONE', 5,
 ( #30162, #98475, #5530, #38032, #64353, #108536 ),
 .UNSPECIFIED., .F., .F.,
 ( 6, 6 ),
 ( -2.000000000000000000, -4.054528290886594277E-08 ),
 .UNSPECIFIED. ) ;
#100542 = CARTESIAN_POINT ( 'NONE',  ( 0.2679975439089999911, 1416.543503932829935, 190.7826617148979835 ) ) ;
#100543 = CARTESIAN_POINT ( 'NONE',  ( -13.41288733981332015, 1379.525778898297631, 211.7978688460160015 ) ) ;
#100544 = VERTEX_POINT ( 'NONE', #96550 ) ;
#100545 = EDGE_LOOP ( 'NONE', ( #69254, #1873, #36050 ) ) ;
#100546 = CARTESIAN_POINT ( 'NONE',  ( 17.50151672410429882, 1415.426561690370136, 209.0279233183210010 ) ) ;
#100547 = CARTESIAN_POINT ( 'NONE',  ( 6.224497175254511738, 1516.718921113260649, 204.9371257324691555 ) ) ;
#100549 = CARTESIAN_POINT ( 'NONE',  ( -4.105765241160000301, 1462.105318180830182, 225.2361590896979919 ) ) ;
#100548 = CARTESIAN_POINT ( 'NONE',  ( 3.380344682699999659, 1455.610420236290111, 218.3745015725090184 ) ) ;
#100550 = CARTESIAN_POINT ( 'NONE',  ( -7.825150488850000308, 1446.296144498489866, 214.7080216625790001 ) ) ;
#100551 = CARTESIAN_POINT ( 'NONE',  ( -11.26041480129999961, 1433.222928179650125, 151.5319910271979893 ) ) ;
#100552 = CARTESIAN_POINT ( 'NONE',  ( -12.53380652166779896, 1445.052232296300190, 185.6742736269380032 ) ) ;
#100553 = DIRECTION ( 'NONE',  ( -0.5220042966316842392, -0.8520752641501264657, -0.03846113000878779997 ) ) ;
#100554 = CARTESIAN_POINT ( 'NONE',  ( -2.314969334973923765, 1525.402221411349728, 243.6179210388351066 ) ) ;
#100555 = CARTESIAN_POINT ( 'NONE',  ( -24.89152731869999968, 1440.652444856679949, 210.4229212863880036 ) ) ;
#100556 = FACE_BOUND ( 'NONE', #76084, .T. ) ;
#100557 = CARTESIAN_POINT ( 'NONE',  ( 2.409539184149999791, 1449.743190781309977, 182.7459288299980074 ) ) ;
#100558 = CARTESIAN_POINT ( 'NONE',  ( 8.606858817780835835, 1364.325397926196729, 210.6218459617142003 ) ) ;
#100559 = CARTESIAN_POINT ( 'NONE',  ( -7.243611849145669801, 1479.647692371829862, 210.0496540924740145 ) ) ;
#100561 = ORIENTED_EDGE ( 'NONE', *, *, #39389, .F. ) ;
#100560 = CARTESIAN_POINT ( 'NONE',  ( 4.989246313819999834, 1471.909539260290103, 189.7082128665990126 ) ) ;
#100562 = ORIENTED_EDGE ( 'NONE', *, *, #13050, .T. ) ;
#100563 = CARTESIAN_POINT ( 'NONE',  ( -11.80736846912400040, 1428.600782186070091, 148.5414466374529923 ) ) ;
#100564 = CARTESIAN_POINT ( 'NONE',  ( 24.13933143269999704, 1497.424724656589888, 206.6888131984590018 ) ) ;
#100565 = CARTESIAN_POINT ( 'NONE',  ( -8.021038987360000760, 1471.498700897329854, 270.0743385271980515 ) ) ;
#100566 = LINE ( 'NONE', #56936, #30115 ) ;
#100567 = CARTESIAN_POINT ( 'NONE',  ( -122.7187414971599964, 1311.832804576489934, 304.2218459572590064 ) ) ;
#100568 = CARTESIAN_POINT ( 'NONE',  ( 41.36928039706089777, 1446.256855822869966, 135.7759721705720040 ) ) ;
#100569 = CARTESIAN_POINT ( 'NONE',  ( 2.038646110889569485, 1525.960063244516959, 241.1857569150894278 ) ) ;
#100570 = CARTESIAN_POINT ( 'NONE',  ( 19.68696007051993035, 1455.842560867163456, 227.5801044884133262 ) ) ;
#100571 = CARTESIAN_POINT ( 'NONE',  ( -25.62242681216090290, 1435.677401875209853, 212.3103032994399939 ) ) ;
#100572 = CARTESIAN_POINT ( 'NONE',  ( -3.703897191089999819, 1458.190786016390120, 219.1639864912989992 ) ) ;
#100573 = CARTESIAN_POINT ( 'NONE',  ( 9.943976501836180759, 1365.461622992593902, 210.6218459616991936 ) ) ;
#100574 = CARTESIAN_POINT ( 'NONE',  ( -28.90439777006010047, 1413.811818966640203, 266.6319722207740028 ) ) ;
#100575 = VERTEX_POINT ( 'NONE', #29878 ) ;
#100576 = CARTESIAN_POINT ( 'NONE',  ( -12.32169104970000006, 1391.303891397440111, 206.9552536725390155 ) ) ;
#100577 = ORIENTED_EDGE ( 'NONE', *, *, #93521, .F. ) ;
#100578 = ORIENTED_EDGE ( 'NONE', *, *, #97339, .F. ) ;
#100579 = CARTESIAN_POINT ( 'NONE',  ( -0.7353365779029981120, 1516.995911393979895, 212.0011643880069698 ) ) ;
#100580 = CARTESIAN_POINT ( 'NONE',  ( 4.828144534977668378, 1423.511443209914432, 184.1101743659536965 ) ) ;
#100581 = CARTESIAN_POINT ( 'NONE',  ( 5.161277877375379575, 1424.205378946189967, 193.2953230041809718 ) ) ;
#100583 = CARTESIAN_POINT ( 'NONE',  ( -17.64670096713561165, 1419.583565028061230, 207.1176534675684877 ) ) ;
#100582 = CARTESIAN_POINT ( 'NONE',  ( -2.478306858074999841, 1516.938330505699923, 212.5844667883370107 ) ) ;
#100584 = CARTESIAN_POINT ( 'NONE',  ( -16.74965842090000123, 1425.425121304829872, 191.0834941450980011 ) ) ;
#100585 = VECTOR ( 'NONE', #58118, 1000.000000000000114 ) ;
#100586 = CARTESIAN_POINT ( 'NONE',  ( -10.12195197648249945, 1470.644448988779914, 212.0626821655110348 ) ) ;
#100587 = VERTEX_POINT ( 'NONE', #64068 ) ;
#100588 = CARTESIAN_POINT ( 'NONE',  ( -26.79413269730000025, 1436.761936273179799, 136.7822071774980088 ) ) ;
#100589 = CARTESIAN_POINT ( 'NONE',  ( -6.556651409415000131, 1516.858146885269889, 202.5689485651570010 ) ) ;
#100590 = EDGE_CURVE ( 'NONE', #86024, #78014, #46225, .T. ) ;
#100591 = CARTESIAN_POINT ( 'NONE',  ( 0.000000000000000000, 1518.913060387330006, 209.1218459616979999 ) ) ;
#100592 = CARTESIAN_POINT ( 'NONE',  ( -42.79837815356560071, 1384.591774741229983, 215.7805842356740129 ) ) ;
#100593 = CARTESIAN_POINT ( 'NONE',  ( -43.27233402150790198, 1430.332577981739860, 269.9334234287720165 ) ) ;
#100594 = CARTESIAN_POINT ( 'NONE',  ( 33.35590117750194139, 1523.678648413191695, 201.9126545693500816 ) ) ;
#100595 = CARTESIAN_POINT ( 'NONE',  ( -6.232532172530000025, 1398.098440467730143, 197.7132727550980178 ) ) ;
#100597 = VERTEX_POINT ( 'NONE', #10324 ) ;
#100596 = CARTESIAN_POINT ( 'NONE',  ( 20.91563430996840012, 1525.795403621570813, 184.9927170714047691 ) ) ;
#100598 = ORIENTED_EDGE ( 'NONE', *, *, #56235, .T. ) ;
#100599 = CARTESIAN_POINT ( 'NONE',  ( 0.1984549593710000226, 1451.686688173929952, 183.0460368089979966 ) ) ;
#100600 = CARTESIAN_POINT ( 'NONE',  ( -29.13898522073073494, 1526.069472839383479, 221.1027213634203576 ) ) ;
#100601 = CARTESIAN_POINT ( 'NONE',  ( -9.813982587879999997, 1383.225161719749849, 200.4195862986289853 ) ) ;
#100602 = CARTESIAN_POINT ( 'NONE',  ( -25.08556694820000033, 1436.445275169010074, 137.7014522548979869 ) ) ;
#100603 = CARTESIAN_POINT ( 'NONE',  ( 22.59589169820000265, 1507.700907224229923, 227.3081670307980175 ) ) ;
#100604 = CARTESIAN_POINT ( 'NONE',  ( 2.299656316094999653, 1516.843453247299749, 211.5982966343670171 ) ) ;
#100605 = CARTESIAN_POINT ( 'NONE',  ( -68.75987617920000616, 1379.748052094799959, 280.1906344666589916 ) ) ;
#100606 = CARTESIAN_POINT ( 'NONE',  ( -1.811215688146619929, 1484.240532944710139, 182.8268356034129738 ) ) ;
#100607 = CARTESIAN_POINT ( 'NONE',  ( 8.530448452174001162, 1437.926137415760195, 210.8253904255420252 ) ) ;
#100608 = CARTESIAN_POINT ( 'NONE',  ( -2.494020320564999782, 1516.876240617270014, 206.8389307488369866 ) ) ;
#100609 = VERTEX_POINT ( 'NONE', #105504 ) ;
#100610 = CARTESIAN_POINT ( 'NONE',  ( -2.691724795918589486, 1451.958513340359787, 184.7155965712029797 ) ) ;
#100611 = CARTESIAN_POINT ( 'NONE',  ( -10.55526070360000013, 1471.506691870590203, 208.2730915841879948 ) ) ;
#100612 = CARTESIAN_POINT ( 'NONE',  ( -19.90154680646875818, 1456.621465229937257, 225.3649839440089409 ) ) ;
#100613 = EDGE_LOOP ( 'NONE', ( #92598, #34256, #86296, #39755, #23067, #8467 ) ) ;
#100614 = CARTESIAN_POINT ( 'NONE',  ( -17.84054676580398180, 1523.580203803270933, 237.8810931560536801 ) ) ;
#100615 = CARTESIAN_POINT ( 'NONE',  ( -22.17127944006911378, 1509.715749581838509, 228.8537622112010581 ) ) ;
#100616 = CARTESIAN_POINT ( 'NONE',  ( -4.071992749581919036, 1441.017388854438877, 184.8896994088449901 ) ) ;
#100617 = CARTESIAN_POINT ( 'NONE',  ( 16.93532580710000346, 1468.845588117029820, 189.7264854529979914 ) ) ;
#100618 = CARTESIAN_POINT ( 'NONE',  ( -11.27553706004265166, 1425.429034480955124, 138.6747463096305353 ) ) ;
#100619 = CARTESIAN_POINT ( 'NONE',  ( -31.54050611717723740, 1436.927665025879378, 136.6348558985098975 ) ) ;
#100620 = CARTESIAN_POINT ( 'NONE',  ( 7.346915560640000287, 1487.962896346489970, 200.9143651426790029 ) ) ;
#100621 = CARTESIAN_POINT ( 'NONE',  ( -4.623067421070000016, 1470.601194648889987, 189.6761541078989808 ) ) ;
#100622 = CARTESIAN_POINT ( 'NONE',  ( 12.49965726624219187, 1384.899971913130003, 209.1218459572589836 ) ) ;
#100623 = EDGE_CURVE ( 'NONE', #42334, #44736, #56912, .T. ) ;
#100624 = CARTESIAN_POINT ( 'NONE',  ( -11.89544747750000120, 1434.541746328260160, 147.6465872843980094 ) ) ;
#100625 = CARTESIAN_POINT ( 'NONE',  ( 16.66257064975578928, 1410.427173609350120, 226.4839826715480342 ) ) ;
#100626 = CARTESIAN_POINT ( 'NONE',  ( -4.615644842514999624, 1517.009964551830080, 216.0692237534070159 ) ) ;
#100627 = ORIENTED_EDGE ( 'NONE', *, *, #11363, .T. ) ;
#100628 = CARTESIAN_POINT ( 'NONE',  ( -11.09668834241330160, 1414.913057819779851, 195.9645814827970014 ) ) ;
#100629 = DIRECTION ( 'NONE',  ( 0.9455185755993177343, 0.000000000000000000, -0.3255681544571540909 ) ) ;
#100630 = CARTESIAN_POINT ( 'NONE',  ( -18.05232962988900169, 1508.551704408389924, 211.0109356106890175 ) ) ;
#100631 = CARTESIAN_POINT ( 'NONE',  ( 0.01429292403579860045, 1475.129915452889918, 220.1645601639990275 ) ) ;
#100632 = CARTESIAN_POINT ( 'NONE',  ( -7.545178029317930246, 1384.916914618600003, 219.0875785980250043 ) ) ;
#100633 = CARTESIAN_POINT ( 'NONE',  ( -11.30252681748399901, 1471.157032186200013, 207.5285798585680084 ) ) ;
#100634 = CARTESIAN_POINT ( 'NONE',  ( -4.717896399877197666, 1508.208081382373848, 220.4986227734547128 ) ) ;
#100635 = CARTESIAN_POINT ( 'NONE',  ( 18.76071169450000298, 1415.996778985530000, 210.2851423563980120 ) ) ;
#100636 = CARTESIAN_POINT ( 'NONE',  ( -2.812687921020009973, 1454.522389872590111, 199.0175643825760119 ) ) ;
#100637 = CARTESIAN_POINT ( 'NONE',  ( -4.326079385514251641, 1515.193466644350337, 210.9648093357023697 ) ) ;
#100638 = CARTESIAN_POINT ( 'NONE',  ( 41.85283392122409651, 1440.913060353459969, 261.7677866120769750 ) ) ;
#100639 = B_SPLINE_CURVE_WITH_KNOTS ( 'NONE', 3,
 ( #42183, #26466, #52257, #745, #59544, #16938, #33761, #51140, #77444, #85266, #76895, #102604, #9130, #94220, #25351, #204, #67405, #8563, #18063, #51692, #109938, #50042, #93656, #86383, #34876, #58437, #60103, #92565, #84169, #103165, #17494, #42735, #34327, #25905, #85833, #43296, #60661, #9669, #43841, #7469, #77987, #93123, #35433, #24257, #41631, #75785 ),
 .UNSPECIFIED., .F., .F.,
 ( 4, 3, 3, 3, 3, 3, 3, 3, 3, 3, 3, 3, 3, 3, 3, 4 ),
 ( -33.33692105922289528, -32.30496137087640562, -30.87533264016670032, -29.45119221417040123, -28.03232753619460027, -26.62582012346450000, -25.22895400231270102, -23.84265630345680265, -23.19230641462139886, -21.81245709143689737, -20.43032364105260257, -19.04908065426700148, -17.67389872415650132, -16.30563378985170075, -14.94618987489860018, -13.59708442930000061 ),
 .UNSPECIFIED. ) ;
#100641 = DIRECTION ( 'NONE',  ( -0.000000000000000000, 1.000000000000000000, 0.000000000000000000 ) ) ;
#100640 = CARTESIAN_POINT ( 'NONE',  ( -10.24327470438359988, 1471.488599568509926, 210.1179836163729817 ) ) ;
#100642 = DIRECTION ( 'NONE',  ( 0.9127217750004207319, -0.3840007055116108625, -0.1395794383376949832 ) ) ;
#100643 = ORIENTED_EDGE ( 'NONE', *, *, #63306, .F. ) ;
#100644 = VERTEX_POINT ( 'NONE', #106053 ) ;
#100645 = CARTESIAN_POINT ( 'NONE',  ( 11.41287573240554032, 1427.618782186570115, 209.6357587079445182 ) ) ;
#100646 = CARTESIAN_POINT ( 'NONE',  ( -15.27152961130000008, 1506.433683729329914, 224.9338604266980326 ) ) ;
#100647 = CARTESIAN_POINT ( 'NONE',  ( -3.395799912579999802, 1442.082743038290118, 200.9143888862090250 ) ) ;
#100648 = CARTESIAN_POINT ( 'NONE',  ( 32.97913964219439720, 1511.187213306747708, 220.2739374644211807 ) ) ;
#100649 = CARTESIAN_POINT ( 'NONE',  ( 2178.386296064867111, -8387.357407334289746, -1553.770216230970163 ) ) ;
#100650 = CARTESIAN_POINT ( 'NONE',  ( -26.02647937380000087, 1444.708500955269983, 212.3004752285879988 ) ) ;
#100651 = CARTESIAN_POINT ( 'NONE',  ( -2.140641997699999965, 1508.551704408389924, 220.0635241299990241 ) ) ;
#100652 = CARTESIAN_POINT ( 'NONE',  ( 19.39983987835127976, 1522.861859112239699, 178.9515629539953636 ) ) ;
#100653 = CARTESIAN_POINT ( 'NONE',  ( -37.80963358037920585, 1383.831454921230034, 238.1220177388399861 ) ) ;
#100654 = EDGE_CURVE ( 'NONE', #105727, #47062, #71265, .T. ) ;
#100655 = CARTESIAN_POINT ( 'NONE',  ( -16.42420382550000113, 1507.212883782629888, 224.6993357452979865 ) ) ;
#100656 = ADVANCED_FACE ( 'NONE', ( #37196 ), #17691, .T. ) ;
#100657 = CARTESIAN_POINT ( 'NONE',  ( 25.16854692840000141, 1451.224506325429957, 137.5711277893979911 ) ) ;
#100658 = CARTESIAN_POINT ( 'NONE',  ( -27.42787280202326983, 1509.319616074060832, 212.0823359202047982 ) ) ;
#100659 = CARTESIAN_POINT ( 'NONE',  ( 11.32936712494479892, 1492.131809937580101, 211.0328881183560270 ) ) ;
#100660 = EDGE_CURVE ( 'NONE', #13629, #49383, #66260, .T. ) ;
#100662 = ORIENTED_EDGE ( 'NONE', *, *, #77661, .F. ) ;
#100661 = CARTESIAN_POINT ( 'NONE',  ( -2.019856026379999836, 1456.316848387589971, 218.3948360566789972 ) ) ;
#100663 = LINE ( 'NONE', #74949, #41360 ) ;
#100664 = CARTESIAN_POINT ( 'NONE',  ( -46.83374554580000648, 1379.942045336279762, 245.6713053846590071 ) ) ;
#100665 = EDGE_CURVE ( 'NONE', #73174, #3165, #23121, .T. ) ;
#100666 = CARTESIAN_POINT ( 'NONE',  ( -20.64057905079999955, 1409.633845290530189, 214.6320756031479959 ) ) ;
#100667 = ORIENTED_EDGE ( 'NONE', *, *, #53238, .T. ) ;
#100668 = ORIENTED_EDGE ( 'NONE', *, *, #60562, .F. ) ;
#100669 = EDGE_CURVE ( 'NONE', #88595, #94000, #91452, .T. ) ;
#100670 = CARTESIAN_POINT ( 'NONE',  ( -8.169799973510000868, 1501.392344667289990, 208.3166649180830063 ) ) ;
#100671 = CARTESIAN_POINT ( 'NONE',  ( -4.077242828485170278, 1515.224507406410112, 205.5390080823180199 ) ) ;
#100673 = DIRECTION ( 'NONE',  ( 0.000000000000000000, 1.000000000000000000, 0.000000000000000000 ) ) ;
#100672 = CARTESIAN_POINT ( 'NONE',  ( -31.81407709660760830, 1501.977400791986611, 221.9534378623334590 ) ) ;
#100675 = ADVANCED_FACE ( 'NONE', ( #14730 ), #78570, .T. ) ;
#100674 = CARTESIAN_POINT ( 'NONE',  ( 11.64374231457060027, 1480.041980269009855, 210.9631198931459721 ) ) ;
#100676 = CARTESIAN_POINT ( 'NONE',  ( -107.6180288740000037, 1380.687228087200083, 298.7908680479590089 ) ) ;
#100677 = CARTESIAN_POINT ( 'NONE',  ( -21.83863729848776458, 1523.580204110582372, 234.9763103240451301 ) ) ;
#100678 = CARTESIAN_POINT ( 'NONE',  ( -8.804153820836120303, 1508.551704408389924, 218.7132714456290046 ) ) ;
#100679 = CARTESIAN_POINT ( 'NONE',  ( -0.3530891408735000181, 1467.116854267079816, 235.6078141451939985 ) ) ;
#100680 = CARTESIAN_POINT ( 'NONE',  ( 0.5309744090729999755, 1408.931602422230071, 186.5522665233980035 ) ) ;
#100681 = CARTESIAN_POINT ( 'NONE',  ( 18.79226589730000185, 1456.307606824690083, 213.7887498653890077 ) ) ;
#100682 = CARTESIAN_POINT ( 'NONE',  ( 1.372916587609890104, 1432.414705139630087, 200.7998117957879742 ) ) ;
#100683 = CARTESIAN_POINT ( 'NONE',  ( -3.686335301026030020, 1441.157504315399819, 159.2179879833419989 ) ) ;
#100684 = CARTESIAN_POINT ( 'NONE',  ( -1.865418649941090079, 1450.587766904189948, 183.6624891833139941 ) ) ;
#100685 = ORIENTED_EDGE ( 'NONE', *, *, #110442, .T. ) ;
#100687 = EDGE_CURVE ( 'NONE', #110307, #12048, #95165, .T. ) ;
#100686 = CARTESIAN_POINT ( 'NONE',  ( -21.92333112166566167, 1524.538969332612623, 184.5696470164554341 ) ) ;
#100688 = CARTESIAN_POINT ( 'NONE',  ( 18.09254145655199864, 1458.632396074990083, 227.9585907476449904 ) ) ;
#100689 = CARTESIAN_POINT ( 'NONE',  ( -13.06415183560000060, 1435.235088203829946, 150.3757994387979977 ) ) ;
#100690 = CARTESIAN_POINT ( 'NONE',  ( -1.160048314478139921E-08, 1473.720592319110210, 262.7804507126890030 ) ) ;
#100691 = CARTESIAN_POINT ( 'NONE',  ( 19.74917098016377892, 1436.419552527919677, 145.7041280508210548 ) ) ;
#100692 = CARTESIAN_POINT ( 'NONE',  ( -23.61227025210000008, 1435.322036687620084, 137.2858276859979867 ) ) ;
#100693 = CARTESIAN_POINT ( 'NONE',  ( -107.4345822860000084, 1387.580258537220061, 310.2252759172590117 ) ) ;
#100694 = EDGE_CURVE ( 'NONE', #53518, #83932, #42148, .T. ) ;
#100695 = CARTESIAN_POINT ( 'NONE',  ( -1.464098976280000075, 1482.221117674429934, 182.5727748270979873 ) ) ;
#100696 = CARTESIAN_POINT ( 'NONE',  ( -10.23589100247646577, 1362.489324292358333, 210.6218459617030021 ) ) ;
#100697 = CARTESIAN_POINT ( 'NONE',  ( -113.4000000000000057, 1306.413060387289988, 304.2218459572590064 ) ) ;
#100698 = CARTESIAN_POINT ( 'NONE',  ( 13.77652653775929892, 1509.191610193870019, 234.0674600905030047 ) ) ;
#100699 = CARTESIAN_POINT ( 'NONE',  ( -8.259628006849998982, 1424.858822388950102, 205.8688264180890144 ) ) ;
#100700 = EDGE_CURVE ( 'NONE', #54152, #2493, #10132, .T. ) ;
#100701 = CARTESIAN_POINT ( 'NONE',  ( 2.486220101774999858, 1516.939658295650133, 209.1086089184300079 ) ) ;
#100702 = CARTESIAN_POINT ( 'NONE',  ( 5.563397900820960196, 1409.046698828469971, 222.4283399726890025 ) ) ;
#100703 = CARTESIAN_POINT ( 'NONE',  ( -14.17772861730700207, 1379.591530685439920, 207.8208986668599891 ) ) ;
#100704 = CARTESIAN_POINT ( 'NONE',  ( 6.937981266933950231, 1424.879596851670158, 213.3109209129980002 ) ) ;
#100705 = EDGE_CURVE ( 'NONE', #57731, #35548, #28748, .T. ) ;
#100706 = VERTEX_POINT ( 'NONE', #43801 ) ;
#100707 = CARTESIAN_POINT ( 'NONE',  ( 3.806770864790000264, 1421.349368237130193, 217.1428155965579947 ) ) ;
#100709 = DIRECTION ( 'NONE',  ( -0.9455185755993178454, 0.000000000000000000, 0.3255681544571539243 ) ) ;
#100708 = CARTESIAN_POINT ( 'NONE',  ( 0.4692969167009999887, 1499.385980790829990, 181.2668337229979727 ) ) ;
#100710 =( BOUNDED_CURVE ( )  B_SPLINE_CURVE ( 3, ( #24120, #31994, #74566, #33089 ),
 .UNSPECIFIED., .F., .F. ) 
 B_SPLINE_CURVE_WITH_KNOTS ( ( 4, 4 ),
 ( 1.914873758155674954, 2.475997143201050132 ),
 .UNSPECIFIED. ) 
 CURVE ( )  GEOMETRIC_REPRESENTATION_ITEM ( )  RATIONAL_B_SPLINE_CURVE ( ( 1.000000000000000000, 0.9739333732078443440, 0.9739333732078443440, 1.000000000000000000 ) ) 
 REPRESENTATION_ITEM ( '' )  );
#100711 = DIRECTION ( 'NONE',  ( -0.6736849260863841948, 0.000000000000000000, 0.7390186874254148774 ) ) ;
#100712 = CARTESIAN_POINT ( 'NONE',  ( 12.53380499174499896, 1445.052233488290085, 169.4755105688890069 ) ) ;
#100713 = CARTESIAN_POINT ( 'NONE',  ( -1.748905560439999896, 1488.269106391890091, 219.8524659834990018 ) ) ;
#100714 = CARTESIAN_POINT ( 'NONE',  ( -5.957780160061970420, 1452.705010119680082, 151.8756781206909920 ) ) ;
#100715 = FACE_OUTER_BOUND ( 'NONE', #90527, .T. ) ;
#100716 = ORIENTED_EDGE ( 'NONE', *, *, #29533, .F. ) ;
#100717 = CARTESIAN_POINT ( 'NONE',  ( 17.04881831986960350, 1423.676757034399998, 228.9400447418400120 ) ) ;
#100718 = CARTESIAN_POINT ( 'NONE',  ( 10.47517306970000028, 1461.766207292889931, 210.2934874650690062 ) ) ;
#100719 = ORIENTED_EDGE ( 'NONE', *, *, #7569, .F. ) ;
#100720 = ORIENTED_EDGE ( 'NONE', *, *, #37738, .F. ) ;
#100721 = CARTESIAN_POINT ( 'NONE',  ( -62.45870848130000041, 1384.816439370750004, 249.2996736312589974 ) ) ;
#100722 = CARTESIAN_POINT ( 'NONE',  ( -24.07468318869999990, 1410.986369303230049, 209.5863555680950014 ) ) ;
#100723 = CARTESIAN_POINT ( 'NONE',  ( -4.066872906969999590, 1425.385209600230155, 186.1255799332980132 ) ) ;
#100724 = CARTESIAN_POINT ( 'NONE',  ( -31.44837959398574867, 1512.187213306747481, 220.9083067115980725 ) ) ;
#100725 = CARTESIAN_POINT ( 'NONE',  ( -45.48552204837235990, 1437.736068879899449, 266.1938101863335078 ) ) ;
#100726 = CARTESIAN_POINT ( 'NONE',  ( -13.72848320130000133, 1498.343405282130107, 232.0117512395979986 ) ) ;
#100727 = CARTESIAN_POINT ( 'NONE',  ( -18.13779422170000188, 1410.879222528129958, 224.5374549592980031 ) ) ;
#100728 = CARTESIAN_POINT ( 'NONE',  ( 44.59751383069639985, 1448.382420665780046, 269.0041120828120143 ) ) ;
#100729 = CARTESIAN_POINT ( 'NONE',  ( -10.44070837812300034, 1391.913060387289988, 204.6731945046309704 ) ) ;
#100730 = EDGE_CURVE ( 'NONE', #95247, #47770, #30077, .T. ) ;
#100731 = DIRECTION ( 'NONE',  ( 1.755985294532464991E-16, -1.000000000000000000, 1.338183447452830017E-16 ) ) ;
#100732 = CARTESIAN_POINT ( 'NONE',  ( 1.703779605225000049, 1517.057265928030120, 205.0766634521770015 ) ) ;
#100733 = ORIENTED_EDGE ( 'NONE', *, *, #96661, .F. ) ;
#100734 = CARTESIAN_POINT ( 'NONE',  ( 18.35990977646854105, 1459.057757268718206, 227.7645059598757484 ) ) ;
#100735 = CARTESIAN_POINT ( 'NONE',  ( -1.034405465910470001, 1444.468934022600024, 199.1208377739500008 ) ) ;
#100736 = CARTESIAN_POINT ( 'NONE',  ( 0.06577166592579929139, 1429.775327338489888, 214.7293410279390002 ) ) ;
#100737 = ORIENTED_EDGE ( 'NONE', *, *, #54943, .T. ) ;
#100738 = CARTESIAN_POINT ( 'NONE',  ( 4.491284101707059939, 1508.884228866460035, 206.6339218519869974 ) ) ;
#100739 = CARTESIAN_POINT ( 'NONE',  ( 26.92975820915080121, 1451.047125116810093, 136.3586291375359849 ) ) ;
#100740 = CARTESIAN_POINT ( 'NONE',  ( -12.45742386984340122, 1512.169469372310004, 194.1709192302429869 ) ) ;
#100741 = CARTESIAN_POINT ( 'NONE',  ( 7.703548237945829769, 1504.124514085119927, 219.2853995089439820 ) ) ;
#100742 = CARTESIAN_POINT ( 'NONE',  ( 7.767274028600000157, 1421.765204529709990, 195.8385879648990056 ) ) ;
#100743 = CARTESIAN_POINT ( 'NONE',  ( -0.05601447201598130227, 1431.857486804389964, 218.6169334100210051 ) ) ;
#100744 = CARTESIAN_POINT ( 'NONE',  ( -4.922543830899999584, 1496.353864017489968, 199.0299218828990035 ) ) ;
#100745 = CARTESIAN_POINT ( 'NONE',  ( 10.74022137903229890, 1409.288117182390124, 190.7342599600210065 ) ) ;
#100747 = CARTESIAN_POINT ( 'NONE',  ( 33.28034951413933129, 1512.187213306747481, 217.4407153818819722 ) ) ;
#100746 = DIRECTION ( 'NONE',  ( 0.9999999999999875655, -4.362347470284412856E-08, -1.513066404587939241E-07 ) ) ;
#100748 = CARTESIAN_POINT ( 'NONE',  ( 11.13262782095319814, 1425.908268888629891, 206.4954163449100122 ) ) ;
#100749 = ADVANCED_FACE ( 'NONE', ( #34839 ), #96415, .T. ) ;
#100750 = CARTESIAN_POINT ( 'NONE',  ( -11.32418084390000068, 1378.916280331980033, 214.2342780821290091 ) ) ;
#100751 = CARTESIAN_POINT ( 'NONE',  ( 7.276969490589999978, 1429.103926496630038, 148.8100812095979961 ) ) ;
#100752 = ORIENTED_EDGE ( 'NONE', *, *, #22937, .T. ) ;
#100753 = CARTESIAN_POINT ( 'NONE',  ( 10.78869841494559978, 1414.913060387399810, 221.8582824516670087 ) ) ;
#100754 = DIRECTION ( 'NONE',  ( -1.755985294532469921E-16, 1.000000000000000000, -1.338183447452831989E-16 ) ) ;
#100755 = CARTESIAN_POINT ( 'NONE',  ( 20.59684415639999955, 1507.762623716630060, 227.3081670307980175 ) ) ;
#100756 = CARTESIAN_POINT ( 'NONE',  ( -10.29442817569999846, 1389.680258987810021, 202.2226486107689993 ) ) ;
#100757 = CARTESIAN_POINT ( 'NONE',  ( 20.22418986319999590, 1476.021096013189890, 210.1149224964580071 ) ) ;
#100758 = CARTESIAN_POINT ( 'NONE',  ( 11.72053595058989828, 1425.791693304140153, 202.8787723380090142 ) ) ;
#100759 = CARTESIAN_POINT ( 'NONE',  ( 0.8465175048109989664, 1430.128326741589945, 217.4134717798089866 ) ) ;
#100760 = CARTESIAN_POINT ( 'NONE',  ( -16.86383896579999941, 1465.456048507830019, 262.6648722463980334 ) ) ;
#100761 = ADVANCED_FACE ( 'NONE', ( #62286 ), #97510, .T. ) ;
#100762 = B_SPLINE_CURVE_WITH_KNOTS ( 'NONE', 3,
 ( #61424, #26114, #87721, #8767 ),
 .UNSPECIFIED., .F., .F.,
 ( 4, 4 ),
 ( 0.9643540914522175100, 1.000000000000000000 ),
 .UNSPECIFIED. ) ;
#100763 = CARTESIAN_POINT ( 'NONE',  ( -8.864146540411450559, 1384.685144641450051, 218.6774944319709846 ) ) ;
#100764 = CARTESIAN_POINT ( 'NONE',  ( 11.14671186430000027, 1434.019362591839808, 151.6529851529979851 ) ) ;
#100765 = CARTESIAN_POINT ( 'NONE',  ( 43.50000000000000000, 1445.861068816730040, 271.1218459616979999 ) ) ;
#100766 = CARTESIAN_POINT ( 'NONE',  ( 12.73643648997659916, 1414.913060387399810, 198.3331475467240068 ) ) ;
#100767 = EDGE_CURVE ( 'NONE', #43749, #49944, #88827, .T. ) ;
#100768 = CARTESIAN_POINT ( 'NONE',  ( 0.04809667444139999887, 1420.202366602630036, 183.9005171462980002 ) ) ;
#100769 = AXIS2_PLACEMENT_3D ( 'NONE', #95114, #43063, #25124 ) ;
#100770 = CARTESIAN_POINT ( 'NONE',  ( -15.06279714670009362, 1422.388303180917092, 229.4662111538715976 ) ) ;
#100771 = DIRECTION ( 'NONE',  ( 0.000000000000000000, 0.000000000000000000, -1.000000000000000000 ) ) ;
#100772 = CARTESIAN_POINT ( 'NONE',  ( 45.63712948719999218, 1440.913080918340029, 268.9747524690979503 ) ) ;
#100773 = CARTESIAN_POINT ( 'NONE',  ( 17.92792478850000037, 1415.296882282229944, 210.0737307021219920 ) ) ;
#100774 = CARTESIAN_POINT ( 'NONE',  ( 21.30585457869999999, 1410.903636177029966, 217.6543277114180057 ) ) ;
#100775 = VECTOR ( 'NONE', #47751, 1000.000000000000000 ) ;
#100776 = CARTESIAN_POINT ( 'NONE',  ( -0.3672702989670010298, 1473.612351522490144, 216.6187257883390203 ) ) ;
#100777 = CARTESIAN_POINT ( 'NONE',  ( -5.513264357029999729, 1374.913060387289988, 203.3066656689789795 ) ) ;
#100778 = CARTESIAN_POINT ( 'NONE',  ( 4.945361357476200142E-08, 1407.050502962379824, 196.1173069476189994 ) ) ;
#100779 = CARTESIAN_POINT ( 'NONE',  ( -2.038847259681869417, 1522.861859112239017, 173.3106345060298281 ) ) ;
#100780 = EDGE_CURVE ( 'NONE', #96332, #94274, #80712, .T. ) ;
#100781 = CARTESIAN_POINT ( 'NONE',  ( 14.17511961927979947, 1428.761297916650165, 195.0897163562519836 ) ) ;
#100782 = CARTESIAN_POINT ( 'NONE',  ( -10.47220825560000002, 1415.931784855930118, 223.5877942017980047 ) ) ;
#100783 = CARTESIAN_POINT ( 'NONE',  ( 0.2068092021342020081, 1459.144971641600023, 182.9897654969599898 ) ) ;
#100785 = ORIENTED_EDGE ( 'NONE', *, *, #46715, .F. ) ;
#100784 = CARTESIAN_POINT ( 'NONE',  ( 0.06333885262469998723, 1408.725629458430149, 223.1955288097980201 ) ) ;
#100786 = CARTESIAN_POINT ( 'NONE',  ( -13.35741048202589809, 1444.324653571830822, 164.9741927960640453 ) ) ;
#100787 = B_SPLINE_CURVE_WITH_KNOTS ( 'NONE', 3,
 ( #2872, #36992, #62232, #95256, #17970, #77904, #70638, #34792 ),
 .UNSPECIFIED., .F., .F.,
 ( 4, 2, 2, 4 ),
 ( 0.000000000000000000, 0.001508139020063445400, 0.003016278040126890801, 0.006032556080253484096 ),
 .UNSPECIFIED. ) ;
#100788 = EDGE_CURVE ( 'NONE', #70084, #75960, #19122, .T. ) ;
#100789 = DIRECTION ( 'NONE',  ( 0.000000000000000000, 0.000000000000000000, -1.000000000000000000 ) ) ;
#100790 = FACE_OUTER_BOUND ( 'NONE', #11379, .T. ) ;
#100791 = CARTESIAN_POINT ( 'NONE',  ( -41.06928241268209234, 1446.732447648640118, 134.0999999985529882 ) ) ;
#100792 = CARTESIAN_POINT ( 'NONE',  ( -109.3493610729999972, 1384.903287640260032, 297.1385568369590260 ) ) ;
#100793 = ORIENTED_EDGE ( 'NONE', *, *, #7428, .F. ) ;
#100794 = B_SPLINE_SURFACE_WITH_KNOTS ( 'NONE', 5, 1, ( 
 ( #22378, #30806 ),
 ( #24038, #90152 ),
 ( #57144, #109727 ),
 ( #64443, #13434 ),
 ( #15091, #49837 ),
 ( #91271, #21828 ) ),
 .UNSPECIFIED., .F., .F., .F.,
 ( 6, 6 ),
 ( 2, 2 ),
 ( 0.000000000000000000, 52.98902693510000006 ),
 ( -1.500000000000000000, 1.500000000000000000 ),
 .UNSPECIFIED. ) ;
#100795 = CARTESIAN_POINT ( 'NONE',  ( -1.436398804920000050, 1485.575541285890040, 197.7087229570989848 ) ) ;
#100796 = CARTESIAN_POINT ( 'NONE',  ( 3.350338079455597029, 1523.604703353109699, 176.1628856388066708 ) ) ;
#100797 = CARTESIAN_POINT ( 'NONE',  ( -9.016783256541959446, 1383.231411182179954, 220.4219636834260143 ) ) ;
#100798 = LINE ( 'NONE', #92400, #99950 ) ;
#100799 = CIRCLE ( 'NONE', #7854, 1.000000000000000888 ) ;
#100800 = CARTESIAN_POINT ( 'NONE',  ( -3.430356047799270058, 1431.707894944020154, 216.7924308075639885 ) ) ;
#100801 = DIRECTION ( 'NONE',  ( -0.1285470394059259891, 0.7041304581555918318, -0.6983379959285959115 ) ) ;
#100802 = CARTESIAN_POINT ( 'NONE',  ( 21.36149126229999951, 1471.309244719029948, 210.4493499929980089 ) ) ;
#100803 = DIRECTION ( 'NONE',  ( -0.9417419115949662300, -0.2378257470769920556, 0.2378257470769920556 ) ) ;
#100804 = CARTESIAN_POINT ( 'NONE',  ( 3.984081755090749688, 1515.551704407335137, 210.9648081771169643 ) ) ;
#100805 = B_SPLINE_SURFACE_WITH_KNOTS ( 'NONE', 5, 4, ( 
 ( #98506, #55975, #53795, #90100, #44830 ),
 ( #78984, #2287, #36399, #2827, #105263 ),
 ( #109139, #6657, #30753, #39716, #15579 ),
 ( #23451, #108568, #73880, #83913, #57089 ),
 ( #15035, #82810, #40811, #31857, #74988 ),
 ( #109676, #90656, #66043, #82266, #13939 ) ),
 .UNSPECIFIED., .F., .F., .F.,
 ( 6, 6 ),
 ( 5, 5 ),
 ( 0.000000000000000000, 52.98902693510000006 ),
 ( 25.78146411700000229, 39.23969207129999859 ),
 .UNSPECIFIED. ) ;
#100806 = CARTESIAN_POINT ( 'NONE',  ( -54.91437447499630053, 1385.038116820099958, 233.6872214610490062 ) ) ;
#100807 = CARTESIAN_POINT ( 'NONE',  ( -10.91810810328910009, 1391.913060387289988, 212.7120084556750044 ) ) ;
#100808 = CARTESIAN_POINT ( 'NONE',  ( 11.26800005207859812, 1422.300764229830065, 207.0940410118970192 ) ) ;
#100809 = CARTESIAN_POINT ( 'NONE',  ( 204.2714532754872323, 1526.382868172863937, 194.5341519463041777 ) ) ;
#100810 = EDGE_CURVE ( 'NONE', #100850, #2071, #54151, .T. ) ;
#100811 = CARTESIAN_POINT ( 'NONE',  ( -15.86483609532009886, 1409.570356571889988, 225.8689455459189901 ) ) ;
#100813 = ORIENTED_EDGE ( 'NONE', *, *, #27283, .F. ) ;
#100812 = CARTESIAN_POINT ( 'NONE',  ( 1.100421420896519953, 1437.654385139740043, 227.6420619421519973 ) ) ;
#100814 = CARTESIAN_POINT ( 'NONE',  ( 3.171904416549999883, 1474.503316444290022, 220.1039004212989880 ) ) ;
#100815 = CARTESIAN_POINT ( 'NONE',  ( 10.94247266901300186, 1470.964281316320239, 209.6238199810090066 ) ) ;
#100816 = CARTESIAN_POINT ( 'NONE',  ( -19.24471802889106442, 1410.946680197057731, 222.4942342983714809 ) ) ;
#100817 = CARTESIAN_POINT ( 'NONE',  ( -109.1218945300000058, 1384.640297123439950, 311.2547333012590229 ) ) ;
#100818 = CARTESIAN_POINT ( 'NONE',  ( -0.1109497542296510042, 1419.781979276719994, 184.1980523464999919 ) ) ;
#100819 = LINE ( 'NONE', #34183, #92941 ) ;
#100820 = CARTESIAN_POINT ( 'NONE',  ( 15.91746618545751524, 1512.594959757391052, 198.1541272149443671 ) ) ;
#100821 = CARTESIAN_POINT ( 'NONE',  ( -17.69798016750000258, 1424.268916621029803, 226.8670750680979893 ) ) ;
#100822 = CARTESIAN_POINT ( 'NONE',  ( -3.141753572004903461, 1511.860476876181110, 201.1893397601683944 ) ) ;
#100823 = CARTESIAN_POINT ( 'NONE',  ( 8.746374439269999357, 1448.961682185689824, 206.1466908165390066 ) ) ;
#100824 = CARTESIAN_POINT ( 'NONE',  ( -100.1346419727999972, 1320.102705746889797, 307.6090480346439904 ) ) ;
#100825 = CARTESIAN_POINT ( 'NONE',  ( 15.96958168569999970, 1519.913060387329779, 226.4768549569980109 ) ) ;
#100826 = FACE_OUTER_BOUND ( 'NONE', #11615, .T. ) ;
#100827 = CARTESIAN_POINT ( 'NONE',  ( -0.7574260232259989456, 1516.837969789639828, 205.8660360680970030 ) ) ;
#100828 = CARTESIAN_POINT ( 'NONE',  ( 3.115733349899999727, 1446.573609258350189, 168.9983159132980006 ) ) ;
#100829 = ORIENTED_EDGE ( 'NONE', *, *, #27571, .T. ) ;
#100830 = EDGE_CURVE ( 'NONE', #10931, #21131, #29743, .T. ) ;
#100831 = CARTESIAN_POINT ( 'NONE',  ( -11.13055623967079555, 1375.886883438980021, 214.2704005330025723 ) ) ;
#100832 = DIRECTION ( 'NONE',  ( -0.9417419115949053898, 0.3363363969979660806, 0.000000000000000000 ) ) ;
#100834 = ORIENTED_EDGE ( 'NONE', *, *, #52202, .F. ) ;
#100833 = CARTESIAN_POINT ( 'NONE',  ( -68.66495634729999153, 1379.747814253419847, 280.2580260664590242 ) ) ;
#100835 = CARTESIAN_POINT ( 'NONE',  ( -17.53940096235950108, 1417.889611524100246, 206.8563643866829977 ) ) ;
#100836 = ORIENTED_EDGE ( 'NONE', *, *, #74895, .T. ) ;
#100837 = FACE_OUTER_BOUND ( 'NONE', #66752, .T. ) ;
#100838 = CARTESIAN_POINT ( 'NONE',  ( 11.09014987159999954, 1501.265658831390056, 206.2946274632390100 ) ) ;
#100840 = CARTESIAN_POINT ( 'NONE',  ( 16.01103362314420053, 1409.480392854180081, 192.8179007169949841 ) ) ;
#100839 = CARTESIAN_POINT ( 'NONE',  ( -10.81843803384433400, 1424.919119117232640, 144.3742235356994001 ) ) ;
#100841 = CARTESIAN_POINT ( 'NONE',  ( 7.725990161824999980, 1517.181921232829836, 211.6070516194370157 ) ) ;
#100842 = CARTESIAN_POINT ( 'NONE',  ( 41.15021254218909519, 1443.107472741189895, 136.8558449723329886 ) ) ;
#100843 = CARTESIAN_POINT ( 'NONE',  ( -106.6934947193090011, 1378.913060387289988, 306.7339471936149948 ) ) ;
#100844 = SPHERICAL_SURFACE ( 'NONE', #16096, 1.999999999990000221 ) ;
#100845 = CARTESIAN_POINT ( 'NONE',  ( 16.60410810222508715, 1460.741495510953882, 229.0095566175009196 ) ) ;
#100846 = CARTESIAN_POINT ( 'NONE',  ( 4.987078393879730065, 1508.551704408389924, 211.6860916102569661 ) ) ;
#100847 =( BOUNDED_CURVE ( )  B_SPLINE_CURVE ( 3, ( #72679, #47474, #46939, #4901 ),
 .UNSPECIFIED., .F., .T. ) 
 B_SPLINE_CURVE_WITH_KNOTS ( ( 4, 4 ),
 ( 0.000000000000000000, 0.7048113239778087680 ),
 .UNSPECIFIED. ) 
 CURVE ( )  GEOMETRIC_REPRESENTATION_ITEM ( )  RATIONAL_B_SPLINE_CURVE ( ( 1.000000000000000000, 0.9590300661663088144, 0.9590300661663088144, 1.000000000000000000 ) ) 
 REPRESENTATION_ITEM ( '' )  );
#100848 = B_SPLINE_CURVE_WITH_KNOTS ( 'NONE', 3,
 ( #22734, #64805, #83226, #40669, #32809, #22186, #66994, #56384, #100013, #23303, #82115, #5969, #5414, #49638, #65348, #14349, #101104, #58588, #66453, #40114, #57498, #91623, #14899, #23847 ),
 .UNSPECIFIED., .F., .F.,
 ( 4, 2, 1, 1, 2, 2, 2, 2, 2, 1, 1, 2, 2, 4 ),
 ( 0.000000000000000000, 0.1249999999997721822, 0.1874999999996589395, 0.2187499999995849431, 0.2343749999995655697, 0.2499999999995461963, 0.3749999999995765609, 0.4999999999996068700, 0.6249999999996371791, 0.6874999999996733724, 0.7187499999997116751, 0.7343749999997076783, 0.7499999999997037925, 1.000000000000000000 ),
 .UNSPECIFIED. ) ;
#100849 = CYLINDRICAL_SURFACE ( 'NONE', #56126, 1.000000000000000888 ) ;
#100850 = VERTEX_POINT ( 'NONE', #14589 ) ;
#100851 = CARTESIAN_POINT ( 'NONE',  ( -17.84104287039070158, 1489.004150074129939, 195.1797407690729926 ) ) ;
#100852 = CARTESIAN_POINT ( 'NONE',  ( 18.02257621027597523, 1526.382868172863937, 235.3484976865586873 ) ) ;
#100853 = ORIENTED_EDGE ( 'NONE', *, *, #37161, .F. ) ;
#100854 = ORIENTED_EDGE ( 'NONE', *, *, #20778, .F. ) ;
#100855 = AXIS2_PLACEMENT_3D ( 'NONE', #92879, #81710, #73338 ) ;
#100856 = CARTESIAN_POINT ( 'NONE',  ( -29.78202337382098719, 1510.000480301286643, 209.1081380337732014 ) ) ;
#100857 = CARTESIAN_POINT ( 'NONE',  ( -6.752164255999639764, 1508.178364352339941, 220.1479925240329862 ) ) ;
#100858 = CARTESIAN_POINT ( 'NONE',  ( -18.43222347473149725, 1508.250680623890048, 209.6150243477850097 ) ) ;
#100859 = CARTESIAN_POINT ( 'NONE',  ( 4.325405441710000076, 1515.219201591190085, 210.9648081929590262 ) ) ;
#100860 = VECTOR ( 'NONE', #105218, 1000.000000000000000 ) ;
#100861 = CARTESIAN_POINT ( 'NONE',  ( -26.55602695130000157, 1507.993014311030038, 202.0788793302480144 ) ) ;
#100862 = CARTESIAN_POINT ( 'NONE',  ( 36.37832872589339672, 1451.642701155429904, 134.7402676982789842 ) ) ;
#100863 = CARTESIAN_POINT ( 'NONE',  ( 2.412365803710859957, 1421.274619602949997, 183.2637791671220100 ) ) ;
#100864 = CARTESIAN_POINT ( 'NONE',  ( 25.98834105490000113, 1441.634093238639934, 138.4860864432980065 ) ) ;
#100865 = CARTESIAN_POINT ( 'NONE',  ( -11.44054090840000093, 1391.153937292269802, 213.9067485665989921 ) ) ;
#100866 = CARTESIAN_POINT ( 'NONE',  ( -83.03334324507059705, 1384.808909933130053, 286.7532168304919651 ) ) ;
#100867 = ORIENTED_EDGE ( 'NONE', *, *, #31531, .T. ) ;
#100868 = CARTESIAN_POINT ( 'NONE',  ( -5.779603138255000161, 1516.738222552470233, 201.4074744291170020 ) ) ;
#100869 = CARTESIAN_POINT ( 'NONE',  ( -6.563915562015000482, 1517.184063036290127, 207.9975562766469750 ) ) ;
#100870 = ORIENTED_EDGE ( 'NONE', *, *, #31011, .F. ) ;
#100871 = CARTESIAN_POINT ( 'NONE',  ( 11.82157071559280048, 1429.389078854110039, 149.1371689452649889 ) ) ;
#100872 = CARTESIAN_POINT ( 'NONE',  ( 2.957482190928379495, 1512.146734775097912, 217.0093202360658609 ) ) ;
#100873 = ORIENTED_EDGE ( 'NONE', *, *, #85906, .F. ) ;
#100874 = CARTESIAN_POINT ( 'NONE',  ( -14.41084201949999866, 1416.311719782429918, 221.3435843107980077 ) ) ;
#100875 = CARTESIAN_POINT ( 'NONE',  ( 7.370119641675869637, 1429.027654456439905, 215.0938587317789938 ) ) ;
#100876 = LINE ( 'NONE', #49409, #74324 ) ;
#100877 = CARTESIAN_POINT ( 'NONE',  ( -9.416464707496981390, 1461.065390459309810, 206.8423381932979908 ) ) ;
#100878 = CARTESIAN_POINT ( 'NONE',  ( -12.93109072819999916, 1422.976826963529902, 222.1731802233979920 ) ) ;
#100879 = CARTESIAN_POINT ( 'NONE',  ( 10.32832267219609967, 1469.723099828480144, 207.2225980447589961 ) ) ;
#100880 = CARTESIAN_POINT ( 'NONE',  ( -10.07154918490000028, 1473.228065907190057, 207.4129428866989997 ) ) ;
#100881 = CARTESIAN_POINT ( 'NONE',  ( 7.793403662019999345, 1494.414358568890066, 218.7662867540790046 ) ) ;
#100882 = CARTESIAN_POINT ( 'NONE',  ( -17.01808899029999722, 1507.624369750830056, 224.5631704104980031 ) ) ;
#100884 = PLANE ( 'NONE',  #54751 ) ;
#100883 = CARTESIAN_POINT ( 'NONE',  ( 12.85312037260000118, 1463.342809956830024, 231.1568051887979891 ) ) ;
#100885 = CARTESIAN_POINT ( 'NONE',  ( -24.18363701780000241, 1464.258769156330118, 212.1671259816380086 ) ) ;
#100886 = ADVANCED_FACE ( 'NONE', ( #15128 ), #58680, .T. ) ;
#100887 = CARTESIAN_POINT ( 'NONE',  ( 3.454119916704999849, 1516.594591938570147, 216.8324563732270178 ) ) ;
#100888 = ORIENTED_EDGE ( 'NONE', *, *, #32585, .F. ) ;
#100889 = CARTESIAN_POINT ( 'NONE',  ( -22.70357455280006320, 1409.705856010732305, 209.2041244077560691 ) ) ;
#100890 = CARTESIAN_POINT ( 'NONE',  ( -0.2682795917991919743, 1457.891717849350016, 229.2666142623699841 ) ) ;
#100891 = CARTESIAN_POINT ( 'NONE',  ( -21.50855465201878403, 1524.374578187332872, 234.1183740972438159 ) ) ;
#100892 = CARTESIAN_POINT ( 'NONE',  ( 5.009478067315000338, 1516.886345593249871, 213.7343532441369973 ) ) ;
#100893 = CARTESIAN_POINT ( 'NONE',  ( 4.329415264797519924, 1515.068899375750107, 212.0799422158490017 ) ) ;
#100894 = CARTESIAN_POINT ( 'NONE',  ( 3.829620113550000315, 1515.551704408389924, 206.7917118356089929 ) ) ;
#100896 = ORIENTED_EDGE ( 'NONE', *, *, #57038, .F. ) ;
#100895 = CARTESIAN_POINT ( 'NONE',  ( -12.44369114979409829, 1501.867506418240055, 211.6083604211140141 ) ) ;
#100897 = CARTESIAN_POINT ( 'NONE',  ( -15.57383198649972478, 1415.691259407821008, 209.6195876535002185 ) ) ;
#100898 = CARTESIAN_POINT ( 'NONE',  ( -15.45814007687169855, 1507.562497965019929, 192.1857156550819923 ) ) ;
#100899 = EDGE_CURVE ( 'NONE', #86629, #107071, #106932, .T. ) ;
#100900 = CARTESIAN_POINT ( 'NONE',  ( -11.86556339589999887, 1432.298474684649818, 149.9824464742980012 ) ) ;
#100901 = CARTESIAN_POINT ( 'NONE',  ( 0.000000000000000000, 1523.409940573003951, 209.1218459616979999 ) ) ;
#100902 = CARTESIAN_POINT ( 'NONE',  ( -6.402186394137180159, 1442.114340014330082, 201.8762545916499960 ) ) ;
#100903 = CARTESIAN_POINT ( 'NONE',  ( 27.03107205873159913, 1451.493498638970550, 136.0706325128519438 ) ) ;
#100904 = CARTESIAN_POINT ( 'NONE',  ( -7.738175793921410417, 1425.683019801390174, 203.9398901317029811 ) ) ;
#100905 = CARTESIAN_POINT ( 'NONE',  ( 5.524836877539999414, 1479.546334898089981, 203.7511963579289898 ) ) ;
#100907 = CARTESIAN_POINT ( 'NONE',  ( -10.32767976395509990, 1481.876697752989912, 206.1677484232849906 ) ) ;
#100906 = CARTESIAN_POINT ( 'NONE',  ( -25.21444118569999659, 1482.720987867629901, 215.4305335357680065 ) ) ;
#100908 = CARTESIAN_POINT ( 'NONE',  ( -16.97075622830800157, 1460.580119305637936, 228.2620270748900282 ) ) ;
#100909 = ORIENTED_EDGE ( 'NONE', *, *, #104233, .T. ) ;
#100910 = CARTESIAN_POINT ( 'NONE',  ( -5.011367984924999242, 1516.974592746400049, 205.6720686163770324 ) ) ;
#100911 = CARTESIAN_POINT ( 'NONE',  ( 3.773527540909999978, 1405.891018842429730, 268.4776619642979654 ) ) ;
#100912 = CARTESIAN_POINT ( 'NONE',  ( 0.02533456534659999856, 1409.857531607930014, 185.0280042643979925 ) ) ;
#100914 = B_SPLINE_CURVE_WITH_KNOTS ( 'NONE', 3,
 ( #26424, #41721, #34832, #60618, #66947, #52757, #75881, #41173, #61724, #19113, #110029, #23799, #69018, #45476, #89641 ),
 .UNSPECIFIED., .F., .F.,
 ( 4, 2, 2, 1, 1, 1, 2, 2, 4 ),
 ( 0.000000000000000000, 0.2500000000000387468, 0.3750000000000583422, 0.4375000000000648370, 0.4687500000000691114, 0.4843750000000749956, 0.4921875000000756617, 0.5000000000000762723, 1.000000000000000000 ),
 .UNSPECIFIED. ) ;
#100913 = CARTESIAN_POINT ( 'NONE',  ( -5.513264357029999729, 1375.413060387289988, 209.1218459572589836 ) ) ;
#100915 = CARTESIAN_POINT ( 'NONE',  ( -0.3501503302830000219, 1508.580655915329999, 237.8908601207980098 ) ) ;
#100916 = CARTESIAN_POINT ( 'NONE',  ( 3.597520269628190270, 1454.162627168660038, 217.7902427506969900 ) ) ;
#100917 = CARTESIAN_POINT ( 'NONE',  ( 11.89463746674639921, 1434.488622511689982, 147.6463952746719883 ) ) ;
#100918 = CARTESIAN_POINT ( 'NONE',  ( 18.22873622136830107, 1457.634151734390116, 229.9687917111629929 ) ) ;
#100919 = CARTESIAN_POINT ( 'NONE',  ( -15.31079571090000080, 1415.244376457269937, 207.2352505607890123 ) ) ;
#100920 = CARTESIAN_POINT ( 'NONE',  ( -14.09544100519999965, 1444.804768886640204, 188.5648275900980195 ) ) ;
#100921 = EDGE_CURVE ( 'NONE', #32575, #10141, #48784, .T. ) ;
#100922 = CARTESIAN_POINT ( 'NONE',  ( -19.88319835444530881, 1485.218947032791220, 190.7798981299888226 ) ) ;
#100923 = CARTESIAN_POINT ( 'NONE',  ( -16.20543174878743287, 1419.737581145931244, 209.9462470130569329 ) ) ;
#100924 = CARTESIAN_POINT ( 'NONE',  ( -9.202596930160000355, 1498.966442822989848, 216.3590987745790244 ) ) ;
#100925 = EDGE_CURVE ( 'NONE', #104047, #18275, #55527, .T. ) ;
#100926 = CARTESIAN_POINT ( 'NONE',  ( 4.046562303720000031, 1471.775282961290031, 189.4720092632990145 ) ) ;
#100927 = CARTESIAN_POINT ( 'NONE',  ( 4.440892098500000496E-16, 1426.979439823029907, 214.3676144195279676 ) ) ;
#100928 = CIRCLE ( 'NONE', #63432, 1.999999999984720223 ) ;
#100930 = EDGE_CURVE ( 'NONE', #35462, #103755, #43424, .T. ) ;
#100929 = CARTESIAN_POINT ( 'NONE',  ( 10.54606093473799966, 1481.256042122329973, 208.4465981898469806 ) ) ;
#100931 = CARTESIAN_POINT ( 'NONE',  ( 21.80961449745507963, 1523.919934424249959, 234.9115581881929415 ) ) ;
#100932 = B_SPLINE_CURVE_WITH_KNOTS ( 'NONE', 3,
 ( #21338, #89668, #23960, #32925, #49755, #75515 ),
 .UNSPECIFIED., .F., .F.,
 ( 4, 2, 4 ),
 ( 1.040834085586084257E-17, 0.001087661325621706431, 0.002175322651243402454 ),
 .UNSPECIFIED. ) ;
#100933 = CARTESIAN_POINT ( 'NONE',  ( -3.730291349180000271, 1475.207392057629932, 269.4937594316980380 ) ) ;
#100934 = CARTESIAN_POINT ( 'NONE',  ( -4.231249791687170081, 1446.302986648280239, 164.6653561940370025 ) ) ;
#100935 = CARTESIAN_POINT ( 'NONE',  ( -21.47619586280000092, 1509.724487542230008, 188.4280987144979633 ) ) ;
#100936 = AXIS2_PLACEMENT_3D ( 'NONE', #54278, #80559, #10037 ) ;
#100937 = CARTESIAN_POINT ( 'NONE',  ( -11.91486543419761546, 1486.509543025264520, 184.3429713432209383 ) ) ;
#100938 = CARTESIAN_POINT ( 'NONE',  ( -45.76759480931980306, 1384.760497626650022, 253.0762944135069858 ) ) ;
#100939 = CARTESIAN_POINT ( 'NONE',  ( -106.5202740518050035, 1391.913060387289988, 303.0849643599170236 ) ) ;
#100940 = AXIS2_PLACEMENT_3D ( 'NONE', #87881, #13326, #80566 ) ;
#100941 = CARTESIAN_POINT ( 'NONE',  ( -9.522333297019999421, 1438.200918636809774, 153.1793569429979982 ) ) ;
#100942 = ADVANCED_FACE ( 'NONE', ( #42013 ), #84555, .T. ) ;
#100943 = B_SPLINE_SURFACE_WITH_KNOTS ( 'NONE', 5, 5, ( 
 ( #61595, #53190, #44795, #45352, #103569, #78948, #26870, #61060, #17887 ),
 ( #51521, #36368, #2255, #27971, #77286, #94059, #52086, #584, #85655 ),
 ( #18436, #34711, #68902, #79492, #103003, #52636, #70560, #9509, #104677 ),
 ( #34162, #43676, #25741, #68348, #102454, #77828, #1136, #63265, #22291 ),
 ( #12263, #4438, #47540, #73288, #62725, #4965, #13347, #20114, #46453 ),
 ( #80586, #21742, #3901, #81659, #36919, #97917, #29616, #38030, #2801 ),
 ( #97376, #98473, #63801, #56493, #88973, #38564, #54849, #90622, #64905 ),
 ( #72209, #30720, #55395, #72742, #29081, #39110, #64351, #107424, #3353 ),
 ( #99013, #80032, #71113, #106332, #20647, #13902, #48089, #105801, #89527 ),
 ( #45896, #96847, #21186, #37478, #105237, #28526, #54306, #12817, #88435 ),
 ( #46997, #81120, #106869, #71681, #30160, #55944, #90065, #11726, #101209 ),
 ( #107976, #108533, #49200, #59258, #24505, #109103, #40778, #50307, #93375 ),
 ( #57054, #74954, #82779, #58696, #66011, #58148, #14460, #16642, #31823 ),
 ( #91728, #6072, #92828, #110185, #5528, #100132, #84437, #82227, #39682 ),
 ( #91180, #23952, #73849, #40225, #65457, #66566, #67107, #7721, #75507 ) ),
 .UNSPECIFIED., .F., .F., .F.,
 ( 6, 3, 3, 3, 6 ),
 ( 6, 3, 6 ),
 ( 31.54023800929859789, 39.18581663660000203, 44.09091811200000421, 49.81951809560000299, 53.72098354768269957 ),
 ( 0.000000000000000000, 1.000000000000000000, 2.000085314782729995 ),
 .UNSPECIFIED. ) ;
#100944 = CARTESIAN_POINT ( 'NONE',  ( -107.3285983110000075, 1378.913060287569806, 300.3204975590590493 ) ) ;
#100945 = CARTESIAN_POINT ( 'NONE',  ( 4.324092179320000007, 1515.269353058490196, 208.7600910743320242 ) ) ;
#100946 = DIRECTION ( 'NONE',  ( 0.9510565162951566398, 0.000000000000000000, 0.3090169943749382919 ) ) ;
#100947 = CARTESIAN_POINT ( 'NONE',  ( 3.350944662710000355, 1464.628126271390101, 199.8699733667390035 ) ) ;
#100948 = CARTESIAN_POINT ( 'NONE',  ( -9.994751287005144036, 1380.244992563594224, 201.8194665170140070 ) ) ;
#100949 = CARTESIAN_POINT ( 'NONE',  ( -15.23519492719600166, 1422.125166135662084, 227.7537822221859756 ) ) ;
#100950 = CARTESIAN_POINT ( 'NONE',  ( 10.60846801522230010, 1479.281623091750134, 206.5255074603050218 ) ) ;
#100951 = ORIENTED_EDGE ( 'NONE', *, *, #55761, .T. ) ;
#100952 = B_SPLINE_SURFACE_WITH_KNOTS ( 'NONE', 5, 5, ( 
 ( #23105, #4673, #98170, #5786, #55102, #57311, #81359, #72988, #37723, #98723, #29864, #107683, #97632, #89774, #11973, #38811, #71927, #29316, #82484, #55651, #47232, #107125, #30967, #39927 ),
 ( #14159, #81915, #89226, #56735, #46154, #30417, #5220, #4139, #21984, #63516, #56175, #90871, #99811, #12522, #46700, #22534, #108225, #72448, #65693, #48345, #65143, #80284, #99256, #80830 ),
 ( #90314, #13592, #106039, #20900, #47780, #106578, #64051, #21441, #74096, #39374, #13043, #73549, #67904, #85217, #102559, #40470, #7966, #102013, #68455, #50542, #15251, #25852, #41018, #67355 ),
 ( #152, #66805, #100906, #48903, #100380, #109348, #24741, #91976, #51092, #16344, #8508, #32629, #58390, #75741, #101452, #91437, #24204, #14713, #57848, #49442, #110432, #84121, #83030, #15783 ),
 ( #33711, #92515, #23665, #25296, #59497, #49984, #109885, #33165, #6321, #93070, #93608, #42133, #7420, #41586, #58939, #84667, #42681, #76283, #32072, #16887, #74644, #34274, #108780, #76839 ),
 ( #66263, #83565, #6858, #75197, #71652, #96255, #17441, #28499, #88404, #69011, #45870, #79462, #72716, #60053, #27947, #53736, #105211, #62694, #12794, #9077, #71086, #63772, #695, #46972 ) ),
 .UNSPECIFIED., .F., .F., .F.,
 ( 6, 6 ),
 ( 6, 3, 3, 3, 3, 3, 3, 6 ),
 ( 36.14021738890000535, 99.41336324060000607 ),
 ( 27.66640413320000036, 34.04499835230000571, 36.53903713200000425, 37.78605652179999908, 38.40956621670000004, 39.03307591160000101, 39.72833424150000070, 40.42359257149999507 ),
 .UNSPECIFIED. ) ;
#100953 = CARTESIAN_POINT ( 'NONE',  ( -2.566563053771131475, 1410.380655407001086, 232.6501522581528434 ) ) ;
#100954 = CARTESIAN_POINT ( 'NONE',  ( -9.582919297036148976, 1448.092179236340144, 190.7786095242630040 ) ) ;
#100955 = CARTESIAN_POINT ( 'NONE',  ( -13.59348226018689942, 1508.032052514259931, 209.4636025531580117 ) ) ;
#100956 = CARTESIAN_POINT ( 'NONE',  ( -2.515613294096589847, 1448.349718810959985, 188.5842421507169888 ) ) ;
#100958 = CARTESIAN_POINT ( 'NONE',  ( -15.01814803086499950, 1514.214451716350140, 194.3960746180669901 ) ) ;
#100957 = CARTESIAN_POINT ( 'NONE',  ( -0.4885701619419999808, 1464.413060387330006, 229.7716327975979880 ) ) ;
#100959 = CARTESIAN_POINT ( 'NONE',  ( 17.26794000855596423, 1525.730671215505254, 236.6572858183501751 ) ) ;
#100960 = CARTESIAN_POINT ( 'NONE',  ( -119.3423021147300034, 1306.483669372790018, 300.9755515165790030 ) ) ;
#100961 = CARTESIAN_POINT ( 'NONE',  ( -13.78858225216500166, 1513.492015765619954, 222.2033214031669957 ) ) ;
#100962 = CARTESIAN_POINT ( 'NONE',  ( -1.011208509896629915, 1420.774206283469766, 183.0065381184390105 ) ) ;
#100963 = CARTESIAN_POINT ( 'NONE',  ( -2.487103457664999961, 1516.577434278289957, 202.5755431900869894 ) ) ;
#100964 = CARTESIAN_POINT ( 'NONE',  ( -0.01912654351157340102, 1347.931987472819856, 209.1220808601199792 ) ) ;
#100965 = CARTESIAN_POINT ( 'NONE',  ( -13.58235846979999906, 1416.828040475229955, 221.9087530951979659 ) ) ;
#100966 = CARTESIAN_POINT ( 'NONE',  ( 16.44145556193499758, 1512.902436350919970, 197.5299575732669837 ) ) ;
#100967 = CARTESIAN_POINT ( 'NONE',  ( -17.11220264658090073, 1420.169995509359978, 204.6828454769579935 ) ) ;
#100968 = CARTESIAN_POINT ( 'NONE',  ( -11.19604652080000129, 1377.051618906870090, 211.6852637316389973 ) ) ;
#100969 = EDGE_CURVE ( 'NONE', #81049, #104688, #51560, .T. ) ;
#100970 = CARTESIAN_POINT ( 'NONE',  ( 19.89292065997459957, 1508.347995227200045, 229.2234713626579889 ) ) ;
#100972 = ORIENTED_EDGE ( 'NONE', *, *, #27175, .F. ) ;
#100971 = CARTESIAN_POINT ( 'NONE',  ( -54.35795438361589760, 1379.711943094660000, 254.1192448666850225 ) ) ;
#100973 = VERTEX_POINT ( 'NONE', #94053 ) ;
#100974 = CARTESIAN_POINT ( 'NONE',  ( 11.63825043920830105, 1433.980580709160222, 151.1735222970980033 ) ) ;
#100975 = CARTESIAN_POINT ( 'NONE',  ( -12.50012693489999904, 1397.670467479229956, 212.9149460363679793 ) ) ;
#100976 = ORIENTED_EDGE ( 'NONE', *, *, #100921, .F. ) ;
#100977 = CARTESIAN_POINT ( 'NONE',  ( -105.3882398639999991, 1379.160164679609807, 305.8019944446589875 ) ) ;
#100978 = CIRCLE ( 'NONE', #2713, 15.40132948099999943 ) ;
#100979 = DIRECTION ( 'NONE',  ( -0.6638413695745983834, -0.7475172490850811036, -0.02307809267670082876 ) ) ;
#100980 = CARTESIAN_POINT ( 'NONE',  ( 4.261662193653270592, 1515.372228416479857, 206.7919396051269985 ) ) ;
#100983 = EDGE_CURVE ( 'NONE', #22899, #15596, #10394, .T. ) ;
#100982 = CARTESIAN_POINT ( 'NONE',  ( -13.83792090743880010, 1508.660897340560041, 183.9592593128280100 ) ) ;
#100981 = CARTESIAN_POINT ( 'NONE',  ( 2.544801979510000312, 1445.822494309589956, 199.7339677725889828 ) ) ;
#100984 = CARTESIAN_POINT ( 'NONE',  ( 6.918006061659999872, 1449.231408575739806, 185.2825139585980025 ) ) ;
#100985 = CARTESIAN_POINT ( 'NONE',  ( -3.858501607638550102, 1463.264545322189861, 200.1250934300819893 ) ) ;
#100986 = CARTESIAN_POINT ( 'NONE',  ( -20.20959865099451847, 1512.187213306747481, 236.2316688286741453 ) ) ;
#100987 =( NAMED_UNIT ( * ) SI_UNIT ( $, .STERADIAN. ) SOLID_ANGLE_UNIT ( ) );
#100988 = CARTESIAN_POINT ( 'NONE',  ( 5.047496844141320160, 1396.089322873039919, 199.3124458601029971 ) ) ;
#100989 = CARTESIAN_POINT ( 'NONE',  ( 1.061258286910000015, 1415.553739807329976, 190.7107924731980120 ) ) ;
#100990 = CARTESIAN_POINT ( 'NONE',  ( 11.56455571449999908, 1431.422381474849999, 151.1349765661979916 ) ) ;
#100991 = CARTESIAN_POINT ( 'NONE',  ( 8.473068888075001581, 1511.778199792620171, 203.0330132217169989 ) ) ;
#100992 = EDGE_LOOP ( 'NONE', ( #95922, #51748, #67971, #55943, #110392, #21120, #14841, #7888, #43850, #95004, #6017, #45488, #82709, #89562, #28333, #84452, #59126, #48335, #55654, #4227, #80496, #57103, #96915, #54297, #10003, #28996 ) ) ;
#100993 = CARTESIAN_POINT ( 'NONE',  ( 12.89178610096769972, 1435.806136340959938, 150.7524150612520089 ) ) ;
#100994 = ORIENTED_EDGE ( 'NONE', *, *, #5122, .F. ) ;
#100995 = ORIENTED_EDGE ( 'NONE', *, *, #55740, .F. ) ;
#100996 = CARTESIAN_POINT ( 'NONE',  ( 13.35361680572849075, 1444.505398037199257, 169.3732864882159106 ) ) ;
#100997 = CARTESIAN_POINT ( 'NONE',  ( -8.485858099410000577, 1465.307528046030257, 233.0823719839980015 ) ) ;
#100998 = CARTESIAN_POINT ( 'NONE',  ( -109.5436877675987688, 1386.781868541095491, 311.1752058669367216 ) ) ;
#100999 = CARTESIAN_POINT ( 'NONE',  ( -2.483949978725000118, 1517.156142772249950, 216.0726795003369887 ) ) ;
#101000 = CARTESIAN_POINT ( 'NONE',  ( -8.480656650225677495, 1511.395875706868765, 213.9949865275974616 ) ) ;
#101001 = ORIENTED_EDGE ( 'NONE', *, *, #54775, .F. ) ;
#101002 = CARTESIAN_POINT ( 'NONE',  ( -12.66333039259999893, 1503.375086606289869, 208.6466812236969872 ) ) ;
#101003 = CARTESIAN_POINT ( 'NONE',  ( 0.4151546846821903003, 1501.977400791986611, 173.3106345060153046 ) ) ;
#101004 = LINE ( 'NONE', #51177, #76070 ) ;
#101005 = VERTEX_POINT ( 'NONE', #60484 ) ;
#101006 = CARTESIAN_POINT ( 'NONE',  ( 3.446942071715000111, 1516.842852731759876, 205.8545543269370057 ) ) ;
#101007 = ORIENTED_EDGE ( 'NONE', *, *, #55721, .F. ) ;
#101008 = CARTESIAN_POINT ( 'NONE',  ( 0.7468175155120010400, 1517.006509894990131, 209.1147170949500094 ) ) ;
#101009 = CARTESIAN_POINT ( 'NONE',  ( -8.754256066850169660, 1451.698950522699988, 206.0561735730059922 ) ) ;
#101010 = CARTESIAN_POINT ( 'NONE',  ( -2.935740633370000019, 1409.954265578529885, 186.6342734662979979 ) ) ;
#101011 = DIRECTION ( 'NONE',  ( 0.8672669759446595128, 0.000000000000000000, -0.4978433412588795237 ) ) ;
#101013 = VERTEX_POINT ( 'NONE', #23 ) ;
#101012 = CARTESIAN_POINT ( 'NONE',  ( 0.2223009155142280091, 1416.826860677879949, 227.1890218400880030 ) ) ;
#101014 = CARTESIAN_POINT ( 'NONE',  ( 22.45965404249999864, 1431.566040525590097, 217.4494758438079884 ) ) ;
#101015 = CARTESIAN_POINT ( 'NONE',  ( -14.77864689549059918, 1508.551704408389924, 210.3595489859820020 ) ) ;
#101016 = AXIS2_PLACEMENT_3D ( 'NONE', #11250, #36977, #44300 ) ;
#101017 = CARTESIAN_POINT ( 'NONE',  ( -62.22036486049999837, 1383.793512663130059, 284.6761640327590044 ) ) ;
#101018 = CARTESIAN_POINT ( 'NONE',  ( 0.000000000000000000, 1512.187213306747481, 209.1218459616979999 ) ) ;
#101019 = CARTESIAN_POINT ( 'NONE',  ( 10.46129002499089999, 1411.316052440500243, 269.3482828489609915 ) ) ;
#101020 = CIRCLE ( 'NONE', #33086, 2.000000000000000444 ) ;
#101021 = CARTESIAN_POINT ( 'NONE',  ( -3.449149233875000053, 1516.947419719950176, 213.7456339395970133 ) ) ;
#101022 = CARTESIAN_POINT ( 'NONE',  ( 24.07543316050000115, 1410.713981489629987, 209.3273838987269926 ) ) ;
#101023 = CARTESIAN_POINT ( 'NONE',  ( -22.01123596709999930, 1509.713525028729919, 189.1765381185980175 ) ) ;
#101024 = CARTESIAN_POINT ( 'NONE',  ( 12.29645462760879937, 1492.351698860680017, 210.2246036700939840 ) ) ;
#101025 = CARTESIAN_POINT ( 'NONE',  ( 5.513199787613100256, 1509.038617475950105, 216.6345962046710270 ) ) ;
#101026 = CARTESIAN_POINT ( 'NONE',  ( 2.882325979385000014, 1516.969638403840008, 210.8235757905769674 ) ) ;
#101027 = LINE ( 'NONE', #66372, #68848 ) ;
#101028 = CARTESIAN_POINT ( 'NONE',  ( 0.1681681976620000019, 1420.473120457930008, 182.7464973445979979 ) ) ;
#101029 = CARTESIAN_POINT ( 'NONE',  ( 10.97658109374170010, 1432.766920830290019, 151.7697937633350023 ) ) ;
#101031 = ORIENTED_EDGE ( 'NONE', *, *, #37375, .F. ) ;
#101030 = CARTESIAN_POINT ( 'NONE',  ( -48.48855173430000320, 1388.337145087740055, 255.7627372621590212 ) ) ;
#101032 = CARTESIAN_POINT ( 'NONE',  ( -39.61210671423299345, 1385.184201439789831, 241.4309191739689879 ) ) ;
#101033 = B_SPLINE_SURFACE_WITH_KNOTS ( 'NONE', 5, 5, ( 
 ( #73397, #63910, #56042, #98024, #56595, #99117 ),
 ( #55503, #5072, #30824, #11834, #96952, #89630 ),
 ( #47097, #108079, #4539, #64999, #73948, #64462 ),
 ( #22395, #38129, #20218, #38673, #72848, #14012 ),
 ( #30270, #54417, #98579, #5639, #80136, #37583 ),
 ( #4003, #71786, #105905, #63375, #97491, #20759 ),
 ( #89084, #12371, #46557, #94438, #78208, #35101 ),
 ( #51351, #69283, #76551, #57165, #82883, #103388 ),
 ( #50807, #16610, #68190, #26694, #102837, #110706 ) ),
 .UNSPECIFIED., .F., .F., .F.,
 ( 6, 3, 6 ),
 ( 6, 6 ),
 ( 13.54778530316779950, 23.82275646639999778, 33.29595707573220409 ),
 ( -1.147433219344110065E-05, 2.000000000000000000 ),
 .UNSPECIFIED. ) ;
#101034 = CARTESIAN_POINT ( 'NONE',  ( 41.56056514950000036, 1440.913060317639975, 261.5690365818979330 ) ) ;
#101035 = CARTESIAN_POINT ( 'NONE',  ( -3.737177908446197794, 1370.322789966642176, 210.0021808679227888 ) ) ;
#101036 = CARTESIAN_POINT ( 'NONE',  ( 1.253776719794245986, 1494.066817944285049, 220.1788260179384054 ) ) ;
#101037 = CARTESIAN_POINT ( 'NONE',  ( -5.402311893739999427, 1434.355786020779988, 154.6519262295979900 ) ) ;
#101038 = LINE ( 'NONE', #57970, #103795 ) ;
#101039 = CARTESIAN_POINT ( 'NONE',  ( 17.71193101166619854, 1522.051704408389924, 196.6727161458730109 ) ) ;
#101041 = CARTESIAN_POINT ( 'NONE',  ( -8.023097652669999746, 1384.898239823859967, 218.7875342523390145 ) ) ;
#101040 = DIRECTION ( 'NONE',  ( 0.000000000000000000, 0.000000000000000000, 1.000000000000000000 ) ) ;
#101042 = CARTESIAN_POINT ( 'NONE',  ( 17.17241001986506177, 1523.382868172864164, 238.6251415217915053 ) ) ;
#101043 = CARTESIAN_POINT ( 'NONE',  ( 31.02592223166964658, 1526.278758871496620, 219.9652544506485015 ) ) ;
#101044 = EDGE_LOOP ( 'NONE', ( #24312, #41506 ) ) ;
#101045 = CARTESIAN_POINT ( 'NONE',  ( -1.710004586925000236, 1516.557392317769882, 202.5758445815369839 ) ) ;
#101046 = CARTESIAN_POINT ( 'NONE',  ( -0.2682674118730000723, 1457.813445294729945, 229.2631846297979905 ) ) ;
#101047 = CIRCLE ( 'NONE', #18801, 2.500000000000002220 ) ;
#101048 = CARTESIAN_POINT ( 'NONE',  ( 23.03439503529999755, 1449.683642696550123, 219.5641606253980171 ) ) ;
#101049 = CARTESIAN_POINT ( 'NONE',  ( 7.957394096424367902, 1438.145637585891109, 153.7040555654163256 ) ) ;
#101050 = CARTESIAN_POINT ( 'NONE',  ( -6.086798803919999834, 1421.074767261429997, 186.7378509026979998 ) ) ;
#101051 =( BOUNDED_SURFACE ( )  B_SPLINE_SURFACE ( 3, 2, ( 
 ( #28788, #54570, #13604 ),
 ( #20911, #29874, #97098 ),
 ( #37736, #65154, #63527 ),
 ( #64615, #107694, #88153 ),
 ( #21995, #54024, #99267 ),
 ( #62987, #106588, #11441 ),
 ( #37191, #38275, #30428 ),
 ( #47241, #71937, #106049 ),
 ( #13055, #90325, #55116 ),
 ( #30979, #98734, #105497 ),
 ( #45615, #98181, #79756 ),
 ( #3062, #81369, #21451 ) ),
 .UNSPECIFIED., .F., .F., .T. ) 
 B_SPLINE_SURFACE_WITH_KNOTS ( ( 4, 2, 2, 2, 2, 4 ),
 ( 3, 3 ),
 ( 0.000000000000000000, 0.001069428368779032790, 0.001604142553168549186, 0.002138856737558065581, 0.003208285106337098371, 0.004277713475116131162 ),
 ( 0.000000000000000000, 1.000000000000000000 ),
 .UNSPECIFIED. ) 
 GEOMETRIC_REPRESENTATION_ITEM ( )  RATIONAL_B_SPLINE_SURFACE ( (
 ( 1.000000000000000000, 0.7071067811866051933, 1.000000000000000000),
 ( 1.000000000000000000, 0.7227579664598644538, 1.000000000000000000),
 ( 1.000000000000000000, 0.7381056972207281630, 1.000000000000000000),
 ( 1.000000000000000000, 0.7607155509935809024, 1.000000000000000000),
 ( 1.000000000000000000, 0.7681829160207560570, 1.000000000000000000),
 ( 1.000000000000000000, 0.7829721389379027396, 1.000000000000000000),
 ( 1.000000000000000000, 0.7902925692255797774, 1.000000000000000000),
 ( 1.000000000000000000, 0.8113688493901506371, 1.000000000000000000),
 ( 1.000000000000000000, 0.8244846461023084272, 1.000000000000000000),
 ( 1.000000000000000000, 0.8485067901407726820, 1.000000000000000000),
 ( 1.000000000000000000, 0.8591713199357238206, 1.000000000000000000),
 ( 1.000000000000000000, 0.8676405061997034540, 1.000000000000000000) ) ) 
 REPRESENTATION_ITEM ( '' )  SURFACE ( )  );
#101052 = FACE_OUTER_BOUND ( 'NONE', #34366, .T. ) ;
#101053 = CARTESIAN_POINT ( 'NONE',  ( 4.053537042790000378, 1441.572390738320109, 183.3424090224980034 ) ) ;
#101054 = CARTESIAN_POINT ( 'NONE',  ( 27.32002834875690311, 1436.780620296950019, 136.7657361291360019 ) ) ;
#101055 = CARTESIAN_POINT ( 'NONE',  ( 39.06740725280500470, 1447.641448397309887, 136.5466146009009947 ) ) ;
#101056 = CARTESIAN_POINT ( 'NONE',  ( -23.42261135620000090, 1434.595605500659985, 214.6024269201780044 ) ) ;
#101057 = CARTESIAN_POINT ( 'NONE',  ( -36.06148001838602113, 1461.985359838420209, 269.2267996494942395 ) ) ;
#101058 = CARTESIAN_POINT ( 'NONE',  ( -107.9217616539999938, 1387.054747972530095, 297.7113990731589865 ) ) ;
#101059 = EDGE_CURVE ( 'NONE', #47770, #71731, #110309, .T. ) ;
#101060 = CARTESIAN_POINT ( 'NONE',  ( -17.59370741740000099, 1418.348682474430007, 226.0262961122979846 ) ) ;
#101061 = CARTESIAN_POINT ( 'NONE',  ( 4.190103204352849886, 1507.220947887740067, 220.0490538541789931 ) ) ;
#101062 = TOROIDAL_SURFACE ( 'NONE', #74252, 1.000000000000000000, 1.000000000000000000 ) ;
#101063 = CARTESIAN_POINT ( 'NONE',  ( -5.510509099684978374, 1471.237799169209666, 269.3375995838932226 ) ) ;
#101064 = ORIENTED_EDGE ( 'NONE', *, *, #22830, .F. ) ;
#101065 = CARTESIAN_POINT ( 'NONE',  ( -8.355888189921600429, 1440.379141069660136, 205.2277604852559705 ) ) ;
#101066 = CARTESIAN_POINT ( 'NONE',  ( -32.06316538499910251, 1416.592306352786409, 269.3144317999657460 ) ) ;
#101067 = CARTESIAN_POINT ( 'NONE',  ( 14.80452861058799918, 1440.352436769449923, 190.1999221398900204 ) ) ;
#101068 = CARTESIAN_POINT ( 'NONE',  ( -14.86238962927253837, 1451.964376860417815, 222.9824286697244418 ) ) ;
#101069 = CARTESIAN_POINT ( 'NONE',  ( 16.16632277704800558, 1512.187213306747481, 236.8966194768523508 ) ) ;
#101070 = B_SPLINE_SURFACE_WITH_KNOTS ( 'NONE', 5, 5, ( 
 ( #66231, #74615, #40439, #40989, #108195, #48873 ),
 ( #109318, #6829, #49411, #108750, #32601, #32042 ),
 ( #23638, #56705, #22504, #75168, #81886, #90841 ),
 ( #100877, #23073, #64577, #24170, #58359, #92484 ),
 ( #90285, #82999, #65664, #15754, #49955, #99781 ),
 ( #98696, #13566, #21955, #5189, #14126, #48316 ),
 ( #82457, #76252, #94699, #8477, #110400, #25270 ),
 ( #121, #95260, #93040, #42651, #35349, #1214 ),
 ( #60579, #68428, #16314, #76805, #50515, #77908 ) ),
 .UNSPECIFIED., .F., .F., .F.,
 ( 6, 3, 6 ),
 ( 6, 6 ),
 ( 3.019990725210560001, 5.187276425779999478, 7.354562126349439843 ),
 ( -0.0004187671794352290015, 2.000000000000000000 ),
 .UNSPECIFIED. ) ;
#101071 = CARTESIAN_POINT ( 'NONE',  ( -3.644351594698530317, 1515.551704204689941, 212.3939699354600066 ) ) ;
#101072 = CARTESIAN_POINT ( 'NONE',  ( 0.000000000000000000, 1412.913060387329779, 209.1218459616979999 ) ) ;
#101074 = ADVANCED_FACE ( 'NONE', ( #24618 ), #24080, .T. ) ;
#101073 = CARTESIAN_POINT ( 'NONE',  ( -38.58235177178170261, 1444.329162691080228, 137.1361782391459769 ) ) ;
#101075 = CARTESIAN_POINT ( 'NONE',  ( 25.34079329589999929, 1436.168901596849992, 137.1732139229980021 ) ) ;
#101076 = CARTESIAN_POINT ( 'NONE',  ( -13.11972090476676733, 1443.041373250473725, 169.4030072996578724 ) ) ;
#101078 = VERTEX_POINT ( 'NONE', #16226 ) ;
#101077 = CARTESIAN_POINT ( 'NONE',  ( -13.61519277519999882, 1409.388513392130108, 226.0716413619979903 ) ) ;
#101079 = CARTESIAN_POINT ( 'NONE',  ( 0.08760820899984020360, 1414.971390223319986, 192.4206628386800162 ) ) ;
#101080 = DIRECTION ( 'NONE',  ( -1.040834085586083310E-14, 0.000000000000000000, 1.000000000000000000 ) ) ;
#101081 = ADVANCED_FACE ( 'NONE', ( #17321 ), #67391, .T. ) ;
#101082 = EDGE_LOOP ( 'NONE', ( #93393, #13213, #110125, #46269, #51253 ) ) ;
#101083 = VERTEX_POINT ( 'NONE', #26294 ) ;
#101084 = CARTESIAN_POINT ( 'NONE',  ( -12.33321116790000005, 1502.561054230289983, 208.9929969191140060 ) ) ;
#101085 = CARTESIAN_POINT ( 'NONE',  ( -20.28160989816897697, 1526.000688113710567, 233.4099348502813314 ) ) ;
#101087 = CARTESIAN_POINT ( 'NONE',  ( -11.53898582669999939, 1459.427238891729985, 220.7971265779980286 ) ) ;
#101086 = CARTESIAN_POINT ( 'NONE',  ( 41.25815740437244017, 1435.010063311743352, 269.6334395952857221 ) ) ;
#101088 = CARTESIAN_POINT ( 'NONE',  ( -6.429626910120000538, 1446.645710171090059, 215.7201002026189940 ) ) ;
#101089 = CARTESIAN_POINT ( 'NONE',  ( -11.17066468859999873, 1433.159422583310061, 151.6197124790980126 ) ) ;
#101090 = CARTESIAN_POINT ( 'NONE',  ( -17.05170201009999786, 1380.306507143900035, 210.4183098381890034 ) ) ;
#101091 = CARTESIAN_POINT ( 'NONE',  ( 9.363526459378379130, 1464.473567072740025, 212.1249062944089872 ) ) ;
#101092 = CARTESIAN_POINT ( 'NONE',  ( -114.5985638465105154, 1306.413060387289988, 306.4158023619849018 ) ) ;
#101093 = CARTESIAN_POINT ( 'NONE',  ( -12.37159932449999822, 1415.628674266529742, 195.6623782650979990 ) ) ;
#101094 = FACE_BOUND ( 'NONE', #6617, .T. ) ;
#101095 = CARTESIAN_POINT ( 'NONE',  ( -2.883410015801580073, 1409.181736952820074, 187.1726418057029946 ) ) ;
#101096 = CARTESIAN_POINT ( 'NONE',  ( 7.383230514405129341, 1364.047475561790179, 208.3718459617061285 ) ) ;
#101097 = CARTESIAN_POINT ( 'NONE',  ( -27.60455267767378729, 1509.989042806181033, 197.3747958975489212 ) ) ;
#101099 = EDGE_LOOP ( 'NONE', ( #24344, #23584 ) ) ;
#101098 = CARTESIAN_POINT ( 'NONE',  ( -1.558958650196000183E-09, 1416.365570055059834, 239.4563497976100166 ) ) ;
#101100 = VERTEX_POINT ( 'NONE', #8389 ) ;
#101101 = CARTESIAN_POINT ( 'NONE',  ( -11.76590084519579982, 1427.017745790240042, 146.1561352580970095 ) ) ;
#101102 = CARTESIAN_POINT ( 'NONE',  ( 24.04366839390669952, 1494.655600297209958, 207.1743948306419725 ) ) ;
#101103 = CARTESIAN_POINT ( 'NONE',  ( -5.151088789370000143, 1471.205953851929962, 269.3380511851980259 ) ) ;
#101104 = CARTESIAN_POINT ( 'NONE',  ( -2.080714710711137450, 1474.229611947080684, 219.1688284120783692 ) ) ;
#101106 = ADVANCED_FACE ( 'NONE', ( #94604 ), #8621, .T. ) ;
#101105 = CARTESIAN_POINT ( 'NONE',  ( -113.4000000000000057, 1348.229899472569969, 310.4276940313059754 ) ) ;
#101107 = CARTESIAN_POINT ( 'NONE',  ( 38.00281594157139864, 1449.406348292719940, 136.2793115458389934 ) ) ;
#101108 = CARTESIAN_POINT ( 'NONE',  ( 16.75801468479999912, 1408.913060387329779, 202.5679462747779667 ) ) ;
#101109 = CARTESIAN_POINT ( 'NONE',  ( -9.092690131330000369, 1384.838170029980120, 199.9433835858289967 ) ) ;
#101110 = B_SPLINE_SURFACE_WITH_KNOTS ( 'NONE', 5, 5, ( 
 ( #20958, #90369, #46762, #90931, #12580, #3661, #47837, #98228, #97139 ),
 ( #31023, #105551, #37790, #107185, #63569, #22591, #106628, #54614, #28838 ),
 ( #64663, #81970, #30475, #29917, #55162, #97685, #13104, #5278, #80891 ),
 ( #21498, #71978, #55711, #65204, #81410, #14218, #47287, #4722, #98780 ),
 ( #22043, #56240, #39433, #73609, #56794, #32136, #33230, #59556, #24805 ),
 ( #93137, #67419, #74708, #23722, #91495, #76348, #109410, #83631, #7483 ),
 ( #48960, #32686, #58452, #108289, #14774, #39982, #100975, #93670, #6927 ),
 ( #108839, #102081, #41084, #75261, #57907, #31575, #83091, #65752, #15313 ),
 ( #59010, #16405, #92041, #33777, #84184, #57368, #6384, #40532, #41644 ),
 ( #66321, #66867, #109951, #110497, #82548, #75800, #100439, #67973, #74158 ),
 ( #99869, #50599, #49506, #23168, #24271, #84731, #92579, #15851, #50056 ),
 ( #101518, #48404, #8028, #5842, #42197, #25364, #95358, #87519, #69077 ) ),
 .UNSPECIFIED., .F., .F., .F.,
 ( 6, 3, 3, 6 ),
 ( 6, 3, 6 ),
 ( 12.74698783810000080, 30.29491413010000045, 39.81482060289999936, 57.85069212530000016 ),
 ( 0.000000000000000000, 1.000000000000000000, 2.000000000000000000 ),
 .UNSPECIFIED. ) ;
#101111 = CARTESIAN_POINT ( 'NONE',  ( 10.01496071350510064, 1468.907470368469831, 208.6044946494789940 ) ) ;
#101112 = DIRECTION ( 'NONE',  ( -0.3522034561021770704, -0.9359206307609502229, -0.002301830946695800680 ) ) ;
#101113 = CARTESIAN_POINT ( 'NONE',  ( 11.64244948864622664, 1363.185827771890899, 209.6218459617033432 ) ) ;
#101114 = CARTESIAN_POINT ( 'NONE',  ( -9.471334638087320457, 1448.015926047950188, 210.3227975281659781 ) ) ;
#101115 = CARTESIAN_POINT ( 'NONE',  ( -10.60590658980659917, 1406.964585531180091, 269.0015838391640273 ) ) ;
#101116 = CARTESIAN_POINT ( 'NONE',  ( -13.40001318606720027, 1436.143823819350018, 150.5590804106440146 ) ) ;
#101117 = VERTEX_POINT ( 'NONE', #85100 ) ;
#101118 = CARTESIAN_POINT ( 'NONE',  ( -4.329448791022380227, 1515.064792310580060, 210.8975365261770207 ) ) ;
#101119 = EDGE_LOOP ( 'NONE', ( #79350, #54227, #96351, #96573 ) ) ;
#101120 = ORIENTED_EDGE ( 'NONE', *, *, #87057, .T. ) ;
#101121 = CARTESIAN_POINT ( 'NONE',  ( 5.009343724018470390, 1422.720564319518871, 184.4316651301672891 ) ) ;
#101122 = CARTESIAN_POINT ( 'NONE',  ( 9.117609068447830367, 1425.283679751730006, 195.1398618588590068 ) ) ;
#101124 = DIRECTION ( 'NONE',  ( -1.000000000000000000, 0.000000000000000000, 0.000000000000000000 ) ) ;
#101123 = CARTESIAN_POINT ( 'NONE',  ( -2.865911554774999814, 1516.906233342200039, 212.5838411289170153 ) ) ;
#101125 = CARTESIAN_POINT ( 'NONE',  ( 7.495834450094876367, 1517.015741767610280, 209.4130272268053261 ) ) ;
#101126 = B_SPLINE_CURVE_WITH_KNOTS ( 'NONE', 5,
 ( #43764, #51068, #17983, #52179, #77371, #7943, #8485, #86310, #94707, #26392, #76259, #33688 ),
 .UNSPECIFIED., .F., .F.,
 ( 6, 3, 3, 6 ),
 ( -25.27124713539999945, -25.02147540209999832, -24.77170366879999719, -21.89878894926970077 ),
 .UNSPECIFIED. ) ;
#101127 = CARTESIAN_POINT ( 'NONE',  ( 2.502366908949907653, 1409.000444965305178, 224.1100396174575167 ) ) ;
#101128 = ORIENTED_EDGE ( 'NONE', *, *, #35804, .T. ) ;
#101129 = DIRECTION ( 'NONE',  ( -0.9125304618754024322, 0.000000000000000000, -0.4090087482554191078 ) ) ;
#101130 = CIRCLE ( 'NONE', #88700, 6.646318662569999702 ) ;
#101131 = CARTESIAN_POINT ( 'NONE',  ( -0.01126495432349849946, 1516.939530130779985, 202.1773791897269916 ) ) ;
#101132 = CARTESIAN_POINT ( 'NONE',  ( -4.319145873661043744, 1421.270721947785205, 186.1375689364567165 ) ) ;
#101134 = AXIS2_PLACEMENT_3D ( 'NONE', #34088, #68281, #51447 ) ;
#101133 = CARTESIAN_POINT ( 'NONE',  ( -49.07695366983040230, 1384.615622046050248, 223.8752598800379872 ) ) ;
#101135 = CARTESIAN_POINT ( 'NONE',  ( -5.091556393439999439, 1407.116996366430158, 197.0899548111979698 ) ) ;
#101136 = DIRECTION ( 'NONE',  ( -0.000000000000000000, -1.000000000000000000, -0.000000000000000000 ) ) ;
#101138 = ORIENTED_EDGE ( 'NONE', *, *, #60651, .T. ) ;
#101137 = CARTESIAN_POINT ( 'NONE',  ( -38.10537780832459731, 1442.926987427690165, 137.1117395883960057 ) ) ;
#101139 = CARTESIAN_POINT ( 'NONE',  ( -24.05132347639830215, 1411.090389413789808, 209.8326646502659969 ) ) ;
#101140 = CARTESIAN_POINT ( 'NONE',  ( 28.13115138590000086, 1508.134099165530188, 210.1250122821180071 ) ) ;
#101141 = CARTESIAN_POINT ( 'NONE',  ( 3.761652188060691682, 1425.538669997582474, 185.2058339228567263 ) ) ;
#101142 = CARTESIAN_POINT ( 'NONE',  ( -12.00444414999999942, 1381.312822588570043, 202.5161199644090289 ) ) ;
#101143 = CARTESIAN_POINT ( 'NONE',  ( -24.52144259279999972, 1435.632488953809798, 137.5271284461979917 ) ) ;
#101144 = B_SPLINE_CURVE_WITH_KNOTS ( 'NONE', 3,
 ( #101447, #67900, #42676, #18550 ),
 .UNSPECIFIED., .F., .F.,
 ( 4, 4 ),
 ( 0.000000000000000000, 1.000000000000000000 ),
 .UNSPECIFIED. ) ;
#101145 = CARTESIAN_POINT ( 'NONE',  ( -24.49688161579999957, 1441.286190042660110, 211.0056646591280014 ) ) ;
#101146 = CARTESIAN_POINT ( 'NONE',  ( 1.717432448265000078, 1516.836638729160086, 211.4041475482669910 ) ) ;
#101147 = CARTESIAN_POINT ( 'NONE',  ( 9.722207004026980570, 1428.114070666289763, 212.2005352792010058 ) ) ;
#101148 = FACE_OUTER_BOUND ( 'NONE', #62820, .T. ) ;
#101149 = CARTESIAN_POINT ( 'NONE',  ( 5.994585642347090904, 1439.856461454209921, 216.6194481787469783 ) ) ;
#101150 = DIRECTION ( 'NONE',  ( 7.205227288424627209E-20, 0.9876883405951701889, 0.1564344650400262826 ) ) ;
#101151 = CARTESIAN_POINT ( 'NONE',  ( -1.717432486395000124, 1516.836638729160086, 206.8395443540670158 ) ) ;
#101152 = ORIENTED_EDGE ( 'NONE', *, *, #16459, .T. ) ;
#101153 = DIRECTION ( 'NONE',  ( 0.000000000000000000, 1.000000000000000000, 0.000000000000000000 ) ) ;
#101154 = CARTESIAN_POINT ( 'NONE',  ( -9.534250030377648955, 1439.230267954009832, 208.6524524575060013 ) ) ;
#101155 = CARTESIAN_POINT ( 'NONE',  ( -20.89050673521863999, 1455.005279222091303, 223.4623653643373302 ) ) ;
#101156 = VERTEX_POINT ( 'NONE', #52078 ) ;
#101157 = CARTESIAN_POINT ( 'NONE',  ( -17.84338787571901364, 1523.382868172864164, 237.8836641337663309 ) ) ;
#101158 = CARTESIAN_POINT ( 'NONE',  ( 12.93087728801789993, 1434.999496278460128, 150.1242520500200044 ) ) ;
#101159 = CARTESIAN_POINT ( 'NONE',  ( 17.51310050168130061, 1459.308345724359924, 228.3567006344079857 ) ) ;
#101160 = CARTESIAN_POINT ( 'NONE',  ( -4.317409491140000277, 1412.932174402340024, 207.9150182743289861 ) ) ;
#101161 = CARTESIAN_POINT ( 'NONE',  ( 27.01382310970000233, 1451.969724731730139, 134.9184576876980088 ) ) ;
#101162 = CARTESIAN_POINT ( 'NONE',  ( 4.851218532629999913, 1487.503864385689894, 198.5929753848990060 ) ) ;
#101163 = CARTESIAN_POINT ( 'NONE',  ( 2.924955189797899813, 1430.826773540479962, 218.1505144264980061 ) ) ;
#101164 = CARTESIAN_POINT ( 'NONE',  ( -15.10324083849999965, 1409.440477179229902, 225.7327363557979822 ) ) ;
#101166 = CARTESIAN_POINT ( 'NONE',  ( -0.1681681984989999989, 1413.717199569329750, 164.8680577770979880 ) ) ;
#101165 = CARTESIAN_POINT ( 'NONE',  ( -2.287084308194999860, 1517.068517094990057, 214.1351209316169957 ) ) ;
#101167 = CARTESIAN_POINT ( 'NONE',  ( -8.883094036332620291, 1385.283542038099995, 218.6640794153470040 ) ) ;
#101168 = CARTESIAN_POINT ( 'NONE',  ( 3.455377977254999955, 1516.627618683580067, 216.0573038954169931 ) ) ;
#101169 = VERTEX_POINT ( 'NONE', #86210 ) ;
#101170 = CARTESIAN_POINT ( 'NONE',  ( -11.40293847520729997, 1414.971993471380074, 196.2990445993690116 ) ) ;
#101171 = CARTESIAN_POINT ( 'NONE',  ( -16.68788013329999842, 1420.510568510920166, 203.3707636713990041 ) ) ;
#101172 = CARTESIAN_POINT ( 'NONE',  ( 2.235819005889999822, 1419.966584392630011, 185.0820763846980128 ) ) ;
#101173 = AXIS2_PLACEMENT_3D ( 'NONE', #92208, #108463, #66492 ) ;
#101174 = AXIS2_PLACEMENT_3D ( 'NONE', #14946, #58637, #92770 ) ;
#101175 = CARTESIAN_POINT ( 'NONE',  ( 0.05161184595879859949, 1475.303443633190000, 220.5712324161989955 ) ) ;
#101176 = CARTESIAN_POINT ( 'NONE',  ( -104.3950658971828460, 1390.067543051406574, 304.1809742105791088 ) ) ;
#101177 = CARTESIAN_POINT ( 'NONE',  ( -21.50400446119279962, 1505.467562055609960, 209.6175409707290100 ) ) ;
#101178 = CARTESIAN_POINT ( 'NONE',  ( -11.23655883251920073, 1471.270429263729966, 207.1105222724550003 ) ) ;
#101179 = CARTESIAN_POINT ( 'NONE',  ( -5.195342543991931628, 1508.245210224850780, 220.3666772047745610 ) ) ;
#101180 = CARTESIAN_POINT ( 'NONE',  ( 17.20238589132565821, 1422.398122266642531, 226.7110313106093145 ) ) ;
#101181 = CARTESIAN_POINT ( 'NONE',  ( 18.59509526533679136, 1425.782355783442199, 224.9721248484763692 ) ) ;
#101182 = CARTESIAN_POINT ( 'NONE',  ( -9.603657968282620217E-07, 1408.141559225309948, 222.5225557192960082 ) ) ;
#101183 = LINE ( 'NONE', #93895, #52700 ) ;
#101185 = CARTESIAN_POINT ( 'NONE',  ( -1.376928043298436100, 1517.151704408390060, 226.4861182474958525 ) ) ;
#101184 = CARTESIAN_POINT ( 'NONE',  ( -14.24607374332530085, 1416.872377924300054, 203.2551249638830200 ) ) ;
#101186 = CARTESIAN_POINT ( 'NONE',  ( 13.00108844889999915, 1422.957393747230071, 222.1873873175979952 ) ) ;
#101187 = ORIENTED_EDGE ( 'NONE', *, *, #33624, .T. ) ;
#101188 = ORIENTED_EDGE ( 'NONE', *, *, #104765, .T. ) ;
#101189 = CARTESIAN_POINT ( 'NONE',  ( -9.930122423809999432, 1499.782504084789934, 217.2571562510489969 ) ) ;
#101190 = CARTESIAN_POINT ( 'NONE',  ( -19.42715338204342501, 1485.587694890019065, 189.9367742298745156 ) ) ;
#101191 = CARTESIAN_POINT ( 'NONE',  ( -29.11003132769999624, 1509.929605081229965, 211.9058968252579973 ) ) ;
#101192 = CARTESIAN_POINT ( 'NONE',  ( 11.45283955604839932, 1502.343333994649811, 211.2592759328639715 ) ) ;
#101193 = CARTESIAN_POINT ( 'NONE',  ( -10.07154918488590134, 1473.228065907060000, 207.4129428866500007 ) ) ;
#101194 = DIRECTION ( 'NONE',  ( -0.7071067811860475283, 0.000000000000000000, -0.7071067811870476172 ) ) ;
#101196 = CIRCLE ( 'NONE', #56554, 2.008813507203440096 ) ;
#101195 = CARTESIAN_POINT ( 'NONE',  ( -3.608621357268490204, 1488.296475687800012, 219.4393136407599911 ) ) ;
#101197 = CARTESIAN_POINT ( 'NONE',  ( -4.123250153539999907, 1515.545045452190152, 208.3730692491820093 ) ) ;
#101198 = CARTESIAN_POINT ( 'NONE',  ( -61.45951696033579736, 1383.794773811220011, 283.0528198679410252 ) ) ;
#101199 = CARTESIAN_POINT ( 'NONE',  ( 15.96653243319999937, 1452.355496787929951, 148.2552934822979864 ) ) ;
#101200 = CARTESIAN_POINT ( 'NONE',  ( 11.39903530061180170, 1471.112746094619979, 209.6182361319149834 ) ) ;
#101201 = CARTESIAN_POINT ( 'NONE',  ( 12.30197900188439952, 1492.344385971049860, 210.1930000934870009 ) ) ;
#101203 = ORIENTED_EDGE ( 'NONE', *, *, #105133, .T. ) ;
#101202 = CARTESIAN_POINT ( 'NONE',  ( -1.929956593220000016, 1456.736549107989958, 218.5607043152189704 ) ) ;
#101204 = LINE ( 'NONE', #32909, #32486 ) ;
#101205 = CARTESIAN_POINT ( 'NONE',  ( -54.73637590230000427, 1382.331405336219859, 270.0802247036589847 ) ) ;
#101206 = CARTESIAN_POINT ( 'NONE',  ( -19.18108385108779856, 1409.582878595139846, 219.3495538156010127 ) ) ;
#101207 = VERTEX_POINT ( 'NONE', #75078 ) ;
#101208 = VERTEX_POINT ( 'NONE', #92392 ) ;
#101209 = CARTESIAN_POINT ( 'NONE',  ( -9.775751096677179675, 1386.869787730469852, 218.1689280660520183 ) ) ;
#101210 = CARTESIAN_POINT ( 'NONE',  ( 34.15097007435170440, 1437.022904788399956, 136.5542998879990080 ) ) ;
#101212 = DIRECTION ( 'NONE',  ( 1.987342477590000096E-13, -6.939952856119990566E-15, -1.000000000000000000 ) ) ;
#101211 = CARTESIAN_POINT ( 'NONE',  ( -11.90008666459999986, 1434.920851464509951, 147.6452002888979962 ) ) ;
#101213 = CARTESIAN_POINT ( 'NONE',  ( -9.160644070140000039, 1462.341874057690120, 205.2627832839989992 ) ) ;
#101214 = CARTESIAN_POINT ( 'NONE',  ( -106.3258853770000059, 1381.775203003109937, 298.5533487220590132 ) ) ;
#101215 = CARTESIAN_POINT ( 'NONE',  ( -11.42988456683059617, 1434.706941777702468, 151.4745012951066201 ) ) ;
#101216 = CARTESIAN_POINT ( 'NONE',  ( -7.939942809495481590, 1508.551704408389924, 218.9616636473319886 ) ) ;
#101217 = CARTESIAN_POINT ( 'NONE',  ( 1.201030227405109896, 1507.126550697769972, 181.0678294923270073 ) ) ;
#101218 = CARTESIAN_POINT ( 'NONE',  ( 18.03271313680000176, 1424.708338662830101, 225.1466562137979963 ) ) ;
#101219 = CARTESIAN_POINT ( 'NONE',  ( 3.396568279634440302, 1487.113085923700055, 197.6558524979510025 ) ) ;
#101220 = CARTESIAN_POINT ( 'NONE',  ( -11.86606300521394353, 1432.348818993920986, 150.6996689860163485 ) ) ;
#101221 = CARTESIAN_POINT ( 'NONE',  ( -2.710844305144630262, 1440.404038868829957, 159.2733880920049785 ) ) ;
#101222 = DIRECTION ( 'NONE',  ( 0.000000000000000000, 1.000000000000000000, 0.000000000000000000 ) ) ;
#101223 = ORIENTED_EDGE ( 'NONE', *, *, #36617, .F. ) ;
#101224 = CARTESIAN_POINT ( 'NONE',  ( 4.074350933259999502E-15, 1428.579607037230062, 149.5143047311979672 ) ) ;
#101225 = CARTESIAN_POINT ( 'NONE',  ( 19.68865308375039902, 1455.839336106299925, 227.5737452897460003 ) ) ;
#101226 = CARTESIAN_POINT ( 'NONE',  ( 15.78884811940000077, 1449.507807645780076, 190.2809706474979805 ) ) ;
#101227 = CARTESIAN_POINT ( 'NONE',  ( -8.859375228535989748E-12, 1470.046988918149964, 254.1474031498040063 ) ) ;
#101228 = CARTESIAN_POINT ( 'NONE',  ( -12.99430343120000053, 1503.123593417290067, 208.6821788852620045 ) ) ;
#101229 = CARTESIAN_POINT ( 'NONE',  ( -2.021349652797419960, 1420.993378913349943, 193.8016399264820109 ) ) ;
#101230 = CARTESIAN_POINT ( 'NONE',  ( 2.224758126099999789, 1476.466451453390164, 198.2506516800989971 ) ) ;
#101231 = CARTESIAN_POINT ( 'NONE',  ( -108.3007714539999995, 1388.465142555530065, 310.2841513672590281 ) ) ;
#101232 = CARTESIAN_POINT ( 'NONE',  ( -0.04889493835150059836, 1486.217974350728127, 181.8156037349973246 ) ) ;
#101233 = CARTESIAN_POINT ( 'NONE',  ( -9.251045835782019111, 1361.603097335492066, 210.6218459617030021 ) ) ;
#101234 = CARTESIAN_POINT ( 'NONE',  ( -45.62076656701439958, 1439.252528880889940, 266.1899235483149937 ) ) ;
#101235 = FACE_OUTER_BOUND ( 'NONE', #103468, .T. ) ;
#101236 = CARTESIAN_POINT ( 'NONE',  ( -8.375043687299998041, 1424.685418102950052, 206.2101447219289696 ) ) ;
#101237 = CARTESIAN_POINT ( 'NONE',  ( 4.037050997585000189, 1516.939819969850078, 209.1086255745840106 ) ) ;
#101238 = CARTESIAN_POINT ( 'NONE',  ( -2.478946879530000036, 1432.276406454319840, 157.5139443807979944 ) ) ;
#101239 = CARTESIAN_POINT ( 'NONE',  ( -14.42421378022759981, 1379.620479347240007, 208.1098118855669838 ) ) ;
#101240 = CARTESIAN_POINT ( 'NONE',  ( 7.380481980853459412, 1426.294419419770065, 212.6173424388080093 ) ) ;
#101241 = CARTESIAN_POINT ( 'NONE',  ( 8.842788026528301870, 1423.233140882379985, 211.5963855810900043 ) ) ;
#101242 = CARTESIAN_POINT ( 'NONE',  ( -26.85028794030449717, 1451.809831805880094, 135.6476290392230055 ) ) ;
#101243 = ORIENTED_EDGE ( 'NONE', *, *, #4240, .T. ) ;
#101244 = CARTESIAN_POINT ( 'NONE',  ( 26.67762292569999971, 1440.913060399449932, 225.6805344092979908 ) ) ;
#101246 = CARTESIAN_POINT ( 'NONE',  ( -4.363122647530000009, 1419.257904667329967, 165.6263425522979844 ) ) ;
#101245 = CARTESIAN_POINT ( 'NONE',  ( -2.596261494520144986, 1525.907212628473872, 177.4701144822249148 ) ) ;
#101247 = CARTESIAN_POINT ( 'NONE',  ( -1.312249485446211450, 1488.152622635656144, 219.9118893847204390 ) ) ;
#101248 = CARTESIAN_POINT ( 'NONE',  ( -24.09814616333339998, 1444.255785637029931, 212.5772553280679915 ) ) ;
#101249 = CARTESIAN_POINT ( 'NONE',  ( -29.11537602464361640, 1509.936047831340375, 204.3288344588696930 ) ) ;
#101250 = CARTESIAN_POINT ( 'NONE',  ( 22.57319362359999815, 1409.701316935530031, 208.7927549349429910 ) ) ;
#101251 = CARTESIAN_POINT ( 'NONE',  ( 4.904030442849999893, 1425.409506399530073, 209.9084226658820000 ) ) ;
#101252 = VERTEX_POINT ( 'NONE', #109228 ) ;
#101253 = FACE_OUTER_BOUND ( 'NONE', #49114, .T. ) ;
#101254 = CARTESIAN_POINT ( 'NONE',  ( 16.50119538672600328, 1422.031755069739802, 227.1504397986250012 ) ) ;
#101255 = CARTESIAN_POINT ( 'NONE',  ( 10.94747859850000005, 1461.374937641390034, 209.8474444777559995 ) ) ;
#101256 = ORIENTED_EDGE ( 'NONE', *, *, #9770, .T. ) ;
#101257 = ORIENTED_EDGE ( 'NONE', *, *, #83249, .T. ) ;
#101258 = CARTESIAN_POINT ( 'NONE',  ( -64.54217663740000432, 1384.956766891789812, 254.0305872787589863 ) ) ;
#101259 = CARTESIAN_POINT ( 'NONE',  ( -23.58958983610000359, 1410.013969636130014, 209.3130814696430093 ) ) ;
#101260 = VERTEX_POINT ( 'NONE', #109764 ) ;
#101261 = CARTESIAN_POINT ( 'NONE',  ( -103.0210057964000043, 1376.302340817389904, 309.8919163327390152 ) ) ;
#101262 = DIRECTION ( 'NONE',  ( 0.000000000000000000, 0.000000000000000000, -1.000000000000000000 ) ) ;
#101263 = CARTESIAN_POINT ( 'NONE',  ( -1.024257868869999921, 1498.353689748030092, 236.8278422010980080 ) ) ;
#101265 = AXIS2_PLACEMENT_3D ( 'NONE', #59859, #109297, #30917 ) ;
#101264 = CARTESIAN_POINT ( 'NONE',  ( -21.04576247069999795, 1410.867134376630247, 218.2990911740579918 ) ) ;
#101266 = EDGE_CURVE ( 'NONE', #62022, #6492, #71627, .T. ) ;
#101267 = CARTESIAN_POINT ( 'NONE',  ( 44.56610056812340304, 1449.954323543940063, 266.7258405368609715 ) ) ;
#101268 = ADVANCED_FACE ( 'NONE', ( #44789 ), #65953, .F. ) ;
#101269 = CARTESIAN_POINT ( 'NONE',  ( -11.17502343409620025, 1391.913060387130145, 206.4900290431199892 ) ) ;
#101270 = CARTESIAN_POINT ( 'NONE',  ( -17.07650506179803784, 1422.150741894849034, 226.7700359724246937 ) ) ;
#101271 = CARTESIAN_POINT ( 'NONE',  ( -2.297085753945000253, 1516.718889242609976, 205.0950684461469962 ) ) ;
#101272 = ORIENTED_EDGE ( 'NONE', *, *, #100687, .F. ) ;
#101273 = CARTESIAN_POINT ( 'NONE',  ( 18.48198528575022692, 1458.805764898813550, 227.6411767142042493 ) ) ;
#101274 = CARTESIAN_POINT ( 'NONE',  ( 1.194678736856909840, 1445.356568564189956, 199.1147239880469897 ) ) ;
#101275 = FACE_OUTER_BOUND ( 'NONE', #13691, .T. ) ;
#101276 = ORIENTED_EDGE ( 'NONE', *, *, #71407, .F. ) ;
#101277 = CARTESIAN_POINT ( 'NONE',  ( -10.92262152852349999, 1480.972147131519705, 210.3691105597789885 ) ) ;
#101278 = ADVANCED_FACE ( 'NONE', ( #88848 ), #21062, .F. ) ;
#101279 = CARTESIAN_POINT ( 'NONE',  ( 6.357608626507394334, 1435.035992033701632, 203.3974798508943422 ) ) ;
#101280 = EDGE_CURVE ( 'NONE', #89888, #14943, #41542, .T. ) ;
#101281 = CARTESIAN_POINT ( 'NONE',  ( 2.487935123020000194, 1508.551704408389924, 204.1347675455010062 ) ) ;
#101282 = CARTESIAN_POINT ( 'NONE',  ( 12.01380273547430022, 1501.779913421650008, 213.3188837843350143 ) ) ;
#101283 = CARTESIAN_POINT ( 'NONE',  ( 8.286012754340001507, 1421.269451573359902, 196.1401172957990013 ) ) ;
#101284 = CARTESIAN_POINT ( 'NONE',  ( 19.74914731032970039, 1409.602715808129915, 217.6725271438159837 ) ) ;
#101285 = CARTESIAN_POINT ( 'NONE',  ( 10.13999722834100048, 1479.891769232120168, 205.9780649761750055 ) ) ;
#101286 = CARTESIAN_POINT ( 'NONE',  ( 12.62627334406020019, 1409.353979568340037, 191.9928717526780133 ) ) ;
#101288 = CARTESIAN_POINT ( 'NONE',  ( 3.827327205999999649, 1425.634807632230149, 171.7326279529979729 ) ) ;
#101287 = CARTESIAN_POINT ( 'NONE',  ( 1.053929134969999959, 1415.609761246630114, 233.1238235151980120 ) ) ;
#101289 = CARTESIAN_POINT ( 'NONE',  ( 14.91703010720000044, 1409.433974557229931, 225.8933006754979829 ) ) ;
#101290 = CARTESIAN_POINT ( 'NONE',  ( -12.22846866959999979, 1380.845870869829923, 215.9110647297389960 ) ) ;
#101291 = CARTESIAN_POINT ( 'NONE',  ( 12.88172607065413544, 1420.897005229514207, 231.3054420824058184 ) ) ;
#101292 = EDGE_LOOP ( 'NONE', ( #109493, #108116, #26514, #21102, #35088 ) ) ;
#101293 = CARTESIAN_POINT ( 'NONE',  ( 13.02322915956219873, 1416.825783990419950, 221.6328433159220026 ) ) ;
#101294 = CARTESIAN_POINT ( 'NONE',  ( 11.62445986000279952, 1432.338721181900155, 150.9949992740019979 ) ) ;
#101295 = CARTESIAN_POINT ( 'NONE',  ( 32.20549126534967854, 1524.425415513989037, 202.1446967539542641 ) ) ;
#101296 = CARTESIAN_POINT ( 'NONE',  ( -10.79874708580000053, 1388.923907300369819, 202.4036804765890167 ) ) ;
#101297 = B_SPLINE_CURVE_WITH_KNOTS ( 'NONE', 3,
 ( #22956, #83983, #15645, #24058, #8368, #76690, #40328, #32492, #49851, #1, #66664, #24601 ),
 .UNSPECIFIED., .F., .F.,
 ( 4, 2, 2, 2, 2, 4 ),
 ( 0.000000000000000000, 0.2500000000000786038, 0.3750000000001127987, 0.4375000000000939249, 0.5000000000000750511, 1.000000000000000000 ),
 .UNSPECIFIED. ) ;
#101298 = CARTESIAN_POINT ( 'NONE',  ( 10.54753901010710138, 1427.432118304579944, 209.9055955873279800 ) ) ;
#101299 = ADVANCED_FACE ( 'NONE', ( #89399 ), #28307, .T. ) ;
#101300 = CARTESIAN_POINT ( 'NONE',  ( 12.43362777651829987, 1421.210458342309948, 203.4350632585469896 ) ) ;
#101301 = CARTESIAN_POINT ( 'NONE',  ( 1.483741821009999962, 1430.780200044390085, 217.7366157072389967 ) ) ;
#101302 = CARTESIAN_POINT ( 'NONE',  ( -17.87874080430000134, 1466.750581352830068, 265.6112252686980355 ) ) ;
#101303 = CARTESIAN_POINT ( 'NONE',  ( -22.28175276906668856, 1509.670458419194802, 191.1299263873633265 ) ) ;
#101304 = CARTESIAN_POINT ( 'NONE',  ( 11.23027220810000060, 1433.733175409749947, 151.5806659527979718 ) ) ;
#101305 = CARTESIAN_POINT ( 'NONE',  ( 32.79207798030000021, 1453.265480487729974, 262.6648722511980054 ) ) ;
#101306 = CARTESIAN_POINT ( 'NONE',  ( -9.843047294206771269, 1461.614624003160088, 208.6138576386200043 ) ) ;
#101307 = ADVANCED_FACE ( 'NONE', ( #4303 ), #6939, .F. ) ;
#101308 = FACE_OUTER_BOUND ( 'NONE', #100992, .T. ) ;
#101309 = CARTESIAN_POINT ( 'NONE',  ( 11.00511108145959938, 1420.479169930370063, 198.1891849291089898 ) ) ;
#101310 = ADVANCED_FACE ( 'NONE', ( #93244 ), #16510, .F. ) ;
#101311 = CARTESIAN_POINT ( 'NONE',  ( 9.297172576236979680, 1464.629289270589879, 212.4694656482230073 ) ) ;
#101312 = CARTESIAN_POINT ( 'NONE',  ( 22.74352444629999681, 1409.874439160429802, 207.7226808069280253 ) ) ;
#101313 = CARTESIAN_POINT ( 'NONE',  ( 10.21356127135914349, 1398.215732791116807, 217.1961878391145149 ) ) ;
#101314 = CARTESIAN_POINT ( 'NONE',  ( -16.56429154530000147, 1409.491498197430019, 225.2428481817979957 ) ) ;
#101315 = CARTESIAN_POINT ( 'NONE',  ( 18.68355583210000148, 1410.903490284329791, 222.0895934915980092 ) ) ;
#101316 = AXIS2_PLACEMENT_3D ( 'NONE', #71936, #4147, #30978 ) ;
#101317 = B_SPLINE_CURVE_WITH_KNOTS ( 'NONE', 3,
 ( #47810, #5248, #6894, #13073 ),
 .UNSPECIFIED., .F., .F.,
 ( 4, 4 ),
 ( 0.000000000000000000, 1.000000000000000000 ),
 .UNSPECIFIED. ) ;
#101318 = CARTESIAN_POINT ( 'NONE',  ( 0.7430128073871236083, 1477.852875664036219, 198.7306773389195484 ) ) ;
#101319 = CARTESIAN_POINT ( 'NONE',  ( -16.16107894238729870, 1409.477417702470120, 193.2192893929600075 ) ) ;
#101320 = CARTESIAN_POINT ( 'NONE',  ( -1.118758552070000079, 1515.569725561690120, 205.1507450494889895 ) ) ;
#101321 = CARTESIAN_POINT ( 'NONE',  ( -2.057041824809803465, 1523.342713519622976, 173.3972930408659749 ) ) ;
#101322 = CARTESIAN_POINT ( 'NONE',  ( -17.66147425336259857, 1440.150478482380095, 218.7822780451419931 ) ) ;
#101323 = CARTESIAN_POINT ( 'NONE',  ( -19.27023455780000205, 1418.866878321930017, 210.2656499040089670 ) ) ;
#101324 = CARTESIAN_POINT ( 'NONE',  ( 0.1696119624267240222, 1480.557672209769862, 182.0704353423009820 ) ) ;
#101326 = ORIENTED_EDGE ( 'NONE', *, *, #5669, .F. ) ;
#101325 = CARTESIAN_POINT ( 'NONE',  ( -3.109694234880000074, 1409.021653302929735, 223.8091977979979958 ) ) ;
#101327 = CARTESIAN_POINT ( 'NONE',  ( -13.51610093809999924, 1444.324653571829913, 169.3501091259980171 ) ) ;
#101328 = CARTESIAN_POINT ( 'NONE',  ( -4.367937192439999450, 1447.898255911189835, 190.6350925615990093 ) ) ;
#101329 = CARTESIAN_POINT ( 'NONE',  ( 11.87907512690000011, 1433.311753932999864, 149.8850494226980175 ) ) ;
#101330 = CARTESIAN_POINT ( 'NONE',  ( -40.49955491220639914, 1447.865363690129925, 134.0999999983799853 ) ) ;
#101331 = FACE_OUTER_BOUND ( 'NONE', #20476, .T. ) ;
#101332 = EDGE_LOOP ( 'NONE', ( #92730, #100854 ) ) ;
#101333 = CARTESIAN_POINT ( 'NONE',  ( -17.72016947434968159, 1524.201816949777822, 180.4881000152817876 ) ) ;
#101334 = CARTESIAN_POINT ( 'NONE',  ( 3.347801439296140380, 1523.382868172864164, 176.1543725841967216 ) ) ;
#101335 = CARTESIAN_POINT ( 'NONE',  ( -104.3428327140408385, 1380.439868052300881, 307.2882731461818366 ) ) ;
#101336 = DIRECTION ( 'NONE',  ( 0.9977304882603014180, 0.06733403890946067227, 0.000000000000000000 ) ) ;
#101337 = CARTESIAN_POINT ( 'NONE',  ( 3.063200971469999701, 1505.793422128889915, 221.5342279770990217 ) ) ;
#101338 = LINE ( 'NONE', #16236, #76799 ) ;
#101339 = DIRECTION ( 'NONE',  ( -0.9455185755993178454, 0.000000000000000000, 0.3255681544571537578 ) ) ;
#101340 = VECTOR ( 'NONE', #70375, 1000.000000000000114 ) ;
#101341 = CARTESIAN_POINT ( 'NONE',  ( -16.66936639845670243, 1512.187213306747481, 180.4828114240741854 ) ) ;
#101342 = CARTESIAN_POINT ( 'NONE',  ( 4.329448776040000446, 1515.064792882589927, 210.9648081929590262 ) ) ;
#101343 = CARTESIAN_POINT ( 'NONE',  ( -69.86459936517930203, 1385.111636070419763, 265.6217149743549726 ) ) ;
#101344 = CARTESIAN_POINT ( 'NONE',  ( -20.64339891394538284, 1523.429859730330236, 238.2599442700839063 ) ) ;
#101345 = CARTESIAN_POINT ( 'NONE',  ( 11.19645453711150118, 1427.175649664649882, 208.5743989061170112 ) ) ;
#101346 = ORIENTED_EDGE ( 'NONE', *, *, #77392, .T. ) ;
#101347 = CARTESIAN_POINT ( 'NONE',  ( -33.92643339480000719, 1450.868067258620158, 136.1711496515980286 ) ) ;
#101348 = CARTESIAN_POINT ( 'NONE',  ( -15.73572830516989995, 1409.462552141119886, 225.2909338128490049 ) ) ;
#101350 = VERTEX_POINT ( 'NONE', #93776 ) ;
#101349 = DIRECTION ( 'NONE',  ( 1.755985294532469921E-16, -1.000000000000000000, 1.338183447452831989E-16 ) ) ;
#101351 = CARTESIAN_POINT ( 'NONE',  ( 4.321260515560000570, 1472.734096669689961, 218.3662689135690016 ) ) ;
#101352 =( BOUNDED_CURVE ( )  B_SPLINE_CURVE ( 3, ( #91229, #14509, #377, #73337 ),
 .UNSPECIFIED., .F., .F. ) 
 B_SPLINE_CURVE_WITH_KNOTS ( ( 4, 4 ),
 ( 4.154228272801879562, 5.270549769551020169 ),
 .UNSPECIFIED. ) 
 CURVE ( )  GEOMETRIC_REPRESENTATION_ITEM ( )  RATIONAL_B_SPLINE_CURVE ( ( 1.000000000000000000, 0.8988204416492726612, 0.8988204416492726612, 1.000000000000000000 ) ) 
 REPRESENTATION_ITEM ( '' )  );
#101353 = CARTESIAN_POINT ( 'NONE',  ( -21.47452075964614338, 1411.021838315141167, 216.8631755304516560 ) ) ;
#101354 = CARTESIAN_POINT ( 'NONE',  ( -109.9857361549999979, 1384.899971913130003, 311.4562995532589866 ) ) ;
#101355 = CARTESIAN_POINT ( 'NONE',  ( 16.78480385485693560, 1526.748660780343471, 236.7163225783321820 ) ) ;
#101356 = B_SPLINE_CURVE_WITH_KNOTS ( 'NONE', 5,
 ( #82738, #100625, #74364, #6029, #23908, #41291 ),
 .UNSPECIFIED., .F., .F.,
 ( 6, 6 ),
 ( 0.000000000000000000, 1.000000000000000000 ),
 .UNSPECIFIED. ) ;
#101357 = CARTESIAN_POINT ( 'NONE',  ( 41.29477646232137289, 1446.681373312819233, 269.6341301600875227 ) ) ;
#101358 = CARTESIAN_POINT ( 'NONE',  ( 15.40733310992444061, 1431.102793365615526, 219.5436081709931102 ) ) ;
#101359 = CARTESIAN_POINT ( 'NONE',  ( 1.537569739530000090, 1415.820179752829972, 232.6983187733980003 ) ) ;
#101360 = CARTESIAN_POINT ( 'NONE',  ( 9.923042113430000200, 1451.489751075389904, 207.3834753964790139 ) ) ;
#101361 = CARTESIAN_POINT ( 'NONE',  ( -8.190304658720000575, 1512.060957475689975, 212.0841603825689958 ) ) ;
#101362 = CARTESIAN_POINT ( 'NONE',  ( 8.486299124169999430, 1519.913060387329779, 230.6230627099979813 ) ) ;
#101363 = CARTESIAN_POINT ( 'NONE',  ( -29.35747451428025556, 1526.382868172571307, 217.1997937176765276 ) ) ;
#101364 = EDGE_CURVE ( 'NONE', #108882, #109440, #96315, .T. ) ;
#101365 = CARTESIAN_POINT ( 'NONE',  ( -6.950214971414999887, 1517.129577905929864, 206.2502655435069983 ) ) ;
#101366 = VECTOR ( 'NONE', #21268, 1000.000000000000000 ) ;
#101368 = EDGE_CURVE ( 'NONE', #91018, #58921, #96977, .T. ) ;
#101367 = CARTESIAN_POINT ( 'NONE',  ( 2.712106673540000124, 1447.524052171519770, 157.8378389823980115 ) ) ;
#101369 = VERTEX_POINT ( 'NONE', #70300 ) ;
#101370 = CARTESIAN_POINT ( 'NONE',  ( 13.58268853699999923, 1416.851343894929869, 196.3340833729979806 ) ) ;
#101372 = VERTEX_POINT ( 'NONE', #43962 ) ;
#101371 = CARTESIAN_POINT ( 'NONE',  ( -68.69690608884340577, 1379.747745670520089, 280.2939418190039760 ) ) ;
#101373 = CARTESIAN_POINT ( 'NONE',  ( -16.17440652799999867, 1423.017051802529977, 229.3744292183979780 ) ) ;
#101374 = VERTEX_POINT ( 'NONE', #17614 ) ;
#101375 = CARTESIAN_POINT ( 'NONE',  ( -1.906498070525230022E-08, 1509.051704408389924, 202.1089243866269953 ) ) ;
#101376 = CARTESIAN_POINT ( 'NONE',  ( -25.25968088059999772, 1449.800564160949989, 206.5373934562080080 ) ) ;
#101378 = CARTESIAN_POINT ( 'NONE',  ( 16.04662172663540076, 1409.498810407800192, 192.7255589890200156 ) ) ;
#101377 = CARTESIAN_POINT ( 'NONE',  ( -10.80134480061109947, 1441.261220175989820, 153.0805715986579969 ) ) ;
#101379 = CARTESIAN_POINT ( 'NONE',  ( 0.01323701367210150005, 1516.939658295650133, 211.6080660720070341 ) ) ;
#101380 = CARTESIAN_POINT ( 'NONE',  ( 40.14205882339999221, 1442.180247714630013, 136.9520358780980018 ) ) ;
#101381 = ADVANCED_FACE ( 'NONE', ( #60218 ), #101708, .T. ) ;
#101382 = CARTESIAN_POINT ( 'NONE',  ( 2.939888137859999853E-10, 1407.100405669929842, 264.8986903017979557 ) ) ;
#101383 = CARTESIAN_POINT ( 'NONE',  ( 2.883409711490000138, 1409.181735907030088, 231.0710487667979862 ) ) ;
#101384 = CARTESIAN_POINT ( 'NONE',  ( 12.65743788132100178, 1500.841905234319711, 210.2807706420859972 ) ) ;
#101385 = CONTEXT_DEPENDENT_SHAPE_REPRESENTATION ( #41345, #97375 ) ;
#101386 = CARTESIAN_POINT ( 'NONE',  ( 4.956729644103719856, 1508.551704408389924, 212.0071758648730054 ) ) ;
#101387 = CARTESIAN_POINT ( 'NONE',  ( -34.35202081865160295, 1437.040941089060198, 136.5493581184059906 ) ) ;
#101388 = EDGE_LOOP ( 'NONE', ( #105609, #4086, #53776, #80304 ) ) ;
#101389 = CARTESIAN_POINT ( 'NONE',  ( -16.53114349369899827, 1465.611506726459993, 220.7423202708849885 ) ) ;
#101390 = CARTESIAN_POINT ( 'NONE',  ( -18.60076228999999870, 1457.261067633329958, 228.0100651602980122 ) ) ;
#101391 = VERTEX_POINT ( 'NONE', #77298 ) ;
#101392 = ORIENTED_EDGE ( 'NONE', *, *, #36371, .T. ) ;
#101393 = AXIS2_PLACEMENT_3D ( 'NONE', #5788, #81361, #90873 ) ;
#101394 = CARTESIAN_POINT ( 'NONE',  ( -1.985912070879999991, 1431.344737485190308, 203.7584604878390167 ) ) ;
#101395 = CARTESIAN_POINT ( 'NONE',  ( 29.38941569566759782, 1446.173485254500065, 137.1432708255389912 ) ) ;
#101396 = CARTESIAN_POINT ( 'NONE',  ( -7.604021728224319432, 1508.390716753870265, 219.6025803338619937 ) ) ;
#101397 = CARTESIAN_POINT ( 'NONE',  ( -14.74338484529040016, 1507.984222099330054, 209.4136964162090067 ) ) ;
#101398 = B_SPLINE_CURVE_WITH_KNOTS ( 'NONE', 3,
 ( #95733, #26305, #36923, #78385, #71119, #103008, #1141, #27417 ),
 .UNSPECIFIED., .F., .F.,
 ( 4, 2, 2, 4 ),
 ( 0.000000000000000000, 0.2500000000000000000, 0.5000000000000000000, 1.000000000000000000 ),
 .UNSPECIFIED. ) ;
#101399 = ADVANCED_FACE ( 'NONE', ( #8409 ), #55259, .T. ) ;
#101400 = DIRECTION ( 'NONE',  ( 0.5877852522924673639, 0.000000000000000000, -0.8090169943749514481 ) ) ;
#101401 = VECTOR ( 'NONE', #24110, 1000.000000000000000 ) ;
#101402 = CARTESIAN_POINT ( 'NONE',  ( -3.350338079455597029, 1523.604703353109699, 242.0808062845893289 ) ) ;
#101403 = CARTESIAN_POINT ( 'NONE',  ( 40.71747596959940552, 1448.637563236709866, 134.4205493173820116 ) ) ;
#101404 = CARTESIAN_POINT ( 'NONE',  ( 5.761714419953206878, 1516.919864955462117, 213.9826803693840986 ) ) ;
#101405 = EDGE_CURVE ( 'NONE', #80510, #42283, #39069, .T. ) ;
#101406 = CARTESIAN_POINT ( 'NONE',  ( 25.77823332670000056, 1439.625665060110123, 137.8633119874980082 ) ) ;
#101407 = CARTESIAN_POINT ( 'NONE',  ( -11.62394760940000005, 1391.913060725860078, 211.5064627571190101 ) ) ;
#101408 = CARTESIAN_POINT ( 'NONE',  ( -90.63163529889820325, 1384.841170975159912, 292.9371972892139411 ) ) ;
#101409 = ORIENTED_EDGE ( 'NONE', *, *, #29046, .F. ) ;
#101410 = CARTESIAN_POINT ( 'NONE',  ( 4.034280915654999689, 1517.049325831759916, 202.1735242262370207 ) ) ;
#101411 = CARTESIAN_POINT ( 'NONE',  ( -3.455495871984999745, 1516.939877939420057, 209.1351200182310208 ) ) ;
#101412 = ORIENTED_EDGE ( 'NONE', *, *, #13778, .F. ) ;
#101414 = ADVANCED_FACE ( 'NONE', ( #34724 ), #6543, .T. ) ;
#101413 = CARTESIAN_POINT ( 'NONE',  ( 11.79395621469850042, 1427.957957693540038, 147.8640485709500183 ) ) ;
#101415 = B_SPLINE_CURVE_WITH_KNOTS ( 'NONE', 3,
 ( #93281, #16544, #68120, #67560, #101663, #74310, #7624, #75408, #23317, #59161, #66467, #109548, #102232, #74853, #6529, #50735, #25510, #108439, #24952, #31720, #65906, #32821, #100024, #57509, #91634, #67008, #101118, #49101 ),
 .UNSPECIFIED., .F., .F.,
 ( 4, 3, 3, 3, 3, 3, 3, 3, 3, 4 ),
 ( 4.991132198461049718, 5.278154230359260346, 5.575591039645609648, 5.870273492830619944, 6.165162712813499368, 6.464350792820829916, 6.767514390815449588, 7.076365246473460324, 7.382407343323190041, 7.657648704650000582 ),
 .UNSPECIFIED. ) ;
#101416 = CARTESIAN_POINT ( 'NONE',  ( 19.78107824579999985, 1507.861720175329992, 229.2768328414980203 ) ) ;
#101417 = ORIENTED_EDGE ( 'NONE', *, *, #104128, .T. ) ;
#101418 = CARTESIAN_POINT ( 'NONE',  ( -13.65307821740000094, 1415.140114704729967, 220.7168886283980100 ) ) ;
#101419 = CARTESIAN_POINT ( 'NONE',  ( -11.86610048948770135, 1432.336024750160050, 149.9824232984959735 ) ) ;
#101420 = CARTESIAN_POINT ( 'NONE',  ( -4.853522982481027093, 1432.607957074035767, 216.0726889064482918 ) ) ;
#101421 = CARTESIAN_POINT ( 'NONE',  ( -1.921445414331789836, 1468.480943170730143, 219.3341389517340190 ) ) ;
#101422 = CARTESIAN_POINT ( 'NONE',  ( -4.280412110000000325, 1421.771089477929763, 185.3634408331980126 ) ) ;
#101423 = CARTESIAN_POINT ( 'NONE',  ( 14.51815713490480064, 1436.250993400889911, 149.9197837022770159 ) ) ;
#101424 = CARTESIAN_POINT ( 'NONE',  ( -9.558504124660036183, 1469.579538799191596, 215.2844292078696071 ) ) ;
#101425 = CARTESIAN_POINT ( 'NONE',  ( -9.958615577691062981, 1410.635533730419411, 188.4118002158843126 ) ) ;
#101426 = CARTESIAN_POINT ( 'NONE',  ( -56.81483858269999843, 1379.709620124910089, 254.2646988397590064 ) ) ;
#101427 = CARTESIAN_POINT ( 'NONE',  ( -16.66912029359999892, 1496.363909377430218, 224.2133594559979883 ) ) ;
#101428 = ADVANCED_FACE ( 'NONE', ( #54319 ), #84742, .T. ) ;
#101430 = CARTESIAN_POINT ( 'NONE',  ( 6.277214161762089795, 1467.366245655900002, 199.9216203958389997 ) ) ;
#101429 = CARTESIAN_POINT ( 'NONE',  ( -21.68513540049999833, 1505.549217140589917, 209.4741210534890001 ) ) ;
#101431 = CYLINDRICAL_SURFACE ( 'NONE', #43774, 2.458500000000005237 ) ;
#101432 = AXIS2_PLACEMENT_3D ( 'NONE', #91449, #31528, #73002 ) ;
#101433 = CARTESIAN_POINT ( 'NONE',  ( 0.01010282929720150019, 1516.939452820819952, 216.8414868732370167 ) ) ;
#101434 = ORIENTED_EDGE ( 'NONE', *, *, #74822, .F. ) ;
#101435 = EDGE_CURVE ( 'NONE', #16284, #39656, #69486, .T. ) ;
#101436 = CARTESIAN_POINT ( 'NONE',  ( 17.05938516367379876, 1517.051704408300111, 223.0487112149370148 ) ) ;
#101437 = CARTESIAN_POINT ( 'NONE',  ( -0.1447896363496347094, 1516.980486180143544, 216.8425613695660275 ) ) ;
#101438 = CARTESIAN_POINT ( 'NONE',  ( 5.784008635194999748, 1516.911981270829983, 214.1231845985469988 ) ) ;
#101439 = CARTESIAN_POINT ( 'NONE',  ( 5.430432121089999953, 1505.407861808090047, 219.8354485799989959 ) ) ;
#101440 = CARTESIAN_POINT ( 'NONE',  ( -11.43219139277870688, 1425.761513233309643, 138.9711987641360338 ) ) ;
#101442 = ORIENTED_EDGE ( 'NONE', *, *, #37764, .F. ) ;
#101441 = CARTESIAN_POINT ( 'NONE',  ( 4.832613776139130124, 1508.551704408389924, 212.6094311844759943 ) ) ;
#101443 = CARTESIAN_POINT ( 'NONE',  ( -8.371438357349999748, 1384.922515940929998, 199.7749755103790221 ) ) ;
#101444 = CARTESIAN_POINT ( 'NONE',  ( 15.69795926444620271, 1519.551704408389924, 222.7678737639049871 ) ) ;
#101445 = CARTESIAN_POINT ( 'NONE',  ( -11.64843198310000005, 1425.854362680330041, 145.0892392246979909 ) ) ;
#101446 = CARTESIAN_POINT ( 'NONE',  ( -4.329791528864999961, 1515.051704408389924, 205.7917117663469924 ) ) ;
#101447 = CARTESIAN_POINT ( 'NONE',  ( 33.91369266730000476, 1450.440660192670066, 136.2454535554979884 ) ) ;
#101448 = CARTESIAN_POINT ( 'NONE',  ( 27.03067664649999813, 1451.714498883330180, 135.7945611549980072 ) ) ;
#101449 = CARTESIAN_POINT ( 'NONE',  ( -2.500000000000000000, 1417.575542696430148, 161.0097146498980010 ) ) ;
#101450 = EDGE_CURVE ( 'NONE', #78256, #34085, #13916, .T. ) ;
#101451 = DIRECTION ( 'NONE',  ( 0.000000000000000000, -0.7071067811865467956, 0.7071067811865481278 ) ) ;
#101453 = CARTESIAN_POINT ( 'NONE',  ( -10.49833687454975717, 1422.381355195064998, 137.0999999980979567 ) ) ;
#101452 = CARTESIAN_POINT ( 'NONE',  ( -20.67946632569999821, 1482.729195731830032, 226.2368318870979920 ) ) ;
#101454 = FACE_OUTER_BOUND ( 'NONE', #37382, .T. ) ;
#101455 = VERTEX_POINT ( 'NONE', #82792 ) ;
#101456 = CARTESIAN_POINT ( 'NONE',  ( 6.935133380425000382, 1516.613881697390070, 205.8602099992770036 ) ) ;
#101457 = CARTESIAN_POINT ( 'NONE',  ( 7.072283668360000775, 1406.251336213230161, 267.2142513328980158 ) ) ;
#101458 = ADVANCED_FACE ( 'NONE', ( #4977 ), #67717, .T. ) ;
#101459 = CARTESIAN_POINT ( 'NONE',  ( 0.3485282687889999509, 1410.306756019930162, 185.0335118036979907 ) ) ;
#101460 = B_SPLINE_CURVE_WITH_KNOTS ( 'NONE', 3,
 ( #31079, #65262, #13155, #28890, #98283, #106682 ),
 .UNSPECIFIED., .F., .F.,
 ( 4, 2, 4 ),
 ( 0.000000000000000000, 0.5000000000000000000, 1.000000000000000000 ),
 .UNSPECIFIED. ) ;
#101461 = EDGE_CURVE ( 'NONE', #47496, #36172, #110620, .T. ) ;
#101462 = B_SPLINE_CURVE_WITH_KNOTS ( 'NONE', 3,
 ( #77446, #33217, #67960, #50587 ),
 .UNSPECIFIED., .F., .F.,
 ( 4, 4 ),
 ( 0.000000000000000000, 0.003000049121573526711 ),
 .UNSPECIFIED. ) ;
#101463 = CARTESIAN_POINT ( 'NONE',  ( 20.43741061629999933, 1430.298857861630040, 196.2683185269980015 ) ) ;
#101464 = CARTESIAN_POINT ( 'NONE',  ( 8.010394309675456626, 1506.575487365668323, 229.7209142108047786 ) ) ;
#101465 = CARTESIAN_POINT ( 'NONE',  ( -8.064928480694979029, 1387.323551673170186, 218.5893119357714056 ) ) ;
#101466 = DIRECTION ( 'NONE',  ( -0.9364122222710381527, 0.3043600949234490649, -0.1746341392729520714 ) ) ;
#101467 = CARTESIAN_POINT ( 'NONE',  ( -18.55872592996471582, 1457.839997766627903, 227.5285588845430595 ) ) ;
#101468 = CARTESIAN_POINT ( 'NONE',  ( -15.35210835959999898, 1415.142250310439749, 207.5991997658489936 ) ) ;
#101469 = CARTESIAN_POINT ( 'NONE',  ( -12.85666456360000076, 1446.605478062839893, 187.9028615879979895 ) ) ;
#101470 = CARTESIAN_POINT ( 'NONE',  ( -20.55257633559999775, 1497.713060387329961, 217.2216651986680063 ) ) ;
#101471 = CARTESIAN_POINT ( 'NONE',  ( -5.301601239306844349, 1495.069293905918585, 198.4488062458674733 ) ) ;
#101472 = CARTESIAN_POINT ( 'NONE',  ( 2.339369641392206489, 1407.692004974928750, 270.1366117262977014 ) ) ;
#101473 = CARTESIAN_POINT ( 'NONE',  ( 1.460551075230569928, 1495.400065749579881, 181.6242104856870299 ) ) ;
#101474 = DIRECTION ( 'NONE',  ( 5.980589973904019347E-17, -1.000000000000000000, 1.736889445713099699E-16 ) ) ;
#101475 = AXIS2_PLACEMENT_3D ( 'NONE', #88409, #72722, #106844 ) ;
#101476 = CARTESIAN_POINT ( 'NONE',  ( -11.77227379640609861, 1507.876490232319838, 208.2428952626790135 ) ) ;
#101477 = CARTESIAN_POINT ( 'NONE',  ( -9.417897711209606726, 1420.662740822867818, 195.0156077546988627 ) ) ;
#101478 = CARTESIAN_POINT ( 'NONE',  ( -18.29970625680000040, 1473.000870360929866, 266.8291869051980143 ) ) ;
#101479 = CARTESIAN_POINT ( 'NONE',  ( -31.00891611928356895, 1524.547873515804895, 196.4334223138416462 ) ) ;
#101480 = CARTESIAN_POINT ( 'NONE',  ( -14.16484771644310925, 1514.105042352133523, 192.5349129913882393 ) ) ;
#101481 = CARTESIAN_POINT ( 'NONE',  ( 17.96224420295349944, 1421.095635167079763, 223.9963144870330041 ) ) ;
#101482 = CARTESIAN_POINT ( 'NONE',  ( -52.68643441635880720, 1384.727329538739923, 267.2268374729209768 ) ) ;
#101483 = CARTESIAN_POINT ( 'NONE',  ( -9.276942849846040673, 1461.680302431059999, 206.2489141960740255 ) ) ;
#101484 = CIRCLE ( 'NONE', #6712, 1.000000000000000000 ) ;
#101485 = FACE_OUTER_BOUND ( 'NONE', #86088, .T. ) ;
#101486 = CARTESIAN_POINT ( 'NONE',  ( 2.021659750777782261, 1408.983658301473724, 230.3023721903324486 ) ) ;
#101487 = CARTESIAN_POINT ( 'NONE',  ( 6.033702791082116157, 1471.717643617360409, 217.3099286337410092 ) ) ;
#101488 = CARTESIAN_POINT ( 'NONE',  ( -45.85459844547133912, 1440.913031240881764, 268.7562811153424605 ) ) ;
#101489 = VECTOR ( 'NONE', #37245, 1000.000000000000114 ) ;
#101490 = CARTESIAN_POINT ( 'NONE',  ( -17.71984068230000275, 1409.531850859229962, 197.2724686579979902 ) ) ;
#101491 = CARTESIAN_POINT ( 'NONE',  ( -8.993343321902724341, 1381.641526762418835, 200.5640689155782184 ) ) ;
#101492 = CARTESIAN_POINT ( 'NONE',  ( -17.17241001986462123, 1512.187213306747481, 238.6251415217917895 ) ) ;
#101493 = CARTESIAN_POINT ( 'NONE',  ( 10.02412832500950124, 1480.534670654839829, 205.8825814297850059 ) ) ;
#101494 = CARTESIAN_POINT ( 'NONE',  ( 1.661536740469999884, 1441.600846913620217, 150.6803463261979914 ) ) ;
#101495 = CARTESIAN_POINT ( 'NONE',  ( -17.45557808899999941, 1442.885315458190007, 219.4073627859989699 ) ) ;
#101496 = CARTESIAN_POINT ( 'NONE',  ( 17.78112816951787067, 1523.954914175594240, 180.4163678545431537 ) ) ;
#101497 = CARTESIAN_POINT ( 'NONE',  ( 16.66442743449040265, 1492.498864362939912, 193.3249227321730075 ) ) ;
#101498 =( BOUNDED_CURVE ( )  B_SPLINE_CURVE ( 3, ( #84941, #58121, #25030, #8234 ),
 .UNSPECIFIED., .F., .F. ) 
 B_SPLINE_CURVE_WITH_KNOTS ( ( 4, 4 ),
 ( 0.1704839434639374984, 0.4574025252004559894 ),
 .UNSPECIFIED. ) 
 CURVE ( )  GEOMETRIC_REPRESENTATION_ITEM ( )  RATIONAL_B_SPLINE_CURVE ( ( 1.000000000000000000, 0.9931515681023461717, 0.9931515681023461717, 1.000000000000000000 ) ) 
 REPRESENTATION_ITEM ( '' )  );
#101500 = CARTESIAN_POINT ( 'NONE',  ( -14.96248399886500202, 1513.868118914750085, 193.8718938829669867 ) ) ;
#101499 = DIRECTION ( 'NONE',  ( -0.000000000000000000, -1.000000000000000000, -0.000000000000000000 ) ) ;
#101501 = CARTESIAN_POINT ( 'NONE',  ( 8.177817319380210392, 1422.878296244719877, 213.9391555383760135 ) ) ;
#101502 = CARTESIAN_POINT ( 'NONE',  ( 16.62424264452790723, 1524.075132568164463, 237.7045363987409701 ) ) ;
#101503 = CARTESIAN_POINT ( 'NONE',  ( -14.43458679349279983, 1420.584116066620027, 213.5288221046679666 ) ) ;
#101504 = CARTESIAN_POINT ( 'NONE',  ( -0.3973293944376590225, 1418.672797618759887, 184.7148006323309914 ) ) ;
#101505 = EDGE_CURVE ( 'NONE', #22898, #94821, #103492, .T. ) ;
#101506 = CARTESIAN_POINT ( 'NONE',  ( 0.7386049046750020608, 1517.122674412569950, 202.5597518628069906 ) ) ;
#101507 = LINE ( 'NONE', #52663, #44655 ) ;
#101509 = CARTESIAN_POINT ( 'NONE',  ( -11.76598840989999850, 1428.979790717830156, 145.3128034382980047 ) ) ;
#101508 = AXIS2_PLACEMENT_3D ( 'NONE', #89516, #30710, #46987 ) ;
#101510 = CARTESIAN_POINT ( 'NONE',  ( 14.92003712803500015, 1512.136030808819896, 196.7378588390670018 ) ) ;
#101511 = FACE_BOUND ( 'NONE', #67296, .T. ) ;
#101512 = CARTESIAN_POINT ( 'NONE',  ( -35.85012805650530510, 1380.172836987449955, 220.5089525084339925 ) ) ;
#101513 = CARTESIAN_POINT ( 'NONE',  ( 20.69641686248409940, 1508.889931363489723, 228.4591762237180035 ) ) ;
#101515 = VERTEX_POINT ( 'NONE', #48667 ) ;
#101514 = CARTESIAN_POINT ( 'NONE',  ( -21.66469037441770240, 1379.608053137539855, 213.7100242930600018 ) ) ;
#101516 = VERTEX_POINT ( 'NONE', #109118 ) ;
#101517 = CARTESIAN_POINT ( 'NONE',  ( 12.04255032705700046, 1433.784197904049961, 149.9177363570349826 ) ) ;
#101518 = CARTESIAN_POINT ( 'NONE',  ( 9.147507710520001797E-12, 1395.913060387330006, 220.1216245146979986 ) ) ;
#101519 = ORIENTED_EDGE ( 'NONE', *, *, #52162, .F. ) ;
#101520 = CARTESIAN_POINT ( 'NONE',  ( -106.0334448509999987, 1378.913060387289988, 305.5503496670590380 ) ) ;
#101521 = CARTESIAN_POINT ( 'NONE',  ( -25.58986275070000005, 1507.958108862429981, 199.5218862797180179 ) ) ;
#101522 = CARTESIAN_POINT ( 'NONE',  ( 3.983717799080809474, 1515.551844914359890, 206.7919068468160049 ) ) ;
#101524 = DIRECTION ( 'NONE',  ( -1.000000000000000000, 0.000000000000000000, 0.000000000000000000 ) ) ;
#101523 = CARTESIAN_POINT ( 'NONE',  ( 3.252451448209999985, 1444.627347679690047, 200.7572266927390103 ) ) ;
#101525 = CARTESIAN_POINT ( 'NONE',  ( 6.598247897499999404, 1507.806513241529956, 235.4227652625980056 ) ) ;
#101526 = EDGE_CURVE ( 'NONE', #46649, #6784, #15429, .T. ) ;
#101527 = CARTESIAN_POINT ( 'NONE',  ( 6.332098049610000778, 1449.232071652019840, 185.0551591760979875 ) ) ;
#101528 = CARTESIAN_POINT ( 'NONE',  ( -2.845602367250000153, 1416.216739748630062, 191.3599216423980067 ) ) ;
#101529 = CARTESIAN_POINT ( 'NONE',  ( 43.48865799104739693, 1440.913053441320244, 270.3367078669490411 ) ) ;
#101530 = CARTESIAN_POINT ( 'NONE',  ( 3.824658609203980042, 1396.046620409630123, 198.7789396447920183 ) ) ;
#101531 = CARTESIAN_POINT ( 'NONE',  ( 2.500000000000000000, 1419.466030184288229, 140.1627189556986650 ) ) ;
#101532 = CARTESIAN_POINT ( 'NONE',  ( 11.86482925309999992, 1432.250691705679856, 150.3967422869979771 ) ) ;
#101533 = CARTESIAN_POINT ( 'NONE',  ( 5.924854864274999855, 1514.639648807489948, 201.3510662795570170 ) ) ;
#101534 = EDGE_LOOP ( 'NONE', ( #21385, #30890, #63871, #109225, #93862 ) ) ;
#101535 = CARTESIAN_POINT ( 'NONE',  ( 13.30447859826429990, 1435.414542389009966, 150.2505690479650013 ) ) ;
#101536 = EDGE_CURVE ( 'NONE', #34381, #48449, #69575, .T. ) ;
#101537 = ORIENTED_EDGE ( 'NONE', *, *, #31306, .F. ) ;
#101538 = ORIENTED_EDGE ( 'NONE', *, *, #12621, .F. ) ;
#101539 = DIRECTION ( 'NONE',  ( 0.7071067811865474617, -5.176495448588656087E-16, 0.7071067811865474617 ) ) ;
#101540 = CARTESIAN_POINT ( 'NONE',  ( -9.295549619430000021, 1464.969213748930088, 232.6937024852979903 ) ) ;
#101541 = CIRCLE ( 'NONE', #60495, 1.999999999999999556 ) ;
#101542 = CARTESIAN_POINT ( 'NONE',  ( -9.038752695348167165, 1474.281940146342549, 204.2026377629549927 ) ) ;
#101543 = CARTESIAN_POINT ( 'NONE',  ( 6.554764161265000055, 1516.786099423779888, 216.8374711732070068 ) ) ;
#101544 = CARTESIAN_POINT ( 'NONE',  ( -17.17241001986523941, 1511.187213306747708, 179.6185504016045797 ) ) ;
#101545 = CARTESIAN_POINT ( 'NONE',  ( -32.97913964219423377, 1511.187213306747708, 220.2739374644216355 ) ) ;
#101546 = CARTESIAN_POINT ( 'NONE',  ( 13.75903321446010175, 1409.893113914890137, 191.3057351114860296 ) ) ;
#101547 = CARTESIAN_POINT ( 'NONE',  ( 1.889251328982650109E-15, 1379.483856714079820, 206.9293834673690071 ) ) ;
#101548 = ORIENTED_EDGE ( 'NONE', *, *, #11341, .T. ) ;
#101549 = CARTESIAN_POINT ( 'NONE',  ( 6.935457925184999262, 1516.627618683580067, 205.6664679548470076 ) ) ;
#101550 = EDGE_LOOP ( 'NONE', ( #103284, #74544, #98960, #37309 ) ) ;
#101551 = CARTESIAN_POINT ( 'NONE',  ( 20.46181040842379772, 1440.913060387330006, 219.2827885314970331 ) ) ;
#101552 = FACE_OUTER_BOUND ( 'NONE', #29127, .T. ) ;
#101553 = EDGE_CURVE ( 'NONE', #79447, #3400, #107023, .T. ) ;
#101554 = CARTESIAN_POINT ( 'NONE',  ( -12.77781222480000167, 1409.526058053829956, 190.2114732551980296 ) ) ;
#101555 = CARTESIAN_POINT ( 'NONE',  ( 7.908505681124999853, 1514.005261957200219, 216.3707927467769991 ) ) ;
#101556 = EDGE_CURVE ( 'NONE', #5409, #103262, #58750, .T. ) ;
#101558 = ORIENTED_EDGE ( 'NONE', *, *, #11684, .T. ) ;
#101557 = CARTESIAN_POINT ( 'NONE',  ( 0.08492873675443529669, 1416.830086716310007, 227.2254341622459890 ) ) ;
#101559 = CARTESIAN_POINT ( 'NONE',  ( 24.19987966749999941, 1436.809810026820060, 213.5205588716879959 ) ) ;
#101560 = DIRECTION ( 'NONE',  ( -0.000000000000000000, -1.000000000000000000, -0.000000000000000000 ) ) ;
#101562 = CARTESIAN_POINT ( 'NONE',  ( 5.383599734016756955, 1505.915176669089760, 219.4473941718215144 ) ) ;
#101561 = VECTOR ( 'NONE', #30678, 1000.000000000000114 ) ;
#101563 = DIRECTION ( 'NONE',  ( -0.9455185755993178454, 0.000000000000000000, 0.3255681544571539243 ) ) ;
#101564 = ADVANCED_FACE ( 'NONE', ( #15016 ), #67782, .F. ) ;
#101565 = B_SPLINE_CURVE_WITH_KNOTS ( 'NONE', 5,
 ( #15262, #40483, #48355, #56747, #108238, #66273, #6874, #31526, #82495, #48914, #65704, #23116 ),
 .UNSPECIFIED., .F., .F.,
 ( 6, 3, 3, 6 ),
 ( 0.000000000000000000, 0.5248584659502879557, 0.7624265191794091789, 1.000000000000000000 ),
 .UNSPECIFIED. ) ;
#101566 = AXIS2_PLACEMENT_3D ( 'NONE', #81816, #5118, #39274 ) ;
#101567 = CARTESIAN_POINT ( 'NONE',  ( -3.448206916814999801, 1516.904492006980036, 213.1642637479369853 ) ) ;
#101568 = EDGE_CURVE ( 'NONE', #64503, #13404, #94488, .T. ) ;
#101569 = CARTESIAN_POINT ( 'NONE',  ( -2.594792379150919981, 1429.144945495409956, 200.1164755763740004 ) ) ;
#101570 = CARTESIAN_POINT ( 'NONE',  ( -21.73076286450000083, 1509.627908364130008, 189.8044754037979942 ) ) ;
#101571 = AXIS2_PLACEMENT_3D ( 'NONE', #13656, #39445, #48414 ) ;
#101572 = CARTESIAN_POINT ( 'NONE',  ( 6.827653871725639867, 1508.551704612109916, 215.5772939192580111 ) ) ;
#101573 = CARTESIAN_POINT ( 'NONE',  ( 4.625693865015000128, 1517.042661899400173, 211.4082922958669997 ) ) ;
#101574 = CARTESIAN_POINT ( 'NONE',  ( -2.684328089744040469, 1448.124395745682250, 154.7387311340914948 ) ) ;
#101575 = CARTESIAN_POINT ( 'NONE',  ( 13.39865760989999899, 1409.380951821229928, 192.5599167449979916 ) ) ;
#101576 = DIRECTION ( 'NONE',  ( -0.4530882417517332339, -0.7475172582769017415, -0.4857252245503692611 ) ) ;
#101578 = ORIENTED_EDGE ( 'NONE', *, *, #25456, .F. ) ;
#101577 = CARTESIAN_POINT ( 'NONE',  ( -68.63560918429999447, 1386.704837996910101, 263.4658735872590114 ) ) ;
#101579 = CARTESIAN_POINT ( 'NONE',  ( -39.34650272300579843, 1385.185695465040226, 240.9764786771909826 ) ) ;
#101580 = B_SPLINE_CURVE_WITH_KNOTS ( 'NONE', 5,
 ( #99511, #72696, #97866, #81074, #56441, #29568, #4390, #80541, #46408, #3856, #63752, #21141 ),
 .UNSPECIFIED., .F., .F.,
 ( 6, 3, 3, 6 ),
 ( 0.000000000000000000, 0.3427427782409787627, 0.7510084151527882668, 1.000000000000000000 ),
 .UNSPECIFIED. ) ;
#101581 = CARTESIAN_POINT ( 'NONE',  ( 34.21460434910000004, 1445.299194187479998, 250.0133502167980453 ) ) ;
#101582 = CARTESIAN_POINT ( 'NONE',  ( -3.324921645876977472, 1370.249766618262356, 208.0786078478728314 ) ) ;
#101583 = DIRECTION ( 'NONE',  ( -0.8775825618903720926, 0.000000000000000000, -0.4794255386042041156 ) ) ;
#101584 = EDGE_CURVE ( 'NONE', #102960, #12156, #51647, .T. ) ;
#101585 = CARTESIAN_POINT ( 'NONE',  ( -8.796782887879999180, 1468.013265501289879, 190.7844261045989640 ) ) ;
#101586 = CARTESIAN_POINT ( 'NONE',  ( 12.30406194763500061, 1511.972232048389969, 224.1970232450669869 ) ) ;
#101588 = CARTESIAN_POINT ( 'NONE',  ( -7.544821718529999721, 1384.901423591120192, 219.0876899922290022 ) ) ;
#101587 = CARTESIAN_POINT ( 'NONE',  ( -7.329930051325000306, 1516.881930554049859, 216.8399805996670011 ) ) ;
#101589 = CARTESIAN_POINT ( 'NONE',  ( -9.571128596670011035, 1448.740117217580064, 208.7132155754160010 ) ) ;
#101590 = CARTESIAN_POINT ( 'NONE',  ( -106.4551009342630010, 1381.717765542610096, 309.6367472382920027 ) ) ;
#101591 = CIRCLE ( 'NONE', #46259, 1.999999999999998668 ) ;
#101592 = ORIENTED_EDGE ( 'NONE', *, *, #108401, .T. ) ;
#101593 = CARTESIAN_POINT ( 'NONE',  ( -2.292307268505000106, 1516.548716157039962, 202.1882291110970300 ) ) ;
#101594 = EDGE_CURVE ( 'NONE', #85718, #82045, #108958, .T. ) ;
#101595 = CARTESIAN_POINT ( 'NONE',  ( 0.3804419299169999880, 1497.014155752930037, 230.6889103195979942 ) ) ;
#101596 = CARTESIAN_POINT ( 'NONE',  ( 12.87903121499999948, 1419.807609159930053, 223.0107373717980010 ) ) ;
#101597 = CARTESIAN_POINT ( 'NONE',  ( -34.09079054513854601, 1524.667648926078982, 217.9059385276673879 ) ) ;
#101598 = ADVANCED_FACE ( 'NONE', ( #110197 ), #58819, .F. ) ;
#101599 = CARTESIAN_POINT ( 'NONE',  ( -7.818293364874802975, 1461.813659484448408, 203.3506159379348048 ) ) ;
#101600 = CARTESIAN_POINT ( 'NONE',  ( 4.105220072099999840, 1467.927057061790038, 218.2260594483290106 ) ) ;
#101601 = CARTESIAN_POINT ( 'NONE',  ( 5.615853708540889500, 1416.377937261669103, 231.4220595556466264 ) ) ;
#101602 = CARTESIAN_POINT ( 'NONE',  ( 32.02225460880060126, 1435.615636428170092, 135.5615768203190044 ) ) ;
#101603 = CARTESIAN_POINT ( 'NONE',  ( 37.96685885719930553, 1448.851682310969863, 136.3764525557429863 ) ) ;
#101604 = CARTESIAN_POINT ( 'NONE',  ( -8.862056518773441027, 1384.892951007370129, 218.6851137863439760 ) ) ;
#101605 = CARTESIAN_POINT ( 'NONE',  ( -108.8566410550000114, 1386.492030720920184, 297.4136311286590058 ) ) ;
#101606 = CARTESIAN_POINT ( 'NONE',  ( 8.309202182009999049, 1507.619014552029967, 183.0708173328979740 ) ) ;
#101607 = CARTESIAN_POINT ( 'NONE',  ( 3.876688749703430137, 1507.337224526469981, 220.1660795228299889 ) ) ;
#101608 = CARTESIAN_POINT ( 'NONE',  ( -40.03500165408544120, 1450.467487820260430, 269.6105336665062282 ) ) ;
#101609 = EDGE_LOOP ( 'NONE', ( #106480, #56972, #95103, #80959, #24360 ) ) ;
#101610 = CARTESIAN_POINT ( 'NONE',  ( 9.805118623159389202, 1463.039694706869113, 208.9028931574285934 ) ) ;
#101611 = CARTESIAN_POINT ( 'NONE',  ( -42.04495720335383169, 1427.613817688321205, 269.0745714257215013 ) ) ;
#101612 = CARTESIAN_POINT ( 'NONE',  ( 14.22586472836579929, 1422.194230000339758, 190.7685836825260139 ) ) ;
#101613 = CARTESIAN_POINT ( 'NONE',  ( -0.3842696321549999849, 1415.775732286429957, 233.4299280523979974 ) ) ;
#101614 = CARTESIAN_POINT ( 'NONE',  ( 11.87050035490000077, 1500.995002434390017, 208.8930718320189897 ) ) ;
#101615 = CARTESIAN_POINT ( 'NONE',  ( -28.47876014660000266, 1509.161042325230028, 208.9577188500109912 ) ) ;
#101616 = LINE ( 'NONE', #24903, #30634 ) ;
#101617 = CARTESIAN_POINT ( 'NONE',  ( -2.801043665293740048, 1515.551704203360032, 212.9510687676740019 ) ) ;
#101618 = DIRECTION ( 'NONE',  ( 0.000000000000000000, -1.836970198721029688E-16, -1.000000000000000000 ) ) ;
#101619 = CARTESIAN_POINT ( 'NONE',  ( -7.854791674351897512, 1451.394299795975940, 152.9879781448754841 ) ) ;
#101620 = CARTESIAN_POINT ( 'NONE',  ( -16.20819593131889746, 1414.913060387399810, 208.4856282769769962 ) ) ;
#101621 = CARTESIAN_POINT ( 'NONE',  ( 25.38824507410000209, 1436.314429228820245, 137.2293497432980018 ) ) ;
#101622 = CARTESIAN_POINT ( 'NONE',  ( -5.157094080490000287, 1434.836961744490054, 211.6805039011290148 ) ) ;
#101623 = ORIENTED_EDGE ( 'NONE', *, *, #20070, .F. ) ;
#101624 = CARTESIAN_POINT ( 'NONE',  ( 1.003994675819599891, 1414.971993471370070, 191.9916610432980235 ) ) ;
#101625 = CARTESIAN_POINT ( 'NONE',  ( -5.984203303400000173, 1409.122033371430007, 229.9503900095979816 ) ) ;
#101626 = ORIENTED_EDGE ( 'NONE', *, *, #15225, .F. ) ;
#101627 = ORIENTED_EDGE ( 'NONE', *, *, #72062, .F. ) ;
#101628 = CARTESIAN_POINT ( 'NONE',  ( 0.6898828221520181270, 1435.696354552260118, 227.5721478921569769 ) ) ;
#101629 = CARTESIAN_POINT ( 'NONE',  ( -15.30505509804103070, 1416.034713203068122, 206.6286703179388553 ) ) ;
#101631 = CARTESIAN_POINT ( 'NONE',  ( -7.245608758899999557, 1458.975067297229998, 211.8132954410479840 ) ) ;
#101630 = CARTESIAN_POINT ( 'NONE',  ( 2.140393166329999985, 1456.253627881090097, 219.1100769117989842 ) ) ;
#101632 = CARTESIAN_POINT ( 'NONE',  ( -8.557074290199999211, 1446.797689270289993, 213.4441513527789880 ) ) ;
#101633 = CARTESIAN_POINT ( 'NONE',  ( 4.144234488730229593, 1424.436899653439923, 184.8007390397289953 ) ) ;
#101634 = CARTESIAN_POINT ( 'NONE',  ( -12.31045119098629925, 1378.376187953739873, 209.7947064970520046 ) ) ;
#101635 = CARTESIAN_POINT ( 'NONE',  ( -2.813926873014771068, 1419.840084512981548, 186.1457758105879634 ) ) ;
#101636 = VECTOR ( 'NONE', #8706, 1000.000000000000000 ) ;
#101637 = CARTESIAN_POINT ( 'NONE',  ( 7.451350174509999924, 1424.542899935769810, 212.3981519012789931 ) ) ;
#101638 = CARTESIAN_POINT ( 'NONE',  ( -24.09223960049999747, 1438.023760012700222, 211.8323666990379763 ) ) ;
#101639 = CARTESIAN_POINT ( 'NONE',  ( -3.296219135334409689, 1454.279253091320015, 199.1722461497759866 ) ) ;
#101640 = CARTESIAN_POINT ( 'NONE',  ( 2.489956268369999837, 1451.499402758130145, 183.7031856439980118 ) ) ;
#101641 = AXIS2_PLACEMENT_3D ( 'NONE', #41932, #82817, #102375 ) ;
#101642 = CARTESIAN_POINT ( 'NONE',  ( 6.890671329650879251, 1363.865351280181812, 209.6218459617148824 ) ) ;
#101643 = CARTESIAN_POINT ( 'NONE',  ( -20.59181392461939808, 1509.749895152629961, 230.9387993182432126 ) ) ;
#101645 = ORIENTED_EDGE ( 'NONE', *, *, #39138, .F. ) ;
#101644 = CARTESIAN_POINT ( 'NONE',  ( 5.485824899879999883, 1494.971430001190129, 220.2122618358989712 ) ) ;
#101646 = ORIENTED_EDGE ( 'NONE', *, *, #48750, .T. ) ;
#101647 = CARTESIAN_POINT ( 'NONE',  ( -11.76350460807940124, 1426.962723605229939, 145.9979234665020158 ) ) ;
#101648 = AXIS2_PLACEMENT_3D ( 'NONE', #40450, #49424, #66789 ) ;
#101649 = CARTESIAN_POINT ( 'NONE',  ( 7.458082240553069120, 1510.848430439774347, 202.9305636724023429 ) ) ;
#101650 = CARTESIAN_POINT ( 'NONE',  ( -3.530738011219999528, 1473.488020316229949, 270.3906828180979574 ) ) ;
#101651 = CARTESIAN_POINT ( 'NONE',  ( -110.0628587348610097, 1384.913582352849971, 296.9513039175640188 ) ) ;
#101652 = CARTESIAN_POINT ( 'NONE',  ( -104.0419184278224094, 1314.643966242388842, 309.3341892202922168 ) ) ;
#101653 = CARTESIAN_POINT ( 'NONE',  ( 22.58439900540000167, 1519.913060387329779, 209.1218459616979999 ) ) ;
#101654 = CARTESIAN_POINT ( 'NONE',  ( -8.168610837440001049, 1384.459582517680019, 199.6726098237590179 ) ) ;
#101655 =( NAMED_UNIT ( * ) SI_UNIT ( $, .STERADIAN. ) SOLID_ANGLE_UNIT ( ) );
#101656 = CARTESIAN_POINT ( 'NONE',  ( -18.71266994490000002, 1408.913060387329779, 208.1472103593870031 ) ) ;
#101657 = B_SPLINE_CURVE_WITH_KNOTS ( 'NONE', 3,
 ( #19344, #20445, #78726, #53544, #96635, #28322 ),
 .UNSPECIFIED., .F., .F.,
 ( 4, 2, 4 ),
 ( -6.000000023196556560E-08, 0.0005507591112004208908, 0.001101578222401073878 ),
 .UNSPECIFIED. ) ;
#101658 = CARTESIAN_POINT ( 'NONE',  ( 7.818221670759999853, 1367.736483592530021, 207.6218459616989946 ) ) ;
#101659 = CARTESIAN_POINT ( 'NONE',  ( -9.220308107448930812, 1448.515117430399869, 210.2021542620989862 ) ) ;
#101660 = CARTESIAN_POINT ( 'NONE',  ( -10.53083746087449946, 1407.392537625429895, 269.4602285795690477 ) ) ;
#101661 = CARTESIAN_POINT ( 'NONE',  ( -13.23941283839999983, 1435.104810100029908, 149.9220718869979976 ) ) ;
#101662 = ORIENTED_EDGE ( 'NONE', *, *, #108912, .T. ) ;
#101663 = CARTESIAN_POINT ( 'NONE',  ( -4.327091944037070093, 1515.154796665630101, 209.3803870859530036 ) ) ;
#101664 = CARTESIAN_POINT ( 'NONE',  ( 13.99038557849999975, 1444.015975867750058, 189.3175554311980022 ) ) ;
#101665 = ORIENTED_EDGE ( 'NONE', *, *, #30216, .F. ) ;
#101666 = ORIENTED_EDGE ( 'NONE', *, *, #2868, .F. ) ;
#101667 = CARTESIAN_POINT ( 'NONE',  ( 4.902054967530699692, 1422.428228210868156, 184.3467753365531507 ) ) ;
#101668 = CARTESIAN_POINT ( 'NONE',  ( 5.314610460026229610, 1424.245163613919885, 193.3438872810020257 ) ) ;
#101669 = CIRCLE ( 'NONE', #28406, 1.000000000000000888 ) ;
#101670 = CARTESIAN_POINT ( 'NONE',  ( 2.297085715815000206, 1516.718889242609976, 213.1486234561869821 ) ) ;
#101671 = CARTESIAN_POINT ( 'NONE',  ( 5.496430521294999316, 1510.805212328559946, 216.6808561328170128 ) ) ;
#101672 = B_SPLINE_CURVE_WITH_KNOTS ( 'NONE', 3,
 ( #35052, #16025, #67577, #42350, #58617, #110654, #9310 ),
 .UNSPECIFIED., .F., .F.,
 ( 4, 3, 4 ),
 ( 0.000000000000000000, 0.3299121248754509628, 0.5294136330519999545 ),
 .UNSPECIFIED. ) ;
#101673 = DIRECTION ( 'NONE',  ( -1.755985294532469921E-16, 1.000000000000000000, -1.338183447452831989E-16 ) ) ;
#101674 = ORIENTED_EDGE ( 'NONE', *, *, #103611, .T. ) ;
#101675 = CARTESIAN_POINT ( 'NONE',  ( -113.4000000000000057, 1379.413060387289988, 304.2218459572590064 ) ) ;
#101676 =( BOUNDED_CURVE ( )  B_SPLINE_CURVE ( 3, ( #47983, #67000, #13797, #56943 ),
 .UNSPECIFIED., .F., .F. ) 
 B_SPLINE_CURVE_WITH_KNOTS ( ( 4, 4 ),
 ( 1.036132151715712713, 2.105460582192766772 ),
 .UNSPECIFIED. ) 
 CURVE ( )  GEOMETRIC_REPRESENTATION_ITEM ( )  RATIONAL_B_SPLINE_CURVE ( ( 1.000000000000000000, 0.9069598517500692125, 0.9069598517500692125, 1.000000000000000000 ) ) 
 REPRESENTATION_ITEM ( '' )  );
#101677 = CARTESIAN_POINT ( 'NONE',  ( 7.326795523374999952, 1516.760434454289907, 203.3416138547669902 ) ) ;
#101678 = ADVANCED_FACE ( 'NONE', ( #68782 ), #108851, .F. ) ;
#101679 = CARTESIAN_POINT ( 'NONE',  ( -27.50534346099999894, 1509.159577300329829, 204.1676302040880273 ) ) ;
#101680 = EDGE_CURVE ( 'NONE', #35166, #4524, #48046, .T. ) ;
#101681 = CARTESIAN_POINT ( 'NONE',  ( -1.328495774590000122, 1467.878694257229881, 230.3318996346980043 ) ) ;
#101682 = CARTESIAN_POINT ( 'NONE',  ( -34.42078214483079535, 1384.567160501399940, 208.3171832722069894 ) ) ;
#101683 = CARTESIAN_POINT ( 'NONE',  ( -2.751920914360000303, 1408.825585090129834, 195.2201059653979769 ) ) ;
#101684 = CARTESIAN_POINT ( 'NONE',  ( -8.588755447433969792, 1437.818850531529961, 207.9413692731380081 ) ) ;
#101686 = EDGE_LOOP ( 'NONE', ( #73283, #74156, #26682, #91511, #82836 ) ) ;
#101685 = CARTESIAN_POINT ( 'NONE',  ( 15.45308517192525599, 1506.474306125858902, 193.4392981697745029 ) ) ;
#101687 = CARTESIAN_POINT ( 'NONE',  ( 3.925166330978474338, 1441.144975113518058, 217.4787537044992121 ) ) ;
#101688 = CARTESIAN_POINT ( 'NONE',  ( 26.99303384979999976, 1488.687911583929917, 211.6160553286979962 ) ) ;
#101689 = CARTESIAN_POINT ( 'NONE',  ( -68.70880675088680789, 1379.747766871069871, 280.3821654378152175 ) ) ;
#101690 = CARTESIAN_POINT ( 'NONE',  ( 10.56340574544989863, 1460.179522302520127, 206.3975810254339933 ) ) ;
#101691 = CARTESIAN_POINT ( 'NONE',  ( -13.96015163203214549, 1516.660421270692041, 191.9693043941119299 ) ) ;
#101692 = CARTESIAN_POINT ( 'NONE',  ( -24.66052414600000020, 1442.238365636329945, 210.7405400769080188 ) ) ;
#101693 = CARTESIAN_POINT ( 'NONE',  ( 3.462620818104999998, 1516.938330505699923, 211.6001527901769919 ) ) ;
#101694 = AXIS2_PLACEMENT_3D ( 'NONE', #87693, #53546, #79842 ) ;
#101695 = CARTESIAN_POINT ( 'NONE',  ( -68.69440785229998880, 1379.747830596759968, 279.9872465871590066 ) ) ;
#101696 = EDGE_CURVE ( 'NONE', #74476, #55773, #102403, .T. ) ;
#101697 = CARTESIAN_POINT ( 'NONE',  ( -15.20812112729999832, 1415.576510420729846, 226.8726329618980060 ) ) ;
#101698 = CARTESIAN_POINT ( 'NONE',  ( 18.80339027203730140, 1425.953307585449693, 225.0197318394450008 ) ) ;
#101699 = CARTESIAN_POINT ( 'NONE',  ( -1.715109485185000171, 1516.963431999339946, 208.3866188148990091 ) ) ;
#101700 = ORIENTED_EDGE ( 'NONE', *, *, #48220, .T. ) ;
#101701 = CARTESIAN_POINT ( 'NONE',  ( 33.91376666158910069, 1435.681799711289841, 142.5056097149810057 ) ) ;
#101702 = CARTESIAN_POINT ( 'NONE',  ( -10.96160898770000180, 1471.053908682290057, 208.7203235810210060 ) ) ;
#101703 =( BOUNDED_SURFACE ( )  B_SPLINE_SURFACE ( 3, 2, ( 
 ( #103745, #61233, #95348 ),
 ( #86940, #10231, #33767 ),
 ( #67963, #42537, #14567 ),
 ( #76143, #67757, #75059 ),
 ( #41994, #108639, #110288 ),
 ( #58795, #15110, #66119 ) ),
 .UNSPECIFIED., .F., .F., .T. ) 
 B_SPLINE_SURFACE_WITH_KNOTS ( ( 4, 2, 4 ),
 ( 3, 3 ),
 ( -2.081668171172168513E-17, 0.001312027981647304791, 0.002624055963294630398 ),
 ( 0.000000000000000000, 1.000000000000000000 ),
 .UNSPECIFIED. ) 
 GEOMETRIC_REPRESENTATION_ITEM ( )  RATIONAL_B_SPLINE_SURFACE ( (
 ( 1.000000000000000000, 0.9376006582765912256, 1.000000000000000000),
 ( 1.000000000000000000, 0.9569320108022220106, 1.000000000000000000),
 ( 1.000000000000000000, 0.9725743441619391083, 1.000000000000000000),
 ( 1.000000000000000000, 0.9942095667135121273, 1.000000000000000000),
 ( 1.000000000000000000, 1.000043666450747049, 1.000000000000000000),
 ( 1.000000000000000000, 1.000000000000000000, 1.000000000000000000) ) ) 
 REPRESENTATION_ITEM ( '' )  SURFACE ( )  );
#101704 = CARTESIAN_POINT ( 'NONE',  ( -3.078458293700000237, 1385.332091261079995, 218.5458417419390003 ) ) ;
#101705 = VERTEX_POINT ( 'NONE', #62611 ) ;
#101706 = CARTESIAN_POINT ( 'NONE',  ( -3.141363374988426660, 1525.159177407155767, 241.5359609335856419 ) ) ;
#101707 = CARTESIAN_POINT ( 'NONE',  ( -22.72723102240144044, 1509.727045134374066, 228.1120738395736964 ) ) ;
#101708 = B_SPLINE_SURFACE_WITH_KNOTS ( 'NONE', 5, 5, ( 
 ( #104412, #85957, #69741, #34450, #45088, #103282, #103860, #28255, #104966, #94336, #27705, #87625 ),
 ( #44517, #78104, #26589, #54049, #88175, #62448, #68626, #102728, #1405, #27161, #9257, #53481 ),
 ( #43416, #77566, #872, #69176, #9796, #35546, #94912, #51817, #36116, #60786, #18186, #78663 ),
 ( #52924, #61345, #87058, #86502, #10913, #95465, #79228, #19279, #34996, #10345, #1981, #77019 ),
 ( #61892, #96008, #2537, #36661, #70855, #96571, #19844, #325, #73442, #31969, #58288, #90208 ),
 ( #14051, #20388, #97119, #81811, #71411, #105526, #22432, #63013, #56083, #40919, #79782, #13492 ),
 ( #74546, #65594, #28815, #92413, #15148, #47683, #48240, #23562, #3087, #24099, #14613, #37215 ),
 ( #5113, #48800, #82923, #40365, #108118, #73988, #30862, #6214, #49337, #39269, #31412, #109247 ),
 ( #107576, #65037, #99154, #6759, #66161, #56635, #90770, #82383, #108678, #100282, #99707, #57756 ),
 ( #5682, #39826, #91875, #23000, #100811, #83464, #57204, #45642, #91328, #75099, #32531, #66702 ),
 ( #17902, #52099, #34175, #1149, #42033, #8969, #67254, #59957, #103016, #25201, #26312, #7324 ),
 ( #101348, #50449, #43141, #41488, #103583, #75648, #86229, #35280, #50991, #9520, #85120, #26885 ) ),
 .UNSPECIFIED., .F., .F., .F.,
 ( 6, 3, 3, 6 ),
 ( 6, 3, 3, 6 ),
 ( 6.265790646049559598, 6.759971547659999302, 7.748257017729999419, 8.343532910357360777 ),
 ( -4.426502619661019944E-05, 0.3262962046579999664, 0.9788886139739999548, 1.447530370220490026 ),
 .UNSPECIFIED. ) ;
#101709 = CARTESIAN_POINT ( 'NONE',  ( 10.11876717485079880, 1468.998983517520173, 232.5874711531799903 ) ) ;
#101710 = CARTESIAN_POINT ( 'NONE',  ( 0.000000000000000000, 1384.913060387289988, 209.1218459572589836 ) ) ;
#101711 = CARTESIAN_POINT ( 'NONE',  ( 15.32773529925650102, 1420.119835273649869, 210.6256678854140034 ) ) ;
#101712 = B_SPLINE_CURVE_WITH_KNOTS ( 'NONE', 3,
 ( #7241, #22351, #100196, #57671, #82292, #56552, #48157, #5592, #68283, #77218, #104054, #76647, #8327, #95109, #18374, #1620, #1069, #35197, #76103, #9445, #17258 ),
 .UNSPECIFIED., .F., .F.,
 ( 4, 2, 2, 2, 1, 1, 1, 1, 1, 2, 2, 2, 4 ),
 ( 0.000000000000000000, 0.2499999999997003508, 0.3749999999995501931, 0.4374999999994747535, 0.4687499999994392819, 0.4843749999994212962, 0.4921874999994121369, 0.4960937499994074740, 0.4980468749994027000, 0.4990234374994019229, 0.4999999999994011457, 0.7499999999997005729, 1.000000000000000000 ),
 .UNSPECIFIED. ) ;
#101713 = CARTESIAN_POINT ( 'NONE',  ( 4.297657077759999389, 1487.299056241089829, 198.3739788318989952 ) ) ;
#101714 = CARTESIAN_POINT ( 'NONE',  ( 4.002785782343220689, 1430.446709099730015, 217.7271167850740028 ) ) ;
#101715 = CARTESIAN_POINT ( 'NONE',  ( 4.225886903421089968, 1441.568770927039850, 166.1380412392189783 ) ) ;
#101717 = CARTESIAN_POINT ( 'NONE',  ( -11.25901873334290038, 1500.172003390719965, 210.8567363214919794 ) ) ;
#101716 = CARTESIAN_POINT ( 'NONE',  ( 6.559168636745000391, 1516.960844870249957, 214.1244393295569921 ) ) ;
#101718 = AXIS2_PLACEMENT_3D ( 'NONE', #49233, #37328, #12114 ) ;
#101719 = CARTESIAN_POINT ( 'NONE',  ( -8.865470775637810164, 1385.143464112529955, 218.6765624161500057 ) ) ;
#101720 = CARTESIAN_POINT ( 'NONE',  ( 6.556022194504999234, 1516.833525648419936, 216.0623193043769845 ) ) ;
#101721 = ORIENTED_EDGE ( 'NONE', *, *, #9062, .T. ) ;
#101722 = CARTESIAN_POINT ( 'NONE',  ( -12.27010798569999928, 1416.835808384130132, 194.6641343254979972 ) ) ;
#101723 = B_SPLINE_SURFACE_WITH_KNOTS ( 'NONE', 5, 5, ( 
 ( #21505, #56247, #55719, #90376, #55167, #90938 ),
 ( #38873, #38327, #72506, #73052, #107193, #81977 ),
 ( #64670, #5849, #99324, #13654, #47844, #105556 ),
 ( #5285, #39441, #16411, #8034, #108846, #40539 ),
 ( #24277, #108296, #75806, #110503, #91502, #7489 ),
 ( #92048, #50605, #6934, #49514, #85284, #41091 ) ),
 .UNSPECIFIED., .F., .F., .F.,
 ( 6, 6 ),
 ( 6, 6 ),
 ( 7.053188784610000539, 25.42450307460000047 ),
 ( 0.000000000000000000, 2.000000000000000000 ),
 .UNSPECIFIED. ) ;
#101724 = EDGE_CURVE ( 'NONE', #18362, #4497, #63575, .T. ) ;
#101725 = CARTESIAN_POINT ( 'NONE',  ( -17.20794664139999952, 1420.221446635479879, 203.8085880389089937 ) ) ;
#101726 = EDGE_LOOP ( 'NONE', ( #108531, #17652, #109407, #56822 ) ) ;
#101727 = VECTOR ( 'NONE', #17287, 1000.000000000000114 ) ;
#101728 = CARTESIAN_POINT ( 'NONE',  ( -16.80827233337889837, 1508.551704408389924, 212.8354810807049944 ) ) ;
#101729 = AXIS2_PLACEMENT_3D ( 'NONE', #59353, #17286, #59900 ) ;
#101730 = CARTESIAN_POINT ( 'NONE',  ( 1.742416831430000146, 1474.343050638090062, 219.6228428829990094 ) ) ;
#101731 = EDGE_CURVE ( 'NONE', #102747, #66886, #4827, .T. ) ;
#101732 = FACE_OUTER_BOUND ( 'NONE', #87234, .T. ) ;
#101733 = CARTESIAN_POINT ( 'NONE',  ( -1.804213505890000180, 1410.351307731129964, 186.0507930254979954 ) ) ;
#101734 = DIRECTION ( 'NONE',  ( 0.000000000000000000, -1.000000000000000000, 0.000000000000000000 ) ) ;
#101735 = CARTESIAN_POINT ( 'NONE',  ( -23.61227025210000008, 1435.322036687620084, 137.2858276859979867 ) ) ;
#101736 = CARTESIAN_POINT ( 'NONE',  ( 18.90690566160000330, 1416.819756528429934, 210.0263056463570024 ) ) ;
#101737 = CARTESIAN_POINT ( 'NONE',  ( 5.312679136500000787, 1493.059131431590231, 218.8466398904690209 ) ) ;
#101738 = CARTESIAN_POINT ( 'NONE',  ( 16.66701395081345538, 1523.530870145311155, 180.4846106723501578 ) ) ;
#101739 = CARTESIAN_POINT ( 'NONE',  ( -4.967309476820000569, 1440.444625599219989, 150.3089546883979892 ) ) ;
#101740 = CARTESIAN_POINT ( 'NONE',  ( 41.26114072546569389, 1440.913060355679818, 261.0027848306349938 ) ) ;
#101742 = FACE_OUTER_BOUND ( 'NONE', #87255, .T. ) ;
#101741 = CARTESIAN_POINT ( 'NONE',  ( -11.19185250109059915, 1418.956138653949893, 197.9931542539910083 ) ) ;
#101743 = CARTESIAN_POINT ( 'NONE',  ( 13.24083268210000064, 1429.096486322929877, 222.2418765336980186 ) ) ;
#101744 = ORIENTED_EDGE ( 'NONE', *, *, #95276, .T. ) ;
#101745 = VERTEX_POINT ( 'NONE', #44676 ) ;
#101746 = CARTESIAN_POINT ( 'NONE',  ( 1.547740551532809983, 1416.449138223310001, 190.2779371676239748 ) ) ;
#101747 = CARTESIAN_POINT ( 'NONE',  ( -19.66414603918734727, 1485.273356660164609, 190.3047461115721433 ) ) ;
#101748 = CARTESIAN_POINT ( 'NONE',  ( -27.89933041909999645, 1509.196990922029954, 210.7395031776179906 ) ) ;
#101749 = CARTESIAN_POINT ( 'NONE',  ( 17.68237282055029880, 1517.151704408390060, 212.5589510568480023 ) ) ;
#101750 = AXIS2_PLACEMENT_3D ( 'NONE', #67096, #91717, #13890 ) ;
#101751 = CARTESIAN_POINT ( 'NONE',  ( 26.27087616454108598, 1509.943490157906808, 223.6899730734042748 ) ) ;
#101752 = CARTESIAN_POINT ( 'NONE',  ( -18.86688640473562373, 1512.187213306747481, 237.4611898188522332 ) ) ;
#101753 = CARTESIAN_POINT ( 'NONE',  ( 20.75865085201310123, 1455.056320380349916, 207.3304550445770076 ) ) ;
#101754 = CARTESIAN_POINT ( 'NONE',  ( -63.46805869144479573, 1383.792271846660014, 286.2010029998429559 ) ) ;
#101755 = CARTESIAN_POINT ( 'NONE',  ( 20.63450640349999787, 1452.049652659229878, 144.1338810006979827 ) ) ;
#101756 = CARTESIAN_POINT ( 'NONE',  ( -28.45107852102471924, 1509.906593941153687, 212.2021872825625621 ) ) ;
#101757 = CARTESIAN_POINT ( 'NONE',  ( 11.00856587417569976, 1491.731810436480146, 211.0639928105959768 ) ) ;
#101759 = EDGE_LOOP ( 'NONE', ( #33093, #88092, #74893, #19003 ) ) ;
#101758 = CARTESIAN_POINT ( 'NONE',  ( -0.9024754025550010272, 1457.070408835690159, 219.3409596864989908 ) ) ;
#101760 = CARTESIAN_POINT ( 'NONE',  ( 31.50799703744294789, 1524.382868172863937, 216.4233194664825248 ) ) ;
#101761 = CARTESIAN_POINT ( 'NONE',  ( -61.91320719539999828, 1380.491709420169855, 255.2400922398589955 ) ) ;
#101762 = CARTESIAN_POINT ( 'NONE',  ( 19.77969251879999746, 1507.818093401829856, 229.2755605921979907 ) ) ;
#101763 = VERTEX_POINT ( 'NONE', #47966 ) ;
#101764 = ORIENTED_EDGE ( 'NONE', *, *, #93484, .T. ) ;
#101765 = CARTESIAN_POINT ( 'NONE',  ( 16.84231947438349764, 1508.205205765930032, 231.2670381483619906 ) ) ;
#101766 = CARTESIAN_POINT ( 'NONE',  ( -21.11353872800000175, 1504.854732156090222, 213.2197078311189955 ) ) ;
#101767 = CARTESIAN_POINT ( 'NONE',  ( -15.95383389570000077, 1506.798305147730161, 224.6865364803979901 ) ) ;
#101768 = CARTESIAN_POINT ( 'NONE',  ( 17.17241001986483795, 1511.187213306747708, 179.6185504016043240 ) ) ;
#101769 = CARTESIAN_POINT ( 'NONE',  ( -7.203791267549999766, 1462.997894367589879, 202.2063197434089830 ) ) ;
#101770 = CARTESIAN_POINT ( 'NONE',  ( -108.7044653689999905, 1381.736054483690168, 297.8421293474590357 ) ) ;
#101771 = CARTESIAN_POINT ( 'NONE',  ( -21.84020450211261277, 1523.481610118012895, 234.9798068777343474 ) ) ;
#101772 = CARTESIAN_POINT ( 'NONE',  ( -20.87069991009999725, 1506.658021081189872, 214.5368842940590071 ) ) ;
#101773 = CARTESIAN_POINT ( 'NONE',  ( -16.03202129173239854, 1508.551704408389924, 213.7937094156460205 ) ) ;
#101774 = CARTESIAN_POINT ( 'NONE',  ( 3.738841759920000118, 1409.547781092230025, 186.1588687207980115 ) ) ;
#101775 = CARTESIAN_POINT ( 'NONE',  ( 12.91074692609340069, 1420.834906917639955, 222.4031488991760170 ) ) ;
#101776 = CARTESIAN_POINT ( 'NONE',  ( -8.126234285584999384, 1514.923664147150021, 202.9950997886369635 ) ) ;
#101777 = CARTESIAN_POINT ( 'NONE',  ( -2.704923982728260068, 1440.770577247940082, 166.9241038796999987 ) ) ;
#101778 = AXIS2_PLACEMENT_3D ( 'NONE', #71216, #45999, #105340 ) ;
#101779 = CARTESIAN_POINT ( 'NONE',  ( -2.706741865136000236, 1451.733424401669936, 184.7389962060059929 ) ) ;
#101780 = CARTESIAN_POINT ( 'NONE',  ( 0.4595755069420000005, 1467.109512415230029, 235.5974104456980172 ) ) ;
#101781 = VERTEX_POINT ( 'NONE', #31703 ) ;
#101782 = B_SPLINE_SURFACE_WITH_KNOTS ( 'NONE', 5, 5, ( 
 ( #81638, #88949, #98451, #90600, #56467, #21165 ),
 ( #4415, #48629, #55373, #82760, #72720, #21720 ),
 ( #6052, #39084, #98991, #71658, #73263, #107402 ),
 ( #30698, #22266, #91708, #43939, #1387, #60764 ),
 ( #76995, #14982, #43393, #69722, #26568, #51229 ),
 ( #34972, #94315, #77543, #847, #42834, #301 ),
 ( #65989, #95444, #9774, #34428, #18708, #17594 ),
 ( #35528, #68601, #52361, #78083, #103840, #60196 ),
 ( #66540, #69155, #49178, #85933, #18164, #85362 ) ),
 .UNSPECIFIED., .F., .F., .F.,
 ( 6, 3, 6 ),
 ( 6, 6 ),
 ( 3.153842328722349819, 5.422189802880000187, 7.690534356440440256 ),
 ( -0.0004137068776518209689, 2.000000000000000000 ),
 .UNSPECIFIED. ) ;
#101783 = CARTESIAN_POINT ( 'NONE',  ( -3.189845314219999395, 1471.643321501789842, 187.3778031497989787 ) ) ;
#101784 = CARTESIAN_POINT ( 'NONE',  ( 11.60004869885206880, 1428.983126981192754, 137.0999999980979851 ) ) ;
#101785 = PLANE ( 'NONE',  #107015 ) ;
#101786 = CARTESIAN_POINT ( 'NONE',  ( 18.89905511659999959, 1416.828040475729949, 210.6687957193779823 ) ) ;
#101787 = CARTESIAN_POINT ( 'NONE',  ( -8.861662123853877304, 1384.878099886156406, 218.6849989278500459 ) ) ;
#101788 = CIRCLE ( 'NONE', #62532, 1.999998248449969873 ) ;
#101789 = CARTESIAN_POINT ( 'NONE',  ( -4.384471102255430024E-11, 1469.871482233950019, 253.6786592827409663 ) ) ;
#101790 = CARTESIAN_POINT ( 'NONE',  ( -13.19474177440000062, 1503.345007237690197, 208.6791437603130248 ) ) ;
#101791 = CARTESIAN_POINT ( 'NONE',  ( -2.093884640795049545, 1421.271540113659967, 193.7238421870019636 ) ) ;
#101792 = CARTESIAN_POINT ( 'NONE',  ( -1.263571840090000009, 1417.414027388429986, 235.3744744869979968 ) ) ;
#101793 = CARTESIAN_POINT ( 'NONE',  ( -2.624961820489999820, 1475.614191382290073, 198.7376068992990099 ) ) ;
#101794 = CARTESIAN_POINT ( 'NONE',  ( -108.0120647289999880, 1388.816386314980036, 310.0183359962589975 ) ) ;
#101795 = CARTESIAN_POINT ( 'NONE',  ( -0.1926505725269009039, 1486.021514730641229, 181.8289695123539786 ) ) ;
#101796 = CARTESIAN_POINT ( 'NONE',  ( 0.05823133897708447637, 1360.390585217553962, 210.6218459616991936 ) ) ;
#101797 = CARTESIAN_POINT ( 'NONE',  ( -45.95009646603779885, 1438.847167528959972, 268.4985374090409778 ) ) ;
#101798 = CARTESIAN_POINT ( 'NONE',  ( 13.46016752625740054, 1508.422424633640048, 233.3101797675730040 ) ) ;
#101799 = CARTESIAN_POINT ( 'NONE',  ( -8.571317710789999822, 1424.360885749340014, 206.8919365348089912 ) ) ;
#101800 = CARTESIAN_POINT ( 'NONE',  ( 3.455495833855000143, 1516.939877939420057, 209.1085718841020196 ) ) ;
#101801 = CYLINDRICAL_SURFACE ( 'NONE', #66291, 1.999999999999999556 ) ;
#101802 = CARTESIAN_POINT ( 'NONE',  ( -6.672894824142502124, 1470.955718715978492, 216.7252699277640602 ) ) ;
#101803 = CARTESIAN_POINT ( 'NONE',  ( 7.454189929035849538, 1426.129717880560065, 212.4394750011670112 ) ) ;
#101804 = CIRCLE ( 'NONE', #76819, 2.000000000000002220 ) ;
#101805 = CARTESIAN_POINT ( 'NONE',  ( -26.56969918195860103, 1451.519818403060071, 136.0976908218790129 ) ) ;
#101806 = ORIENTED_EDGE ( 'NONE', *, *, #43355, .F. ) ;
#101807 = CARTESIAN_POINT ( 'NONE',  ( 7.968534124619999904E-12, 1418.241830526630110, 231.9989422678980304 ) ) ;
#101809 = CARTESIAN_POINT ( 'NONE',  ( -15.29936285970580023, 1512.951873711589997, 222.9557858335909941 ) ) ;
#101808 = CARTESIAN_POINT ( 'NONE',  ( -11.08420618087970055, 1492.086055949669799, 207.0911962512699915 ) ) ;
#101810 = CARTESIAN_POINT ( 'NONE',  ( -2.243003920383240146, 1419.511934557899849, 185.9793846685319920 ) ) ;
#101811 = DIRECTION ( 'NONE',  ( -0.01594118961724032973, -0.9969860201949399814, 0.07592597717146747083 ) ) ;
#101812 = CARTESIAN_POINT ( 'NONE',  ( 7.893069735660001029, 1424.490648431219824, 211.8460496558390105 ) ) ;
#101813 = CARTESIAN_POINT ( 'NONE',  ( 2.500000000000000000, 1448.894380913990062, 182.3534011237979939 ) ) ;
#101814 = CARTESIAN_POINT ( 'NONE',  ( 18.20258715539999983, 1429.723789929190161, 209.1218459616989946 ) ) ;
#101815 = ORIENTED_EDGE ( 'NONE', *, *, #50282, .F. ) ;
#101816 = CARTESIAN_POINT ( 'NONE',  ( -0.6031919701292450808, 1409.206624385790064, 270.3713721421309515 ) ) ;
#101817 = CARTESIAN_POINT ( 'NONE',  ( 6.346443515254469148, 1418.380699742210254, 232.6272524216070110 ) ) ;
#101818 = CARTESIAN_POINT ( 'NONE',  ( 8.132247801209091520, 1436.307234911819933, 206.3069409763359943 ) ) ;
#101819 = VERTEX_POINT ( 'NONE', #91056 ) ;
#101820 = ORIENTED_EDGE ( 'NONE', *, *, #41416, .F. ) ;
#101821 = DIRECTION ( 'NONE',  ( -5.980589973904019347E-17, 1.000000000000000000, -1.736889445713099699E-16 ) ) ;
#101822 = ORIENTED_EDGE ( 'NONE', *, *, #78971, .T. ) ;
#101823 = PLANE ( 'NONE',  #95646 ) ;
#101824 = CIRCLE ( 'NONE', #80368, 6.842541678089994583 ) ;
#101825 = CARTESIAN_POINT ( 'NONE',  ( -2.409586283469999923, 1426.663880916129983, 144.1938086916980239 ) ) ;
#101826 = CARTESIAN_POINT ( 'NONE',  ( -18.58858086442659996, 1429.707054241190008, 194.6563974369069854 ) ) ;
#101827 = CARTESIAN_POINT ( 'NONE',  ( 3.116136652999580203, 1509.034536824670113, 213.6092057033540073 ) ) ;
#101828 = ADVANCED_FACE ( 'NONE', ( #72102 ), #26485, .T. ) ;
#101829 = CARTESIAN_POINT ( 'NONE',  ( 36.94315808685519187, 1461.917959960340113, 268.5012768873260143 ) ) ;
#101830 = CARTESIAN_POINT ( 'NONE',  ( -10.98953490978640168, 1391.913060387049882, 205.9689414614919940 ) ) ;
#101831 = CARTESIAN_POINT ( 'NONE',  ( -17.21301869208722124, 1422.369372973762665, 226.6884971801745792 ) ) ;
#101832 = CARTESIAN_POINT ( 'NONE',  ( 4.997250153905000047, 1516.727068157269969, 205.8570671527170077 ) ) ;
#101833 = ORIENTED_EDGE ( 'NONE', *, *, #39442, .F. ) ;
#101834 = CARTESIAN_POINT ( 'NONE',  ( 18.23897009793844859, 1459.291141722666453, 227.8679119275740561 ) ) ;
#101835 = CARTESIAN_POINT ( 'NONE',  ( 14.98757060048970047, 1513.799047785590119, 194.4265915126370032 ) ) ;
#101836 = CARTESIAN_POINT ( 'NONE',  ( 15.48933771679000060, 1431.961443115730162, 219.1762183192749944 ) ) ;
#101837 = ORIENTED_EDGE ( 'NONE', *, *, #108164, .F. ) ;
#101839 = CIRCLE ( 'NONE', #85793, 1.999999999999999556 ) ;
#101838 = CARTESIAN_POINT ( 'NONE',  ( 4.678144232538230085, 1508.611354625609920, 206.6339229097249870 ) ) ;
#101841 = EDGE_CURVE ( 'NONE', #39681, #47741, #26245, .T. ) ;
#101840 = CARTESIAN_POINT ( 'NONE',  ( 6.600633841864996576, 1435.170991571107834, 203.6679139044261717 ) ) ;
#101842 = CARTESIAN_POINT ( 'NONE',  ( -4.504070374734999938, 1508.551704408389924, 213.0883275018930192 ) ) ;
#101843 = CARTESIAN_POINT ( 'NONE',  ( -1.842962231260000028, 1515.551704408389924, 212.9514660752490158 ) ) ;
#101844 = CARTESIAN_POINT ( 'NONE',  ( 7.398264911990000137, 1422.106259636749883, 195.6015909957990289 ) ) ;
#101845 = CARTESIAN_POINT ( 'NONE',  ( -2.672909466071800466, 1432.986942304690047, 218.2820170679659952 ) ) ;
#101846 = CARTESIAN_POINT ( 'NONE',  ( -4.678725631789999895, 1495.985945357489982, 198.7901154368990149 ) ) ;
#101847 = CARTESIAN_POINT ( 'NONE',  ( 2.098606530373039902, 1408.986345342219920, 186.9550871089749933 ) ) ;
#101849 = DIRECTION ( 'NONE',  ( 4.465978680329379737E-17, 1.000000000000000000, -2.349386720892264891E-16 ) ) ;
#101848 = CARTESIAN_POINT ( 'NONE',  ( 1.200765764030000238, 1417.120114711829956, 233.8531050740980106 ) ) ;
#101850 = DIRECTION ( 'NONE',  ( -7.283063041540821170E-15, 0.9876883405951697448, 0.1564344650400280867 ) ) ;
#101851 = CARTESIAN_POINT ( 'NONE',  ( -10.74491738439999899, 1379.840458593170069, 215.5533963907290058 ) ) ;
#101852 = CARTESIAN_POINT ( 'NONE',  ( 2.646294106703178439, 1525.055402519451945, 241.6502424680635954 ) ) ;
#101853 = ORIENTED_EDGE ( 'NONE', *, *, #9938, .T. ) ;
#101854 = CARTESIAN_POINT ( 'NONE',  ( 11.73069774356920014, 1414.913057862230062, 220.5398999955840225 ) ) ;
#101855 = CARTESIAN_POINT ( 'NONE',  ( 5.170554601400000116, 1484.055082523290139, 219.7711189574989703 ) ) ;
#101856 = CARTESIAN_POINT ( 'NONE',  ( 32.15938645527133843, 1524.538768545233779, 202.1426263946930533 ) ) ;
#101857 = B_SPLINE_SURFACE_WITH_KNOTS ( 'NONE', 5, 4, ( 
 ( #92512, #5781, #108775, #5216, #56731 ),
 ( #15247, #65139, #99253, #6318, #39923 ),
 ( #66802, #90868, #14156, #48342, #82481 ),
 ( #31509, #24738, #15779, #49981, #23102 ),
 ( #41015, #91972, #99807, #32069, #67351 ),
 ( #49439, #83561, #40465, #109345, #75194 ) ),
 .UNSPECIFIED., .F., .F., .F.,
 ( 6, 6 ),
 ( 5, 5 ),
 ( -1.139299598668300043E-05, 11.48858425020000062 ),
 ( 25.78146411700000229, 39.23969207129999859 ),
 .UNSPECIFIED. ) ;
#101858 = CARTESIAN_POINT ( 'NONE',  ( -11.54624697350000062, 1388.394384052139912, 202.2644599199190054 ) ) ;
#101859 = CARTESIAN_POINT ( 'NONE',  ( 9.398642880860540672, 1427.777155254299942, 211.5857661256089841 ) ) ;
#101860 = CARTESIAN_POINT ( 'NONE',  ( 11.18358067844100034, 1422.622611808279999, 203.3483468631889934 ) ) ;
#101861 = CARTESIAN_POINT ( 'NONE',  ( 13.02322703161950024, 1416.825784015089994, 221.6328457863429833 ) ) ;
#101862 = CARTESIAN_POINT ( 'NONE',  ( -6.092217291859999939, 1469.463552789130063, 265.6112252686980355 ) ) ;
#101863 = AXIS2_PLACEMENT_3D ( 'NONE', #55189, #73638, #89314 ) ;
#101864 = CARTESIAN_POINT ( 'NONE',  ( -21.47555121375469867, 1509.121809597113042, 191.7875346140812951 ) ) ;
#101865 = CARTESIAN_POINT ( 'NONE',  ( 11.87331171179999956, 1433.127290053990009, 150.2013614949980251 ) ) ;
#101866 = CARTESIAN_POINT ( 'NONE',  ( 8.800012970690000103, 1452.709869713229864, 209.1218459616979999 ) ) ;
#101867 = B_SPLINE_SURFACE_WITH_KNOTS ( 'NONE', 5, 5, ( 
 ( #28290, #34484, #95493, #102759, #68659, #902, #27736, #78699, #357 ),
 ( #61926, #79261, #96606, #26055, #2012, #96043, #62486, #44550, #9285 ),
 ( #35028, #61374, #18761, #53515, #8714, #94945, #77596, #19875, #85987 ),
 ( #87092, #85415, #77051, #60250, #36148, #94367, #17649, #69207, #10947 ),
 ( #10377, #52958, #18214, #43447, #70332, #103316, #52410, #42893, #26624 ),
 ( #86535, #60820, #19314, #87658, #9829, #103892, #104444, #45119, #43998 ),
 ( #2571, #36693, #78133, #1436, #35582, #69774, #70887, #27191, #105001 ),
 ( #45883, #105787, #44783, #78933, #55381, #11178, #63787, #87887, #106318 ),
 ( #12804, #64337, #54835, #46984, #29070, #80020, #80572, #72729, #96269 ) ),
 .UNSPECIFIED., .F., .F., .F.,
 ( 6, 3, 6 ),
 ( 6, 3, 6 ),
 ( 22.40717020724860120, 46.28443321930000565, 74.85727727459999414 ),
 ( 0.000000000000000000, 1.000000000000000000, 2.000000000000000000 ),
 .UNSPECIFIED. ) ;
#101868 = CARTESIAN_POINT ( 'NONE',  ( -10.13020485171709950, 1461.692418066599885, 209.8925213690289979 ) ) ;
#101869 = LINE ( 'NONE', #33564, #38549 ) ;
#101870 = CIRCLE ( 'NONE', #10712, 1.999999954393705037 ) ;
#101871 = CARTESIAN_POINT ( 'NONE',  ( 9.501937463079149992, 1425.198055971670101, 196.1347459188490063 ) ) ;
#101872 = CARTESIAN_POINT ( 'NONE',  ( 8.798972287939317738, 1464.673512069870185, 213.6296587821800017 ) ) ;
#101873 = FACE_OUTER_BOUND ( 'NONE', #61281, .T. ) ;
#101874 = CARTESIAN_POINT ( 'NONE',  ( -29.72561318641060168, 1509.951099604490082, 208.7905312278460030 ) ) ;
#101875 = VECTOR ( 'NONE', #95087, 1000.000000000000000 ) ;
#101877 = B_SPLINE_CURVE_WITH_KNOTS ( 'NONE', 5,
 ( #38856, #73035, #107174, #30466, #64652, #56230 ),
 .UNSPECIFIED., .F., .F.,
 ( 6, 6 ),
 ( -1.999999954793280077, 0.000000000000000000 ),
 .UNSPECIFIED. ) ;
#101876 = CARTESIAN_POINT ( 'NONE',  ( -7.871069549766747109, 1426.247912565474508, 206.9070274792266559 ) ) ;
#101878 = CARTESIAN_POINT ( 'NONE',  ( 4.687651746879999415, 1478.378160227390254, 228.9010599218989910 ) ) ;
#101879 = CARTESIAN_POINT ( 'NONE',  ( -39.99258969340072412, 1438.670160836478544, 135.1922399653822708 ) ) ;
#101880 = CARTESIAN_POINT ( 'NONE',  ( 3.374302901398949839, 1508.029867056955027, 220.2219692825980530 ) ) ;
#101881 = CARTESIAN_POINT ( 'NONE',  ( -2.383407846124329765, 1522.906363951597314, 174.9517353176864844 ) ) ;
#101882 = CARTESIAN_POINT ( 'NONE',  ( -20.43379411225540210, 1466.940147600540058, 211.2182735651869905 ) ) ;
#101883 = CARTESIAN_POINT ( 'NONE',  ( 2.492130623175000448, 1516.778761582560037, 212.5675310476169955 ) ) ;
#101884 = CARTESIAN_POINT ( 'NONE',  ( -19.70057179385869972, 1418.794758439270026, 207.3135327979470048 ) ) ;
#101885 = CARTESIAN_POINT ( 'NONE',  ( 0.1979593984663390038, 1464.158265199940161, 182.7746200214319856 ) ) ;
#101887 = ORIENTED_EDGE ( 'NONE', *, *, #53555, .T. ) ;
#101886 = CARTESIAN_POINT ( 'NONE',  ( -3.911218387651921979, 1414.913060387329779, 193.3684778321149622 ) ) ;
#101888 = CARTESIAN_POINT ( 'NONE',  ( -13.76936860679999874, 1443.913060387329097, 176.3340081878980641 ) ) ;
#101889 = DIRECTION ( 'NONE',  ( 0.3090169943749423997, 0.000000000000000000, 0.9510565162951553075 ) ) ;
#101890 = CARTESIAN_POINT ( 'NONE',  ( 12.06084908070000061, 1433.903750942899933, 149.8851033673979884 ) ) ;
#101891 = CARTESIAN_POINT ( 'NONE',  ( -40.38917806203690475, 1448.047423120109897, 134.0999999983369833 ) ) ;
#101892 = CARTESIAN_POINT ( 'NONE',  ( -36.02435062347289829, 1445.276583446800032, 137.0631246289250100 ) ) ;
#101893 = EDGE_LOOP ( 'NONE', ( #52020, #28856, #53059, #44557, #35682 ) ) ;
#101894 = CARTESIAN_POINT ( 'NONE',  ( -10.18171327880000021, 1472.619598059789951, 209.5761564533819978 ) ) ;
#101895 = CARTESIAN_POINT ( 'NONE',  ( -2.793439186891359949, 1486.025328193850100, 182.0741020391329812 ) ) ;
#101896 = CARTESIAN_POINT ( 'NONE',  ( -17.37509865559999866, 1416.823418193129783, 214.4574835448779879 ) ) ;
#101897 = CARTESIAN_POINT ( 'NONE',  ( 7.389795930078929764, 1504.900412948340090, 213.9846519657809836 ) ) ;
#101898 = CARTESIAN_POINT ( 'NONE',  ( -9.564290896847950307, 1437.870856459579954, 211.8468459910199897 ) ) ;
#101899 = CARTESIAN_POINT ( 'NONE',  ( -108.9164604828789180, 1381.958826580047571, 310.7542428962289023 ) ) ;
#101900 = AXIS2_PLACEMENT_3D ( 'NONE', #61214, #79649, #52240 ) ;
#101901 = CARTESIAN_POINT ( 'NONE',  ( 15.90990255763500016, 1516.814170398969964, 193.9190501556669801 ) ) ;
#101902 = DIRECTION ( 'NONE',  ( 1.776356839400250465E-15, 0.000000000000000000, 1.000000000000000000 ) ) ;
#101903 = CARTESIAN_POINT ( 'NONE',  ( 3.902542241760000419, 1426.015650185330060, 185.2953857086980065 ) ) ;
#101904 = CARTESIAN_POINT ( 'NONE',  ( -74.59479506201390109, 1385.134432623380007, 274.7545841228630366 ) ) ;
#101905 = CARTESIAN_POINT ( 'NONE',  ( -10.31564862673620020, 1391.913060387289988, 213.9236953778939778 ) ) ;
#101906 = CARTESIAN_POINT ( 'NONE',  ( 11.63491105067470066, 1421.973764464760052, 207.9107772468980215 ) ) ;
#101907 = VERTEX_POINT ( 'NONE', #66986 ) ;
#101908 = CARTESIAN_POINT ( 'NONE',  ( -28.55764294989999996, 1451.460584126430149, 136.1042256204979708 ) ) ;
#101909 = CARTESIAN_POINT ( 'NONE',  ( 13.51702042466233600, 1443.501467202829645, 169.3754641244197217 ) ) ;
#101911 = ORIENTED_EDGE ( 'NONE', *, *, #49377, .F. ) ;
#101910 = CARTESIAN_POINT ( 'NONE',  ( 0.3947013525697100622, 1437.804170063959873, 227.6754659744219680 ) ) ;
#101912 = CARTESIAN_POINT ( 'NONE',  ( 2.366934492629999998, 1474.701470341489994, 220.3007639910990179 ) ) ;
#101913 = ADVANCED_FACE ( 'NONE', ( #75919 ), #8760, .T. ) ;
#101914 = B_SPLINE_CURVE_WITH_KNOTS ( 'NONE', 3,
 ( #65851, #47934, #4289, #107832, #5373, #99969, #31120, #14861, #40628, #5931 ),
 .UNSPECIFIED., .F., .F.,
 ( 4, 2, 2, 2, 4 ),
 ( 3.469446951953614189E-18, 0.0007406479101618155831, 0.001481295820323627697, 0.002221943730485440027, 0.002962591640647251924 ),
 .UNSPECIFIED. ) ;
#101915 = CARTESIAN_POINT ( 'NONE',  ( 12.51045652733512803, 1415.677402202029953, 211.4999743317719663 ) ) ;
#101917 = CARTESIAN_POINT ( 'NONE',  ( -7.951048262496951402, 1364.788525692098119, 209.6218459617148824 ) ) ;
#101916 = B_SPLINE_CURVE_WITH_KNOTS ( 'NONE', 5,
 ( #47179, #79693, #81308, #2999, #38759, #72395 ),
 .UNSPECIFIED., .F., .F.,
 ( 6, 6 ),
 ( 0.000000000000000000, 1.000000000000000000 ),
 .UNSPECIFIED. ) ;
#101918 = CARTESIAN_POINT ( 'NONE',  ( -8.955241798779999485, 1494.044665287490034, 202.1005013471790335 ) ) ;
#101919 = AXIS2_PLACEMENT_3D ( 'NONE', #30184, #54874, #64376 ) ;
#101920 = ADVANCED_FACE ( 'NONE', ( #31511 ), #40902, .T. ) ;
#101921 = CARTESIAN_POINT ( 'NONE',  ( 42.06232107555830169, 1440.913060387330006, 269.6487541170399709 ) ) ;
#101922 = CARTESIAN_POINT ( 'NONE',  ( 0.4151546846821903003, 1522.382868172863937, 244.9330574173806951 ) ) ;
#101923 = EDGE_CURVE ( 'NONE', #10343, #109438, #30203, .T. ) ;
#101924 = CARTESIAN_POINT ( 'NONE',  ( 16.25240189476375008, 1432.151868409839153, 218.3259014903973991 ) ) ;
#101925 = CARTESIAN_POINT ( 'NONE',  ( 1.450664468150000053, 1415.792771685530170, 232.7840273826980138 ) ) ;
#101926 = CARTESIAN_POINT ( 'NONE',  ( 8.526934319540000473, 1449.624708711990024, 204.5462524797590049 ) ) ;
#101927 = CARTESIAN_POINT ( 'NONE',  ( -4.145978979534980458E-15, 1375.413060387289988, 209.1218459572589836 ) ) ;
#101928 = CARTESIAN_POINT ( 'NONE',  ( 21.75648121771956411, 1509.708962386752546, 188.8810923022467705 ) ) ;
#101929 = CARTESIAN_POINT ( 'NONE',  ( -30.31118248176270669, 1526.186458717542337, 216.6939452248811335 ) ) ;
#101930 = CARTESIAN_POINT ( 'NONE',  ( -3.268235758764999943, 1516.890356958860139, 206.2562572478169898 ) ) ;
#101931 = CARTESIAN_POINT ( 'NONE',  ( 2.499999989320000005, 1447.977245594400074, 159.5593905798980074 ) ) ;
#101932 = CARTESIAN_POINT ( 'NONE',  ( -2.500000000000000000, 1436.180951016360041, 157.6151257071979899 ) ) ;
#101933 = CARTESIAN_POINT ( 'NONE',  ( -2.490606800900000195, 1496.797481259589858, 198.0109085349990039 ) ) ;
#101935 = EDGE_LOOP ( 'NONE', ( #53812, #50210 ) ) ;
#101934 = CARTESIAN_POINT ( 'NONE',  ( -68.50318901198390620, 1379.747522081850093, 280.0875204781369803 ) ) ;
#101936 = CARTESIAN_POINT ( 'NONE',  ( 40.71279077584669892, 1444.187195803030136, 137.0114455636829973 ) ) ;
#101937 = EDGE_LOOP ( 'NONE', ( #34539, #60722, #58123, #54211 ) ) ;
#101938 = CARTESIAN_POINT ( 'NONE',  ( -16.35769669196890419, 1514.438069590152509, 223.7531373634772649 ) ) ;
#101939 = CARTESIAN_POINT ( 'NONE',  ( -23.99427320719999912, 1410.919622273529967, 208.2638409563230084 ) ) ;
#101941 = CARTESIAN_POINT ( 'NONE',  ( 15.86112125244039817, 1410.431337872899803, 191.5898895329879963 ) ) ;
#101940 = CARTESIAN_POINT ( 'NONE',  ( -11.19545718725239958, 1426.041279750870217, 113.0052507005540008 ) ) ;
#101942 = CARTESIAN_POINT ( 'NONE',  ( -7.321193745875000047, 1516.534976163889951, 211.4135222436570132 ) ) ;
#101943 = CARTESIAN_POINT ( 'NONE',  ( 18.34728769450661900, 1509.673048444232336, 185.3862757340986320 ) ) ;
#101944 = VECTOR ( 'NONE', #73219, 1000.000000000000000 ) ;
#101945 = CARTESIAN_POINT ( 'NONE',  ( 2.292469552788555465, 1449.805609130731227, 182.1508050511279180 ) ) ;
#101946 = B_SPLINE_SURFACE_WITH_KNOTS ( 'NONE', 3, 5, ( 
 ( #103558, #77819, #53758, #61587, #52076, #28517 ),
 ( #576, #10054, #9502, #36911, #44228, #2791 ),
 ( #85646, #62148, #102996, #1128, #95720, #71106 ),
 ( #105230, #62718, #18985, #94601, #95172, #20106 ) ),
 .UNSPECIFIED., .F., .F., .F.,
 ( 4, 4 ),
 ( 6, 6 ),
 ( 5.479555871570000569, 5.505626611620000332 ),
 ( 0.000000000000000000, 1.000000000000000000 ),
 .UNSPECIFIED. ) ;
#101947 = SURFACE_SIDE_STYLE ('',( #7357 ) ) ;
#101948 = CARTESIAN_POINT ( 'NONE',  ( -12.89620243338210059, 1379.263018346050103, 208.6490890656160104 ) ) ;
#101949 = CARTESIAN_POINT ( 'NONE',  ( 12.68260786739960011, 1500.745025545950057, 209.9285465654390066 ) ) ;
#101950 = ITEM_DEFINED_TRANSFORMATION ( 'NONE', 'NONE', #95,  #21632 ) ;
#101951 = CARTESIAN_POINT ( 'NONE',  ( 4.580254622799669662, 1508.551704408389924, 212.9784530087700318 ) ) ;
#101952 = CARTESIAN_POINT ( 'NONE',  ( -34.59119253931500282, 1437.071637960610133, 136.5445694851690064 ) ) ;
#101953 = EDGE_LOOP ( 'NONE', ( #98008, #49823, #5276, #2015 ) ) ;
#101954 = CARTESIAN_POINT ( 'NONE',  ( 13.41275991522839917, 1396.898936538649878, 207.0368130037109893 ) ) ;
#101955 = CARTESIAN_POINT ( 'NONE',  ( 9.369980246745740260, 1462.099920443929932, 206.4857951425539966 ) ) ;
#101956 = AXIS2_PLACEMENT_3D ( 'NONE', #101544, #93160, #37129 ) ;
#101957 = CARTESIAN_POINT ( 'NONE',  ( -19.00906408819999882, 1456.707065538329971, 228.7066581731980079 ) ) ;
#101958 = ORIENTED_EDGE ( 'NONE', *, *, #94010, .T. ) ;
#101959 = ORIENTED_EDGE ( 'NONE', *, *, #50822, .T. ) ;
#101960 = CARTESIAN_POINT ( 'NONE',  ( -11.99447448239999936, 1410.787978745530154, 219.9627945351979861 ) ) ;
#101961 = CARTESIAN_POINT ( 'NONE',  ( 10.53440680805939955, 1452.831114188890069, 210.2190104787899827 ) ) ;
#101962 = CARTESIAN_POINT ( 'NONE',  ( -2.487935121788300119, 1509.038615937200120, 204.6345961869410246 ) ) ;
#101963 = CARTESIAN_POINT ( 'NONE',  ( -11.81019069571562774, 1417.596857770419547, 199.2280744327704838 ) ) ;
#101964 = AXIS2_PLACEMENT_3D ( 'NONE', #73571, #57331, #22004 ) ;
#101965 = CARTESIAN_POINT ( 'NONE',  ( 4.326992699989999913, 1515.158586642790169, 209.1218459614979963 ) ) ;
#101966 = CARTESIAN_POINT ( 'NONE',  ( -6.843521712735489260, 1453.772848492380035, 202.7227712865530123 ) ) ;
#101967 = CARTESIAN_POINT ( 'NONE',  ( -13.04207679966010147, 1409.368499744919745, 225.9431846064669855 ) ) ;
#101968 = DIRECTION ( 'NONE',  ( -5.980589973904019347E-17, 1.000000000000000000, -1.736889445713099699E-16 ) ) ;
#101969 = CARTESIAN_POINT ( 'NONE',  ( 27.07184576870000114, 1440.506430296650024, 137.2141704726979867 ) ) ;
#101970 = DIRECTION ( 'NONE',  ( 4.465978680329379737E-17, 1.000000000000000000, -2.349386720892264891E-16 ) ) ;
#101971 = CARTESIAN_POINT ( 'NONE',  ( -96.75625392299259886, 1384.863480572399794, 295.5060220262309940 ) ) ;
#101972 = ORIENTED_EDGE ( 'NONE', *, *, #32256, .F. ) ;
#101973 = CARTESIAN_POINT ( 'NONE',  ( 3.452917022905000355, 1517.089216728169959, 202.1725802860869976 ) ) ;
#101974 = CARTESIAN_POINT ( 'NONE',  ( 3.261652286895000419, 1516.939580991450157, 209.1085619926769823 ) ) ;
#101975 = ORIENTED_EDGE ( 'NONE', *, *, #63596, .T. ) ;
#101976 = CARTESIAN_POINT ( 'NONE',  ( 19.25089118869999893, 1455.005958191190075, 207.2694656823390176 ) ) ;
#101977 = B_SPLINE_CURVE_WITH_KNOTS ( 'NONE', 3,
 ( #16733, #109731, #92922, #16195, #67747, #8356, #42520, #50396, #84524, #7813, #33550, #110828, #51482, #78908, #88395, #87863, #79450, #1652, #2762, #102963, #20075, #69416, #45314, #69971, #70524, #52047, #36881, #71076, #19520, #34673, #35787, #86183, #2215, #105200 ),
 .UNSPECIFIED., .F., .F.,
 ( 4, 3, 3, 3, 3, 3, 3, 3, 3, 3, 3, 4 ),
 ( -26.06149361980000023, -24.76029548010210135, -23.45909734040419892, -22.14719351067359909, -21.39637773376540153, -20.04300759126989817, -18.69429331602630029, -17.34897622602300160, -16.01021078912490125, -14.67612915947669983, -13.34696737019829982, -12.02292824550000105 ),
 .UNSPECIFIED. ) ;
#101978 = CARTESIAN_POINT ( 'NONE',  ( 3.196833426707265335, 1511.813436676099627, 217.0699578229602196 ) ) ;
#101979 = EDGE_LOOP ( 'NONE', ( #25281, #23199, #78121, #89034 ) ) ;
#101980 = CARTESIAN_POINT ( 'NONE',  ( -14.23393746390000025, 1416.021639799829927, 221.4291795454980161 ) ) ;
#101981 = EDGE_CURVE ( 'NONE', #911, #40948, #65969, .T. ) ;
#101982 = CARTESIAN_POINT ( 'NONE',  ( 5.415590649712958893, 1429.910603248089956, 216.9138056063569877 ) ) ;
#101983 = CARTESIAN_POINT ( 'NONE',  ( -16.65376764594610037, 1508.454796205149933, 213.7212175226700026 ) ) ;
#101984 = CARTESIAN_POINT ( 'NONE',  ( -10.21381549268537725, 1491.160059455200326, 213.2743110981627126 ) ) ;
#101985 = CARTESIAN_POINT ( 'NONE',  ( -4.540052047909999722, 1423.807313613229780, 184.6930058418980138 ) ) ;
#101986 = CARTESIAN_POINT ( 'NONE',  ( -9.775296951400726186, 1446.595182981042853, 153.4780497659124023 ) ) ;
#101987 = DIRECTION ( 'NONE',  ( -1.000000000000000000, -2.249639673992789970E-32, -1.224646799147350002E-16 ) ) ;
#101988 = CARTESIAN_POINT ( 'NONE',  ( 5.312679136500000787, 1493.059131431590231, 218.8466398904690209 ) ) ;
#101989 = CARTESIAN_POINT ( 'NONE',  ( -51.80693370059999836, 1379.719625093879813, 243.7027045558589862 ) ) ;
#101990 = CARTESIAN_POINT ( 'NONE',  ( -16.81933045710000130, 1496.363585094529981, 224.0712623398979986 ) ) ;
#101992 = CARTESIAN_POINT ( 'NONE',  ( 2.487935098288932778, 1508.551704408389924, 213.9544627682086286 ) ) ;
#101991 = CARTESIAN_POINT ( 'NONE',  ( 17.60692135329999886, 1458.113405358530144, 229.3981720485979849 ) ) ;
#101993 = CARTESIAN_POINT ( 'NONE',  ( -4.859690594346670167, 1423.466502886267790, 184.6308178099481552 ) ) ;
#101994 = B_SPLINE_SURFACE_WITH_KNOTS ( 'NONE', 5, 5, ( 
 ( #39747, #65519, #83946, #49816, #99077, #38634 ),
 ( #30227, #64417, #73354, #30784, #22358, #99626 ),
 ( #57121, #91246, #14527, #48717, #74473, #108601 ),
 ( #31889, #66075, #68287, #93439, #76653, #16708 ),
 ( #9450, #110803, #35201, #43615, #52017, #85586 ),
 ( #17262, #51454, #8882, #69388, #58757, #102935 ) ),
 .UNSPECIFIED., .F., .F., .F.,
 ( 6, 6 ),
 ( 6, 6 ),
 ( 28.72930409989999845, 41.05058650750000027 ),
 ( 0.000000000000000000, 2.000000000000000000 ),
 .UNSPECIFIED. ) ;
#101995 = CARTESIAN_POINT ( 'NONE',  ( -5.360127758099149986, 1422.242654706269832, 144.1589408359039908 ) ) ;
#101996 = ORIENTED_EDGE ( 'NONE', *, *, #48902, .T. ) ;
#101997 = CARTESIAN_POINT ( 'NONE',  ( 18.24652371554340036, 1424.504995576649890, 223.7081814311490007 ) ) ;
#101998 = CARTESIAN_POINT ( 'NONE',  ( -21.46337646344873562, 1524.972613296804184, 234.5040406280893706 ) ) ;
#101999 = CARTESIAN_POINT ( 'NONE',  ( -2.896892187767880156, 1484.263391075600111, 183.3160938869699805 ) ) ;
#102000 = CARTESIAN_POINT ( 'NONE',  ( -17.19449298599652920, 1410.877585917538909, 192.1747057623898911 ) ) ;
#102002 = ORIENTED_EDGE ( 'NONE', *, *, #76957, .T. ) ;
#102001 = CARTESIAN_POINT ( 'NONE',  ( -11.30420028228749985, 1500.584958202139887, 210.9988023051070059 ) ) ;
#102003 = CARTESIAN_POINT ( 'NONE',  ( 0.5790313230850000492, 1453.165958254130146, 188.8726570487980041 ) ) ;
#102004 = AXIS2_PLACEMENT_3D ( 'NONE', #69983, #78354, #27390 ) ;
#102005 = CARTESIAN_POINT ( 'NONE',  ( 0.7637831719629990523, 1508.279675140790005, 220.7126945919989964 ) ) ;
#102006 = CARTESIAN_POINT ( 'NONE',  ( -11.82677958210000035, 1429.701853304430188, 149.3212236813980098 ) ) ;
#102007 = CARTESIAN_POINT ( 'NONE',  ( 1.859161530581180166, 1431.069669433720037, 199.8328166829190025 ) ) ;
#102008 = CARTESIAN_POINT ( 'NONE',  ( -10.80279757036180044, 1461.800106919070004, 211.1805521804130024 ) ) ;
#102009 = LINE ( 'NONE', #17437, #27152 ) ;
#102010 = LINE ( 'NONE', #52746, #60967 ) ;
#102011 = CARTESIAN_POINT ( 'NONE',  ( -113.4000000000000057, 1379.913060387289988, 304.2218459572590064 ) ) ;
#102012 = ADVANCED_FACE ( 'NONE', ( #81358 ), #18633, .F. ) ;
#102014 = CARTESIAN_POINT ( 'NONE',  ( -9.902328854349999432, 1479.355524923690155, 213.2350952645890061 ) ) ;
#102013 = CARTESIAN_POINT ( 'NONE',  ( -19.82812931440000170, 1470.089036833630189, 226.5638250403980010 ) ) ;
#102015 = DIRECTION ( 'NONE',  ( 0.000000000000000000, 0.000000000000000000, 1.000000000000000000 ) ) ;
#102016 = ORIENTED_EDGE ( 'NONE', *, *, #103879, .T. ) ;
#102017 = CARTESIAN_POINT ( 'NONE',  ( -4.624099329465000352, 1516.962555622980062, 205.8665050058069994 ) ) ;
#102018 = CARTESIAN_POINT ( 'NONE',  ( 21.98324444889999896, 1409.895860934730081, 267.6462823665979727 ) ) ;
#102019 = CARTESIAN_POINT ( 'NONE',  ( -173.8335085727391913, 1526.382868172863937, 317.3879012941878273 ) ) ;
#102020 = CARTESIAN_POINT ( 'NONE',  ( 21.11335034690000256, 1449.726224339279952, 195.7155535830980000 ) ) ;
#102021 = CARTESIAN_POINT ( 'NONE',  ( 0.06596416509929559080, 1508.967883553199954, 238.8759510148510117 ) ) ;
#102022 = CARTESIAN_POINT ( 'NONE',  ( 4.492546581380000958, 1453.878649273890005, 217.3453973181289882 ) ) ;
#102023 =( BOUNDED_CURVE ( )  B_SPLINE_CURVE ( 3, ( #81111, #6616, #110177, #40769 ),
 .UNSPECIFIED., .F., .F. ) 
 B_SPLINE_CURVE_WITH_KNOTS ( ( 4, 4 ),
 ( 1.144746442793614261, 1.570758305569332380 ),
 .UNSPECIFIED. ) 
 CURVE ( )  GEOMETRIC_REPRESENTATION_ITEM ( )  RATIONAL_B_SPLINE_CURVE ( ( 1.000000000000000000, 0.9849332539703330447, 0.9849332539703330447, 1.000000000000000000 ) ) 
 REPRESENTATION_ITEM ( '' )  );
#102024 = CARTESIAN_POINT ( 'NONE',  ( -40.67152590493699904, 1442.641813676910033, 136.9878664284970000 ) ) ;
#102025 = DIRECTION ( 'NONE',  ( 0.000000000000000000, 0.000000000000000000, 1.000000000000000000 ) ) ;
#102026 = CIRCLE ( 'NONE', #164, 2.000000000000001776 ) ;
#102027 = CARTESIAN_POINT ( 'NONE',  ( -14.98285036589999919, 1415.729638096350072, 205.4713522697590236 ) ) ;
#102028 = CARTESIAN_POINT ( 'NONE',  ( -12.97256195459999795, 1446.865982279580066, 187.9439210766980182 ) ) ;
#102029 = CARTESIAN_POINT ( 'NONE',  ( -5.664944777449460567, 1484.831651990110004, 198.6533526945029848 ) ) ;
#102030 = CARTESIAN_POINT ( 'NONE',  ( 0.4151546846821903003, 1511.187213306747708, 174.3106345060153046 ) ) ;
#102031 = CARTESIAN_POINT ( 'NONE',  ( -5.245637547039999404, 1497.146055658990008, 219.2578757579989883 ) ) ;
#102032 = ORIENTED_EDGE ( 'NONE', *, *, #52198, .F. ) ;
#102033 = CARTESIAN_POINT ( 'NONE',  ( -1.450592998049999860, 1477.402861163290027, 201.6210515953190168 ) ) ;
#102034 = CARTESIAN_POINT ( 'NONE',  ( -11.30426874151759975, 1409.307814150319928, 199.3369101544629700 ) ) ;
#102035 = LINE ( 'NONE', #85801, #12628 ) ;
#102036 = CARTESIAN_POINT ( 'NONE',  ( -12.28855869350000063, 1378.253616442990051, 210.0769077263690008 ) ) ;
#102037 = CARTESIAN_POINT ( 'NONE',  ( -14.57658230699999891, 1474.036347059630089, 268.9619602272979932 ) ) ;
#102038 = CARTESIAN_POINT ( 'NONE',  ( -18.65075743919999951, 1443.653128712389844, 211.8055058365289938 ) ) ;
#102039 = CARTESIAN_POINT ( 'NONE',  ( -12.50784581141053842, 1391.398398864934734, 210.4070514657185242 ) ) ;
#102040 = CARTESIAN_POINT ( 'NONE',  ( -24.11238158259271813, 1444.454182330793856, 211.7733111310209608 ) ) ;
#102041 = CARTESIAN_POINT ( 'NONE',  ( -54.74134739851029963, 1384.717926922609877, 271.3113735593159959 ) ) ;
#102042 = CARTESIAN_POINT ( 'NONE',  ( -14.93124696056320033, 1384.941737462140054, 200.6042365411380217 ) ) ;
#102043 = CIRCLE ( 'NONE', #78906, 1.999999999999997780 ) ;
#102044 = CARTESIAN_POINT ( 'NONE',  ( 11.23669755143010107, 1415.007830321379970, 222.5597074813329925 ) ) ;
#102045 = CARTESIAN_POINT ( 'NONE',  ( 0.8265244082521410185, 1408.941923255679967, 231.1644249228330068 ) ) ;
#102046 = ADVANCED_FACE ( 'NONE', ( #20975 ), #63785, .F. ) ;
#102047 = CARTESIAN_POINT ( 'NONE',  ( -18.66420869458074705, 1526.382868172864164, 185.4599087859683095 ) ) ;
#102048 = CARTESIAN_POINT ( 'NONE',  ( -29.30029655192939586, 1525.907212628473872, 196.8717316207790589 ) ) ;
#102049 = EDGE_CURVE ( 'NONE', #12260, #73043, #28844, .T. ) ;
#102050 = CARTESIAN_POINT ( 'NONE',  ( -22.42121221859999736, 1409.696026370929985, 207.7819003571480039 ) ) ;
#102051 = EDGE_CURVE ( 'NONE', #89942, #8151, #84935, .T. ) ;
#102052 = ADVANCED_FACE ( 'NONE', ( #16820 ), #8441, .F. ) ;
#102053 = CARTESIAN_POINT ( 'NONE',  ( -12.23669307423070052, 1377.661331666050273, 207.7794331870949804 ) ) ;
#102054 = CARTESIAN_POINT ( 'NONE',  ( 5.170554601400000116, 1484.055082523290139, 219.7711189574989703 ) ) ;
#102055 = CARTESIAN_POINT ( 'NONE',  ( 10.24103526349649940, 1480.245554142349874, 206.6866148605930107 ) ) ;
#102056 = EDGE_CURVE ( 'NONE', #30516, #6988, #38146, .T. ) ;
#102057 = CARTESIAN_POINT ( 'NONE',  ( -1.247677516857949989E-10, 1452.913060387320002, 152.5211338456990120 ) ) ;
#102058 = ADVANCED_FACE ( 'NONE', ( #56258 ), #31967, .T. ) ;
#102059 = CARTESIAN_POINT ( 'NONE',  ( -17.52911390707280148, 1441.908568393189853, 219.1841137618270068 ) ) ;
#102060 = CARTESIAN_POINT ( 'NONE',  ( -5.513200305162849979, 1508.884117426709963, 216.6305509556679851 ) ) ;
#102061 = CARTESIAN_POINT ( 'NONE',  ( -11.73709356449999852, 1426.695943566229971, 144.1748013794979784 ) ) ;
#102064 = CARTESIAN_POINT ( 'NONE',  ( -8.629930252190000317, 1384.437861086550129, 199.9043375559089952 ) ) ;
#102063 = VECTOR ( 'NONE', #6609, 1000.000000000000000 ) ;
#102062 = CARTESIAN_POINT ( 'NONE',  ( 5.513435558014999849, 1508.551704408389924, 216.1347675157070114 ) ) ;
#102065 = CARTESIAN_POINT ( 'NONE',  ( 11.73275740876320050, 1426.698660301100062, 143.8638901049260141 ) ) ;
#102066 = CARTESIAN_POINT ( 'NONE',  ( -126.7681019193000225, 1325.797319984390015, 296.9188185942790028 ) ) ;
#102067 = CARTESIAN_POINT ( 'NONE',  ( -30.90487439922565116, 1525.907212628473644, 201.8101144455181952 ) ) ;
#102068 = ADVANCED_FACE ( 'NONE', ( #98799 ), #35494, .T. ) ;
#102069 = LINE ( 'NONE', #76334, #34120 ) ;
#102070 = CIRCLE ( 'NONE', #85941, 0.9999999999999988898 ) ;
#102071 = CARTESIAN_POINT ( 'NONE',  ( -2.488360667435000284, 1516.616791731099966, 203.3506968572170308 ) ) ;
#102072 = CARTESIAN_POINT ( 'NONE',  ( -3.187512671122507690, 1398.008355567684930, 221.7452893070936568 ) ) ;
#102073 = FACE_OUTER_BOUND ( 'NONE', #5583, .T. ) ;
#102074 = DIRECTION ( 'NONE',  ( 0.000000000000000000, -1.338183447452830017E-16, -1.000000000000000000 ) ) ;
#102075 = DIRECTION ( 'NONE',  ( 0.000000000000000000, -1.000000000000000000, 0.000000000000000000 ) ) ;
#102076 = CARTESIAN_POINT ( 'NONE',  ( 20.82852640818889967, 1508.920542461920149, 228.0213171461830086 ) ) ;
#102078 = ORIENTED_EDGE ( 'NONE', *, *, #90530, .F. ) ;
#102077 = CARTESIAN_POINT ( 'NONE',  ( -57.01644491799999770, 1379.744987730500043, 259.4421383624589907 ) ) ;
#102079 = ORIENTED_EDGE ( 'NONE', *, *, #77220, .T. ) ;
#102080 = CARTESIAN_POINT ( 'NONE',  ( 11.94112542547770062, 1433.728687859460024, 150.4558864976919779 ) ) ;
#102081 = CARTESIAN_POINT ( 'NONE',  ( -9.622035674789998438, 1396.249069277030003, 215.8735477280980035 ) ) ;
#102082 = ORIENTED_EDGE ( 'NONE', *, *, #71721, .F. ) ;
#102083 = CARTESIAN_POINT ( 'NONE',  ( -105.6866551539999932, 1378.955223242689954, 305.6848347894589892 ) ) ;
#102084 = CARTESIAN_POINT ( 'NONE',  ( -109.4839831700000019, 1384.925032507449941, 311.2841082172590177 ) ) ;
#102085 = CARTESIAN_POINT ( 'NONE',  ( 3.829222816048220235, 1515.551704203360032, 206.3208014481249961 ) ) ;
#102087 = CARTESIAN_POINT ( 'NONE',  ( -113.4000000000000057, 1377.913060387289988, 304.2218459572590064 ) ) ;
#102086 = CARTESIAN_POINT ( 'NONE',  ( -13.90334061950993139, 1519.913060387329779, 183.6719516668990480 ) ) ;
#102088 = LINE ( 'NONE', #20289, #102613 ) ;
#102089 = ADVANCED_FACE ( 'NONE', ( #58872 ), #7849, .T. ) ;
#102090 = CIRCLE ( 'NONE', #19842, 39.03564169359999170 ) ;
#102091 = CARTESIAN_POINT ( 'NONE',  ( 3.174524293809999786, 1468.704260245830028, 183.1758726002980211 ) ) ;
#102092 = CARTESIAN_POINT ( 'NONE',  ( 1.882487193640000056, 1467.451596611890182, 219.3027413508989980 ) ) ;
#102093 = CARTESIAN_POINT ( 'NONE',  ( 16.31544538450000204, 1410.855193277729995, 226.7200764645979802 ) ) ;
#102094 = PRESENTATION_STYLE_ASSIGNMENT (( #50610 ) ) ;
#102096 = ADVANCED_FACE ( 'NONE', ( #11233 ), #87942, .F. ) ;
#102095 = CARTESIAN_POINT ( 'NONE',  ( 4.319575047684679703, 1396.063903275030043, 198.9757873032580164 ) ) ;
#102097 = CARTESIAN_POINT ( 'NONE',  ( 13.59781065039149972, 1415.089996094040089, 197.7253638271529894 ) ) ;
#102098 = CARTESIAN_POINT ( 'NONE',  ( 11.85528857480000120, 1431.583028049670020, 149.9311469192980155 ) ) ;
#102099 = B_SPLINE_CURVE_WITH_KNOTS ( 'NONE', 3,
 ( #48128, #74441, #30754, #100704, #108569, #90657, #82267, #108009, #64388, #39147, #81696, #91760, #98507, #107459, #64935, #49236, #99048, #13940, #32421, #31858, #31304, #13384, #39717, #47571, #74989, #92309, #5566, #56528, #73323, #40260, #40812, #82811, #49782, #15036, #73881, #83359, #21775, #14495, #15580, #55976, #65488, #66044, #66600, #99598, #23986, #22881, #48687, #57090, #83914, #91215, #100169, #6104, #23452, #57647, #6658, #109140, #58182, #7220, #41377, #75542, #30193, #18352, #51427, #69356, #35172, #43586, #77193, #9423, #60394, #103465, #77735, #8853, #26772, #34621, #60960, #86676, #16682, #43037, #110220, #95085, #496, #1048, #41925, #93966, #25651, #76624, #68805, #102907, #26205, #8304, #76081, #7759, #94514, #52544, #9973, #51989, #84472, #17788, #58728, #110776, #42466, #44143, #34068, #109677, #33494, #101803, #67695, #25095, #32953, #68259, #67143, #102368, #101240, #85557, #24540, #92863, #86129, #50879, #16143, #85010, #50346, #59300, #93415, #59842, #17230, #53100, #71590, #70467, #28435, #18904 ),
 .UNSPECIFIED., .F., .F.,
 ( 4, 3, 3, 3, 3, 3, 3, 3, 3, 3, 3, 3, 3, 3, 3, 3, 3, 3, 3, 3, 3, 3, 3, 3, 3, 3, 3, 3, 3, 3, 3, 3, 3, 3, 3, 3, 3, 3, 3, 3, 3, 3, 3, 4 ),
 ( 0.000000000000000000, 0.4989958285304099683, 0.8732426999282179025, 1.187904378483179979, 1.485459211540649971, 1.764154662664569884, 1.995983314121640095, 2.218900690584800106, 2.411230156830109994, 2.588723306273699620, 2.751770446255200397, 2.887652819974260154, 3.035486073829570142, 3.141664737081030445, 3.183319327684869915, 3.276504077055930164, 3.377348710061859993, 3.470358065450380280, 3.556407254322629719, 3.641400281485230206, 3.717201824902540253, 3.726393308647829805, 3.795380765736819928, 3.871873908516200391, 3.948738929127949771, 4.018859912850369476, 4.077147876327860132, 4.166923348113540371, 4.261100944480360475, 4.361051690202209841, 4.473351797408369634, 4.591235991841460695, 4.702032100850900065, 4.748093182062699924, 4.895722542919810572, 5.060544476256770174, 5.242866039422230173, 5.511025200193289564, 5.770121536528019845, 6.041084857940309583, 6.328006033295999977, 6.655379715367800486, 7.044317073833579634, 7.372157449769999538 ),
 .UNSPECIFIED. ) ;
#102100 = CARTESIAN_POINT ( 'NONE',  ( 6.787530778265000286, 1514.254015528269974, 201.2664419476070066 ) ) ;
#102101 = VERTEX_POINT ( 'NONE', #61641 ) ;
#102102 = CARTESIAN_POINT ( 'NONE',  ( 13.02703478251429914, 1435.306670126899917, 150.3834776061850107 ) ) ;
#102103 = ORIENTED_EDGE ( 'NONE', *, *, #55979, .F. ) ;
#102104 = EDGE_CURVE ( 'NONE', #101260, #94134, #92708, .T. ) ;
#102105 = ORIENTED_EDGE ( 'NONE', *, *, #71943, .F. ) ;
#102106 = CARTESIAN_POINT ( 'NONE',  ( 13.31747089092944769, 1444.561669151125898, 169.3769345727364737 ) ) ;
#102107 = CARTESIAN_POINT ( 'NONE',  ( -6.617277180400000347, 1464.914593472730076, 234.0919820975980201 ) ) ;
#102108 = DIRECTION ( 'NONE',  ( 0.000000000000000000, 1.000000000000000000, 0.000000000000000000 ) ) ;
#102109 = CARTESIAN_POINT ( 'NONE',  ( 3.454119916704999849, 1516.594591938570147, 216.8324563732270178 ) ) ;
#102110 = CARTESIAN_POINT ( 'NONE',  ( -8.384987537200094820, 1511.400228778148630, 213.7058500936460632 ) ) ;
#102111 = EDGE_CURVE ( 'NONE', #20038, #17543, #21151, .T. ) ;
#102112 = CARTESIAN_POINT ( 'NONE',  ( -4.115857443736018695, 1425.929640604822680, 186.1083528362279651 ) ) ;
#102113 = CARTESIAN_POINT ( 'NONE',  ( 7.396545043095000160, 1511.069621805459974, 202.7496783316070150 ) ) ;
#102114 = CARTESIAN_POINT ( 'NONE',  ( -3.771520288500000539, 1380.389610323579973, 208.3364477064349956 ) ) ;
#102115 = VERTEX_POINT ( 'NONE', #18485 ) ;
#102116 = CARTESIAN_POINT ( 'NONE',  ( -0.01323705180209850014, 1516.939658295650133, 206.6356258303270010 ) ) ;
#102117 = ORIENTED_EDGE ( 'NONE', *, *, #109055, .T. ) ;
#102118 = CARTESIAN_POINT ( 'NONE',  ( 20.20849196857150432, 1440.913060387330006, 217.7572800574920109 ) ) ;
#102119 = CARTESIAN_POINT ( 'NONE',  ( -19.26469919840000244, 1508.010672792329842, 229.6096138898979859 ) ) ;
#102120 = CARTESIAN_POINT ( 'NONE',  ( -9.192816412500000922, 1410.609185766430073, 188.0952304701980040 ) ) ;
#102121 = CARTESIAN_POINT ( 'NONE',  ( 7.651189237105000096, 1514.325389163589989, 214.8282438176370022 ) ) ;
#102123 = ORIENTED_EDGE ( 'NONE', *, *, #95986, .F. ) ;
#102122 = CARTESIAN_POINT ( 'NONE',  ( 0.1744917581285969910, 1415.933499560010205, 226.9784926752139995 ) ) ;
#102124 = CARTESIAN_POINT ( 'NONE',  ( 24.43147358619999565, 1438.163733812159990, 212.9042240985579895 ) ) ;
#102125 = DIRECTION ( 'NONE',  ( 0.000000000000000000, 0.000000000000000000, 1.000000000000000000 ) ) ;
#102126 = CARTESIAN_POINT ( 'NONE',  ( -102.7498137299999996, 1383.762281939259992, 311.0461218402589907 ) ) ;
#102127 = CARTESIAN_POINT ( 'NONE',  ( 10.96946812545280103, 1432.347663862999980, 151.7701354189910035 ) ) ;
#102128 = CARTESIAN_POINT ( 'NONE',  ( 22.14913372576365802, 1525.402221411349956, 182.5746398196713187 ) ) ;
#102129 = CARTESIAN_POINT ( 'NONE',  ( -0.7369042090349989804, 1517.080322339569875, 214.1333973382469935 ) ) ;
#102130 = CARTESIAN_POINT ( 'NONE',  ( 3.717177354979999571, 1462.278529190689824, 228.4137915130989995 ) ) ;
#102131 = EDGE_CURVE ( 'NONE', #95431, #65868, #98066, .T. ) ;
#102132 = CARTESIAN_POINT ( 'NONE',  ( -21.52112661409999816, 1509.604705971930116, 189.3622936410980060 ) ) ;
#102133 = CARTESIAN_POINT ( 'NONE',  ( 7.166260500400270850, 1508.551565390750284, 215.1547094865549923 ) ) ;
#102134 = CARTESIAN_POINT ( 'NONE',  ( 0.7578857918350010436, 1516.872851364150165, 211.6022732247369902 ) ) ;
#102136 = EDGE_CURVE ( 'NONE', #4089, #9923, #26605, .T. ) ;
#102135 = CARTESIAN_POINT ( 'NONE',  ( 9.512629190459559680, 1434.630476851629965, 206.8407525937180083 ) ) ;
#102137 = CARTESIAN_POINT ( 'NONE',  ( 13.30361809040000054, 1409.377632970929881, 191.9462305274980167 ) ) ;
#102138 = CARTESIAN_POINT ( 'NONE',  ( -13.08655243744227370, 1486.036966649576243, 185.2250414900032922 ) ) ;
#102140 = VERTEX_POINT ( 'NONE', #27456 ) ;
#102139 = CARTESIAN_POINT ( 'NONE',  ( -68.70832551159999468, 1385.106080149109857, 263.4315270082590246 ) ) ;
#102141 = CARTESIAN_POINT ( 'NONE',  ( -58.60909715759989780, 1385.073142730379914, 278.5419364966310241 ) ) ;
#102142 = CARTESIAN_POINT ( 'NONE',  ( 43.50124905439999878, 1443.586705889949826, 263.8967010718980077 ) ) ;
#102143 = CARTESIAN_POINT ( 'NONE',  ( -26.94471178607729911, 1509.853990456620068, 220.7433800216579982 ) ) ;
#102144 = CARTESIAN_POINT ( 'NONE',  ( -3.755850673020599828, 1508.470365865729946, 237.1708643925190074 ) ) ;
#102145 = CARTESIAN_POINT ( 'NONE',  ( -24.04659120089999647, 1444.796772349789762, 212.0316830079879935 ) ) ;
#102146 = CARTESIAN_POINT ( 'NONE',  ( 27.69925877688100258, 1441.434395746940027, 137.3015763641899980 ) ) ;
#102147 = EDGE_CURVE ( 'NONE', #22181, #19615, #53806, .T. ) ;
#102148 = AXIS2_PLACEMENT_3D ( 'NONE', #31378, #40333, #65560 ) ;
#102150 = FACE_OUTER_BOUND ( 'NONE', #107206, .T. ) ;
#102149 = FACE_OUTER_BOUND ( 'NONE', #81588, .T. ) ;
#102151 = DIRECTION ( 'NONE',  ( 0.000000000000000000, -1.000000000000000000, -0.000000000000000000 ) ) ;
#102152 = CARTESIAN_POINT ( 'NONE',  ( -108.3776759915979966, 1383.424114602280042, 310.9628763870520061 ) ) ;
#102153 = ORIENTED_EDGE ( 'NONE', *, *, #57084, .T. ) ;
#102154 = CARTESIAN_POINT ( 'NONE',  ( 5.776491095245000373, 1516.858301627840092, 203.3390965304970166 ) ) ;
#102155 = CARTESIAN_POINT ( 'NONE',  ( -8.356095914484159337, 1508.431967280379922, 219.3425879849650073 ) ) ;
#102156 = CARTESIAN_POINT ( 'NONE',  ( -1.551161424019060098, 1463.265709907049995, 199.4650991780359846 ) ) ;
#102157 = CARTESIAN_POINT ( 'NONE',  ( 24.55110742759999809, 1443.479132512090018, 214.0305984285579939 ) ) ;
#102158 = CARTESIAN_POINT ( 'NONE',  ( 10.92857032808210072, 1460.888924644350027, 208.5047758900509791 ) ) ;
#102159 = CARTESIAN_POINT ( 'NONE',  ( -6.719886226586697653, 1423.239092103852499, 186.8024023424373752 ) ) ;
#102160 = CARTESIAN_POINT ( 'NONE',  ( 3.919632032540000477, 1466.374841473789729, 219.0280172745789855 ) ) ;
#102161 = CARTESIAN_POINT ( 'NONE',  ( 1.367745396099944832, 1468.963081466252106, 219.0596951095364773 ) ) ;
#102162 = AXIS2_PLACEMENT_3D ( 'NONE', #4918, #39059, #65407 ) ;
#102163 = CARTESIAN_POINT ( 'NONE',  ( 27.58302672510169629, 1436.789581487599889, 136.7578142616270043 ) ) ;
#102164 = ADVANCED_FACE ( 'NONE', ( #77328 ), #53240, .F. ) ;
#102165 = CARTESIAN_POINT ( 'NONE',  ( -38.61927355701700293, 1444.188087899089851, 137.1592452686400065 ) ) ;
#102166 = CARTESIAN_POINT ( 'NONE',  ( -3.045280019940000305, 1464.258769156330118, 184.9382089438980188 ) ) ;
#102167 = CARTESIAN_POINT ( 'NONE',  ( -2.847678236620000192, 1430.845636562190066, 201.2564352188489920 ) ) ;
#102168 = CARTESIAN_POINT ( 'NONE',  ( 11.97338606960000007, 1507.452600680129763, 184.7136217416980060 ) ) ;
#102169 = CARTESIAN_POINT ( 'NONE',  ( -21.28825147355507497, 1525.253972588461920, 183.8869829075299549 ) ) ;
#102171 =( BOUNDED_CURVE ( )  B_SPLINE_CURVE ( 3, ( #12090, #88259, #88807, #63100 ),
 .UNSPECIFIED., .F., .T. ) 
 B_SPLINE_CURVE_WITH_KNOTS ( ( 4, 4 ),
 ( 4.151398476256234815, 5.273379648758210081 ),
 .UNSPECIFIED. ) 
 CURVE ( )  GEOMETRIC_REPRESENTATION_ITEM ( )  RATIONAL_B_SPLINE_CURVE ( ( 1.000000000000000000, 0.8978190064439198759, 0.8978190064439198759, 1.000000000000000000 ) ) 
 REPRESENTATION_ITEM ( '' )  );
#102170 = VECTOR ( 'NONE', #9355, 1000.000000000000000 ) ;
#102172 = CARTESIAN_POINT ( 'NONE',  ( -31.23437356469425907, 1518.913060387330006, 222.8968241038848248 ) ) ;
#102173 = ORIENTED_EDGE ( 'NONE', *, *, #39061, .T. ) ;
#102175 = EDGE_CURVE ( 'NONE', #36205, #78937, #2837, .T. ) ;
#102174 = CARTESIAN_POINT ( 'NONE',  ( -4.675540975309999681, 1462.620895424390028, 200.5633310686890241 ) ) ;
#102176 = CARTESIAN_POINT ( 'NONE',  ( -32.22920765839177903, 1416.715264199195417, 269.3109577515642172 ) ) ;
#102177 = CARTESIAN_POINT ( 'NONE',  ( -3.801734761035370447, 1509.034524749680031, 213.6092044152910034 ) ) ;
#102178 = DIRECTION ( 'NONE',  ( -1.755985294532469921E-16, 1.000000000000000000, -1.338183447452831989E-16 ) ) ;
#102179 = CARTESIAN_POINT ( 'NONE',  ( 10.86223758978695919, 1424.799205147552584, 138.1967566982364417 ) ) ;
#102181 = CARTESIAN_POINT ( 'NONE',  ( 31.02592223166955421, 1526.278758871496620, 198.2784374727472709 ) ) ;
#102180 = CARTESIAN_POINT ( 'NONE',  ( 11.59305468459999844, 1501.418989384490033, 208.8071487272210049 ) ) ;
#102182 = CARTESIAN_POINT ( 'NONE',  ( -13.04677262373687086, 1444.843571945705435, 186.3517559318727024 ) ) ;
#102183 = CARTESIAN_POINT ( 'NONE',  ( 7.793367779400000472, 1427.553872258489946, 212.4452625024690064 ) ) ;
#102184 = CARTESIAN_POINT ( 'NONE',  ( -2.329939107268110376, 1515.551844914359890, 213.1055637611929967 ) ) ;
#102185 = AXIS2_PLACEMENT_3D ( 'NONE', #103276, #26583, #110048 ) ;
#102186 = CARTESIAN_POINT ( 'NONE',  ( -12.98683036598197660, 1419.640195994466694, 228.2241801252318680 ) ) ;
#102187 = CARTESIAN_POINT ( 'NONE',  ( -7.499939553001469861, 1451.406347848051610, 153.0894475933693286 ) ) ;
#102188 = CARTESIAN_POINT ( 'NONE',  ( -17.90185111903100079, 1415.935475482089942, 209.1297322982429989 ) ) ;
#102189 = CARTESIAN_POINT ( 'NONE',  ( 24.52609508589999976, 1435.360108756510044, 136.2737900993979849 ) ) ;
#102190 = EDGE_CURVE ( 'NONE', #21931, #71163, #15519, .T. ) ;
#102191 = CARTESIAN_POINT ( 'NONE',  ( -13.51731348217402306, 1443.821176527551415, 169.3508350027707934 ) ) ;
#102192 = VERTEX_POINT ( 'NONE', #98515 ) ;
#102193 = CARTESIAN_POINT ( 'NONE',  ( -0.2465388108111499776, 1414.971349104640012, 192.4488333816270256 ) ) ;
#102194 = EDGE_CURVE ( 'NONE', #35904, #93500, #12857, .T. ) ;
#102195 = CARTESIAN_POINT ( 'NONE',  ( -10.71339921265560058, 1409.287180531749982, 227.5724379022690016 ) ) ;
#102196 = ORIENTED_EDGE ( 'NONE', *, *, #40376, .T. ) ;
#102197 = ORIENTED_EDGE ( 'NONE', *, *, #38793, .T. ) ;
#102198 = CARTESIAN_POINT ( 'NONE',  ( -0.2129047818200029696, 1500.069404719889917, 230.4573127901989835 ) ) ;
#102199 = CARTESIAN_POINT ( 'NONE',  ( -15.52168468949967384, 1415.982095105879580, 207.6414872824098836 ) ) ;
#102201 = CARTESIAN_POINT ( 'NONE',  ( -26.58541136060000198, 1442.644663293830035, 225.2688052828980005 ) ) ;
#102200 = CARTESIAN_POINT ( 'NONE',  ( 10.97483803849999973, 1426.062443049630019, 97.29894937469791216 ) ) ;
#102202 = FACE_OUTER_BOUND ( 'NONE', #41697, .T. ) ;
#102203 = CARTESIAN_POINT ( 'NONE',  ( 4.275225064648620510, 1425.369712006890040, 185.3838194923779952 ) ) ;
#102204 = EDGE_CURVE ( 'NONE', #92390, #22181, #10191, .T. ) ;
#102205 = CARTESIAN_POINT ( 'NONE',  ( -12.30675062099569850, 1378.370996218429809, 209.8570216548399969 ) ) ;
#102206 = CARTESIAN_POINT ( 'NONE',  ( -2.704797619127560004, 1420.195902051749727, 186.0070988970391568 ) ) ;
#102207 = CARTESIAN_POINT ( 'NONE',  ( -2.127574403380531720, 1524.244163922423695, 244.5104606571523789 ) ) ;
#102208 = CARTESIAN_POINT ( 'NONE',  ( -12.62835224979999893, 1416.067629290630066, 195.5863397732979934 ) ) ;
#102209 = CARTESIAN_POINT ( 'NONE',  ( -5.381311933963230487, 1511.468585895311890, 200.7968825339673913 ) ) ;
#102210 = CARTESIAN_POINT ( 'NONE',  ( 2.623518071850000410, 1448.928635941619859, 183.1137651247979932 ) ) ;
#102211 = CARTESIAN_POINT ( 'NONE',  ( 7.383885237739054475, 1362.992059837184343, 207.6218459616988241 ) ) ;
#102212 = EDGE_CURVE ( 'NONE', #29403, #6013, #77044, .T. ) ;
#102213 = CARTESIAN_POINT ( 'NONE',  ( -26.94609914958298091, 1509.966636646189500, 222.4048654676792296 ) ) ;
#102214 = EDGE_CURVE ( 'NONE', #44485, #57348, #29661, .T. ) ;
#102216 = ORIENTED_EDGE ( 'NONE', *, *, #35114, .F. ) ;
#102215 = CARTESIAN_POINT ( 'NONE',  ( -7.706458268878440518E-10, 1416.874386753929912, 237.4765920278839815 ) ) ;
#102217 = ORIENTED_EDGE ( 'NONE', *, *, #11205, .F. ) ;
#102218 = CARTESIAN_POINT ( 'NONE',  ( -11.83030941994529961, 1429.922132322770040, 149.4306578747379888 ) ) ;
#102219 = CARTESIAN_POINT ( 'NONE',  ( 1.145290945507940084, 1458.110487998910003, 199.6352770989870180 ) ) ;
#102220 = CARTESIAN_POINT ( 'NONE',  ( -3.068143279839999682, 1471.712358786229970, 269.8661856461979482 ) ) ;
#102221 = CARTESIAN_POINT ( 'NONE',  ( 10.24652809674144649, 1501.212611039424701, 203.9352555582063928 ) ) ;
#102222 = CARTESIAN_POINT ( 'NONE',  ( -105.2220349633250862, 1311.832804576488797, 308.6894886186424856 ) ) ;
#102223 = CARTESIAN_POINT ( 'NONE',  ( 1.488474718494355198, 1526.348417187218502, 239.9133697138477146 ) ) ;
#102224 = CARTESIAN_POINT ( 'NONE',  ( -1.138407481869679883, 1475.515787706559877, 197.7305842908260161 ) ) ;
#102225 =( NAMED_UNIT ( * ) PLANE_ANGLE_UNIT ( ) SI_UNIT ( $, .RADIAN. ) );
#102226 = CARTESIAN_POINT ( 'NONE',  ( 38.64468768876599825, 1444.005792394500077, 137.1818110905059882 ) ) ;
#102227 = CARTESIAN_POINT ( 'NONE',  ( 9.879744843524427722, 1368.750325468937035, 209.6218459617033432 ) ) ;
#102228 = CARTESIAN_POINT ( 'NONE',  ( -10.33301352385990057, 1447.717428273800124, 209.8082491242700200 ) ) ;
#102229 = CARTESIAN_POINT ( 'NONE',  ( -8.384869426575338736, 1406.402803996059902, 267.2065357290120460 ) ) ;
#102230 = CARTESIAN_POINT ( 'NONE',  ( -14.33169648120709994, 1436.128833957109919, 150.0042863882840152 ) ) ;
#102231 = EDGE_LOOP ( 'NONE', ( #27660, #12730, #6848, #14327 ) ) ;
#102232 = CARTESIAN_POINT ( 'NONE',  ( -4.327871496238200777, 1515.125026768160069, 209.9123818876519749 ) ) ;
#102233 = EDGE_CURVE ( 'NONE', #5500, #51188, #31610, .T. ) ;
#102234 = CARTESIAN_POINT ( 'NONE',  ( 13.63158477449999850, 1446.168541001489984, 189.0290012264979964 ) ) ;
#102235 = ORIENTED_EDGE ( 'NONE', *, *, #48798, .F. ) ;
#102236 = ORIENTED_EDGE ( 'NONE', *, *, #4394, .F. ) ;
#102237 = B_SPLINE_CURVE_WITH_KNOTS ( 'NONE', 5,
 ( #10594, #2768, #44204, #54815, #20082, #1106 ),
 .UNSPECIFIED., .F., .F.,
 ( 6, 6 ),
 ( 0.000000000000000000, 1.000000000000000000 ),
 .UNSPECIFIED. ) ;
#102238 = CARTESIAN_POINT ( 'NONE',  ( 7.709253415549203403, 1516.542698387791233, 206.5079181198552760 ) ) ;
#102239 = LINE ( 'NONE', #369, #106346 ) ;
#102240 = ADVANCED_FACE ( 'NONE', ( #97422 ), #63846, .F. ) ;
#102241 = CARTESIAN_POINT ( 'NONE',  ( 6.559168636745000391, 1516.960844870249957, 214.1244393295569921 ) ) ;
#102242 = FACE_OUTER_BOUND ( 'NONE', #49527, .T. ) ;
#102243 = CARTESIAN_POINT ( 'NONE',  ( -16.35102150754449823, 1489.056232056260114, 229.5676014274860108 ) ) ;
#102244 = ORIENTED_EDGE ( 'NONE', *, *, #69646, .T. ) ;
#102245 = DIRECTION ( 'NONE',  ( 0.000000000000000000, -0.7071067811865474617, -0.7071067811865474617 ) ) ;
#102246 = CARTESIAN_POINT ( 'NONE',  ( 3.449777315724999571, 1516.974592746400049, 204.1104779853070283 ) ) ;
#102247 = AXIS2_PLACEMENT_3D ( 'NONE', #83435, #91296, #48767 ) ;
#102248 = CARTESIAN_POINT ( 'NONE',  ( -27.92008070680000031, 1508.619330697029909, 206.8298810821879954 ) ) ;
#102249 = CARTESIAN_POINT ( 'NONE',  ( -4.463702467710766619, 1420.728434188236406, 186.4092242688610668 ) ) ;
#102250 = CARTESIAN_POINT ( 'NONE',  ( -42.20971106035590026, 1384.589822447700044, 215.1439631396389984 ) ) ;
#102251 = DIRECTION ( 'NONE',  ( 0.2922845185089309461, -0.1043872945603406127, -0.9506171958124757237 ) ) ;
#102252 = CARTESIAN_POINT ( 'NONE',  ( -10.94922716044850119, 1470.861560421989907, 209.5255082995269902 ) ) ;
#102254 = ORIENTED_EDGE ( 'NONE', *, *, #74428, .F. ) ;
#102253 = CARTESIAN_POINT ( 'NONE',  ( 21.10561344245438065, 1525.661275128775742, 184.9336819308397537 ) ) ;
#102255 = CARTESIAN_POINT ( 'NONE',  ( -24.37209804522549916, 1430.523523475739921, 210.5057520659609906 ) ) ;
#102256 = CARTESIAN_POINT ( 'NONE',  ( 23.50062167809999991, 1488.679648897129937, 220.9815905391980095 ) ) ;
#102257 = CARTESIAN_POINT ( 'NONE',  ( -46.82349676020197649, 1379.680994877702915, 239.8269233030615339 ) ) ;
#102258 = CARTESIAN_POINT ( 'NONE',  ( 16.66936639845652834, 1518.913060387330006, 237.7608804993219280 ) ) ;
#102259 = CARTESIAN_POINT ( 'NONE',  ( -12.99826179536609949, 1436.002654027139897, 150.7444092751300388 ) ) ;
#102260 = CARTESIAN_POINT ( 'NONE',  ( 4.625693865015000128, 1517.042661899400173, 211.4082922958669997 ) ) ;
#102261 = CARTESIAN_POINT ( 'NONE',  ( -68.73855403010000487, 1379.747900905000051, 280.1049392198590340 ) ) ;
#102262 = CARTESIAN_POINT ( 'NONE',  ( -18.83642247210000065, 1444.248298674089938, 209.1218459616989946 ) ) ;
#102263 = CARTESIAN_POINT ( 'NONE',  ( -25.98102620619109970, 1446.564900598659960, 138.2990622187889755 ) ) ;
#102264 = CARTESIAN_POINT ( 'NONE',  ( -6.951517170504999399, 1517.194816588360027, 207.9969518818670053 ) ) ;
#102265 = ORIENTED_EDGE ( 'NONE', *, *, #11862, .F. ) ;
#102266 = CARTESIAN_POINT ( 'NONE',  ( -2.535709347209119890, 1451.956901329029961, 184.6703102415019941 ) ) ;
#102267 = CARTESIAN_POINT ( 'NONE',  ( -2.377121702169999740, 1410.304607662629905, 232.7018834577980044 ) ) ;
#102268 = CIRCLE ( 'NONE', #54047, 24.33258347882036432 ) ;
#102269 = CARTESIAN_POINT ( 'NONE',  ( -20.07303063531396603, 1456.359329617847379, 225.0559024278571769 ) ) ;
#102270 = VERTEX_POINT ( 'NONE', #38069 ) ;
#102271 = CARTESIAN_POINT ( 'NONE',  ( -41.65674268029999894, 1443.992461967939789, 135.6790812281979868 ) ) ;
#102272 = CARTESIAN_POINT ( 'NONE',  ( -11.02166737461350010, 1492.206447049650023, 203.6901558032419928 ) ) ;
#102273 = CARTESIAN_POINT ( 'NONE',  ( 12.35981619036649981, 1435.019032516630205, 150.7822008033989789 ) ) ;
#102274 = CARTESIAN_POINT ( 'NONE',  ( -4.074752427351803874, 1441.099746912515457, 184.8041399762123547 ) ) ;
#102275 = CARTESIAN_POINT ( 'NONE',  ( -14.81511931610000055, 1416.828882134419928, 206.5603892752189950 ) ) ;
#102276 = CARTESIAN_POINT ( 'NONE',  ( -16.85976061912534263, 1525.821544997590536, 236.1944305375347994 ) ) ;
#102277 = CARTESIAN_POINT ( 'NONE',  ( 4.021865650940000592, 1487.198045919489914, 198.2747322527989979 ) ) ;
#102278 = CARTESIAN_POINT ( 'NONE',  ( 2.010167598323350013, 1431.137515179070078, 218.3977979629700030 ) ) ;
#102279 = DIRECTION ( 'NONE',  ( 1.835183309750130004E-16, 1.000000000000000000, 1.599799320660000123E-19 ) ) ;
#102281 = CARTESIAN_POINT ( 'NONE',  ( -1.842963446620164092, 1515.320037145748756, 204.8511296326253159 ) ) ;
#102280 = CARTESIAN_POINT ( 'NONE',  ( 2.877113070465000089, 1516.697242742309982, 214.1184881303969973 ) ) ;
#102282 = CARTESIAN_POINT ( 'NONE',  ( -8.861665967949491574, 1385.086004207679935, 218.6801736522280066 ) ) ;
#102283 = CARTESIAN_POINT ( 'NONE',  ( -7.717505791104999346, 1516.857914730730045, 216.8393517232070167 ) ) ;
#102284 = EDGE_LOOP ( 'NONE', ( #92277, #48434, #22606, #19619 ) ) ;
#102285 = CARTESIAN_POINT ( 'NONE',  ( -11.40468314538169992, 1414.972329067380088, 195.9645814929980077 ) ) ;
#102286 = CARTESIAN_POINT ( 'NONE',  ( 15.80579254656381138, 1409.464994508550490, 192.9618219584179997 ) ) ;
#102287 = VERTEX_POINT ( 'NONE', #85018 ) ;
#102288 = CARTESIAN_POINT ( 'NONE',  ( -16.57873794416559932, 1508.551704408389924, 213.1306309380350115 ) ) ;
#102289 = CARTESIAN_POINT ( 'NONE',  ( 2.664388089274176696, 1523.844789899199895, 176.1122506963328931 ) ) ;
#102290 = CARTESIAN_POINT ( 'NONE',  ( -21.26826130359999922, 1504.995118174490017, 212.3995629039989979 ) ) ;
#102291 = CARTESIAN_POINT ( 'NONE',  ( -11.40436649515589984, 1470.754293980279954, 209.1665043884289901 ) ) ;
#102292 = CARTESIAN_POINT ( 'NONE',  ( 1.807973860705883729, 1416.690826690935182, 232.7107328888371001 ) ) ;
#102293 = CARTESIAN_POINT ( 'NONE',  ( 18.63578313170000200, 1416.568813547830132, 209.6898099495820134 ) ) ;
#102294 = CARTESIAN_POINT ( 'NONE',  ( 5.467155153583750149, 1493.854051205442147, 218.8016796649062883 ) ) ;
#102295 = CARTESIAN_POINT ( 'NONE',  ( -4.915203104360000630, 1434.541746329560056, 150.1320020560979742 ) ) ;
#102296 = CARTESIAN_POINT ( 'NONE',  ( 45.64477911114779829, 1440.913060379309854, 266.1600766877090223 ) ) ;
#102298 = DIRECTION ( 'NONE',  ( 1.000000000000000000, 0.000000000000000000, 0.000000000000000000 ) ) ;
#102297 = CARTESIAN_POINT ( 'NONE',  ( -2.265088008643420192, 1421.884433507809945, 193.4623903222540093 ) ) ;
#102299 = CARTESIAN_POINT ( 'NONE',  ( 0.7251570665222376588, 1526.278758871496848, 241.9800489742293053 ) ) ;
#102300 = VERTEX_POINT ( 'NONE', #16150 ) ;
#102301 = EDGE_LOOP ( 'NONE', ( #97219, #72085, #31879, #71339 ) ) ;
#102302 = CARTESIAN_POINT ( 'NONE',  ( -11.86610048948770135, 1432.336024750160050, 149.9824232984959735 ) ) ;
#102303 = CARTESIAN_POINT ( 'NONE',  ( -4.138993644310000164, 1515.551749209589843, 209.1218459616989946 ) ) ;
#102304 = CARTESIAN_POINT ( 'NONE',  ( -24.40358107970000034, 1441.574771168059897, 212.0768376997980056 ) ) ;
#102305 = CARTESIAN_POINT ( 'NONE',  ( 7.985525884112817607, 1410.564564186529651, 187.6169077096484159 ) ) ;
#102306 = CARTESIAN_POINT ( 'NONE',  ( -3.200428057587697328, 1425.998269221526471, 185.6653851470253755 ) ) ;
#102307 = DIRECTION ( 'NONE',  ( -5.980589973904019347E-17, 1.000000000000000000, -1.736889445713099699E-16 ) ) ;
#102308 = CARTESIAN_POINT ( 'NONE',  ( -4.487249792034999629, 1509.038615934169911, 205.6342535031670025 ) ) ;
#102309 = B_SPLINE_CURVE_WITH_KNOTS ( 'NONE', 5,
 ( #57279, #34243, #91407, #57819, #83535, #58909 ),
 .UNSPECIFIED., .F., .F.,
 ( 6, 6 ),
 ( 0.000000000000000000, 1.000000000000000000 ),
 .UNSPECIFIED. ) ;
#102310 = CARTESIAN_POINT ( 'NONE',  ( 14.17511973000000047, 1428.761297070790079, 195.0897165316990254 ) ) ;
#102311 = CARTESIAN_POINT ( 'NONE',  ( -60.12749137407530498, 1383.796527668070212, 280.8331374614150491 ) ) ;
#102312 = CARTESIAN_POINT ( 'NONE',  ( 16.22045774760000114, 1452.203078162129941, 148.6092594038979939 ) ) ;
#102313 = CARTESIAN_POINT ( 'NONE',  ( 17.68237282055029880, 1522.051704408389924, 212.5589510568480023 ) ) ;
#102315 = VERTEX_POINT ( 'NONE', #67701 ) ;
#102314 = CARTESIAN_POINT ( 'NONE',  ( 1.875671004969999833, 1456.514200624189925, 219.5762891113990065 ) ) ;
#102316 = CARTESIAN_POINT ( 'NONE',  ( -18.26113587671628835, 1459.251075348199493, 227.8504342410868446 ) ) ;
#102317 = CIRCLE ( 'NONE', #7544, 12.49965726619999984 ) ;
#102318 = CARTESIAN_POINT ( 'NONE',  ( -32.63285090699999813, 1382.325048536849863, 229.5366794896590079 ) ) ;
#102319 = ADVANCED_FACE ( 'NONE', ( #7766 ), #100175, .F. ) ;
#102320 = CARTESIAN_POINT ( 'NONE',  ( 19.77970646006350108, 1507.962483444719965, 229.2896370130209789 ) ) ;
#102321 = ORIENTED_EDGE ( 'NONE', *, *, #68742, .F. ) ;
#102322 = EDGE_LOOP ( 'NONE', ( #84124, #20346 ) ) ;
#102323 = CARTESIAN_POINT ( 'NONE',  ( 17.40063846696789795, 1509.472889227200085, 232.3001343056659778 ) ) ;
#102324 = DIRECTION ( 'NONE',  ( 0.000000000000000000, 1.000000000000000000, 0.000000000000000000 ) ) ;
#102325 = CARTESIAN_POINT ( 'NONE',  ( 38.40016583756019486, 1439.005933973110132, 136.6388233531990011 ) ) ;
#102327 = CARTESIAN_POINT ( 'NONE',  ( -4.329448776275169664, 1515.064792882719985, 206.7917118343879963 ) ) ;
#102326 = CARTESIAN_POINT ( 'NONE',  ( 22.28696231330000188, 1506.798305107930219, 209.3970118511340104 ) ) ;
#102328 = EDGE_CURVE ( 'NONE', #16982, #63865, #91696, .T. ) ;
#102329 = CARTESIAN_POINT ( 'NONE',  ( 11.56580875524219998, 1480.193683599319911, 211.4103531732560270 ) ) ;
#102330 = CARTESIAN_POINT ( 'NONE',  ( -109.3690719439999981, 1384.479823484100052, 297.1383975656590337 ) ) ;
#102331 = EDGE_CURVE ( 'NONE', #87392, #38412, #37338, .T. ) ;
#102332 = CARTESIAN_POINT ( 'NONE',  ( -32.38601544705579727, 1523.530935881284904, 216.1237228173876304 ) ) ;
#102333 = CARTESIAN_POINT ( 'NONE',  ( 41.65675406397859604, 1443.992462633329978, 135.6790809494980010 ) ) ;
#102334 = DIRECTION ( 'NONE',  ( -5.980589973904019347E-17, 1.000000000000000000, -1.736889445713099699E-16 ) ) ;
#102335 = CARTESIAN_POINT ( 'NONE',  ( 3.024002413519999877, 1409.955320795729904, 185.7438941976979834 ) ) ;
#102336 = CARTESIAN_POINT ( 'NONE',  ( -0.9166357444073550687, 1485.892889838330120, 197.2561232801839992 ) ) ;
#102337 = CARTESIAN_POINT ( 'NONE',  ( 2.382436964801011303, 1426.901689560120076, 137.0999999980980135 ) ) ;
#102338 = CARTESIAN_POINT ( 'NONE',  ( -2.500000009292929981, 1439.653988136930138, 157.1385067185380251 ) ) ;
#102339 = VECTOR ( 'NONE', #50788, 1000.000000000000000 ) ;
#102340 = EDGE_CURVE ( 'NONE', #61114, #85936, #1535, .T. ) ;
#102341 = CARTESIAN_POINT ( 'NONE',  ( -2.653122947949710042, 1450.219879838080033, 184.3098072337210169 ) ) ;
#102342 = CARTESIAN_POINT ( 'NONE',  ( 0.5800689402049999943, 1465.108714862629995, 238.1056003411979987 ) ) ;
#102343 = ORIENTED_EDGE ( 'NONE', *, *, #42389, .F. ) ;
#102344 =( BOUNDED_CURVE ( )  B_SPLINE_CURVE ( 3, ( #74449, #76088, #16688, #110226 ),
 .UNSPECIFIED., .F., .T. ) 
 B_SPLINE_CURVE_WITH_KNOTS ( ( 4, 4 ),
 ( 3.097738652567880280, 3.109953943715398683 ),
 .UNSPECIFIED. ) 
 CURVE ( )  GEOMETRIC_REPRESENTATION_ITEM ( )  RATIONAL_B_SPLINE_CURVE ( ( 1.000000000000000000, 0.9999875655938355035, 0.9999875655938355035, 1.000000000000000000 ) ) 
 REPRESENTATION_ITEM ( '' )  );
#102346 = CARTESIAN_POINT ( 'NONE',  ( -4.495215926552520003, 1481.166686022519798, 231.0476533587359995 ) ) ;
#102345 = B_SPLINE_CURVE_WITH_KNOTS ( 'NONE', 5,
 ( #97115, #104408, #52919, #96004, #3631, #63008 ),
 .UNSPECIFIED., .F., .F.,
 ( 6, 6 ),
 ( 0.000000000000000000, 1.000000000000000000 ),
 .UNSPECIFIED. ) ;
#102347 = CARTESIAN_POINT ( 'NONE',  ( -42.06231081589999832, 1442.393258506680013, 269.6487546124980099 ) ) ;
#102348 = DIRECTION ( 'NONE',  ( -0.3083968794178160722, -0.4480171631737070448, 0.8391495613221381378 ) ) ;
#102349 = CARTESIAN_POINT ( 'NONE',  ( 21.98270307507978671, 1506.436298853234575, 208.8042839102180039 ) ) ;
#102350 = CARTESIAN_POINT ( 'NONE',  ( -17.94925291060000205, 1468.366100212389938, 200.1415149508490003 ) ) ;
#102351 = CARTESIAN_POINT ( 'NONE',  ( -2.986490615134639819E-10, 1470.706479902790079, 255.8596430159340116 ) ) ;
#102352 = CARTESIAN_POINT ( 'NONE',  ( 19.54265149998314754, 1436.412494327520335, 145.9155188746681802 ) ) ;
#102353 = CARTESIAN_POINT ( 'NONE',  ( -1.555569193359999991, 1415.296882296330068, 227.2022622829979639 ) ) ;
#102354 = CARTESIAN_POINT ( 'NONE',  ( -7.535715290459999771, 1417.922762214429895, 231.4272348479980224 ) ) ;
#102355 = CARTESIAN_POINT ( 'NONE',  ( -2.642331102980000068, 1475.301074652890065, 198.3937767294989953 ) ) ;
#102356 = CARTESIAN_POINT ( 'NONE',  ( -107.9094517300000149, 1388.661150411839799, 309.9624615272590518 ) ) ;
#102357 = CARTESIAN_POINT ( 'NONE',  ( -0.2591898832630973870, 1485.931169546443243, 181.8387173835997146 ) ) ;
#102358 = CARTESIAN_POINT ( 'NONE',  ( 6.135919523401898168, 1359.334529397649248, 208.3718459617010978 ) ) ;
#102359 = CARTESIAN_POINT ( 'NONE',  ( -45.52430914911710147, 1438.500102775369896, 268.9779564349610155 ) ) ;
#102360 = CARTESIAN_POINT ( 'NONE',  ( 13.44640270494290135, 1508.358158129190087, 233.2747887588230071 ) ) ;
#102361 = FACE_OUTER_BOUND ( 'NONE', #46692, .T. ) ;
#102362 = ORIENTED_EDGE ( 'NONE', *, *, #73258, .F. ) ;
#102363 = CARTESIAN_POINT ( 'NONE',  ( -2.879318455905000018, 1516.995911393979895, 208.3865093923290033 ) ) ;
#102364 = CARTESIAN_POINT ( 'NONE',  ( -2.478862593460000152, 1433.766044927639996, 157.5584562999979994 ) ) ;
#102366 = EDGE_CURVE ( 'NONE', #79565, #65905, #102344, .T. ) ;
#102365 = EDGE_CURVE ( 'NONE', #25781, #39065, #71355, .T. ) ;
#102367 = CARTESIAN_POINT ( 'NONE',  ( 19.40941048885533249, 1456.875960972931580, 224.4905711428775419 ) ) ;
#102368 = CARTESIAN_POINT ( 'NONE',  ( 7.392999751807240116, 1426.269867617909995, 212.5881189270220091 ) ) ;
#102369 = CARTESIAN_POINT ( 'NONE',  ( -25.83594673127759833, 1451.994654212179967, 135.3393805079549850 ) ) ;
#102370 = ORIENTED_EDGE ( 'NONE', *, *, #15100, .T. ) ;
#102371 = CARTESIAN_POINT ( 'NONE',  ( -5.472761979749999715E-09, 1419.629243942729772, 225.6556823431979808 ) ) ;
#102373 = CARTESIAN_POINT ( 'NONE',  ( -15.30997868661039973, 1512.715996828740117, 222.6464017490669960 ) ) ;
#102372 = CARTESIAN_POINT ( 'NONE',  ( -11.11407518912900017, 1492.021456573850173, 207.0665889738719727 ) ) ;
#102374 = ADVANCED_FACE ( 'NONE', ( #8312 ), #1686, .T. ) ;
#102375 = DIRECTION ( 'NONE',  ( 3.828568698926946970E-16, 0.000000000000000000, -1.000000000000000000 ) ) ;
#102376 = CARTESIAN_POINT ( 'NONE',  ( -22.76393692011477654, 1450.407194713662193, 220.5314342327505130 ) ) ;
#102377 = CARTESIAN_POINT ( 'NONE',  ( 8.075468704329999525, 1426.465554857850066, 211.6438910379590084 ) ) ;
#102378 = LINE ( 'NONE', #101813, #1644 ) ;
#102379 = CARTESIAN_POINT ( 'NONE',  ( -14.53473304376390018, 1379.710786975620067, 208.2794084638009906 ) ) ;
#102380 = ORIENTED_EDGE ( 'NONE', *, *, #39933, .T. ) ;
#102381 = CARTESIAN_POINT ( 'NONE',  ( -3.081586005759989977, 1408.632027716779930, 270.4281154310780266 ) ) ;
#102382 = CARTESIAN_POINT ( 'NONE',  ( 4.804957937011430147, 1418.134047065659843, 233.3128310201539932 ) ) ;
#102383 = CARTESIAN_POINT ( 'NONE',  ( -0.3285615615811641188, 1508.336832367442184, 237.7487474441950042 ) ) ;
#102385 = ORIENTED_EDGE ( 'NONE', *, *, #87830, .T. ) ;
#102384 = CARTESIAN_POINT ( 'NONE',  ( 1.317811661047101568, 1517.051704408389924, 223.5300434977941677 ) ) ;
#102386 = ORIENTED_EDGE ( 'NONE', *, *, #62419, .F. ) ;
#102387 = CARTESIAN_POINT ( 'NONE',  ( -32.78250617288034618, 1511.187213306747708, 218.3079823578271430 ) ) ;
#102388 = CARTESIAN_POINT ( 'NONE',  ( -1.039113094294850104, 1409.452461688270205, 185.5619659655799865 ) ) ;
#102389 = CARTESIAN_POINT ( 'NONE',  ( -109.9849253298559972, 1384.914539739569818, 311.4561054518049446 ) ) ;
#102390 = CARTESIAN_POINT ( 'NONE',  ( -43.73460936356224238, 1430.821771421699395, 266.2442057452738595 ) ) ;
#102391 = CARTESIAN_POINT ( 'NONE',  ( -20.00429177317949936, 1474.940804442650006, 193.2183630961679910 ) ) ;
#102392 = CARTESIAN_POINT ( 'NONE',  ( -22.68195972959999906, 1425.804545574829945, 215.0649984192980071 ) ) ;
#102393 = CARTESIAN_POINT ( 'NONE',  ( 35.44508287519440159, 1462.853361191130034, 269.0528564058240022 ) ) ;
#102394 = CARTESIAN_POINT ( 'NONE',  ( -11.65263573226700089, 1391.913060387150153, 208.7517851132730016 ) ) ;
#102395 = CARTESIAN_POINT ( 'NONE',  ( 20.71343476517512627, 1524.726013923371283, 179.9059455038195381 ) ) ;
#102396 = CARTESIAN_POINT ( 'NONE',  ( 0.7356989345870019736, 1517.020847257979995, 205.6609797614169963 ) ) ;
#102397 = ORIENTED_EDGE ( 'NONE', *, *, #63863, .T. ) ;
#102398 = CARTESIAN_POINT ( 'NONE',  ( 18.25718033079806091, 1459.257182848304637, 227.8536879214166504 ) ) ;
#102399 = CARTESIAN_POINT ( 'NONE',  ( 1.022675170609709916, 1445.282598627109792, 199.0986583360879933 ) ) ;
#102400 = CARTESIAN_POINT ( 'NONE',  ( 15.69795926888880189, 1521.951704408389787, 222.7678737654429995 ) ) ;
#102401 = ORIENTED_EDGE ( 'NONE', *, *, #59297, .F. ) ;
#102403 = B_SPLINE_CURVE_WITH_KNOTS ( 'NONE', 3,
 ( #105122, #11063, #36811, #71002, #62039, #96164, #88318, #69889, #46344, #37365 ),
 .UNSPECIFIED., .F., .F.,
 ( 4, 2, 2, 2, 4 ),
 ( 0.000000000000000000, 0.0007189769279726045429, 0.001437953855945209086, 0.002156930783917813520, 0.002875907711890418172 ),
 .UNSPECIFIED. ) ;
#102402 = CARTESIAN_POINT ( 'NONE',  ( 3.440555586329999915, 1448.974144786239776, 184.1239056742980154 ) ) ;
#102404 = CARTESIAN_POINT ( 'NONE',  ( 27.01916100210560145, 1450.861483528779900, 136.4170495654999797 ) ) ;
#102405 = CARTESIAN_POINT ( 'NONE',  ( -4.836838691967080273, 1508.551704408389924, 212.4671294835000310 ) ) ;
#102406 = CARTESIAN_POINT ( 'NONE',  ( -18.61904574209999907, 1389.810251683270280, 216.3045377948590158 ) ) ;
#102407 = CARTESIAN_POINT ( 'NONE',  ( 8.190748369970000553, 1421.378881458010255, 196.0919654739990108 ) ) ;
#102408 = CARTESIAN_POINT ( 'NONE',  ( -0.5009090896308688867, 1432.030616873689951, 218.6088325375140187 ) ) ;
#102409 = CARTESIAN_POINT ( 'NONE',  ( -3.591208274099999986, 1495.697152948690018, 197.7417738467989921 ) ) ;
#102410 = CARTESIAN_POINT ( 'NONE',  ( 1.608553044152920108, 1408.969232297379904, 186.8221281591610250 ) ) ;
#102412 = CARTESIAN_POINT ( 'NONE',  ( 28.81652261710051022, 1526.349684470114198, 220.0454371960102549 ) ) ;
#102411 = CARTESIAN_POINT ( 'NONE',  ( 30.29139619032462249, 1523.843263703802677, 195.7510757159135721 ) ) ;
#102413 = CARTESIAN_POINT ( 'NONE',  ( -0.5779273184081697989, 1517.151704408390060, 186.0802614738061607 ) ) ;
#102414 = CARTESIAN_POINT ( 'NONE',  ( -11.84288296679999952, 1378.858663654499878, 213.2050210349089809 ) ) ;
#102415 = CARTESIAN_POINT ( 'NONE',  ( 2.471035510942662050, 1525.556090473913628, 241.2503633023762575 ) ) ;
#102416 = ORIENTED_EDGE ( 'NONE', *, *, #33520, .T. ) ;
#102417 = CARTESIAN_POINT ( 'NONE',  ( 11.99589392260669918, 1415.088136167450102, 221.1498175758559910 ) ) ;
#102418 = B_SPLINE_SURFACE_WITH_KNOTS ( 'NONE', 5, 1, ( 
 ( #73024, #4168 ),
 ( #63549, #55689 ),
 ( #72479, #63014 ),
 ( #28816, #20937 ),
 ( #107163, #3088 ),
 ( #89811, #106609 ),
 ( #30455, #64639 ),
 ( #22021, #29893 ),
 ( #3639, #71412 ),
 ( #98209, #13628 ),
 ( #21477, #47816 ),
 ( #81951, #73588 ),
 ( #14194, #14751 ),
 ( #24245, #74135 ),
 ( #5821, #66840 ),
 ( #108266, #75236 ),
 ( #91471, #33751 ),
 ( #15289, #31552 ),
 ( #65729, #92018 ),
 ( #67947, #58980 ),
 ( #58427, #48938 ),
 ( #57347, #6360 ),
 ( #40508, #83068 ),
 ( #75775, #42171 ) ),
 .UNSPECIFIED., .F., .F., .F.,
 ( 6, 3, 3, 3, 3, 3, 3, 6 ),
 ( 2, 2 ),
 ( 0.000000000000000000, 1.521747480829999999, 3.044513117910000233, 6.090044392050000255, 24.62876410220000167, 44.04928580589999854, 64.58019525850001230, 84.36259054880000008 ),
 ( 2.018291271429999867, 3.029411390890000000 ),
 .UNSPECIFIED. ) ;
#102419 = CARTESIAN_POINT ( 'NONE',  ( 11.45641041208300059, 1432.340941410350069, 151.2730070997519931 ) ) ;
#102420 = CARTESIAN_POINT ( 'NONE',  ( 31.79838993233245859, 1525.159177407155312, 202.0929476855948224 ) ) ;
#102421 = CARTESIAN_POINT ( 'NONE',  ( -14.33548952289999967, 1390.363893295419984, 208.3507362592630159 ) ) ;
#102422 = CARTESIAN_POINT ( 'NONE',  ( 9.255168820965479881, 1422.794170407699994, 212.0163054975980117 ) ) ;
#102423 = CARTESIAN_POINT ( 'NONE',  ( -35.12261413890779949, 1450.282964114529932, 136.2298589479320015 ) ) ;
#102424 = CARTESIAN_POINT ( 'NONE',  ( -11.00021946413910001, 1462.586022203469838, 208.1031543993230173 ) ) ;
#102425 = CARTESIAN_POINT ( 'NONE',  ( -14.73695825029999895, 1462.639194746130215, 255.3819207742980097 ) ) ;
#102426 = CARTESIAN_POINT ( 'NONE',  ( -8.905790132374109547, 1384.416626165959769, 218.6501556148870122 ) ) ;
#102427 = CARTESIAN_POINT ( 'NONE',  ( 11.86805344210000079, 1433.542299609339807, 150.5539803834979864 ) ) ;
#102428 = CARTESIAN_POINT ( 'NONE',  ( 1.554312234479999851E-15, 1455.844446582929777, 219.6133832206979832 ) ) ;
#102429 = CARTESIAN_POINT ( 'NONE',  ( -10.58089751883319884, 1462.237251693409917, 208.9718616002229794 ) ) ;
#102430 = CARTESIAN_POINT ( 'NONE',  ( -9.526209128037958607, 1423.233055757800230, 192.3205453756600036 ) ) ;
#102431 = CARTESIAN_POINT ( 'NONE',  ( 8.547027738309338929, 1419.998520249890134, 194.9826476886919977 ) ) ;
#102432 = CARTESIAN_POINT ( 'NONE',  ( 5.445195913439840218, 1467.322352123520204, 217.4938090916859892 ) ) ;
#102433 = CARTESIAN_POINT ( 'NONE',  ( 22.43804736130000066, 1409.696614266430061, 208.0348436616479830 ) ) ;
#102434 = CARTESIAN_POINT ( 'NONE',  ( 12.60060242696761179, 1398.286606401453810, 205.9241517394453638 ) ) ;
#102435 = CARTESIAN_POINT ( 'NONE',  ( -28.33771605659999793, 1510.031322598729957, 222.5657443468980148 ) ) ;
#102436 = CARTESIAN_POINT ( 'NONE',  ( -8.003970385414945099, 1425.916565961161268, 207.5703587753713748 ) ) ;
#102437 = CARTESIAN_POINT ( 'NONE',  ( -2.525349509968036088, 1476.996657561013308, 199.0229261902041173 ) ) ;
#102438 = DIRECTION ( 'NONE',  ( -1.000000000000000000, 0.000000000000000000, 0.000000000000000000 ) ) ;
#102439 = CARTESIAN_POINT ( 'NONE',  ( -1.842963895390000273, 1515.551704166990021, 205.1377641647089831 ) ) ;
#102440 = CARTESIAN_POINT ( 'NONE',  ( 4.873735476160000246, 1472.089320948289924, 218.0431589096889695 ) ) ;
#102441 = CARTESIAN_POINT ( 'NONE',  ( 20.33643746716989753, 1475.138452556609991, 218.0161092331550208 ) ) ;
#102442 = CARTESIAN_POINT ( 'NONE',  ( 6.948321705865000197, 1517.049325831759916, 213.1561268858870051 ) ) ;
#102443 = CARTESIAN_POINT ( 'NONE',  ( -17.10099446617070029, 1420.024199383779887, 206.1776963727390068 ) ) ;
#102444 = CARTESIAN_POINT ( 'NONE',  ( 0.1709732279705020175, 1479.758167021719828, 182.1047789143250100 ) ) ;
#102446 = ORIENTED_EDGE ( 'NONE', *, *, #80382, .T. ) ;
#102445 = CARTESIAN_POINT ( 'NONE',  ( -23.84533141485470153, 1452.080363065020038, 136.9869391916130041 ) ) ;
#102447 = CARTESIAN_POINT ( 'NONE',  ( -27.95977047539996718, 1444.740067931808653, 175.9996750486979238 ) ) ;
#102448 = DIRECTION ( 'NONE',  ( 0.7067700363771036720, 0.03085824620770448445, 0.7067700363771035610 ) ) ;
#102449 = CARTESIAN_POINT ( 'NONE',  ( 11.87909651009999834, 1433.311731933790043, 149.7888166638980181 ) ) ;
#102450 = CARTESIAN_POINT ( 'NONE',  ( -40.11569180352149999, 1438.966375984959768, 134.0999999981379744 ) ) ;
#102451 = CARTESIAN_POINT ( 'NONE',  ( -7.649966233313090669, 1508.551704408389924, 219.0282755267929815 ) ) ;
#102452 = VERTEX_POINT ( 'NONE', #91222 ) ;
#102453 = CARTESIAN_POINT ( 'NONE',  ( -11.40675845049999992, 1470.736590895890004, 209.2409589557610161 ) ) ;
#102454 = CARTESIAN_POINT ( 'NONE',  ( -12.46581701093480099, 1390.671825296710040, 212.4770441740029980 ) ) ;
#102455 = CARTESIAN_POINT ( 'NONE',  ( 7.294530591305462330, 1447.438264182228068, 203.6988537847500709 ) ) ;
#102456 = CARTESIAN_POINT ( 'NONE',  ( -22.03465957474533710, 1522.862737210649584, 235.4136513321633117 ) ) ;
#102457 = CARTESIAN_POINT ( 'NONE',  ( -3.982766651553749870, 1432.979116022980179, 216.7759890233299984 ) ) ;
#102458 = CARTESIAN_POINT ( 'NONE',  ( -15.56469051740000076, 1506.798305107229908, 193.1680121121979994 ) ) ;
#102459 = CARTESIAN_POINT ( 'NONE',  ( -14.99634941789999942, 1415.350563318459990, 212.7117730710989747 ) ) ;
#102460 = CARTESIAN_POINT ( 'NONE',  ( -13.48561158899999946, 1379.693418477929981, 211.4566258570390005 ) ) ;
#102461 = CARTESIAN_POINT ( 'NONE',  ( -11.90356457640000087, 1391.442765664790159, 205.8043614906389962 ) ) ;
#102462 = CARTESIAN_POINT ( 'NONE',  ( -84.88875595641219718, 1385.175798546129954, 288.6381895591889588 ) ) ;
#102463 = CARTESIAN_POINT ( 'NONE',  ( -18.15646965371402644, 1522.906363951597314, 238.1669781545290903 ) ) ;
#102464 = CARTESIAN_POINT ( 'NONE',  ( 10.46793285443070154, 1425.962962126699949, 207.8293122372670041 ) ) ;
#102465 = ORIENTED_EDGE ( 'NONE', *, *, #81705, .T. ) ;
#102466 = CARTESIAN_POINT ( 'NONE',  ( -29.29916111349999852, 1451.889927077430229, 134.8511816846980196 ) ) ;
#102467 = CARTESIAN_POINT ( 'NONE',  ( 12.53380499169999851, 1442.773887286369927, 169.4755105685979970 ) ) ;
#102468 = EDGE_CURVE ( 'NONE', #86629, #9574, #14503, .T. ) ;
#102470 = EDGE_LOOP ( 'NONE', ( #32423, #85043, #66971, #92437 ) ) ;
#102469 = CARTESIAN_POINT ( 'NONE',  ( 4.229167303610000594, 1436.983388288790138, 227.1518914930990150 ) ) ;
#102471 = CARTESIAN_POINT ( 'NONE',  ( 4.727292513470000124, 1474.107684878189957, 219.5305710966990205 ) ) ;
#102472 = CARTESIAN_POINT ( 'NONE',  ( 1.842962214803819831, 1515.372048948338943, 204.8601094092262542 ) ) ;
#102473 = CARTESIAN_POINT ( 'NONE',  ( -8.119505269034053896, 1363.763538997089199, 210.6218459617142003 ) ) ;
#102474 = CARTESIAN_POINT ( 'NONE',  ( -7.000192180139999998, 1494.404549418689840, 199.4211192133089980 ) ) ;
#102475 = EDGE_CURVE ( 'NONE', #25053, #67299, #59590, .T. ) ;
#102476 = CARTESIAN_POINT ( 'NONE',  ( 38.90393960482792579, 1452.456950825172953, 269.5913181406285730 ) ) ;
#102477 = CARTESIAN_POINT ( 'NONE',  ( -11.60004869885203682, 1426.786830457828273, 134.3786150874268799 ) ) ;
#102478 = CARTESIAN_POINT ( 'NONE',  ( 16.17654417561950098, 1432.051473137853691, 218.4400530825793396 ) ) ;
#102479 = CARTESIAN_POINT ( 'NONE',  ( 10887.13479812350670, -2340.220200558883789, -7120.152215564383368 ) ) ;
#102480 = CARTESIAN_POINT ( 'NONE',  ( 9.326190216649999698, 1450.430212708290128, 205.2552756270490022 ) ) ;
#102481 = CARTESIAN_POINT ( 'NONE',  ( -106.6287828259400072, 1306.483669372790018, 304.2218459572590064 ) ) ;
#102482 = CARTESIAN_POINT ( 'NONE',  ( -9.766226206179759117, 1367.813519127536438, 210.6218459617030021 ) ) ;
#102483 = CARTESIAN_POINT ( 'NONE',  ( -31.12456774391152337, 1525.960063244516959, 217.0912716842400698 ) ) ;
#102484 = CARTESIAN_POINT ( 'NONE',  ( -6.949574985774999547, 1517.102359858469754, 205.8627441332170065 ) ) ;
#102485 = CARTESIAN_POINT ( 'NONE',  ( 3.117854674740000220, 1446.609948951180058, 165.9235411017980084 ) ) ;
#102486 = DIRECTION ( 'NONE',  ( -1.755985294532469921E-16, 1.000000000000000000, -1.338183447452831989E-16 ) ) ;
#102487 = CARTESIAN_POINT ( 'NONE',  ( 14.35456882750000140, 1416.827520077930103, 196.6651910167979906 ) ) ;
#102489 = EDGE_LOOP ( 'NONE', ( #83369, #2115, #79483, #43454, #3264 ) ) ;
#102488 = CARTESIAN_POINT ( 'NONE',  ( -68.75469704279311145, 1379.747881236529793, 280.3330792319889611 ) ) ;
#102490 = DIRECTION ( 'NONE',  ( 0.000000000000000000, 0.07083107041538988513, -0.9974883254774514763 ) ) ;
#102491 = VERTEX_POINT ( 'NONE', #69364 ) ;
#102492 = CARTESIAN_POINT ( 'NONE',  ( -15.90990259576500065, 1512.830284628050094, 220.0820010595669771 ) ) ;
#102493 = CARTESIAN_POINT ( 'NONE',  ( -23.34982412229999937, 1410.912491278129892, 205.8672349166580204 ) ) ;
#102495 = CARTESIAN_POINT ( 'NONE',  ( 17.19010109773460115, 1410.596273358489725, 192.2276381356939794 ) ) ;
#102494 = CARTESIAN_POINT ( 'NONE',  ( -11.12799046640000178, 1426.892988489029904, 99.91667177869788929 ) ) ;
#102496 = CARTESIAN_POINT ( 'NONE',  ( 5.788097227154999302, 1517.099836525840146, 211.6039138304569747 ) ) ;
#102497 = EDGE_CURVE ( 'NONE', #98691, #22920, #14151, .T. ) ;
#102498 = CARTESIAN_POINT ( 'NONE',  ( 9.369692350036283202, 1509.366787681659162, 180.5745519987570162 ) ) ;
#102499 = CARTESIAN_POINT ( 'NONE',  ( 2.123651873717662841, 1450.063259378257044, 182.0352679771010003 ) ) ;
#102500 = CARTESIAN_POINT ( 'NONE',  ( -12.36522994357800087, 1378.525463850149890, 209.2776376259250242 ) ) ;
#102501 = CARTESIAN_POINT ( 'NONE',  ( 29.54414221403980179, 1509.931130577039994, 209.6497321865869878 ) ) ;
#102502 = CARTESIAN_POINT ( 'NONE',  ( -5.081549875360000357, 1391.866816797490173, 214.6180254208989879 ) ) ;
#102503 = CARTESIAN_POINT ( 'NONE',  ( -37.40887072121479662, 1438.171435685040024, 136.5752352137649837 ) ) ;
#102504 = VERTEX_POINT ( 'NONE', #62072 ) ;
#102505 = CARTESIAN_POINT ( 'NONE',  ( 10.77209975170500122, 1396.289230399710050, 213.2400182897270042 ) ) ;
#102506 = CARTESIAN_POINT ( 'NONE',  ( -19.15298488520000220, 1464.559837765089924, 213.8319524061190009 ) ) ;
#102507 = CARTESIAN_POINT ( 'NONE',  ( -17.26192056690000243, 1459.742557600430018, 228.3453419790980092 ) ) ;
#102508 = EDGE_LOOP ( 'NONE', ( #81858, #72670, #84335, #92206 ) ) ;
#102509 = ORIENTED_EDGE ( 'NONE', *, *, #59852, .T. ) ;
#102510 = CARTESIAN_POINT ( 'NONE',  ( -29.55500859232640209, 1509.961759442807761, 210.8697166764131339 ) ) ;
#102511 = CARTESIAN_POINT ( 'NONE',  ( 8.380162515710001259, 1425.070964763900065, 194.6834137014990063 ) ) ;
#102512 = DIRECTION ( 'NONE',  ( -0.4999999999998399058, 0.7071067811867739472, 0.4999999999998399058 ) ) ;
#102513 = CARTESIAN_POINT ( 'NONE',  ( -12.19226287358214833, 1417.436307414769544, 199.7077872052550731 ) ) ;
#102514 = CARTESIAN_POINT ( 'NONE',  ( 4.091836660730000297, 1515.531866980889845, 210.2412738621790140 ) ) ;
#102515 = CARTESIAN_POINT ( 'NONE',  ( -4.591899558935420345, 1455.336696413800155, 200.8800319518429944 ) ) ;
#102516 = CARTESIAN_POINT ( 'NONE',  ( -1.228114782090000023, 1461.197819184229957, 235.1858097754980008 ) ) ;
#102517 = DIRECTION ( 'NONE',  ( -1.987897879952545076E-13, 0.000000000000000000, 1.000000000000000000 ) ) ;
#102518 = CARTESIAN_POINT ( 'NONE',  ( 9.707000155197439639, 1452.234455235359974, 209.8042379339860020 ) ) ;
#102519 = CARTESIAN_POINT ( 'NONE',  ( -104.2765687246049993, 1384.887396391249922, 296.8490877439370479 ) ) ;
#102520 = ORIENTED_EDGE ( 'NONE', *, *, #37776, .T. ) ;
#102521 = CARTESIAN_POINT ( 'NONE',  ( 5.001338628314999646, 1516.911981270829983, 203.3378372969070256 ) ) ;
#102522 = CARTESIAN_POINT ( 'NONE',  ( 1.715109447055000125, 1516.963431999339946, 209.8570730874349977 ) ) ;
#102523 = ORIENTED_EDGE ( 'NONE', *, *, #42986, .T. ) ;
#102524 = CARTESIAN_POINT ( 'NONE',  ( 19.13172296059999766, 1454.817774558389829, 206.3490106532590005 ) ) ;
#102525 = CARTESIAN_POINT ( 'NONE',  ( 19.97245611310000157, 1487.538185644830037, 227.4393568152979981 ) ) ;
#102526 = ORIENTED_EDGE ( 'NONE', *, *, #21997, .T. ) ;
#102527 = CARTESIAN_POINT ( 'NONE',  ( -13.36059434050000050, 1414.988017874730076, 220.3623401557979946 ) ) ;
#102528 = CARTESIAN_POINT ( 'NONE',  ( -11.54407319952080080, 1432.339775637740104, 151.1365582528090101 ) ) ;
#102529 = CARTESIAN_POINT ( 'NONE',  ( -3.430374836980000008, 1431.708658569990121, 216.7924588047190184 ) ) ;
#102530 = CARTESIAN_POINT ( 'NONE',  ( -4.368232472647803455, 1488.977261507675621, 219.1147625199656375 ) ) ;
#102531 = CARTESIAN_POINT ( 'NONE',  ( -5.042932594320000739, 1422.466626064029924, 185.3903934186979825 ) ) ;
#102532 = CARTESIAN_POINT ( 'NONE',  ( 10.87756687473890160, 1470.161469495209985, 206.9927029381979935 ) ) ;
#102533 = CARTESIAN_POINT ( 'NONE',  ( -9.218333506580000503, 1473.255740393489759, 204.2345550927689999 ) ) ;
#102534 = CARTESIAN_POINT ( 'NONE',  ( 7.031363022279999875, 1494.605019377190047, 219.3119659920989761 ) ) ;
#102535 = CARTESIAN_POINT ( 'NONE',  ( -44.22148322110000151, 1379.678134692099775, 229.5078809691590038 ) ) ;
#102536 = AXIS2_PLACEMENT_3D ( 'NONE', #19701, #1832, #53904 ) ;
#102537 = CARTESIAN_POINT ( 'NONE',  ( 24.80387804530560203, 1461.773651900399955, 206.2179137791540029 ) ) ;
#102539 = DIRECTION ( 'NONE',  ( 0.000000000000000000, -0.9990482215818579093, 0.04361938736533144123 ) ) ;
#102538 = CARTESIAN_POINT ( 'NONE',  ( -21.68299751200000003, 1505.523879562090087, 209.6298452977370061 ) ) ;
#102540 = CARTESIAN_POINT ( 'NONE',  ( -4.529993016832083441, 1423.777408052882720, 184.3664072715177724 ) ) ;
#102541 = CARTESIAN_POINT ( 'NONE',  ( -3.472209666708114817, 1506.379719591498088, 187.4566518126731864 ) ) ;
#102542 = VERTEX_POINT ( 'NONE', #19473 ) ;
#102543 = CARTESIAN_POINT ( 'NONE',  ( -2.414372322354871425, 1486.072943997549146, 181.9601385338485500 ) ) ;
#102544 = CARTESIAN_POINT ( 'NONE',  ( 2.073027880074009399, 1516.528002108337205, 216.8307126571504284 ) ) ;
#102545 = CARTESIAN_POINT ( 'NONE',  ( -2.917573657582420044, 1484.880000574953101, 183.1918739895752140 ) ) ;
#102546 = DIRECTION ( 'NONE',  ( -0.000000000000000000, -1.000000000000000000, -0.000000000000000000 ) ) ;
#102548 = ORIENTED_EDGE ( 'NONE', *, *, #52715, .T. ) ;
#102547 = CARTESIAN_POINT ( 'NONE',  ( 0.08387812437511810160, 1515.158224561690076, 204.7948437802780006 ) ) ;
#102549 = CARTESIAN_POINT ( 'NONE',  ( 0.7253211429939999677, 1453.159462793229750, 188.7266509659980045 ) ) ;
#102550 = CARTESIAN_POINT ( 'NONE',  ( 173.8335085727383955, 1524.382868172863937, 100.8557906292069930 ) ) ;
#102551 = CARTESIAN_POINT ( 'NONE',  ( -11.53630120159999883, 1429.335606864229931, 150.4996243470979778 ) ) ;
#102552 = CARTESIAN_POINT ( 'NONE',  ( -10.85273938805417160, 1425.445994626150878, 147.0837058438643226 ) ) ;
#102553 = CARTESIAN_POINT ( 'NONE',  ( 2.392804902923610033, 1445.901086195959806, 199.3053874824840079 ) ) ;
#102554 = DIRECTION ( 'NONE',  ( -5.980589973904019347E-17, 1.000000000000000000, -1.736889445713099699E-16 ) ) ;
#102555 = CARTESIAN_POINT ( 'NONE',  ( -7.027669101106630123, 1426.313406588260023, 202.9938954506890241 ) ) ;
#102556 = CARTESIAN_POINT ( 'NONE',  ( 11.95011813770030429, 1433.524584343693277, 149.8874522332942547 ) ) ;
#102557 = B_SPLINE_CURVE_WITH_KNOTS ( 'NONE', 3,
 ( #18475, #35868, #34750, #44833, #70052, #27449, #78988, #33630, #67824, #101936, #25223, #2830, #57515, #48558, #91082, #46488, #36949, #39591, #31726, #28003, #29111, #28561, #79527, #63297, #65364, #65912, #36402, #73762, #11226, #23322, #104709, #89007, #62190, #62759, #91639, #37511, #53798, #96317, #97415, #99471 ),
 .UNSPECIFIED., .F., .F.,
 ( 4, 3, 3, 3, 3, 3, 3, 3, 3, 3, 3, 3, 3, 4 ),
 ( -1.512517454966539887, -1.431847012466620050, -1.315728653153140026, -1.197778018496070018, -1.078754818121699932, -0.9581669488396040713, -0.8368756102960169807, -0.7152076346036029264, -0.5935212885821531392, -0.4725472813379960613, -0.3524846561758310237, -0.2335963589277290087, -0.1160647746509679834, -2.220446049250313081E-16 ),
 .UNSPECIFIED. ) ;
#102558 = CARTESIAN_POINT ( 'NONE',  ( -11.60004869885203682, 0.000000000000000000, 137.0999999980979851 ) ) ;
#102560 = CARTESIAN_POINT ( 'NONE',  ( -10.99409911865420142, 1481.669864629989888, 208.2822106822179933 ) ) ;
#102559 = CARTESIAN_POINT ( 'NONE',  ( -20.30114903109999958, 1470.087487068429937, 225.8186208082980215 ) ) ;
#102561 = CARTESIAN_POINT ( 'NONE',  ( -121.3990240114689385, 1384.913060387289988, 304.3468054064544503 ) ) ;
#102562 = VERTEX_POINT ( 'NONE', #36838 ) ;
#102563 = CARTESIAN_POINT ( 'NONE',  ( -3.462620856235000044, 1516.938330505699923, 206.6435391121569864 ) ) ;
#102564 = CARTESIAN_POINT ( 'NONE',  ( 14.47246893939999879, 1408.205947428329864, 269.4256199600980040 ) ) ;
#102565 = CARTESIAN_POINT ( 'NONE',  ( 24.39393896809999873, 1435.492404634590002, 137.6392883061979830 ) ) ;
#102566 = CARTESIAN_POINT ( 'NONE',  ( 18.47093090970000162, 1430.306966399830117, 192.6788482552979929 ) ) ;
#102567 = CYLINDRICAL_SURFACE ( 'NONE', #108929, 2.000000000000001332 ) ;
#102568 = CARTESIAN_POINT ( 'NONE',  ( -10.39150615120248489, 1390.644890799487484, 215.8008389675831893 ) ) ;
#102569 = CARTESIAN_POINT ( 'NONE',  ( 22.51756156282889876, 1509.699390964210124, 227.9212218486820234 ) ) ;
#102570 = CARTESIAN_POINT ( 'NONE',  ( 4.725705173089999711, 1464.404288624430137, 236.3620497209980158 ) ) ;
#102571 = CARTESIAN_POINT ( 'NONE',  ( -16.02532890700000223, 1417.348757203270225, 206.0160147869889897 ) ) ;
#102572 = CARTESIAN_POINT ( 'NONE',  ( -13.47130175449999889, 1444.268114455909881, 187.0193666120979685 ) ) ;
#102573 = CARTESIAN_POINT ( 'NONE',  ( -2.170627987649289992, 1485.611815795640041, 197.4219879416550327 ) ) ;
#102574 = DIRECTION ( 'NONE',  ( 1.000000000000000000, -0.000000000000000000, 0.000000000000000000 ) ) ;
#102575 = CARTESIAN_POINT ( 'NONE',  ( 44.93133208270179324, 1436.268902546335994, 269.6838198007974370 ) ) ;
#102576 = ORIENTED_EDGE ( 'NONE', *, *, #97273, .F. ) ;
#102577 = CARTESIAN_POINT ( 'NONE',  ( 1.458127919845290110, 1497.749922849950053, 181.5217294836100166 ) ) ;
#102578 = CARTESIAN_POINT ( 'NONE',  ( -13.17864806199019867, 1409.373268918529902, 216.1559522034339977 ) ) ;
#102579 = CARTESIAN_POINT ( 'NONE',  ( -11.84975450817150033, 1508.199963107450003, 208.6376032033030015 ) ) ;
#102580 = CARTESIAN_POINT ( 'NONE',  ( 3.829620113550000315, 1515.051704408389924, 209.0973262533439936 ) ) ;
#102581 = CARTESIAN_POINT ( 'NONE',  ( -9.928260447259999566, 1475.299515453429876, 267.4967718279980318 ) ) ;
#102582 = DIRECTION ( 'NONE',  ( 0.2254368866614593903, -0.7071067811863919195, -0.6702075873433606112 ) ) ;
#102583 = CARTESIAN_POINT ( 'NONE',  ( -14.75867395745958000, 1514.537581216768785, 192.8458395396856986 ) ) ;
#102584 = CARTESIAN_POINT ( 'NONE',  ( 18.02593473381579514, 1424.491817304190135, 224.3631323497979793 ) ) ;
#102585 = CARTESIAN_POINT ( 'NONE',  ( -79.98755288028320365, 1384.638602750850168, 303.8468171847529788 ) ) ;
#102586 = CARTESIAN_POINT ( 'NONE',  ( -24.55973745244772388, 1437.066950768452216, 210.6038051167893173 ) ) ;
#102587 = CARTESIAN_POINT ( 'NONE',  ( -3.312638106410000116, 1440.449723275869928, 155.6633363266980155 ) ) ;
#102588 = CARTESIAN_POINT ( 'NONE',  ( -106.5446895480000080, 1379.366632456400112, 300.3036432984590078 ) ) ;
#102589 = CARTESIAN_POINT ( 'NONE',  ( 9.803834995107230554, 1522.051704408389924, 221.6221720662910002 ) ) ;
#102590 = DIRECTION ( 'NONE',  ( 0.7074300732568278294, 0.02470400251969398497, 0.7063514732138287400 ) ) ;
#102591 = CARTESIAN_POINT ( 'NONE',  ( -23.77655729059999956, 1410.665078721029886, 207.4249854038280034 ) ) ;
#102592 = CARTESIAN_POINT ( 'NONE',  ( 17.27701498020000059, 1415.425644477329797, 206.3581100805980100 ) ) ;
#102593 = CARTESIAN_POINT ( 'NONE',  ( 4.798101961140000427, 1484.634215563789894, 219.1327562436990206 ) ) ;
#102594 = CARTESIAN_POINT ( 'NONE',  ( 4.416167311050000599, 1423.572941315969956, 193.9044136913989860 ) ) ;
#102595 = DIRECTION ( 'NONE',  ( 0.000000000000000000, 0.000000000000000000, -1.000000000000000000 ) ) ;
#102596 = CARTESIAN_POINT ( 'NONE',  ( 11.44399576807470176, 1434.340548105539938, 225.7446294064320114 ) ) ;
#102597 = CARTESIAN_POINT ( 'NONE',  ( 17.42134945962404657, 1525.253972588461465, 181.0775141427824337 ) ) ;
#102598 = CARTESIAN_POINT ( 'NONE',  ( -7.544890056106759779, 1384.926148859619843, 219.0875905756669795 ) ) ;
#102600 = DIRECTION ( 'NONE',  ( -0.7054602837451257047, 1.421085471461279404E-14, -0.7087494536564008518 ) ) ;
#102599 = CARTESIAN_POINT ( 'NONE',  ( -22.50660609259999845, 1409.865199589130043, 210.7488977859379986 ) ) ;
#102601 = CARTESIAN_POINT ( 'NONE',  ( 11.69802026906100068, 1426.721460024069984, 141.3784292230029678 ) ) ;
#102602 = CARTESIAN_POINT ( 'NONE',  ( -2.919081270098979441, 1368.383855509380055, 210.4211783971049954 ) ) ;
#102603 = CARTESIAN_POINT ( 'NONE',  ( -1.491506560153236682, 1511.187213306747708, 242.6732489767341576 ) ) ;
#102604 = CARTESIAN_POINT ( 'NONE',  ( 5.749238445798059871, 1447.708474149499807, 200.6605380239639942 ) ) ;
#102605 = CIRCLE ( 'NONE', #93657, 1.000000000000001332 ) ;
#102606 = FACE_OUTER_BOUND ( 'NONE', #10540, .T. ) ;
#102607 = CARTESIAN_POINT ( 'NONE',  ( 7.325541787135000149, 1516.710692850270107, 204.1167749238070144 ) ) ;
#102608 = CARTESIAN_POINT ( 'NONE',  ( -10.12929865658589890, 1398.213355889394961, 217.3039673584101479 ) ) ;
#102609 = CARTESIAN_POINT ( 'NONE',  ( -0.1955981723043500320, 1414.913060387329779, 193.0575580317509718 ) ) ;
#102610 = FACE_BOUND ( 'NONE', #17745, .T. ) ;
#102611 = CARTESIAN_POINT ( 'NONE',  ( -18.45185438929999933, 1430.290683276829895, 194.4308410190979828 ) ) ;
#102612 = CARTESIAN_POINT ( 'NONE',  ( 5.476215863316349797, 1506.245585586920015, 219.4133328000820029 ) ) ;
#102613 = VECTOR ( 'NONE', #54495, 1000.000000000000000 ) ;
#102615 = ORIENTED_EDGE ( 'NONE', *, *, #52796, .T. ) ;
#102614 = CARTESIAN_POINT ( 'NONE',  ( -61.32702018127960031, 1379.729903114180161, 268.3509515309739868 ) ) ;
#102616 = ORIENTED_EDGE ( 'NONE', *, *, #34092, .F. ) ;
#102617 = CARTESIAN_POINT ( 'NONE',  ( 11.61080405201120058, 1434.661580301569984, 151.3319073679200244 ) ) ;
#102618 = CARTESIAN_POINT ( 'NONE',  ( 21.95754362317981290, 1524.412928176728883, 184.5446601790259820 ) ) ;
#102619 = ORIENTED_EDGE ( 'NONE', *, *, #65180, .T. ) ;
#102620 = CARTESIAN_POINT ( 'NONE',  ( -107.2961829519999952, 1379.578066573650176, 309.1743912152589928 ) ) ;
#102621 = CARTESIAN_POINT ( 'NONE',  ( -10.36068074410219886, 1448.206033820939865, 208.6438493282829825 ) ) ;
#102622 = DIRECTION ( 'NONE',  ( 0.02616798426500960631, 0.9993150019883682011, 0.02616798426500950570 ) ) ;
#102624 = CARTESIAN_POINT ( 'NONE',  ( 13.64449414243759939, 1453.162678562290012, 224.5410799634850036 ) ) ;
#102623 = CARTESIAN_POINT ( 'NONE',  ( -17.38483621660000011, 1410.884422118429939, 225.7833436061980024 ) ) ;
#102625 = CARTESIAN_POINT ( 'NONE',  ( 19.34051166222370099, 1498.116123037349780, 229.0881779061390091 ) ) ;
#102626 = CARTESIAN_POINT ( 'NONE',  ( 16.93884295710000387, 1507.634939731529812, 188.0954314088980084 ) ) ;
#102627 = CARTESIAN_POINT ( 'NONE',  ( -0.3610880125209999791, 1416.520646107730045, 191.0797029597979986 ) ) ;
#102628 = DIRECTION ( 'NONE',  ( -0.6736849260863841948, 0.000000000000000000, 0.7390186874254148774 ) ) ;
#102629 = B_SPLINE_SURFACE_WITH_KNOTS ( 'NONE', 5, 5, ( 
 ( #36019, #104314, #27607, #19174, #70756, #62345, #96470, #19749, #30898, #3537, #90250, #80770 ),
 ( #4078, #88632, #88084, #39308, #46637, #97569, #81299, #80219, #38203, #28713, #56116, #55586 ),
 ( #106515, #107064, #30349, #13532, #12988, #47171, #11911, #4614, #55037, #21377, #37660, #64540 ),
 ( #89164, #73480, #71866, #38748, #97029, #72386, #105983, #72925, #98657, #21921, #37108, #29804 ),
 ( #62919, #98103, #89710, #47718, #81849, #11372, #12455, #20292, #5152, #107616, #65077, #29259 ),
 ( #99192, #63992, #22472, #45543, #79683, #2989, #71309, #105422, #54496, #46087, #63450, #20841 ),
 ( #24541, #51990, #50880, #9424, #43038, #77195, #25096, #43587, #84473, #51428, #109679, #33495 ),
 ( #69357, #76625, #49783, #102369, #7760, #8306, #34069, #41927, #41379, #85012, #35174, #58729 ),
 ( #77736, #497, #93967, #76083, #68261, #83916, #32955, #101805, #59302, #92310, #67144, #85558 ),
 ( #103467, #7221, #93416, #110221, #1049, #50348, #25652, #67696, #8855, #59843, #16683, #42467 ),
 ( #110778, #17234, #34622, #68806, #102908, #101242, #26207, #60396, #94515, #17790, #86131, #56672 ),
 ( #15581, #75543, #92865, #16144, #37949, #105147, #26774, #28437, #11097, #36835, #12178, #60961 ) ),
 .UNSPECIFIED., .F., .F., .F.,
 ( 6, 3, 3, 6 ),
 ( 6, 3, 3, 6 ),
 ( 13.14947839535670049, 14.22551365930000067, 16.37671448909999938, 17.67727092117560161 ),
 ( -0.0005573452897113489839, 0.3064376381380000125, 0.9193129144130000041, 1.583189345828600159 ),
 .UNSPECIFIED. ) ;
#102630 = CARTESIAN_POINT ( 'NONE',  ( -1.701027861004999808, 1516.937508036699910, 211.6166039682370013 ) ) ;
#102631 = DIRECTION ( 'NONE',  ( 0.000000000000000000, 0.000000000000000000, -1.000000000000000000 ) ) ;
#102632 = CARTESIAN_POINT ( 'NONE',  ( 13.49369409791039942, 1415.034069335220238, 197.8294454127749873 ) ) ;
#102633 = CARTESIAN_POINT ( 'NONE',  ( 11.86544875260000076, 1432.297029634840101, 150.3972660524979972 ) ) ;
#102634 = CARTESIAN_POINT ( 'NONE',  ( 8.191860436744999419, 1512.696049264740168, 202.1234250822469960 ) ) ;
#102635 = ORIENTED_EDGE ( 'NONE', *, *, #109619, .F. ) ;
#102636 = CARTESIAN_POINT ( 'NONE',  ( 13.72147666485579975, 1434.975561705699874, 148.6099413304839914 ) ) ;
#102637 = ORIENTED_EDGE ( 'NONE', *, *, #61635, .T. ) ;
#102638 = EDGE_LOOP ( 'NONE', ( #94656, #7542, #23031, #42010 ) ) ;
#102639 = EDGE_CURVE ( 'NONE', #17126, #33889, #5110, .T. ) ;
#102640 = CARTESIAN_POINT ( 'NONE',  ( 13.33628935843344543, 1444.532992900501313, 169.3750409159077037 ) ) ;
#102641 = CARTESIAN_POINT ( 'NONE',  ( -0.3266743759550000403, 1466.747038422030073, 235.5969264059980333 ) ) ;
#102642 = CARTESIAN_POINT ( 'NONE',  ( -8.351543752122086772, 1474.679204586614105, 203.1296262194932467 ) ) ;
#102643 = CARTESIAN_POINT ( 'NONE',  ( 0.7526715501680020237, 1516.710624944440042, 216.8354948044169817 ) ) ;
#102644 = CARTESIAN_POINT ( 'NONE',  ( -8.115358832489173224, 1511.538143004863514, 212.8694838649076928 ) ) ;
#102645 = STYLED_ITEM ( 'NONE', ( #22205 ), #9778 ) ;
#102646 = CARTESIAN_POINT ( 'NONE',  ( -18.63123577993770752, 1445.268454213514360, 213.9833683865410308 ) ) ;
#102647 = CARTESIAN_POINT ( 'NONE',  ( -35.12950831648389993, 1379.640695976296456, 218.1006992214701086 ) ) ;
#102648 = CARTESIAN_POINT ( 'NONE',  ( -11.59474938690000023, 1376.271391995119984, 207.1178716385390146 ) ) ;
#102649 = ORIENTED_EDGE ( 'NONE', *, *, #2971, .F. ) ;
#102650 = CARTESIAN_POINT ( 'NONE',  ( 3.445685077385000294, 1516.778761582560037, 206.6297153089269898 ) ) ;
#102651 = ORIENTED_EDGE ( 'NONE', *, *, #65051, .F. ) ;
#102652 = CARTESIAN_POINT ( 'NONE',  ( -104.4921371840429885, 1379.706968095510092, 304.0176578806480165 ) ) ;
#102653 = CARTESIAN_POINT ( 'NONE',  ( -113.4000000000000057, 1306.913060387289988, 304.2218459572590064 ) ) ;
#102654 = ORIENTED_EDGE ( 'NONE', *, *, #64704, .F. ) ;
#102655 = CARTESIAN_POINT ( 'NONE',  ( -12.07537077539999970, 1409.501584340330055, 189.8778375757980257 ) ) ;
#102656 = CARTESIAN_POINT ( 'NONE',  ( 7.468172848634999639, 1513.423632355050131, 215.5921778456470008 ) ) ;
#102658 = VERTEX_POINT ( 'NONE', #61515 ) ;
#102657 = CARTESIAN_POINT ( 'NONE',  ( -4.738498500012391368, 1427.169020172040746, 134.0999999980979851 ) ) ;
#102659 = CARTESIAN_POINT ( 'NONE',  ( 24.27347683669999867, 1436.628682044180096, 213.1746251037879745 ) ) ;
#102660 = CARTESIAN_POINT ( 'NONE',  ( -13.70184035893560015, 1508.551704408389924, 210.3434241671160123 ) ) ;
#102661 = CARTESIAN_POINT ( 'NONE',  ( -113.4000000000000057, 1384.024049419740095, 311.1211866832589976 ) ) ;
#102662 = CARTESIAN_POINT ( 'NONE',  ( 4.500000000000000000, 1425.929641636930000, 183.3886486283980162 ) ) ;
#102663 = CARTESIAN_POINT ( 'NONE',  ( 21.30823923614893189, 1524.382868172804365, 184.4507411017295908 ) ) ;
#102664 = B_SPLINE_SURFACE_WITH_KNOTS ( 'NONE', 5, 1, ( 
 ( #4087, #12995 ),
 ( #29267, #90258 ),
 ( #71318, #47178 ),
 ( #13541, #64000 ),
 ( #28166, #98111 ),
 ( #88093, #38211 ),
 ( #81859, #21386 ),
 ( #47726, #63459 ),
 ( #73489, #4623 ),
 ( #5160, #11380 ),
 ( #55595, #45552 ),
 ( #72932, #62354 ),
 ( #79692, #2997 ),
 ( #37118, #107072 ),
 ( #105432, #105991 ),
 ( #20849, #28721 ),
 ( #89718, #62927 ),
 ( #54505, #20301 ),
 ( #11918, #46096 ),
 ( #80227, #37670 ),
 ( #97578, #55045 ),
 ( #89172, #12463 ),
 ( #58331, #67297 ),
 ( #6801, #101389 ),
 ( #24684, #84612 ),
 ( #40961, #108167 ),
 ( #75140, #49380 ),
 ( #33108, #41528 ),
 ( #15727, #109288 ),
 ( #39869, #82968 ),
 ( #22479, #65086 ),
 ( #32573, #31458 ),
 ( #66748, #57251 ),
 ( #74587, #30908 ),
 ( #48286, #92456 ),
 ( #74035, #65638 ),
 ( #66202, #49928 ),
 ( #84065, #14097 ),
 ( #7905, #99754 ),
 ( #99200, #100851 ),
 ( #107625, #23044 ),
 ( #91378, #93012 ),
 ( #56679, #100322 ),
 ( #83507, #109827 ),
 ( #24141, #48845 ),
 ( #6262, #7363 ),
 ( #40410, #90815 ),
 ( #82430, #75686 ),
 ( #5726, #14657 ),
 ( #108723, #32013 ),
 ( #23606, #57794 ) ),
 .UNSPECIFIED., .F., .F., .F.,
 ( 6, 3, 3, 3, 3, 3, 3, 3, 3, 3, 3, 3, 3, 3, 3, 3, 6 ),
 ( 2, 2 ),
 ( 0.000000000000000000, 28.69702819429999963, 61.04778752440000034, 93.62768910810000023, 123.7336603250000024, 156.1762685979999787, 187.3272846180000215, 220.4669312460000015, 237.3878297990000021, 254.2938300590000154, 289.2398204710000300, 325.3030936050000150, 360.8626869010000178, 395.8828220460000011, 432.6128460950000090, 468.8934854820000169, 502.1482307969999965 ),
 ( -1.776356839400000001E-15, 2.001751835784610023 ),
 .UNSPECIFIED. ) ;
#102665 = CARTESIAN_POINT ( 'NONE',  ( -4.613762395014999740, 1516.939574742129935, 214.9064842900469898 ) ) ;
#102666 = CARTESIAN_POINT ( 'NONE',  ( -3.247779998094530107, 1428.782300086839996, 200.3378027425290213 ) ) ;
#102667 = CARTESIAN_POINT ( 'NONE',  ( -22.27620224390000203, 1509.702625319529943, 189.6894443050980215 ) ) ;
#102669 = EDGE_CURVE ( 'NONE', #39464, #42444, #99976, .T. ) ;
#102668 = CARTESIAN_POINT ( 'NONE',  ( 22.08327125186925954, 1523.604703353109699, 184.4267662568470598 ) ) ;
#102670 = CARTESIAN_POINT ( 'NONE',  ( -7.321455911854999776, 1516.545806094630279, 211.6076919691270177 ) ) ;
#102671 = EDGE_CURVE ( 'NONE', #2310, #23969, #43518, .T. ) ;
#102672 = CARTESIAN_POINT ( 'NONE',  ( 13.75903549669999926, 1409.893112527829999, 191.3057326489980028 ) ) ;
#102673 =( BOUNDED_CURVE ( )  B_SPLINE_CURVE ( 3, ( #26237, #102395, #103499, #32982 ),
 .UNSPECIFIED., .F., .F. ) 
 B_SPLINE_CURVE_WITH_KNOTS ( ( 4, 4 ),
 ( 3.141592653589793116, 4.712388980384689674 ),
 .UNSPECIFIED. ) 
 CURVE ( )  GEOMETRIC_REPRESENTATION_ITEM ( )  RATIONAL_B_SPLINE_CURVE ( ( 1.000000000000000000, 0.8047378541243649375, 0.8047378541243649375, 1.000000000000000000 ) ) 
 REPRESENTATION_ITEM ( '' )  );
#102674 = CARTESIAN_POINT ( 'NONE',  ( -18.04045458515061995, 1486.173875672780696, 188.5074830145843521 ) ) ;
#102675 = EDGE_CURVE ( 'NONE', #31992, #944, #40929, .T. ) ;
#102677 = ORIENTED_EDGE ( 'NONE', *, *, #110075, .F. ) ;
#102676 = CARTESIAN_POINT ( 'NONE',  ( -57.30562384310000112, 1388.282717979049949, 240.5566957094589782 ) ) ;
#102678 = CARTESIAN_POINT ( 'NONE',  ( -64.31586160255349682, 1385.046231101620151, 287.7684490242009474 ) ) ;
#102679 = CARTESIAN_POINT ( 'NONE',  ( 36.52134894070000115, 1445.557347021360101, 254.5790014346980286 ) ) ;
#102680 = ADVANCED_FACE ( 'NONE', ( #43043 ), #66877, .F. ) ;
#102681 = CARTESIAN_POINT ( 'NONE',  ( -22.08327125186908191, 1523.604703353109699, 233.8169256665491105 ) ) ;
#102682 = CARTESIAN_POINT ( 'NONE',  ( -2.409034624560000282, 1511.999350511789999, 206.7128113371389873 ) ) ;
#102683 = CARTESIAN_POINT ( 'NONE',  ( -1.547605067268360113, 1508.721288987890148, 238.0070242337440050 ) ) ;
#102684 = CARTESIAN_POINT ( 'NONE',  ( -23.70328061310000223, 1446.840119191189842, 215.0759071426080311 ) ) ;
#102685 = TOROIDAL_SURFACE ( 'NONE', #70536, 5.868098490439999537, 1.000000000000000000 ) ;
#102687 = CARTESIAN_POINT ( 'NONE',  ( 19.24600158930000049, 1456.014086358630038, 226.4361891347980134 ) ) ;
#102686 = CARTESIAN_POINT ( 'NONE',  ( 0.7526715501680020237, 1516.710624944440042, 216.8354948044169817 ) ) ;
#102688 = CARTESIAN_POINT ( 'NONE',  ( -9.936111480414750119, 1448.113236486630058, 209.3298349216750012 ) ) ;
#102689 = CARTESIAN_POINT ( 'NONE',  ( -108.6994105457680035, 1383.219165405780132, 310.9122041113990349 ) ) ;
#102690 = ORIENTED_EDGE ( 'NONE', *, *, #98671, .T. ) ;
#102691 = CARTESIAN_POINT ( 'NONE',  ( 1.123101578415000024, 1517.157901477309906, 203.3331546065870157 ) ) ;
#102692 = CARTESIAN_POINT ( 'NONE',  ( 0.2144067139459999993, 1406.265208649629812, 269.2947081879980260 ) ) ;
#102693 = CARTESIAN_POINT ( 'NONE',  ( 28.27139721233038827, 1526.382868172863937, 198.6830693683571667 ) ) ;
#102694 = AXIS2_PLACEMENT_3D ( 'NONE', #6188, #83439, #7297 ) ;
#102695 = CARTESIAN_POINT ( 'NONE',  ( 12.82945534090000095, 1428.689089259029743, 223.8443168781979864 ) ) ;
#102696 = CARTESIAN_POINT ( 'NONE',  ( -13.59512407998240135, 1507.703338069740084, 209.3532897553030239 ) ) ;
#102697 = EDGE_CURVE ( 'NONE', #29992, #51216, #80339, .T. ) ;
#102698 = CARTESIAN_POINT ( 'NONE',  ( 3.409085372019999838, 1467.742650992889821, 218.4995240695689915 ) ) ;
#102699 = CARTESIAN_POINT ( 'NONE',  ( -1.431952011063330366, 1469.731770489434439, 219.0844453393653168 ) ) ;
#102700 = CARTESIAN_POINT ( 'NONE',  ( 27.07063991995919849, 1435.441545612230129, 135.7158103180489945 ) ) ;
#102701 = CARTESIAN_POINT ( 'NONE',  ( 37.56297661588190095, 1449.170392729680088, 136.3356801895480146 ) ) ;
#102702 = CARTESIAN_POINT ( 'NONE',  ( -31.98368035039945312, 1465.292284392873171, 269.3160916878242688 ) ) ;
#102703 = CARTESIAN_POINT ( 'NONE',  ( -1.785930250549999876, 1430.082233120889896, 200.6040445722289860 ) ) ;
#102704 = CARTESIAN_POINT ( 'NONE',  ( -4.148647832312248873, 1448.210448412289907, 185.1107006651311906 ) ) ;
#102705 = CARTESIAN_POINT ( 'NONE',  ( -21.92050665148230237, 1524.523992613103019, 184.5693265961525640 ) ) ;
#102706 = EDGE_CURVE ( 'NONE', #12743, #22102, #60996, .T. ) ;
#102707 = CARTESIAN_POINT ( 'NONE',  ( -1.892509460324644843, 1445.288012513316517, 217.9545851404853352 ) ) ;
#102708 = ORIENTED_EDGE ( 'NONE', *, *, #110303, .F. ) ;
#102709 = CARTESIAN_POINT ( 'NONE',  ( 0.5238716634341910039, 1409.870337634420139, 185.0929748826949890 ) ) ;
#102710 = CARTESIAN_POINT ( 'NONE',  ( 12.91347167809999874, 1434.774310044250115, 146.4344529612980068 ) ) ;
#102711 = ADVANCED_FACE ( 'NONE', ( #49421 ), #23900, .F. ) ;
#102712 = CARTESIAN_POINT ( 'NONE',  ( -3.910153998790829810, 1508.551704408439946, 213.9552835279250189 ) ) ;
#102713 = CARTESIAN_POINT ( 'NONE',  ( 15.47406948735730126, 1461.410564919109902, 189.5408260342219933 ) ) ;
#102714 = CARTESIAN_POINT ( 'NONE',  ( 10.88562390665740054, 1424.831925956591249, 138.2234943703446390 ) ) ;
#102716 = DIRECTION ( 'NONE',  ( 1.000000000000000000, 0.000000000000000000, 0.000000000000000000 ) ) ;
#102715 = CARTESIAN_POINT ( 'NONE',  ( 5.662343758720000508, 1504.894618425089902, 220.5557215505990314 ) ) ;
#102717 = CARTESIAN_POINT ( 'NONE',  ( -29.24528536989999949, 1509.871747141630067, 209.9183570146090005 ) ) ;
#102718 = CIRCLE ( 'NONE', #49224, 27.48039273450891073 ) ;
#102719 = CARTESIAN_POINT ( 'NONE',  ( 7.786809421259999198, 1425.366053415200213, 211.4289136434089755 ) ) ;
#102720 = CARTESIAN_POINT ( 'NONE',  ( -10.33108858841420030, 1384.889309772979914, 218.7842458343939995 ) ) ;
#102721 = CARTESIAN_POINT ( 'NONE',  ( 42.28240996344969460, 1440.913018452919914, 269.8809620301270229 ) ) ;
#102722 = CARTESIAN_POINT ( 'NONE',  ( -15.03694588066141868, 1451.150679764012921, 149.6984823041283335 ) ) ;
#102723 = CARTESIAN_POINT ( 'NONE',  ( -6.356619906689999766, 1483.629449051089978, 200.3071127286890203 ) ) ;
#102724 = CARTESIAN_POINT ( 'NONE',  ( 25.15255372800000089, 1436.299077768329880, 137.5035669820980218 ) ) ;
#102725 = CARTESIAN_POINT ( 'NONE',  ( -11.00145890658190062, 1396.297239797879911, 207.8695728886200129 ) ) ;
#102726 = ORIENTED_EDGE ( 'NONE', *, *, #25079, .F. ) ;
#102727 = VECTOR ( 'NONE', #957, 1000.000000000000000 ) ;
#102728 = CARTESIAN_POINT ( 'NONE',  ( -17.17297594112050163, 1410.145097443089981, 225.7364921415430103 ) ) ;
#102729 = CARTESIAN_POINT ( 'NONE',  ( 2.471608048749999842, 1438.194204504490017, 150.4833623973980252 ) ) ;
#102730 = VERTEX_POINT ( 'NONE', #78474 ) ;
#102731 = ORIENTED_EDGE ( 'NONE', *, *, #33237, .F. ) ;
#102732 = DIRECTION ( 'NONE',  ( 1.149679124779773953E-17, 1.000000000000000000, -1.829746454213089849E-16 ) ) ;
#102733 = CARTESIAN_POINT ( 'NONE',  ( -15.24330594657070748, 1416.048311171039131, 206.3693755384788062 ) ) ;
#102735 = CARTESIAN_POINT ( 'NONE',  ( -3.179033943583710276, 1457.997354099609993, 219.3203918230290128 ) ) ;
#102734 = CARTESIAN_POINT ( 'NONE',  ( 0.4151546846821903003, 1501.977400791986611, 175.3106345060153046 ) ) ;
#102736 = CARTESIAN_POINT ( 'NONE',  ( 24.01654869009999871, 1411.112688614930221, 209.9218154780569989 ) ) ;
#102737 = CARTESIAN_POINT ( 'NONE',  ( 4.164654618643389483, 1424.779710594659946, 185.0949776876690009 ) ) ;
#102738 = CARTESIAN_POINT ( 'NONE',  ( -2.604853897581669742, 1420.561510432767136, 185.7674481731004050 ) ) ;
#102739 = CARTESIAN_POINT ( 'NONE',  ( 7.901854723500001398, 1423.732064818020035, 212.4548200391890020 ) ) ;
#102740 = CARTESIAN_POINT ( 'NONE',  ( 20.81805062950000362, 1457.016307409189949, 206.8942079858889826 ) ) ;
#102741 = CARTESIAN_POINT ( 'NONE',  ( 8.460916142840000376, 1509.208523567629982, 181.0428522260980060 ) ) ;
#102742 = CARTESIAN_POINT ( 'NONE',  ( 3.649946445679999485, 1449.553923602460145, 184.1602381183980128 ) ) ;
#102743 = B_SPLINE_SURFACE_WITH_KNOTS ( 'NONE', 5, 5, ( 
 ( #28031, #1760, #44303, #62220, #45415, #27475 ),
 ( #43196, #61129, #9570, #35898, #79558, #61666 ),
 ( #2856, #17957, #60565, #103069, #19624, #26940 ),
 ( #95242, #104742, #77892, #96347, #95790, #36979 ),
 ( #105295, #28586, #78446, #36430, #34781, #18506 ),
 ( #52704, #77348, #26370, #86838, #87401, #94685 ) ),
 .UNSPECIFIED., .F., .F., .F.,
 ( 6, 6 ),
 ( 6, 6 ),
 ( 5.893388896116969811, 9.819930328983028645 ),
 ( -0.0002947352030313690231, 0.5000000000000000000 ),
 .UNSPECIFIED. ) ;
#102744 = CARTESIAN_POINT ( 'NONE',  ( 8.899640782778483583, 1364.433807194531028, 207.6218459616988241 ) ) ;
#102747 = VERTEX_POINT ( 'NONE', #34808 ) ;
#102746 = DIRECTION ( 'NONE',  ( 0.000000000000000000, 1.000000000000000000, 0.000000000000000000 ) ) ;
#102745 = PRODUCT_DEFINITION ( 'UNKNOWN', '', #33320, #2079 ) ;
#102748 = ORIENTED_EDGE ( 'NONE', *, *, #94458, .T. ) ;
#102749 = DIRECTION ( 'NONE',  ( -6.498030146439999846E-14, -1.000000000000000000, -7.271071663860000024E-13 ) ) ;
#102750 = CARTESIAN_POINT ( 'NONE',  ( -1.089377596668410053, 1508.669637244069918, 201.3050124727430159 ) ) ;
#102751 = CARTESIAN_POINT ( 'NONE',  ( -2.462320445819999909E-09, 1473.897694201330069, 270.2927087787980440 ) ) ;
#102752 = CARTESIAN_POINT ( 'NONE',  ( 13.23538125255438125, 1434.875856760270153, 146.8238586004999320 ) ) ;
#102753 = CARTESIAN_POINT ( 'NONE',  ( -2.794270253690000150, 1486.375510484630013, 181.7653640124980257 ) ) ;
#102754 = CARTESIAN_POINT ( 'NONE',  ( -5.519906363166400709, 1440.499855196290127, 154.7645174855159951 ) ) ;
#102755 = CARTESIAN_POINT ( 'NONE',  ( -8.875403652970000223, 1384.475744644940050, 199.9572674755190178 ) ) ;
#102756 = CARTESIAN_POINT ( 'NONE',  ( 16.66700976312933946, 1523.530935881284904, 237.7590780485273569 ) ) ;
#102757 = CARTESIAN_POINT ( 'NONE',  ( 38.64637139974560398, 1443.913060387190171, 137.1864063390110005 ) ) ;
#102758 = CARTESIAN_POINT ( 'NONE',  ( 9.961564800042728152, 1367.346295917899852, 207.6218459616987673 ) ) ;
#102759 = CARTESIAN_POINT ( 'NONE',  ( -0.06333902539661169506, 1408.725629450729912, 195.0481631183849913 ) ) ;
#102760 = CARTESIAN_POINT ( 'NONE',  ( -20.55457359352670110, 1409.641135491380055, 268.8772925003830210 ) ) ;
#102761 = CARTESIAN_POINT ( 'NONE',  ( -14.53519835277139904, 1435.864472234740106, 149.7571133851789966 ) ) ;
#102762 = ORIENTED_EDGE ( 'NONE', *, *, #30691, .T. ) ;
#102763 = CARTESIAN_POINT ( 'NONE',  ( 3.074703527060000052, 1441.333178254290033, 218.5515148082390056 ) ) ;
#102764 = CARTESIAN_POINT ( 'NONE',  ( 13.62998674540000010, 1443.967433543380139, 188.6491937973979987 ) ) ;
#102765 = B_SPLINE_SURFACE_WITH_KNOTS ( 'NONE', 5, 5, ( 
 ( #65825, #15926, #110016, #100506, #42261, #22666 ),
 ( #24341, #92108, #83704, #40051, #50127, #56866 ),
 ( #57437, #33292, #101041, #67485, #84256, #108363 ),
 ( #15385, #99943, #41706, #23238, #75866, #91562 ),
 ( #101588, #40603, #74773, #108914, #50663, #23785 ),
 ( #6998, #16472, #41157, #109473, #8093, #27124 ) ),
 .UNSPECIFIED., .F., .F., .F.,
 ( 6, 6 ),
 ( 6, 6 ),
 ( 0.4226346287780000099, 0.4682762820520000036 ),
 ( 0.000000000000000000, 2.000000000000000000 ),
 .UNSPECIFIED. ) ;
#102766 = CIRCLE ( 'NONE', #65248, 2.000000000000000444 ) ;
#102767 = EDGE_LOOP ( 'NONE', ( #9975, #14793, #97856, #97625 ) ) ;
#102768 = ORIENTED_EDGE ( 'NONE', *, *, #94108, .T. ) ;
#102769 = ADVANCED_FACE ( 'NONE', ( #52183 ), #86585, .T. ) ;
#102770 = CARTESIAN_POINT ( 'NONE',  ( -1.997114497637953345, 1517.051704408389924, 229.8748770088220965 ) ) ;
#102771 = CARTESIAN_POINT ( 'NONE',  ( -21.32683180188266192, 1525.211477436245787, 183.8595778313278686 ) ) ;
#102772 = EDGE_CURVE ( 'NONE', #37255, #64180, #35573, .T. ) ;
#102773 = CIRCLE ( 'NONE', #54565, 1.999999954375424105 ) ;
#102774 = CARTESIAN_POINT ( 'NONE',  ( 0.01306000193830150063, 1516.939762005280045, 213.7404293621069939 ) ) ;
#102775 = CARTESIAN_POINT ( 'NONE',  ( 7.500384403881742656, 1516.975677308576451, 209.2665120174619631 ) ) ;
#102776 = CIRCLE ( 'NONE', #61664, 0.9999999999999411582 ) ;
#102777 = B_SPLINE_SURFACE_WITH_KNOTS ( 'NONE', 5, 5, ( 
 ( #57055, #108534, #91181, #57611, #74409, #41339 ),
 ( #4966, #14461, #66012, #58149, #81660, #82228 ),
 ( #32917, #100671, #82780, #73289, #23953, #67108 ),
 ( #30721, #48654, #56494, #109104, #39683, #6073 ),
 ( #99014, #90623, #73850, #40226, #83878, #7182 ),
 ( #109642, #107425, #31824, #100133, #64906, #23418 ) ),
 .UNSPECIFIED., .F., .F., .F.,
 ( 6, 6 ),
 ( 6, 6 ),
 ( 5.893388375696040349, 9.819929736123960140 ),
 ( 0.000000000000000000, 0.5002947206939659663 ),
 .UNSPECIFIED. ) ;
#102778 = ORIENTED_EDGE ( 'NONE', *, *, #102904, .T. ) ;
#102779 = DIRECTION ( 'NONE',  ( 0.000000000000000000, -0.07083107041561081951, -0.9974883254774358221 ) ) ;
#102780 = CARTESIAN_POINT ( 'NONE',  ( 2.640434834157888933, 1526.748660780343471, 241.3121066639437515 ) ) ;
#102781 = CARTESIAN_POINT ( 'NONE',  ( -5.782749439735000330, 1516.858301627840092, 203.3453548368569841 ) ) ;
#102782 = ADVANCED_FACE ( 'NONE', ( #35362 ), #41824, .F. ) ;
#102783 = CARTESIAN_POINT ( 'NONE',  ( -26.74681214179999955, 1508.000506563529825, 202.6166866765980217 ) ) ;
#102784 = B_SPLINE_SURFACE_WITH_KNOTS ( 'NONE', 5, 5, ( 
 ( #74549, #6762, #75102, #59408, #33069, #31972 ),
 ( #100285, #51539, #67258, #15688, #34178, #83467 ),
 ( #109790, #101351, #57759, #68364, #85674, #49341 ),
 ( #7327, #40368, #24642, #66164, #91878, #102471 ),
 ( #41491, #109250, #40923, #92975, #23565, #58840 ),
 ( #32534, #85124, #108682, #16249, #67803, #100814 ),
 ( #49894, #50452, #8412, #17344, #84027, #93519 ),
 ( #76736, #76187, #110335, #75651, #7869, #101912 ),
 ( #42036, #25204, #16790, #50994, #42584, #25760 ) ),
 .UNSPECIFIED., .F., .F., .F.,
 ( 6, 3, 6 ),
 ( 6, 6 ),
 ( 0.000000000000000000, 3.343413285960000092, 6.686826571920000184 ),
 ( 0.000000000000000000, 2.000000000000000000 ),
 .UNSPECIFIED. ) ;
#102785 = CARTESIAN_POINT ( 'NONE',  ( -4.250070793035421346, 1421.703404060810726, 185.6649461142346524 ) ) ;
#102786 = CARTESIAN_POINT ( 'NONE',  ( -37.81300040260060058, 1384.576380814120057, 210.9400181599590098 ) ) ;
#102787 = CARTESIAN_POINT ( 'NONE',  ( -5.135476803700000481, 1408.035052921730085, 196.9098792946979870 ) ) ;
#102788 = CARTESIAN_POINT ( 'NONE',  ( -5.649719788644999241, 1514.243099272629934, 216.7708803706970002 ) ) ;
#102790 = EDGE_LOOP ( 'NONE', ( #76577, #61671, #104812, #3221, #56809 ) ) ;
#102789 = CARTESIAN_POINT ( 'NONE',  ( -7.341715959830000138, 1447.503732850919960, 185.7896193941979845 ) ) ;
#102791 = CARTESIAN_POINT ( 'NONE',  ( -114.8382766158126174, 1306.413060387289988, 306.8545936429301264 ) ) ;
#102792 = CARTESIAN_POINT ( 'NONE',  ( 26.22657672280000085, 1469.244931003429883, 211.2286983240879863 ) ) ;
#102793 = CARTESIAN_POINT ( 'NONE',  ( 19.78687179431750209, 1477.275181142720157, 225.5437915623070069 ) ) ;
#102794 = CARTESIAN_POINT ( 'NONE',  ( -25.77733573009999901, 1435.590736967609928, 136.2196633588979751 ) ) ;
#102795 = CARTESIAN_POINT ( 'NONE',  ( 2.493073829755000137, 1516.826109302209943, 211.9861720575370043 ) ) ;
#102796 = CARTESIAN_POINT ( 'NONE',  ( -68.73029257049999785, 1379.747872838770036, 280.0412483861589976 ) ) ;
#102797 = CARTESIAN_POINT ( 'NONE',  ( -15.36549427709999982, 1420.414141551129887, 227.0219849000980048 ) ) ;
#102798 = CARTESIAN_POINT ( 'NONE',  ( -30.36938634820402072, 1525.506926151471134, 221.4200516883777823 ) ) ;
#102800 = ADVANCED_FACE ( 'NONE', ( #81751 ), #100794, .F. ) ;
#102799 = AXIS2_PLACEMENT_3D ( 'NONE', #43056, #35193, #36295 ) ;
#102801 = CARTESIAN_POINT ( 'NONE',  ( 5.000329995535000016, 1516.770163853809890, 208.3657552043160024 ) ) ;
#102802 = ORIENTED_EDGE ( 'NONE', *, *, #61954, .F. ) ;
#102803 = CARTESIAN_POINT ( 'NONE',  ( -1.987196561129769945, 1451.943606313749797, 184.3861899504009898 ) ) ;
#102804 = CARTESIAN_POINT ( 'NONE',  ( -4.411357854800000311, 1412.836356211030079, 232.1857068625979821 ) ) ;
#102805 = CARTESIAN_POINT ( 'NONE',  ( -17.46729035290000098, 1385.008859354100196, 219.9589867226589774 ) ) ;
#102806 = ADVANCED_FACE ( 'NONE', ( #57698 ), #68707, .F. ) ;
#102807 = VERTEX_POINT ( 'NONE', #40311 ) ;
#102808 = CARTESIAN_POINT ( 'NONE',  ( -11.30456612219839840, 1385.307194473369918, 218.8490163376000055 ) ) ;
#102810 = ORIENTED_EDGE ( 'NONE', *, *, #11089, .F. ) ;
#102809 = CARTESIAN_POINT ( 'NONE',  ( -3.600510465689999773, 1428.725171273389833, 200.8945958432190082 ) ) ;
#102811 = CARTESIAN_POINT ( 'NONE',  ( 12.30222356331140077, 1434.228817860290064, 149.7285221497980103 ) ) ;
#102812 = CARTESIAN_POINT ( 'NONE',  ( -4.112992287346649789, 1441.414772796051693, 184.3124314157482502 ) ) ;
#102813 = VECTOR ( 'NONE', #52147, 1000.000000000000000 ) ;
#102814 = CARTESIAN_POINT ( 'NONE',  ( -22.26576771697250123, 1509.633339851660139, 227.8536643167900309 ) ) ;
#102815 = CARTESIAN_POINT ( 'NONE',  ( -1.137831540960000165, 1408.952794340330001, 186.7671042942980080 ) ) ;
#102816 = CARTESIAN_POINT ( 'NONE',  ( 0.4363688355183920065, 1517.051704408389924, 201.4773664372389987 ) ) ;
#102817 = CARTESIAN_POINT ( 'NONE',  ( 4.235259697215119523, 1441.487973001730097, 163.7720251071719986 ) ) ;
#102818 = EDGE_CURVE ( 'NONE', #51888, #15423, #100226, .T. ) ;
#102820 = CARTESIAN_POINT ( 'NONE',  ( -2.828449817540000133, 1421.423221026929923, 184.8604656580980077 ) ) ;
#102819 = CARTESIAN_POINT ( 'NONE',  ( 5.008848199894999631, 1516.858456333729919, 214.1219297979669989 ) ) ;
#102821 = FACE_OUTER_BOUND ( 'NONE', #68363, .T. ) ;
#102822 = CARTESIAN_POINT ( 'NONE',  ( -6.554151464375000735, 1516.906641539930206, 216.4536580562070185 ) ) ;
#102823 = ORIENTED_EDGE ( 'NONE', *, *, #30897, .T. ) ;
#102824 = CARTESIAN_POINT ( 'NONE',  ( -12.78701144699999936, 1416.830000968330069, 195.3261870004980096 ) ) ;
#102825 = DIRECTION ( 'NONE',  ( 0.000000000000000000, -1.000000000000000000, 0.000000000000000000 ) ) ;
#102826 = ORIENTED_EDGE ( 'NONE', *, *, #48439, .T. ) ;
#102827 = CARTESIAN_POINT ( 'NONE',  ( 2.848182016099999547, 1421.430268250230029, 183.3773441410979785 ) ) ;
#102828 = EDGE_CURVE ( 'NONE', #76110, #101372, #56584, .T. ) ;
#102829 = CARTESIAN_POINT ( 'NONE',  ( -121.2403273175383589, 1390.939237335599955, 304.3931724222538264 ) ) ;
#102830 = CARTESIAN_POINT ( 'NONE',  ( 2.136371150128812957, 1525.856065479248173, 176.8742974859703452 ) ) ;
#102831 = UNCERTAINTY_MEASURE_WITH_UNIT (LENGTH_MEASURE( 1.000000000000000082E-05 ), #80354, 'distance_accuracy_value', 'NONE');
#102832 = CARTESIAN_POINT ( 'NONE',  ( 3.279449832749999683, 1443.043429850790062, 217.3931667607889722 ) ) ;
#102833 = DIRECTION ( 'NONE',  ( -0.5224574779879248565, 0.7067418228238977473, 0.4770263929449307105 ) ) ;
#102834 = CARTESIAN_POINT ( 'NONE',  ( 762.4595027433168752, -8387.357407334287927, 2038.119698773175060 ) ) ;
#102835 = CARTESIAN_POINT ( 'NONE',  ( 17.76981827703365013, 1423.499564355630127, 226.0984388876629225 ) ) ;
#102836 = CARTESIAN_POINT ( 'NONE',  ( 11.59735442540000072, 1491.204275857490074, 206.7872505231089804 ) ) ;
#102837 = CARTESIAN_POINT ( 'NONE',  ( 9.990308914500090509, 1460.215773286300191, 206.0069800743260089 ) ) ;
#102838 = CARTESIAN_POINT ( 'NONE',  ( 15.58656453949999943, 1453.146242307530201, 195.7022669009980120 ) ) ;
#102839 = CARTESIAN_POINT ( 'NONE',  ( 37.94792208049119608, 1440.913060383530137, 256.1973595134240327 ) ) ;
#102841 = CARTESIAN_POINT ( 'NONE',  ( -2.880242083973940215, 1486.014389300230050, 182.1002674444409877 ) ) ;
#102840 = CARTESIAN_POINT ( 'NONE',  ( -13.82563399418980055, 1416.641875147470046, 202.2508794157299974 ) ) ;
#102842 = CARTESIAN_POINT ( 'NONE',  ( 11.93818824289999903, 1433.480083226980014, 149.8972169559980046 ) ) ;
#102843 = ORIENTED_EDGE ( 'NONE', *, *, #80838, .F. ) ;
#102844 = CARTESIAN_POINT ( 'NONE',  ( -7.716404340140000429, 1508.514490008389885, 219.3175259690989947 ) ) ;
#102845 = CARTESIAN_POINT ( 'NONE',  ( 26.38087806250000256, 1488.565686197229979, 207.2125440848780045 ) ) ;
#102846 = EDGE_CURVE ( 'NONE', #19461, #98304, #10555, .T. ) ;
#102847 = CARTESIAN_POINT ( 'NONE',  ( -29.22958589439999955, 1509.933780018729749, 211.7723606779179875 ) ) ;
#102848 = CARTESIAN_POINT ( 'NONE',  ( 6.928228050084153544, 1410.528584160930222, 187.1351645713825462 ) ) ;
#102849 = CARTESIAN_POINT ( 'NONE',  ( 762.4595027417112760, -8387.357407334286108, 2038.119698773842174 ) ) ;
#102850 = EDGE_CURVE ( 'NONE', #23029, #84300, #34669, .T. ) ;
#102851 = CARTESIAN_POINT ( 'NONE',  ( 9.515252399970000496, 1407.295241224529946, 218.7370609393180132 ) ) ;
#102852 = FACE_OUTER_BOUND ( 'NONE', #22915, .T. ) ;
#102853 = CARTESIAN_POINT ( 'NONE',  ( -3.139465476176170000, 1486.898214819829946, 220.2800545222459903 ) ) ;
#102854 = CARTESIAN_POINT ( 'NONE',  ( -19.04699134789089854, 1444.155793973100117, 199.5979840530640104 ) ) ;
#102855 = CARTESIAN_POINT ( 'NONE',  ( -62.46055455354049712, 1383.793505938100225, 284.6514352238460219 ) ) ;
#102856 = CIRCLE ( 'NONE', #68943, 1.000000000039231285 ) ;
#102857 = CARTESIAN_POINT ( 'NONE',  ( -107.4477384240240099, 1379.886883745280102, 299.0757736425410371 ) ) ;
#102858 = CARTESIAN_POINT ( 'NONE',  ( -9.037727763111515600, 1438.144578922800520, 210.5737952941265689 ) ) ;
#102859 = CARTESIAN_POINT ( 'NONE',  ( -2.521927849235349850, 1516.537893464249919, 201.4127202309169888 ) ) ;
#102861 = ORIENTED_EDGE ( 'NONE', *, *, #100983, .T. ) ;
#102860 = CARTESIAN_POINT ( 'NONE',  ( 25.23673856130000104, 1509.794357971529962, 195.3594004736979741 ) ) ;
#102862 = CARTESIAN_POINT ( 'NONE',  ( -17.69970948712861158, 1460.181651798936628, 228.1664494889768093 ) ) ;
#102863 = CARTESIAN_POINT ( 'NONE',  ( -50.77724190669999871, 1380.391473192369858, 232.2877509419589899 ) ) ;
#102864 = CARTESIAN_POINT ( 'NONE',  ( 8.402537688823850104, 1436.678101434069958, 207.1924150616570159 ) ) ;
#102865 = ORIENTED_EDGE ( 'NONE', *, *, #102497, .T. ) ;
#102866 = EDGE_LOOP ( 'NONE', ( #83649, #13303, #66144, #38976 ) ) ;
#102867 = CARTESIAN_POINT ( 'NONE',  ( 19.17417272014210283, 1508.304322950820278, 229.7399540503319884 ) ) ;
#102868 = CARTESIAN_POINT ( 'NONE',  ( -8.895525269423981030, 1462.225683208909913, 227.1187923881540200 ) ) ;
#102869 = CARTESIAN_POINT ( 'NONE',  ( 38.79039661010919815, 1439.444248131590030, 136.6768088287299747 ) ) ;
#102871 = CARTESIAN_POINT ( 'NONE',  ( -35.93744657210000071, 1447.859701337770048, 254.6052923994979835 ) ) ;
#102870 = CARTESIAN_POINT ( 'NONE',  ( 18.89028803260000089, 1434.820761660039807, 209.0360204046969841 ) ) ;
#102872 = CARTESIAN_POINT ( 'NONE',  ( 9.788533930052889076, 1435.243776026920159, 208.4605043225519694 ) ) ;
#102873 = CARTESIAN_POINT ( 'NONE',  ( -109.8039227080000018, 1383.848756845119851, 297.0961322820589885 ) ) ;
#102874 = DIRECTION ( 'NONE',  ( -0.9510565162951566398, 0.000000000000000000, -0.3090169943749382919 ) ) ;
#102875 = CARTESIAN_POINT ( 'NONE',  ( -19.91083394019999986, 1484.850239523630080, 191.2132470572979912 ) ) ;
#102876 = CARTESIAN_POINT ( 'NONE',  ( 2.135518920310000013, 1409.155356716130200, 186.0513290997979823 ) ) ;
#102877 = CARTESIAN_POINT ( 'NONE',  ( 1.792759577082169820, 1486.608927711839897, 197.3295603274380028 ) ) ;
#102878 = CARTESIAN_POINT ( 'NONE',  ( -5.445836181560000711, 1441.097906891670164, 154.8052917044979893 ) ) ;
#102879 = CARTESIAN_POINT ( 'NONE',  ( 8.534303549887848561, 1434.919570507270009, 206.3689778209339920 ) ) ;
#102880 = CARTESIAN_POINT ( 'NONE',  ( -12.88231326090629913, 1422.424595942170072, 203.9020998089539773 ) ) ;
#102881 = CARTESIAN_POINT ( 'NONE',  ( -3.534844613916279688, 1450.759385590300099, 184.8958323056850190 ) ) ;
#102882 = CARTESIAN_POINT ( 'NONE',  ( 1.999662964720000158, 1464.770985739130083, 236.6485670609980048 ) ) ;
#102883 = ORIENTED_EDGE ( 'NONE', *, *, #91241, .T. ) ;
#102884 = AXIS2_PLACEMENT_3D ( 'NONE', #105078, #66953, #109492 ) ;
#102885 = CARTESIAN_POINT ( 'NONE',  ( -4.705754339071280157, 1479.984670612119771, 230.9466448169910109 ) ) ;
#102886 = CARTESIAN_POINT ( 'NONE',  ( -44.70562379640000472, 1442.567860055949950, 269.9105898675979915 ) ) ;
#102887 = CARTESIAN_POINT ( 'NONE',  ( -27.50547247590620259, 1446.424453594049965, 137.1666655446350092 ) ) ;
#102888 = CARTESIAN_POINT ( 'NONE',  ( -3.604910588070000088, 1439.699991058859950, 185.4007874081979992 ) ) ;
#102889 = CARTESIAN_POINT ( 'NONE',  ( 16.32506211009999930, 1488.226337218230128, 188.7019445247979945 ) ) ;
#102890 = CARTESIAN_POINT ( 'NONE',  ( -9.987187384052590294E-09, 1473.076079583149976, 261.4091305460700028 ) ) ;
#102891 = CARTESIAN_POINT ( 'NONE',  ( -12.78956172709999883, 1502.763085786289821, 208.8827437375920226 ) ) ;
#102892 = CARTESIAN_POINT ( 'NONE',  ( -1.393184507720000020, 1415.579607678529783, 227.5929094376980117 ) ) ;
#102893 = CARTESIAN_POINT ( 'NONE',  ( -10.08879832530000087, 1419.700932331030117, 231.6349072129980016 ) ) ;
#102894 = CARTESIAN_POINT ( 'NONE',  ( 0.3230418169460009814, 1476.414103484889893, 198.3680131446989776 ) ) ;
#102895 = CARTESIAN_POINT ( 'NONE',  ( -104.7469540929999994, 1389.907464193929854, 306.5069411088589391 ) ) ;
#102896 = CIRCLE ( 'NONE', #36742, 1.999999999999999556 ) ;
#102897 = CARTESIAN_POINT ( 'NONE',  ( -0.2497437932752624434, 1485.943969500690173, 181.8371981571018239 ) ) ;
#102898 = CARTESIAN_POINT ( 'NONE',  ( 1.842394330875738673, 1359.242016496408041, 210.6218459617030021 ) ) ;
#102899 = CARTESIAN_POINT ( 'NONE',  ( -45.83609828259869801, 1437.696264054630092, 268.5022178222189950 ) ) ;
#102900 = CARTESIAN_POINT ( 'NONE',  ( -2.694370070079999735, 1428.717074573929949, 185.1363698905980186 ) ) ;
#102901 = CARTESIAN_POINT ( 'NONE',  ( 7.012921545474999796, 1508.551704408389924, 203.6084103740869864 ) ) ;
#102902 = EDGE_LOOP ( 'NONE', ( #24503, #43419, #80533, #57254 ) ) ;
#102903 = CARTESIAN_POINT ( 'NONE',  ( 2.879318417774999972, 1516.995911393979895, 209.8571825100049750 ) ) ;
#102904 = EDGE_CURVE ( 'NONE', #38555, #27144, #64942, .T. ) ;
#102905 = CARTESIAN_POINT ( 'NONE',  ( -14.28029386204369899, 1390.367275669339961, 209.8449220790990069 ) ) ;
#102906 = CARTESIAN_POINT ( 'NONE',  ( -2.496647090823195470, 1469.968832673554289, 218.9194591004516042 ) ) ;
#102907 = CARTESIAN_POINT ( 'NONE',  ( 7.525900132721149660, 1425.843575467760047, 212.2409298998749989 ) ) ;
#102908 = CARTESIAN_POINT ( 'NONE',  ( -26.83284804043870153, 1451.909710471250037, 135.4138440258689968 ) ) ;
#102909 = ORIENTED_EDGE ( 'NONE', *, *, #16997, .T. ) ;
#102910 = CARTESIAN_POINT ( 'NONE',  ( -14.60873270509999955, 1470.816572150829870, 194.8395487178979977 ) ) ;
#102912 = CARTESIAN_POINT ( 'NONE',  ( 15.39218709410000052, 1506.810797420630024, 193.3968663410979900 ) ) ;
#102911 = CARTESIAN_POINT ( 'NONE',  ( -2.570808432944301725, 1525.317359687841417, 176.7848587726591632 ) ) ;
#102913 = CARTESIAN_POINT ( 'NONE',  ( 0.000000000000000000, 1526.382868172863937, 209.1218459616979999 ) ) ;
#102914 = CARTESIAN_POINT ( 'NONE',  ( -19.55701159338780215, 1456.127805513401881, 228.1967745818641049 ) ) ;
#102915 = EDGE_CURVE ( 'NONE', #16730, #104691, #79404, .T. ) ;
#102916 = CARTESIAN_POINT ( 'NONE',  ( -2.919023784219999751, 1461.299471294090154, 228.5190642125989768 ) ) ;
#102917 = FACE_OUTER_BOUND ( 'NONE', #18841, .T. ) ;
#102918 = ORIENTED_EDGE ( 'NONE', *, *, #11862, .T. ) ;
#102919 = CARTESIAN_POINT ( 'NONE',  ( -4.308968488989159518, 1408.710846737909833, 270.4270427888720292 ) ) ;
#102920 = CARTESIAN_POINT ( 'NONE',  ( 6.550870144104999682, 1516.727502608469877, 208.3674577492799926 ) ) ;
#102921 = CARTESIAN_POINT ( 'NONE',  ( 8.893954816108170291, 1419.211828825139946, 232.2343367069420310 ) ) ;
#102922 = CARTESIAN_POINT ( 'NONE',  ( 8.159145002205340447, 1435.857859259829866, 206.4447587482620179 ) ) ;
#102924 = EDGE_LOOP ( 'NONE', ( #75076, #39299, #40129 ) ) ;
#102923 = CARTESIAN_POINT ( 'NONE',  ( -3.406640539343045671, 1367.128124208074041, 209.6218459617148824 ) ) ;
#102925 = ORIENTED_EDGE ( 'NONE', *, *, #15031, .F. ) ;
#102926 = CARTESIAN_POINT ( 'NONE',  ( -22.64963451372929981, 1409.703995751010098, 209.5275992923249930 ) ) ;
#102927 = CARTESIAN_POINT ( 'NONE',  ( -0.4457311135394249613, 1409.096194338759915, 185.6363386297540217 ) ) ;
#102928 = FACE_OUTER_BOUND ( 'NONE', #17056, .T. ) ;
#102929 = CARTESIAN_POINT ( 'NONE',  ( 20.98459803409886959, 1519.551704408389924, 216.7582258867871587 ) ) ;
#102930 = CARTESIAN_POINT ( 'NONE',  ( -18.14005346051209955, 1415.388767200230177, 195.1132133976919931 ) ) ;
#102931 = CARTESIAN_POINT ( 'NONE',  ( -19.86345851500000137, 1425.811316569130213, 222.6950000957980080 ) ) ;
#102932 = CARTESIAN_POINT ( 'NONE',  ( 37.07563244675080227, 1462.054830057500112, 267.9004510718949632 ) ) ;
#102933 = AXIS2_PLACEMENT_3D ( 'NONE', #98650, #57235, #49365 ) ;
#102934 = CARTESIAN_POINT ( 'NONE',  ( -2.390460581662895656, 1466.906621117755549, 235.1802628545677010 ) ) ;
#102935 = CARTESIAN_POINT ( 'NONE',  ( -3.812371265849999968, 1428.459941732490051, 200.5740418003289847 ) ) ;
#102936 = CARTESIAN_POINT ( 'NONE',  ( 3.446942071715000111, 1516.842852731759876, 205.8545543269370057 ) ) ;
#102937 = VERTEX_POINT ( 'NONE', #34117 ) ;
#102938 = CARTESIAN_POINT ( 'NONE',  ( -11.94265413316043656, 1433.497479536225455, 149.9944130464578222 ) ) ;
#102939 = CARTESIAN_POINT ( 'NONE',  ( 1.527006335184809993, 1453.898422402579854, 183.4371394172420082 ) ) ;
#102940 = CARTESIAN_POINT ( 'NONE',  ( 0.000000000000000000, 1512.187213306747481, 209.1218459616979999 ) ) ;
#102941 = ORIENTED_EDGE ( 'NONE', *, *, #42194, .F. ) ;
#102942 = CARTESIAN_POINT ( 'NONE',  ( -1.451575880177540023, 1457.988782316290099, 229.8657700608300161 ) ) ;
#102943 = EDGE_CURVE ( 'NONE', #75707, #21719, #52042, .T. ) ;
#102944 = CARTESIAN_POINT ( 'NONE',  ( 26.07109846599830050, 1452.002629622410041, 135.0133573619999936 ) ) ;
#102945 = CARTESIAN_POINT ( 'NONE',  ( -4.271224532677689645, 1508.551704408389924, 213.3620110914459929 ) ) ;
#102946 = CARTESIAN_POINT ( 'NONE',  ( -3.078458307160000018, 1389.883663780020015, 214.5934223984789924 ) ) ;
#102947 = ADVANCED_FACE ( 'NONE', ( #93458 ), #17959, .F. ) ;
#102948 = CARTESIAN_POINT ( 'NONE',  ( -8.945448071766088916, 1385.615055044318524, 218.6252746482883538 ) ) ;
#102949 = CARTESIAN_POINT ( 'NONE',  ( 17.90246463440000113, 1410.035002130830208, 193.6991388332980080 ) ) ;
#102950 = LINE ( 'NONE', #35215, #93083 ) ;
#102951 = CARTESIAN_POINT ( 'NONE',  ( 2.637369437447386389, 1439.648528781137884, 183.5003223541247905 ) ) ;
#102953 = CARTESIAN_POINT ( 'NONE',  ( -19.40632858663824933, 1425.506857333870357, 223.5429138958425597 ) ) ;
#102952 = CARTESIAN_POINT ( 'NONE',  ( 1.331911112270000030, 1417.152951162330055, 233.7702109215979931 ) ) ;
#102954 = CARTESIAN_POINT ( 'NONE',  ( 1.067515872454499970, 1451.920614097839916, 183.2424258504900081 ) ) ;
#102955 = EDGE_CURVE ( 'NONE', #85994, #71507, #107107, .T. ) ;
#102956 = FACE_OUTER_BOUND ( 'NONE', #53189, .T. ) ;
#102957 = B_SPLINE_CURVE_WITH_KNOTS ( 'NONE', 5,
 ( #52745, #1239, #94167, #51635, #26413, #60605 ),
 .UNSPECIFIED., .F., .F.,
 ( 6, 6 ),
 ( -2.000000000000000000, 0.000000000000000000 ),
 .UNSPECIFIED. ) ;
#102958 = CARTESIAN_POINT ( 'NONE',  ( -2.470168521978396203, 1512.187213306747481, 175.3649660270905315 ) ) ;
#102959 = CARTESIAN_POINT ( 'NONE',  ( 6.750002614367778264, 1418.487218233497970, 233.5578456803374934 ) ) ;
#102960 = VERTEX_POINT ( 'NONE', #78903 ) ;
#102961 = CARTESIAN_POINT ( 'NONE',  ( -1.770994272916314172, 1526.211528530236592, 177.6852349320064945 ) ) ;
#102962 = CARTESIAN_POINT ( 'NONE',  ( 10.96946812545280103, 1432.347663862999980, 151.7701354189910035 ) ) ;
#102963 = CARTESIAN_POINT ( 'NONE',  ( -9.052602208344991297, 1483.887799354419940, 201.3830137227830051 ) ) ;
#102964 = ADVANCED_FACE ( 'NONE', ( #87859 ), #20071, .F. ) ;
#102965 = AXIS2_PLACEMENT_3D ( 'NONE', #31015, #84721, #42187 ) ;
#102966 = CARTESIAN_POINT ( 'NONE',  ( -13.66482009279999943, 1390.428771231109977, 209.8137776769819993 ) ) ;
#102967 = CARTESIAN_POINT ( 'NONE',  ( 8.904193304007050003, 1426.574205491320299, 210.6754700860900016 ) ) ;
#102968 = CARTESIAN_POINT ( 'NONE',  ( 1.208874843759933038, 1421.371554683040586, 193.7626136730214625 ) ) ;
#102969 = CARTESIAN_POINT ( 'NONE',  ( -4.327725855061320459, 1515.130588580269887, 208.4066028149230192 ) ) ;
#102970 = CARTESIAN_POINT ( 'NONE',  ( -21.37693747720000204, 1443.303628178600093, 224.8635561966979708 ) ) ;
#102971 = CARTESIAN_POINT ( 'NONE',  ( -21.44621506493709973, 1509.083182011242798, 191.8119323521389106 ) ) ;
#102972 = CARTESIAN_POINT ( 'NONE',  ( 11.63847943070000035, 1433.482589826759977, 151.0612159216979933 ) ) ;
#102973 = CARTESIAN_POINT ( 'NONE',  ( 11.06589455810000011, 1457.157324861229881, 234.3916895697979612 ) ) ;
#102974 = CARTESIAN_POINT ( 'NONE',  ( 11.80289467588129959, 1415.088012641449950, 196.9360298139739882 ) ) ;
#102975 = AXIS2_PLACEMENT_3D ( 'NONE', #52458, #70937, #105053 ) ;
#102976 = CARTESIAN_POINT ( 'NONE',  ( 18.38166525818579800, 1428.164269971480053, 201.4944236828210080 ) ) ;
#102977 = CARTESIAN_POINT ( 'NONE',  ( 10.23386993751040031, 1423.173846909970280, 200.2029385363399854 ) ) ;
#102978 = CARTESIAN_POINT ( 'NONE',  ( -3.263276722441742717, 1524.760046179776054, 176.4719413543065514 ) ) ;
#102979 = CARTESIAN_POINT ( 'NONE',  ( -15.78890742300000127, 1486.496171638329997, 186.5216181066980141 ) ) ;
#102980 = CARTESIAN_POINT ( 'NONE',  ( 7.615013220904412350, 1398.139290501694404, 219.7751663341437620 ) ) ;
#102981 = CARTESIAN_POINT ( 'NONE',  ( -26.08589733633370145, 1509.953121808929836, 192.9123034651479998 ) ) ;
#102982 = EDGE_CURVE ( 'NONE', #4206, #74270, #85669, .T. ) ;
#102983 = CARTESIAN_POINT ( 'NONE',  ( -8.092407232544459816, 1425.062004142523392, 209.6995862100099828 ) ) ;
#102984 = CARTESIAN_POINT ( 'NONE',  ( 3.313292261855492082, 1446.583017422768989, 170.5342543665201163 ) ) ;
#102985 = CARTESIAN_POINT ( 'NONE',  ( -41.18635921427883062, 1440.753220515532576, 135.3771779697534328 ) ) ;
#102986 = CARTESIAN_POINT ( 'NONE',  ( -1.460285906039999970, 1515.203804957989860, 204.7960373641490150 ) ) ;
#102987 = CARTESIAN_POINT ( 'NONE',  ( 11.36538105552331501, 1434.589103438910797, 151.5115492014778908 ) ) ;
#102988 =( BOUNDED_CURVE ( )  B_SPLINE_CURVE ( 3, ( #91757, #15033, #108564, #31301 ),
 .UNSPECIFIED., .F., .F. ) 
 B_SPLINE_CURVE_WITH_KNOTS ( ( 4, 4 ),
 ( 2.603837571717090071, 2.914415234293290080 ),
 .UNSPECIFIED. ) 
 CURVE ( )  GEOMETRIC_REPRESENTATION_ITEM ( )  RATIONAL_B_SPLINE_CURVE ( ( 1.000000000000000000, 0.9919779331734855932, 0.9919779331734855932, 1.000000000000000000 ) ) 
 REPRESENTATION_ITEM ( '' )  );
#102989 = CARTESIAN_POINT ( 'NONE',  ( 20.81805065521579934, 1457.016308257720084, 206.8942077970259845 ) ) ;
#102990 = EDGE_CURVE ( 'NONE', #5947, #71944, #12771, .T. ) ;
#102991 = CARTESIAN_POINT ( 'NONE',  ( -7.711550716115000093, 1516.630499592039996, 213.1573366827869904 ) ) ;
#102992 = CARTESIAN_POINT ( 'NONE',  ( -20.36506032882270034, 1418.448525618100120, 208.7072595077149799 ) ) ;
#102993 = CARTESIAN_POINT ( 'NONE',  ( 0.1684383342722930166, 1481.247972760530047, 182.0407818193630192 ) ) ;
#102995 = ORIENTED_EDGE ( 'NONE', *, *, #69977, .F. ) ;
#102994 = CARTESIAN_POINT ( 'NONE',  ( 4.987363902569999397, 1436.241616658689964, 206.8881657827189997 ) ) ;
#102996 = CARTESIAN_POINT ( 'NONE',  ( -1.121351043030000216, 1416.825532269230052, 228.0848332775979941 ) ) ;
#102997 = CARTESIAN_POINT ( 'NONE',  ( -33.08110269718211072, 1445.052233488288266, 154.3415468483447910 ) ) ;
#102998 = DIRECTION ( 'NONE',  ( -5.980589973904019347E-17, 1.000000000000000000, -1.736889445713099699E-16 ) ) ;
#102999 = CARTESIAN_POINT ( 'NONE',  ( -32.13439773946823408, 1525.163527997504616, 217.0282454366101206 ) ) ;
#103000 = CARTESIAN_POINT ( 'NONE',  ( -17.51542736287469992, 1417.552205557379921, 206.7802911192910358 ) ) ;
#103001 = ORIENTED_EDGE ( 'NONE', *, *, #42604, .T. ) ;
#103002 = CARTESIAN_POINT ( 'NONE',  ( -10.19876720080000077, 1472.745415185489946, 209.0901046235979948 ) ) ;
#103003 = CARTESIAN_POINT ( 'NONE',  ( -12.67911190924929876, 1390.817978749060103, 211.5986899158650090 ) ) ;
#103004 = CARTESIAN_POINT ( 'NONE',  ( 6.037737136446180486, 1446.437918506160258, 202.3744026597657069 ) ) ;
#103005 = CARTESIAN_POINT ( 'NONE',  ( -16.56943046651996099, 1526.189899547014875, 182.6454527705575970 ) ) ;
#103006 = CARTESIAN_POINT ( 'NONE',  ( -3.220366543789920488, 1433.265472343769943, 218.1215055313249991 ) ) ;
#103007 = CARTESIAN_POINT ( 'NONE',  ( -108.4300939784633186, 1381.280801279105845, 310.3690016902303910 ) ) ;
#103008 = CARTESIAN_POINT ( 'NONE',  ( -12.27979310579503114, 1377.633317686999817, 208.2390977848808404 ) ) ;
#103009 = DIRECTION ( 'NONE',  ( -0.000000000000000000, -1.000000000000000000, -0.000000000000000000 ) ) ;
#103010 = B_SPLINE_CURVE_WITH_KNOTS ( 'NONE', 5,
 ( #69297, #60903, #25594, #86620, #17730, #10470 ),
 .UNSPECIFIED., .F., .F.,
 ( 6, 6 ),
 ( 0.000000000000000000, 1.000000000000000000 ),
 .UNSPECIFIED. ) ;
#103011 = CARTESIAN_POINT ( 'NONE',  ( -12.30071208829999918, 1391.739025408870020, 208.7164210746560116 ) ) ;
#103012 = CARTESIAN_POINT ( 'NONE',  ( -67.88634661955258309, 1385.101574011260027, 261.4157710435330273 ) ) ;
#103013 = CARTESIAN_POINT ( 'NONE',  ( 2.994688454485729956, 1464.609795419120246, 236.6065850994260131 ) ) ;
#103014 = CARTESIAN_POINT ( 'NONE',  ( -37.65558013879999777, 1379.730903953030065, 220.7433301062589805 ) ) ;
#103015 = ORIENTED_EDGE ( 'NONE', *, *, #65289, .F. ) ;
#103016 = CARTESIAN_POINT ( 'NONE',  ( -15.81248221509479812, 1410.431092464730000, 226.6593714454470216 ) ) ;
#103018 = ORIENTED_EDGE ( 'NONE', *, *, #96150, .F. ) ;
#103017 = CARTESIAN_POINT ( 'NONE',  ( 2.253566441613126910E-10, 1426.918876941764893, 134.0999999980979851 ) ) ;
#103019 = CARTESIAN_POINT ( 'NONE',  ( 6.595526062923129373, 1466.717679795370032, 216.5467274825269897 ) ) ;
#103020 = ORIENTED_EDGE ( 'NONE', *, *, #10600, .T. ) ;
#103021 = CARTESIAN_POINT ( 'NONE',  ( 23.82032192280000160, 1509.070381045429940, 222.7384874576979996 ) ) ;
#103022 = CARTESIAN_POINT ( 'NONE',  ( -8.461434042299536884, 1363.810109312981240, 207.6218459616988241 ) ) ;
#103023 = CARTESIAN_POINT ( 'NONE',  ( -6.349572003580000512, 1494.536298393890092, 198.5213465523989953 ) ) ;
#103024 = CARTESIAN_POINT ( 'NONE',  ( -5.021037887259439003, 1440.968375784700129, 155.1907004240329968 ) ) ;
#103025 = CARTESIAN_POINT ( 'NONE',  ( 15.10371975099999986, 1409.440493903229935, 192.9533947891980006 ) ) ;
#103026 = CARTESIAN_POINT ( 'NONE',  ( 19.42500282749999840, 1440.913060387330006, 212.4633492400480179 ) ) ;
#103027 = CARTESIAN_POINT ( 'NONE',  ( 2.220446049249999755E-16, 1516.051704408390151, 209.1218459616989946 ) ) ;
#103028 = CARTESIAN_POINT ( 'NONE',  ( 20.11865583365249677, 1457.295773309100014, 209.3900325861709746 ) ) ;
#103029 = CARTESIAN_POINT ( 'NONE',  ( -21.84222938500011679, 1507.845663673426770, 226.4317239180982710 ) ) ;
#103030 = CARTESIAN_POINT ( 'NONE',  ( -8.962252599297759303, 1366.920250605815909, 210.6218459616991936 ) ) ;
#103031 = CARTESIAN_POINT ( 'NONE',  ( 20.59684415428669979, 1507.762623717989982, 227.6602567528719874 ) ) ;
#103032 = CARTESIAN_POINT ( 'NONE',  ( 4.609673241434999902, 1516.754149861460064, 205.8564388142570181 ) ) ;
#103033 = CARTESIAN_POINT ( 'NONE',  ( 4.293785987919999769, 1447.009251274299913, 154.3906956833980075 ) ) ;
#103034 = CARTESIAN_POINT ( 'NONE',  ( -10.10023367162169983, 1522.051704408389924, 185.1638560673330005 ) ) ;
#103035 = CARTESIAN_POINT ( 'NONE',  ( 14.45750875900000132, 1416.828042640230024, 196.8520545293980319 ) ) ;
#103037 = EDGE_LOOP ( 'NONE', ( #6493, #99814, #30733, #41203 ) ) ;
#103036 = CARTESIAN_POINT ( 'NONE',  ( -68.77190087506669158, 1379.747925807530009, 280.3125204381590265 ) ) ;
#103038 = AXIS2_PLACEMENT_3D ( 'NONE', #76544, #61433, #33989 ) ;
#103039 = DIRECTION ( 'NONE',  ( 1.794299266459999922E-16, 1.000000000000000000, 1.181975866886321963E-16 ) ) ;
#103040 = ORIENTED_EDGE ( 'NONE', *, *, #50748, .F. ) ;
#103041 = CARTESIAN_POINT ( 'NONE',  ( -16.27599028281260019, 1514.537600263860895, 223.8805438227635989 ) ) ;
#103042 = CARTESIAN_POINT ( 'NONE',  ( -24.09077679880000034, 1449.794656643329972, 202.7835535694879923 ) ) ;
#103044 = CARTESIAN_POINT ( 'NONE',  ( 16.29419587174599826, 1409.489892375330101, 193.0344759318469983 ) ) ;
#103043 = CARTESIAN_POINT ( 'NONE',  ( -11.50815781787750147, 1426.421521582019977, 127.8416712200489940 ) ) ;
#103045 = CARTESIAN_POINT ( 'NONE',  ( 2.299656316094999653, 1516.843453247299749, 211.5982966343670171 ) ) ;
#103046 = CARTESIAN_POINT ( 'NONE',  ( 17.38707324475434746, 1509.640293562321631, 184.6720443489594459 ) ) ;
#103047 = CARTESIAN_POINT ( 'NONE',  ( -21.04915883790000208, 1471.323284330029992, 208.5356106908370180 ) ) ;
#103048 = CARTESIAN_POINT ( 'NONE',  ( -41.23304013239999932, 1435.760839457339898, 261.5842231913979958 ) ) ;
#103049 = CARTESIAN_POINT ( 'NONE',  ( -12.95149561310000053, 1379.302527901269741, 208.6156618013899902 ) ) ;
#103050 = CARTESIAN_POINT ( 'NONE',  ( 28.40191814900270018, 1508.834101303340049, 209.4333091118389802 ) ) ;
#103051 = APPLICATION_PROTOCOL_DEFINITION ( 'draft international standard', 'automotive_design', 1998, #72126 ) ;
#103052 = CARTESIAN_POINT ( 'NONE',  ( 4.822058355276690023, 1508.551704408389924, 212.5065985955260146 ) ) ;
#103053 = B_SPLINE_CURVE_WITH_KNOTS ( 'NONE', 3,
 ( #83432, #56050, #98034, #65563, #6729, #81778 ),
 .UNSPECIFIED., .F., .F.,
 ( 4, 2, 4 ),
 ( -0.1558952665523989922, -0.07794716665277695578, -2.594126852384359694E-06 ),
 .UNSPECIFIED. ) ;
#103054 = CARTESIAN_POINT ( 'NONE',  ( -38.00991624508050393, 1438.636109681070138, 136.6089179658529815 ) ) ;
#103055 = ORIENTED_EDGE ( 'NONE', *, *, #25710, .F. ) ;
#103056 = CARTESIAN_POINT ( 'NONE',  ( 13.78199155278950094, 1397.422248721489950, 206.9763111428489992 ) ) ;
#103058 = AXIS2_PLACEMENT_3D ( 'NONE', #84613, #58332, #84067 ) ;
#103057 = CARTESIAN_POINT ( 'NONE',  ( 10.07185917612419956, 1460.294335048200082, 206.2511351615570163 ) ) ;
#103059 = CARTESIAN_POINT ( 'NONE',  ( -17.12053142319999921, 1459.474259415330152, 228.5189956839979857 ) ) ;
#103060 = ORIENTED_EDGE ( 'NONE', *, *, #25434, .T. ) ;
#103061 = ORIENTED_EDGE ( 'NONE', *, *, #18144, .F. ) ;
#103062 = CARTESIAN_POINT ( 'NONE',  ( -18.97219799319119815, 1486.246528605739741, 189.3000344508529906 ) ) ;
#103063 = CARTESIAN_POINT ( 'NONE',  ( 7.105419199340579675E-15, 1425.409945881219983, 153.8891009232719966 ) ) ;
#103064 = ORIENTED_EDGE ( 'NONE', *, *, #57709, .F. ) ;
#103065 = LINE ( 'NONE', #94680, #72483 ) ;
#103066 = CARTESIAN_POINT ( 'NONE',  ( -9.958774778861073429, 1418.280608540457479, 197.3728175944318082 ) ) ;
#103067 = DIRECTION ( 'NONE',  ( 0.000000000000000000, 1.000000000000000000, 0.000000000000000000 ) ) ;
#103068 = CARTESIAN_POINT ( 'NONE',  ( 27.56721560699687146, 1509.458871272823671, 206.1447979657547478 ) ) ;
#103069 = CARTESIAN_POINT ( 'NONE',  ( 6.725623893241880147, 1508.728101229370168, 201.9181371664530218 ) ) ;
#103070 = CARTESIAN_POINT ( 'NONE',  ( 10.12770055993100016, 1452.320269254320010, 209.2677959960770124 ) ) ;
#103071 = DIRECTION ( 'NONE',  ( -0.4090087482554295439, 0.000000000000000000, -0.9125304618753977692 ) ) ;
#103072 = CARTESIAN_POINT ( 'NONE',  ( -89.55229520999530735, 1384.836914095840029, 292.2851226604299768 ) ) ;
#103073 = ORIENTED_EDGE ( 'NONE', *, *, #35568, .F. ) ;
#103074 = CARTESIAN_POINT ( 'NONE',  ( -7.331183129075000693, 1516.882217593000178, 202.1801186797769674 ) ) ;
#103075 = CARTESIAN_POINT ( 'NONE',  ( -2.486220139904999904, 1516.939658295650133, 209.1350829839039989 ) ) ;
#103076 = ORIENTED_EDGE ( 'NONE', *, *, #10386, .F. ) ;
#103077 = CARTESIAN_POINT ( 'NONE',  ( 11.81166646117249996, 1428.828521759150135, 148.7357659156419913 ) ) ;
#103078 = CARTESIAN_POINT ( 'NONE',  ( 3.000838584243140428, 1512.040964529592429, 217.0177385286994820 ) ) ;
#103079 = VERTEX_POINT ( 'NONE', #2211 ) ;
#103080 = CARTESIAN_POINT ( 'NONE',  ( -1.452061816759999902, 1467.474562141730075, 183.2045861867980250 ) ) ;
#103081 = ADVANCED_FACE ( 'NONE', ( #36323 ), #25739, .T. ) ;
#103082 = CARTESIAN_POINT ( 'NONE',  ( -5.938778458005980809, 1508.471255113249981, 219.9128644399360155 ) ) ;
#103083 = CARTESIAN_POINT ( 'NONE',  ( -113.4000000000000057, 1306.413060387289988, 304.2218459572590064 ) ) ;
#103084 = FACE_OUTER_BOUND ( 'NONE', #7948, .T. ) ;
#103085 = CARTESIAN_POINT ( 'NONE',  ( -4.915892415680000127, 1423.440305011429928, 184.6741102763979825 ) ) ;
#103086 = CARTESIAN_POINT ( 'NONE',  ( 13.09236780528799926, 1411.228464131030023, 270.0792911668929719 ) ) ;
#103087 = DIRECTION ( 'NONE',  ( -0.4794255386042020062, 2.935634756405659852E-17, 0.8775825618903733139 ) ) ;
#103088 = CARTESIAN_POINT ( 'NONE',  ( 0.8350686643532190256, 1526.382868172863937, 177.3106345060153046 ) ) ;
#103089 = CARTESIAN_POINT ( 'NONE',  ( -10.05941745090078143, 1410.638996758815210, 188.4493189201661210 ) ) ;
#103090 = CARTESIAN_POINT ( 'NONE',  ( -41.85969401239999854, 1379.735023715520128, 226.1594769080589913 ) ) ;
#103091 = CARTESIAN_POINT ( 'NONE',  ( -15.93334107429999946, 1485.110845200029871, 224.0169806397979926 ) ) ;
#103093 = CARTESIAN_POINT ( 'NONE',  ( 8.986732482983370573, 1468.575268126999845, 202.3908276555110035 ) ) ;
#103092 = CARTESIAN_POINT ( 'NONE',  ( 17.79624440539999952, 1458.182673695930134, 228.6901989446980110 ) ) ;
#103094 = CARTESIAN_POINT ( 'NONE',  ( -4.752998812148558017, 1423.601010648300417, 184.5372248178350958 ) ) ;
#103095 = CARTESIAN_POINT ( 'NONE',  ( -10.73514660131351839, 1424.973046421745494, 139.1354236205272343 ) ) ;
#103096 = CARTESIAN_POINT ( 'NONE',  ( -2.975022846544269850, 1495.689959026299903, 216.9727101957990101 ) ) ;
#103097 = EDGE_LOOP ( 'NONE', ( #3161, #26648, #20177, #57851 ) ) ;
#103098 = CARTESIAN_POINT ( 'NONE',  ( -3.487592469391230132, 1509.038615938009798, 204.6345961782960217 ) ) ;
#103099 = AXIS2_PLACEMENT_3D ( 'NONE', #15261, #91446, #14722 ) ;
#103100 = ADVANCED_FACE ( 'NONE', ( #88663 ), #83825, .F. ) ;
#103101 = CARTESIAN_POINT ( 'NONE',  ( -20.49599333844820137, 1525.960063244516959, 233.8638087104926058 ) ) ;
#103102 = CARTESIAN_POINT ( 'NONE',  ( -2.927028964964125457, 1485.034416825944163, 183.1263100967265416 ) ) ;
#103103 = CARTESIAN_POINT ( 'NONE',  ( -14.93718008229999938, 1416.181292664740113, 212.9156384192889959 ) ) ;
#103105 = ORIENTED_EDGE ( 'NONE', *, *, #43319, .T. ) ;
#103104 = CARTESIAN_POINT ( 'NONE',  ( -0.05006135368913040146, 1515.158685764440179, 204.7948558572980176 ) ) ;
#103106 = B_SPLINE_CURVE_WITH_KNOTS ( 'NONE', 5,
 ( #68142, #102252, #94970, #44023, #59181, #35604 ),
 .UNSPECIFIED., .F., .F.,
 ( 6, 6 ),
 ( -1.999999977866010026, 0.000000000000000000 ),
 .UNSPECIFIED. ) ;
#103107 = CARTESIAN_POINT ( 'NONE',  ( 0.7305497199880000014, 1471.316885392330050, 187.9286521196980004 ) ) ;
#103108 = CARTESIAN_POINT ( 'NONE',  ( -15.28377182955919977, 1507.620489270460212, 191.9630984214329885 ) ) ;
#103109 = CARTESIAN_POINT ( 'NONE',  ( -11.83460451569999883, 1430.051560513030154, 149.9498806582980137 ) ) ;
#103110 = CARTESIAN_POINT ( 'NONE',  ( 19.40526558876458907, 1456.941577366487991, 224.5007284994117072 ) ) ;
#103111 = CARTESIAN_POINT ( 'NONE',  ( -11.03761941066989927, 1462.381893958199953, 208.9991076938630101 ) ) ;
#103112 = CARTESIAN_POINT ( 'NONE',  ( -4.992349863779999453, 1391.620913471789891, 203.8075142969990168 ) ) ;
#103113 = CARTESIAN_POINT ( 'NONE',  ( -1.073363620209200085E-15, 1380.371560387289946, 209.1218459616989946 ) ) ;
#103114 = CARTESIAN_POINT ( 'NONE',  ( -15.71561347966500222, 1514.030803186779849, 224.2184393400669933 ) ) ;
#103115 = FACE_OUTER_BOUND ( 'NONE', #258, .T. ) ;
#103117 = CARTESIAN_POINT ( 'NONE',  ( -10.97550978995469961, 1481.752618510480033, 208.0127154857229925 ) ) ;
#103116 = CARTESIAN_POINT ( 'NONE',  ( 33.91369278643569629, 1437.010534640189690, 136.5611839302279691 ) ) ;
#103118 = CARTESIAN_POINT ( 'NONE',  ( -16.55764869240000081, 1460.395321624930148, 228.3393650202980041 ) ) ;
#103119 = CARTESIAN_POINT ( 'NONE',  ( 7.321193707744999557, 1516.534976163889951, 206.8301696586770220 ) ) ;
#103120 = CARTESIAN_POINT ( 'NONE',  ( 14.40766152700000013, 1408.465220730830197, 269.5837135859979981 ) ) ;
#103121 = CARTESIAN_POINT ( 'NONE',  ( 2.689344463419570452, 1464.716346866380036, 236.9361821190090041 ) ) ;
#103122 = CARTESIAN_POINT ( 'NONE',  ( 18.90842699680000294, 1430.304836455529994, 193.3988046526980042 ) ) ;
#103123 = CARTESIAN_POINT ( 'NONE',  ( -23.69221647310000023, 1436.197216314300022, 212.4790823011979910 ) ) ;
#103124 = CARTESIAN_POINT ( 'NONE',  ( 6.555713241385960011, 1506.475290693023453, 230.1454641328169259 ) ) ;
#103125 = CARTESIAN_POINT ( 'NONE',  ( -11.42085373761049993, 1500.664288095930033, 209.5050427075310040 ) ) ;
#103126 = CARTESIAN_POINT ( 'NONE',  ( -40.71429805386350154, 1443.131898661159994, 137.0441744550780072 ) ) ;
#103127 = EDGE_CURVE ( 'NONE', #20179, #5014, #104784, .T. ) ;
#103128 = CARTESIAN_POINT ( 'NONE',  ( -17.19739463999666285, 1525.960063244516959, 181.9833109756550584 ) ) ;
#103129 = CARTESIAN_POINT ( 'NONE',  ( -15.89469460119999766, 1416.172609518619993, 209.1989024842829963 ) ) ;
#103130 = CARTESIAN_POINT ( 'NONE',  ( -13.83903651480000008, 1444.969018072280051, 188.3469987607979874 ) ) ;
#103131 = CARTESIAN_POINT ( 'NONE',  ( 0.000000000000000000, 1526.382868172863937, 240.9330574173806951 ) ) ;
#103132 = CARTESIAN_POINT ( 'NONE',  ( -30.78499955540000244, 1436.901323119660219, 136.6581730245979713 ) ) ;
#103133 = CARTESIAN_POINT ( 'NONE',  ( -3.619842073959999684, 1497.142537609690180, 220.5541519757989875 ) ) ;
#103134 = ORIENTED_EDGE ( 'NONE', *, *, #27274, .F. ) ;
#103135 = CARTESIAN_POINT ( 'NONE',  ( -3.077691755255000050, 1511.730395268069969, 201.3186441269170075 ) ) ;
#103136 = CARTESIAN_POINT ( 'NONE',  ( -12.68420265674900094, 1409.356002504509888, 217.0171520026799783 ) ) ;
#103137 = CARTESIAN_POINT ( 'NONE',  ( 11.26969769241764219, 1425.486564486241832, 139.1357072137798809 ) ) ;
#103138 = CARTESIAN_POINT ( 'NONE',  ( -2.500000000000000000, 1411.429641636930000, 127.2892455880980123 ) ) ;
#103139 = AXIS2_PLACEMENT_3D ( 'NONE', #37717, #104925, #46148 ) ;
#103140 = CARTESIAN_POINT ( 'NONE',  ( -12.52817736919999980, 1473.792528260629979, 269.6003666339980214 ) ) ;
#103141 = CARTESIAN_POINT ( 'NONE',  ( -18.48166340339999891, 1443.454462795790050, 212.6921494033990143 ) ) ;
#103142 = DIRECTION ( 'NONE',  ( 0.9750097311986455351, 0.1381407795329493426, -0.1739918075599369285 ) ) ;
#103143 = FACE_OUTER_BOUND ( 'NONE', #73444, .T. ) ;
#103144 = CARTESIAN_POINT ( 'NONE',  ( -65.00736949162829603, 1384.677693943300028, 288.7496629741240213 ) ) ;
#103145 = CARTESIAN_POINT ( 'NONE',  ( -27.68635198675820064, 1384.964471995969916, 204.4027686579379974 ) ) ;
#103146 = CARTESIAN_POINT ( 'NONE',  ( -13.75903449370000153, 1409.893112547430064, 226.9379585588980035 ) ) ;
#103147 = CARTESIAN_POINT ( 'NONE',  ( 11.97935895607569989, 1415.724942524390144, 223.2960686490259832 ) ) ;
#103148 = DIRECTION ( 'NONE',  ( 0.8775825618903754233, 0.000000000000000000, 0.4794255386041978984 ) ) ;
#103149 = CARTESIAN_POINT ( 'NONE',  ( -13.16517659032117038, 1517.151704408390060, 224.1947148507618408 ) ) ;
#103150 = CARTESIAN_POINT ( 'NONE',  ( -8.848016400190001463, 1384.939924038890013, 199.9247971377489819 ) ) ;
#103151 = CARTESIAN_POINT ( 'NONE',  ( -22.51439127229999926, 1409.699280255230178, 208.1503399454410328 ) ) ;
#103152 = CARTESIAN_POINT ( 'NONE',  ( 15.66638256379999916, 1416.825421875629900, 199.0472708910980089 ) ) ;
#103153 = CARTESIAN_POINT ( 'NONE',  ( 4.566741015489999889, 1485.595084333989917, 218.8629924376189990 ) ) ;
#103154 = DIRECTION ( 'NONE',  ( 0.000000000000000000, 0.000000000000000000, -1.000000000000000000 ) ) ;
#103155 = CARTESIAN_POINT ( 'NONE',  ( 7.341316150999999179E-16, 1441.600846913620217, 150.7224806086979640 ) ) ;
#103156 = CIRCLE ( 'NONE', #6623, 0.5000000000000000000 ) ;
#103157 = CARTESIAN_POINT ( 'NONE',  ( -17.63206642429129900, 1440.541090996499861, 218.8715579270100022 ) ) ;
#103158 = CARTESIAN_POINT ( 'NONE',  ( 17.34064570863430887, 1525.506926151471589, 181.3217111118486571 ) ) ;
#103159 = CARTESIAN_POINT ( 'NONE',  ( 13.84584237522359906, 1499.900173460709766, 227.7510556141490099 ) ) ;
#103161 = CARTESIAN_POINT ( 'NONE',  ( 11.20854089337319870, 1414.996442620860080, 222.5314268542019818 ) ) ;
#103160 = CARTESIAN_POINT ( 'NONE',  ( -23.10251492229999926, 1410.654477831930080, 210.9078341742080056 ) ) ;
#103162 = CARTESIAN_POINT ( 'NONE',  ( -1.742717375088950107E-15, 1375.426148861440197, 209.1218459572589836 ) ) ;
#103163 = CARTESIAN_POINT ( 'NONE',  ( 9.821586882074960556, 1435.575910505290040, 209.2747408604490147 ) ) ;
#103164 = CARTESIAN_POINT ( 'NONE',  ( -11.06280732299999947, 1490.126969804790178, 211.8519967247989939 ) ) ;
#103165 = CARTESIAN_POINT ( 'NONE',  ( 8.748194321763609338, 1449.742677337359737, 203.5399419409159805 ) ) ;
#103166 = DIRECTION ( 'NONE',  ( -0.8200914087126657259, -0.4884709562387143933, -0.2980708074718346201 ) ) ;
#103167 = CARTESIAN_POINT ( 'NONE',  ( -5.781490582474999584, 1516.807958722750072, 202.5702025453269925 ) ) ;
#103168 = CARTESIAN_POINT ( 'NONE',  ( 5.009886284249999377, 1430.069699660889910, 217.1776678749689893 ) ) ;
#103169 = DIRECTION ( 'NONE',  ( 0.000000000000000000, 1.000000000000000000, 0.000000000000000000 ) ) ;
#103170 = DIRECTION ( 'NONE',  ( 3.828568698926945491E-16, 0.000000000000000000, -1.000000000000000000 ) ) ;
#103171 = CARTESIAN_POINT ( 'NONE',  ( 2.771712507760000221, 1509.009850720929990, 238.2056319702980147 ) ) ;
#103172 = CARTESIAN_POINT ( 'NONE',  ( 40.01057657059909900, 1448.816588776699973, 135.4138680875709895 ) ) ;
#103175 = ORIENTED_EDGE ( 'NONE', *, *, #64415, .T. ) ;
#103174 = CARTESIAN_POINT ( 'NONE',  ( -61.44418850211069838, 1379.737850744239950, 268.2889715896209850 ) ) ;
#103173 = AXIS2_PLACEMENT_3D ( 'NONE', #66568, #93377, #23419 ) ;
#103176 = ORIENTED_EDGE ( 'NONE', *, *, #39710, .F. ) ;
#103177 = CARTESIAN_POINT ( 'NONE',  ( 11.95523955411000117, 1433.542691738470012, 149.9852572030879969 ) ) ;
#103178 = CARTESIAN_POINT ( 'NONE',  ( 26.65386906330000016, 1508.586510756630105, 215.9800495173180082 ) ) ;
#103179 = VERTEX_POINT ( 'NONE', #5751 ) ;
#103180 = CARTESIAN_POINT ( 'NONE',  ( -108.0661743619999982, 1378.913060387289988, 308.5496304198589996 ) ) ;
#103181 = CARTESIAN_POINT ( 'NONE',  ( -10.36694999858590016, 1448.084678120760145, 208.9249857694410082 ) ) ;
#103182 = DIRECTION ( 'NONE',  ( 0.000000000000000000, 1.000000000000000000, 0.000000000000000000 ) ) ;
#103184 = CARTESIAN_POINT ( 'NONE',  ( 4.418986906789999836, 1428.481734779130193, 91.31218443469779800 ) ) ;
#103183 = CARTESIAN_POINT ( 'NONE',  ( 16.00482466429749806, 1421.840373356649934, 191.1776750418199811 ) ) ;
#103185 = CARTESIAN_POINT ( 'NONE',  ( 19.18761048174300043, 1498.115689341469988, 229.1975969832560054 ) ) ;
#103186 = CARTESIAN_POINT ( 'NONE',  ( 1.697557679380000017, 1507.641431191929996, 181.1359668789980049 ) ) ;
#103187 = CARTESIAN_POINT ( 'NONE',  ( 2.727465513059999846, 1467.148923109990164, 219.0926697488289960 ) ) ;
#103188 = LINE ( 'NONE', #43323, #59071 ) ;
#103189 = CARTESIAN_POINT ( 'NONE',  ( 3.461995158685000185, 1516.906233342200039, 211.9877574868770012 ) ) ;
#103190 = CARTESIAN_POINT ( 'NONE',  ( 36.70996913324480460, 1436.286710641320269, 134.0999999969339740 ) ) ;
#103191 = CARTESIAN_POINT ( 'NONE',  ( 13.10606020890036838, 1519.551704408389924, 225.8214468947291493 ) ) ;
#103192 = CARTESIAN_POINT ( 'NONE',  ( 6.490306520025000303, 1514.605246816799763, 201.0943966606369884 ) ) ;
#103193 = VERTEX_POINT ( 'NONE', #91405 ) ;
#103194 = CARTESIAN_POINT ( 'NONE',  ( 13.72600532257040129, 1434.976387550540039, 148.7247796194869807 ) ) ;
#103195 = CARTESIAN_POINT ( 'NONE',  ( -0.4182119524568259639, 1432.129988308659904, 200.7098003538619935 ) ) ;
#103196 = EDGE_LOOP ( 'NONE', ( #56678, #28516, #101666, #28988 ) ) ;
#103197 = ORIENTED_EDGE ( 'NONE', *, *, #11712, .T. ) ;
#103198 = CARTESIAN_POINT ( 'NONE',  ( -7.449529122645000001, 1511.198876514819858, 215.3846915273670106 ) ) ;
#103199 = CARTESIAN_POINT ( 'NONE',  ( -0.7165940425340000530, 1466.721451273230059, 235.5244447404979837 ) ) ;
#103200 = CARTESIAN_POINT ( 'NONE',  ( -11.92254695265209996, 1407.392238798829794, 215.8238487423210188 ) ) ;
#103201 = CIRCLE ( 'NONE', #110323, 1.999999999999999556 ) ;
#103202 = CARTESIAN_POINT ( 'NONE',  ( -0.7403206051589980019, 1517.139320148880188, 216.8467205834170102 ) ) ;
#103203 = CARTESIAN_POINT ( 'NONE',  ( 1.846216073831150162, 1465.868771192480153, 198.2512937515799933 ) ) ;
#103204 = CARTESIAN_POINT ( 'NONE',  ( 11.79334844382369951, 1421.931009736009855, 209.2876916042509947 ) ) ;
#103205 = CARTESIAN_POINT ( 'NONE',  ( -60.87734639771428391, 1379.727522264731078, 263.3640292216577450 ) ) ;
#103206 = CARTESIAN_POINT ( 'NONE',  ( 2.435277524900000046, 1464.768429074390042, 199.5670726285990213 ) ) ;
#103207 = CARTESIAN_POINT ( 'NONE',  ( 1.515709095849999910, 1508.947667959530008, 238.4644442293979978 ) ) ;
#103208 = VERTEX_POINT ( 'NONE', #4109 ) ;
#103209 = CARTESIAN_POINT ( 'NONE',  ( 7.709032137684999952, 1516.534320418310244, 206.6366287381669906 ) ) ;
#103210 = EDGE_LOOP ( 'NONE', ( #79905, #28416, #10829, #82110, #4412, #102103, #75369 ) ) ;
#103211 = CARTESIAN_POINT ( 'NONE',  ( 21.04234019475320139, 1440.913060387330006, 222.5617771367410000 ) ) ;
#103212 = CARTESIAN_POINT ( 'NONE',  ( -19.05944678440000217, 1508.258419023829902, 229.7388470496979949 ) ) ;
#103213 = VERTEX_POINT ( 'NONE', #98692 ) ;
#103214 = CARTESIAN_POINT ( 'NONE',  ( -13.22514030490000003, 1410.307657465529928, 189.8332610226980250 ) ) ;
#103215 = CARTESIAN_POINT ( 'NONE',  ( 6.867779371605000627, 1512.132770473900109, 216.2848484671970084 ) ) ;
#103217 = VERTEX_POINT ( 'NONE', #30934 ) ;
#103216 = CARTESIAN_POINT ( 'NONE',  ( -10.79382126600000014, 1414.913060387329779, 196.1395803457980094 ) ) ;
#103218 = CARTESIAN_POINT ( 'NONE',  ( 22.94699394379999902, 1432.795231260740138, 217.1269739022579870 ) ) ;
#103219 = CARTESIAN_POINT ( 'NONE',  ( -16.45376569770029818, 1508.551704408389924, 210.3850702157819796 ) ) ;
#103220 = CARTESIAN_POINT ( 'NONE',  ( 5.597778194180000888, 1506.679269386989972, 219.3685102149989916 ) ) ;
#103221 = DIRECTION ( 'NONE',  ( 0.8672669759446699489, 0.000000000000000000, 0.4978433412588613716 ) ) ;
#103223 = CARTESIAN_POINT ( 'NONE',  ( 5.398680167209999325, 1433.945743868580166, 154.6429197126979886 ) ) ;
#103222 = CARTESIAN_POINT ( 'NONE',  ( 22.03465957474550407, 1522.382868172863937, 182.8300405912328586 ) ) ;
#103224 = AXIS2_PLACEMENT_3D ( 'NONE', #81509, #72590, #13197 ) ;
#103225 = CARTESIAN_POINT ( 'NONE',  ( 5.007588646914999941, 1516.804776704140068, 214.8970827629769644 ) ) ;
#103226 = CARTESIAN_POINT ( 'NONE',  ( 2.782344708190000127, 1462.431012131489751, 228.5889832501989929 ) ) ;
#103227 = CARTESIAN_POINT ( 'NONE',  ( 0.000000000000000000, 1523.409940573003951, 233.8211094035767985 ) ) ;
#103228 = EDGE_CURVE ( 'NONE', #88474, #100188, #4640, .T. ) ;
#103229 = CARTESIAN_POINT ( 'NONE',  ( 30.01999557802941254, 1525.848196786131666, 221.1300219709211490 ) ) ;
#103230 = CARTESIAN_POINT ( 'NONE',  ( -4.995994825704999975, 1516.665179208830068, 211.6114635085770033 ) ) ;
#103231 = CARTESIAN_POINT ( 'NONE',  ( -11.87206752526750009, 1482.026096006810121, 208.5610132530620149 ) ) ;
#103232 = CARTESIAN_POINT ( 'NONE',  ( 30.60461244942487014, 1523.621879633028811, 221.8232741897816993 ) ) ;
#103234 = ORIENTED_EDGE ( 'NONE', *, *, #24188, .T. ) ;
#103233 = CARTESIAN_POINT ( 'NONE',  ( -76.09690353929998707, 1385.004314140359838, 301.2232021421590389 ) ) ;
#103235 = CARTESIAN_POINT ( 'NONE',  ( 27.41412850780000099, 1466.213804920729899, 262.1296345509980483 ) ) ;
#103236 = EDGE_CURVE ( 'NONE', #53370, #40922, #38233, .T. ) ;
#103237 = CARTESIAN_POINT ( 'NONE',  ( 2.787859546404547917, 1451.851357346741679, 183.8246711244312053 ) ) ;
#103238 = CYLINDRICAL_SURFACE ( 'NONE', #21735, 2.000000000000007550 ) ;
#103239 = CARTESIAN_POINT ( 'NONE',  ( -3.692180645651279569, 1507.990633139789907, 236.8685678891660018 ) ) ;
#103240 = CARTESIAN_POINT ( 'NONE',  ( 7.311826422820000282, 1422.546741514869836, 195.5507102769989842 ) ) ;
#103241 = AXIS2_PLACEMENT_3D ( 'NONE', #99670, #22960, #100771 ) ;
#103243 = CARTESIAN_POINT ( 'NONE',  ( 19.03008511520000212, 1457.014020104829797, 226.0360847140979956 ) ) ;
#103242 = CARTESIAN_POINT ( 'NONE',  ( 11.87300248480000064, 1432.863459016110028, 150.3956791023980202 ) ) ;
#103244 = DIRECTION ( 'NONE',  ( 1.755985294532464991E-16, -1.000000000000000000, 1.338183447452830017E-16 ) ) ;
#103245 = CARTESIAN_POINT ( 'NONE',  ( -107.6819331251149947, 1381.733213848179957, 310.0307816245309596 ) ) ;
#103246 = ORIENTED_EDGE ( 'NONE', *, *, #56826, .T. ) ;
#103247 = CARTESIAN_POINT ( 'NONE',  ( -5.782749439735000330, 1516.858301627840092, 203.3453548368569841 ) ) ;
#103248 = CARTESIAN_POINT ( 'NONE',  ( 0.1080140957969999982, 1405.749477561829963, 267.5371647991979671 ) ) ;
#103249 = CARTESIAN_POINT ( 'NONE',  ( 27.72455317350000215, 1507.994297268330001, 207.7087345480979934 ) ) ;
#103250 = AXIS2_PLACEMENT_3D ( 'NONE', #6391, #32692, #14780 ) ;
#103251 = FACE_OUTER_BOUND ( 'NONE', #69394, .T. ) ;
#103252 = LINE ( 'NONE', #838, #55670 ) ;
#103253 = CARTESIAN_POINT ( 'NONE',  ( 3.266177458080000040, 1467.802312483090191, 218.5517732847689842 ) ) ;
#103254 = CARTESIAN_POINT ( 'NONE',  ( 0.08449630495836644994, 1469.347514019179016, 219.1765324506605452 ) ) ;
#103255 = CARTESIAN_POINT ( 'NONE',  ( -43.73019116030650366, 1440.913060406610157, 264.0439818999259955 ) ) ;
#103256 = DIRECTION ( 'NONE',  ( 0.000000000000000000, 0.000000000000000000, 1.000000000000000000 ) ) ;
#103257 = CARTESIAN_POINT ( 'NONE',  ( 3.774758283729999557E-15, 1461.407663422529822, 243.9198229339980060 ) ) ;
#103258 = CARTESIAN_POINT ( 'NONE',  ( -17.16388877745028907, 1523.678648413191695, 238.6174304775216228 ) ) ;
#103259 = CARTESIAN_POINT ( 'NONE',  ( 8.381577504150859781, 1438.875682636792817, 211.6325970076460976 ) ) ;
#103260 = CARTESIAN_POINT ( 'NONE',  ( -21.66438254905709826, 1525.042337199240137, 184.7096065694357208 ) ) ;
#103261 = CYLINDRICAL_SURFACE ( 'NONE', #24154, 0.9999999999999465983 ) ;
#103262 = VERTEX_POINT ( 'NONE', #63484 ) ;
#103263 = CARTESIAN_POINT ( 'NONE',  ( 0.3331981960608920157, 1408.924696555890023, 186.0526659833350038 ) ) ;
#103264 = CARTESIAN_POINT ( 'NONE',  ( 3.860559482726539926, 1456.030320310470188, 219.0185799711049981 ) ) ;
#103265 = CARTESIAN_POINT ( 'NONE',  ( -22.08523692261585580, 1523.530935881284904, 184.4211863326293326 ) ) ;
#103266 = CARTESIAN_POINT ( 'NONE',  ( -33.91369110859999836, 1435.681798638700002, 135.0664268289980043 ) ) ;
#103267 = CARTESIAN_POINT ( 'NONE',  ( 5.417888360169999669E-14, 1475.048391926230124, 269.6500679732980075 ) ) ;
#103270 = DIRECTION ( 'NONE',  ( -1.000000000000000000, 0.000000000000000000, 0.000000000000000000 ) ) ;
#103269 = CIRCLE ( 'NONE', #78277, 2.000000000000001776 ) ;
#103268 = CARTESIAN_POINT ( 'NONE',  ( 12.25846076559999887, 1500.678402377489874, 208.9469212626399894 ) ) ;
#103271 = CARTESIAN_POINT ( 'NONE',  ( 19.74164504280149757, 1455.376031929259852, 226.0788368184279875 ) ) ;
#103272 = CARTESIAN_POINT ( 'NONE',  ( 8.911818219449999745, 1428.279464179490105, 213.0373091593789923 ) ) ;
#103273 = CARTESIAN_POINT ( 'NONE',  ( -17.16271615814169849, 1384.870831643229849, 219.9644665330189923 ) ) ;
#103274 = B_SPLINE_CURVE_WITH_KNOTS ( 'NONE', 3,
 ( #44383, #27562, #61746, #33741, #69043, #34854, #85245, #67936, #94200, #102042, #1838, #9643, #10207, #77964, #34303, #18040, #78527, #104275, #59525, #1272, #85809, #25329, #76870, #26446, #95322, #183, #69599, #27018, #16372, #70163, #18584, #84696, #35411, #93637, #52779, #16917, #17471, #43274, #77420, #724, #103145, #60640, #38706, #104825, #79092, #87486, #80175, #106474, #2945, #53910, #63949, #2400, #105942, #29221, #55540, #47131, #97525, #11330, #10773, #29759, #95868, #20795, #20252, #11871, #21334, #38164, #4036, #72882, #107020, #37066, #98063, #30308, #12409, #37619, #71821, #19707, #79643, #54997, #63410, #89664, #12950, #44945, #81257, #46593, #89120, #4572, #46043, #54452, #71262, #62302, #80728, #19134, #53338, #36518, #70711, #72345, #3491, #28111, #105383, #96429, #88045, #45501, #28671, #62876, #96988, #88588, #5676, #39822, #56077, #31963, #73983, #108113, #109782, #49885, #90766, #84018, #75093, #7318, #58283, #15143, #5107, #66698, #90203, #100806, #39262, #109242, #83459, #82917, #47677, #65032, #6754, #48795, #99150, #92408, #24094, #65589, #41482, #107570, #15680, #22994, #75643, #40914, #49333, #6209, #73436, #64498, #100277, #31407, #23557, #91323, #14046, #66156, #14605, #98614, #81806, #57749, #21877, #13487, #48236, #32526, #30857, #22428, #91869, #40360, #74541, #56630, #82377, #99702, #108673, #57199, #77835, #24634, #77294, #103012, #25196, #18445, #60500, #42575, #86225, #9516, #101343, #86781, #67248, #10070, #61069, #94622, #51531, #26308, #85115, #43136, #592, #33599, #101904, #52644, #85665, #92968, #84569, #39, #44244, #50986, #25750, #76726, #78388, #33060, #59399, #58831, #43684, #16240, #26880, #17897, #7860, #59952, #34170, #52094, #67794, #68356, #103578, #95186, #68910, #42028, #110326, #17337, #93510, #50444, #76177, #102462, #16782, #8403, #35276, #94068, #8965, #69461, #1144, #34720, #12270, #104134, #27420, #70020, #37487, #62164, #88982, #3361, #62734, #29626, #19000, #80040, #35837, #3909, #106340, #29089, #61603, #21194, #104685, #71691, #36926, #20124, #53773, #53200, #63810, #12825, #47005, #96855, #46462, #19567, #70567, #80595, #95736, #11735, #45904, #72218, #97927, #105809, #27979, #87340, #38038, #1696, #36378, #96290, #55404, #10636, #87909, #89536, #44804, #78957, #2264, #11198, #45362, #54316, #88445, #79501, #2808, #71123, #105244, #28535, #63274, #97385, #20656, #54858, #82789, #109115, #58159, #4974, #39118, #57622 ),
 .UNSPECIFIED., .F., .F.,
 ( 4, 3, 3, 3, 3, 3, 3, 3, 3, 3, 3, 3, 3, 3, 3, 3, 3, 3, 3, 3, 3, 3, 3, 3, 3, 3, 3, 3, 3, 3, 3, 3, 3, 3, 3, 3, 3, 3, 3, 3, 3, 3, 3, 3, 3, 3, 3, 3, 3, 3, 3, 3, 3, 3, 3, 3, 3, 3, 3, 3, 3, 3, 3, 3, 3, 3, 3, 3, 3, 3, 3, 3, 3, 3, 3, 3, 3, 3, 3, 3, 3, 3, 3, 3, 3, 3, 3, 3, 3, 3, 3, 3, 3, 3, 3, 3, 3, 3, 3, 3, 3, 4 ),
 ( 8.502096524649999765, 10.07864787959089981, 11.93479254620110019, 13.53107985676839853, 14.91300515749670019, 15.39383910900589925, 16.53746239350300229, 17.65458387737769996, 18.74843729357949940, 19.85248863406109976, 20.89822462007209936, 21.92896863737080082, 22.94591180423740084, 23.95008399577969982, 24.93651389660379891, 25.91373036143600217, 26.87743017290080161, 27.58084801743209979, 28.63657303752779981, 29.71534806165689702, 30.81785565885160239, 31.94355054423600038, 33.12499366665170442, 34.29034599565019903, 35.45679948715110186, 36.61536720514430243, 37.81029928474870161, 38.92267659857289885, 40.01573463098910111, 41.08144785925959752, 41.39509552356179967, 42.90409533963379829, 44.42240685342919448, 45.95641701915690192, 47.50713568527189778, 49.07569676298640360, 50.66338138030639726, 52.27164696925940035, 53.93007767069119751, 55.59733588536930426, 57.29035514786890104, 59.01163268845090215, 60.78223427696999437, 62.58432007834910138, 64.44189006276219800, 65.53909258071379895, 67.04466091477729606, 68.62874293280711413, 70.27935153705820426, 72.01713397602310351, 73.87821637511270012, 75.94820385017399644, 78.63691978283431183, 80.96957215551108789, 82.94440381128279682, 84.75275152858640126, 86.41315054547159491, 88.01530566766550123, 89.54414943656179560, 90.91108773666839227, 93.83029885312799934, 96.80610674239019886, 99.57495006331539855, 102.2152258246999992, 104.7433345856459965, 107.1773875570659982, 109.5324586405310043, 111.7902715113670098, 114.0014454456810000, 116.1495204710570022, 117.6367619672259934, 119.0972352214530048, 120.5529424179680262, 122.0399992496289912, 123.4355467568209832, 124.8016281987520131, 126.1383812957949999, 127.4470804953769942, 128.7157394665759966, 129.9643185484640071, 131.2068578098609919, 132.4493970712580335, 133.6732891993179919, 135.0123274964250015, 136.6169184369290122, 138.3144093969239918, 139.6958786578699971, 140.9759288702229867, 142.1124124449380020, 143.2059073724689995, 144.2494749791640061, 144.8160795072840017, 146.1144237599960150, 147.4424597893359987, 148.8129228152089922, 150.2046619519239812, 151.6094994080520166, 153.0694599465389842, 154.4582506042169996, 155.8279853376390065, 157.1656630716910001, 157.4493415620000007 ),
 .UNSPECIFIED. ) ;
#103275 = B_SPLINE_CURVE_WITH_KNOTS ( 'NONE', 3,
 ( #7725, #8267, #76590, #102329, #16647, #110741, #100674, #68223, #92832, #110188, #58152, #25615, #75511, #16108, #51390, #109645, #59807, #23957, #41886, #76044, #93926, #57614, #85522, #462, #8817 ),
 .UNSPECIFIED., .F., .F.,
 ( 4, 3, 3, 3, 3, 3, 3, 3, 4 ),
 ( -7.690123547477719868, -7.578754016464039900, -6.856148510135199992, -6.131423372794370330, -5.422190055320710300, -5.213236018046780273, -4.581108567758639616, -3.740027080196560050, -3.154256035599999564 ),
 .UNSPECIFIED. ) ;
#103276 = CARTESIAN_POINT ( 'NONE',  ( -5.864566082395439750, 1517.051704408389924, 192.0899093523580063 ) ) ;
#103277 = CARTESIAN_POINT ( 'NONE',  ( -17.40764059099999628, 1414.996444526030018, 207.5654758040780052 ) ) ;
#103278 = CARTESIAN_POINT ( 'NONE',  ( -8.719918377449999980, 1483.750365165289850, 201.5181060481390034 ) ) ;
#103279 = CARTESIAN_POINT ( 'NONE',  ( 24.61958478200000044, 1435.541888381590070, 137.0853135175979958 ) ) ;
#103280 = CARTESIAN_POINT ( 'NONE',  ( -8.998480011645090926, 1396.227294235010049, 202.6956182965139988 ) ) ;
#103281 = ORIENTED_EDGE ( 'NONE', *, *, #12558, .F. ) ;
#103282 = CARTESIAN_POINT ( 'NONE',  ( -16.90341314920719995, 1409.749895306139933, 225.4593008893319848 ) ) ;
#103283 = CARTESIAN_POINT ( 'NONE',  ( 11.96519809220000141, 1440.444625599219989, 147.6189886498980002 ) ) ;
#103284 = ORIENTED_EDGE ( 'NONE', *, *, #13099, .F. ) ;
#103285 = ORIENTED_EDGE ( 'NONE', *, *, #42666, .F. ) ;
#103286 = CARTESIAN_POINT ( 'NONE',  ( 20.58427237330526438, 1512.187213306747481, 216.4826520421586338 ) ) ;
#103287 = CARTESIAN_POINT ( 'NONE',  ( -173.8335085727399871, 1524.382868172863937, 100.8557906292094231 ) ) ;
#103289 = CARTESIAN_POINT ( 'NONE',  ( -0.8560893484002659592, 1457.237409688020080, 219.7250069795780121 ) ) ;
#103288 = DIRECTION ( 'NONE',  ( -0.01486624123577086690, -0.9944765560314704489, -0.1039007910234840543 ) ) ;
#103290 = DIRECTION ( 'NONE',  ( 0.000000000000000000, 1.000000000000000000, 0.000000000000000000 ) ) ;
#103291 = CARTESIAN_POINT ( 'NONE',  ( -11.25103233189999941, 1433.013630249540029, 151.5370651328979932 ) ) ;
#103292 = AXIS2_PLACEMENT_3D ( 'NONE', #44625, #102833, #2081 ) ;
#103293 = CARTESIAN_POINT ( 'NONE',  ( -2.557132965088358745, 1420.768154751241354, 185.5685875094732751 ) ) ;
#103294 = CARTESIAN_POINT ( 'NONE',  ( 7.944350852719999523, 1425.480812533560083, 211.5441705370589887 ) ) ;
#103295 = CARTESIAN_POINT ( 'NONE',  ( -9.104803454449999833, 1421.479062531979935, 192.1853131694989827 ) ) ;
#103296 = CARTESIAN_POINT ( 'NONE',  ( 8.313290118299999421, 1507.316777386929971, 183.0869028357980142 ) ) ;
#103297 = FACE_OUTER_BOUND ( 'NONE', #8237, .T. ) ;
#103298 = CARTESIAN_POINT ( 'NONE',  ( 9.842969107833919651, 1365.740588703670028, 210.6218459616987957 ) ) ;
#103300 = VERTEX_POINT ( 'NONE', #57277 ) ;
#103299 = DIRECTION ( 'NONE',  ( 1.000000000000000000, 0.000000000000000000, 1.942890293094025713E-13 ) ) ;
#103301 = ORIENTED_EDGE ( 'NONE', *, *, #70106, .T. ) ;
#103302 = CARTESIAN_POINT ( 'NONE',  ( -41.15075926320000121, 1443.752932596629989, 136.9300405401980072 ) ) ;
#103303 = ADVANCED_FACE ( 'NONE', ( #55069 ), #33790, .F. ) ;
#103304 = FACE_OUTER_BOUND ( 'NONE', #48029, .T. ) ;
#103305 = CARTESIAN_POINT ( 'NONE',  ( -2.255308465020000153, 1472.005448226929957, 270.0715991240979861 ) ) ;
#103306 = CARTESIAN_POINT ( 'NONE',  ( 12.32497982002866266, 1434.251326250639295, 147.3969771501246839 ) ) ;
#103307 = CARTESIAN_POINT ( 'NONE',  ( -0.5851024498960000209, 1486.106971620530203, 181.8803045006980028 ) ) ;
#103308 = B_SPLINE_CURVE_WITH_KNOTS ( 'NONE', 3,
 ( #80228, #107626, #21387, #46099, #4624, #39319 ),
 .UNSPECIFIED., .F., .F.,
 ( 4, 2, 4 ),
 ( 2.797157557069881010E-17, 0.001087661325621672604, 0.002175322651243317019 ),
 .UNSPECIFIED. ) ;
#103310 = EDGE_CURVE ( 'NONE', #40014, #68662, #31480, .T. ) ;
#103309 = DIRECTION ( 'NONE',  ( -1.000000000000000000, -2.249639673992789970E-32, -1.224646799147350002E-16 ) ) ;
#103311 = CARTESIAN_POINT ( 'NONE',  ( -1.474640905272780023, 1475.430171080190121, 197.7716959656699771 ) ) ;
#103312 = CARTESIAN_POINT ( 'NONE',  ( -36.33136068457189793, 1451.260137002700048, 135.5554792738989818 ) ) ;
#103313 = ADVANCED_FACE ( 'NONE', ( #29288 ), #82907, .F. ) ;
#103314 = CARTESIAN_POINT ( 'NONE',  ( -2.500000000000000000, 1448.203469879150134, 169.7706540686479855 ) ) ;
#103315 = CARTESIAN_POINT ( 'NONE',  ( 9.478478336866400511, 1368.047529015550481, 210.6218459617030021 ) ) ;
#103316 = CARTESIAN_POINT ( 'NONE',  ( 13.58011004080560014, 1408.357478272720073, 204.5339713451270143 ) ) ;
#103317 = CARTESIAN_POINT ( 'NONE',  ( -10.48381364300569984, 1407.657513889099846, 269.6151450982960114 ) ) ;
#103318 = CARTESIAN_POINT ( 'NONE',  ( -13.75801960019769865, 1434.977933834450141, 148.5785497869700009 ) ) ;
#103319 = VERTEX_POINT ( 'NONE', #25819 ) ;
#103320 = CARTESIAN_POINT ( 'NONE',  ( 3.658687503250000361, 1424.106386281430105, 183.9658221167980230 ) ) ;
#103321 = CARTESIAN_POINT ( 'NONE',  ( 13.57984947760000161, 1443.954740135339762, 188.4659268699979862 ) ) ;
#103322 = ORIENTED_EDGE ( 'NONE', *, *, #68117, .T. ) ;
#103323 = CIRCLE ( 'NONE', #92624, 32.13701971169416538 ) ;
#103324 = VERTEX_POINT ( 'NONE', #50512 ) ;
#103325 = CARTESIAN_POINT ( 'NONE',  ( 4.796254352853694058, 1422.272280406457867, 184.2473515962519173 ) ) ;
#103326 = CARTESIAN_POINT ( 'NONE',  ( -8.962252599310001955, 1366.920250605820002, 207.6218459616989946 ) ) ;
#103327 = VECTOR ( 'NONE', #56899, 1000.000000000000000 ) ;
#103328 = CARTESIAN_POINT ( 'NONE',  ( -4.998515195425000002, 1516.787536375099990, 213.1617432482970003 ) ) ;
#103329 = CARTESIAN_POINT ( 'NONE',  ( -17.77992640079999731, 1470.471868837129932, 189.4977790897980015 ) ) ;
#103330 = B_SPLINE_SURFACE_WITH_KNOTS ( 'NONE', 5, 5, ( 
 ( #32583, #100859, #24150, #110381, #58340, #33660 ),
 ( #8459, #49936, #92464, #42633, #7373, #84075 ),
 ( #41537, #67305, #25805, #24693, #102514, #91389 ),
 ( #48855, #66213, #50498, #58888, #85174, #93564 ),
 ( #84620, #7914, #76784, #68410, #42086, #67852 ),
 ( #101965, #102, #82979, #25251, #16838, #59454 ) ),
 .UNSPECIFIED., .F., .F., .F.,
 ( 6, 6 ),
 ( 6, 6 ),
 ( 2.324858856890000158, 4.991117563570000470 ),
 ( 0.000000000000000000, 0.5000000000000000000 ),
 .UNSPECIFIED. ) ;
#103331 = CIRCLE ( 'NONE', #37264, 29.84605316648919526 ) ;
#103332 = VERTEX_POINT ( 'NONE', #15750 ) ;
#103333 = CARTESIAN_POINT ( 'NONE',  ( -204.2714532754873744, 1526.382868172863937, 223.7095399770904010 ) ) ;
#103334 = VECTOR ( 'NONE', #56388, 1000.000000000000114 ) ;
#103335 =( BOUNDED_CURVE ( )  B_SPLINE_CURVE ( 3, ( #92221, #74890, #8199, #93857 ),
 .UNSPECIFIED., .F., .F. ) 
 B_SPLINE_CURVE_WITH_KNOTS ( ( 4, 4 ),
 ( 1.431195359047013893, 1.487065270106493919 ),
 .UNSPECIFIED. ) 
 CURVE ( )  GEOMETRIC_REPRESENTATION_ITEM ( )  RATIONAL_B_SPLINE_CURVE ( ( 1.000000000000000000, 0.9997398963350896395, 0.9997398963350896395, 1.000000000000000000 ) ) 
 REPRESENTATION_ITEM ( '' )  );
#103336 = CARTESIAN_POINT ( 'NONE',  ( 9.986924024219998586, 1415.932617990029939, 224.5919156272979933 ) ) ;
#103337 = CARTESIAN_POINT ( 'NONE',  ( 0.7376675027960020170, 1517.104497701820037, 203.3349981924270082 ) ) ;
#103338 = CARTESIAN_POINT ( 'NONE',  ( -28.15433623620000247, 1508.637654267429980, 208.1158776034079949 ) ) ;
#103339 = CARTESIAN_POINT ( 'NONE',  ( -2.714430944004193158, 1517.051704408389696, 217.0111434691034731 ) ) ;
#103340 = CARTESIAN_POINT ( 'NONE',  ( -39.75532303620000363, 1384.581637800209819, 212.4630896483189701 ) ) ;
#103341 = ADVANCED_FACE ( 'NONE', ( #60017 ), #46389, .F. ) ;
#103342 = CARTESIAN_POINT ( 'NONE',  ( -55.77908735024080045, 1384.648364377080043, 235.3611123942870051 ) ) ;
#103343 = CARTESIAN_POINT ( 'NONE',  ( -4.131009387019999757, 1408.874545657929957, 195.5701569932979851 ) ) ;
#103344 = CARTESIAN_POINT ( 'NONE',  ( -12.57480364899999969, 1409.852123968930073, 227.8141353385980210 ) ) ;
#103346 = ORIENTED_EDGE ( 'NONE', *, *, #324, .F. ) ;
#103345 = CARTESIAN_POINT ( 'NONE',  ( -12.41052241149999880, 1445.069700341559837, 185.9600454165980068 ) ) ;
#103347 = CARTESIAN_POINT ( 'NONE',  ( -24.08291145960179946, 1411.090674597109910, 208.6097594128350181 ) ) ;
#103348 = CARTESIAN_POINT ( 'NONE',  ( 27.02980867440000168, 1488.688182087729956, 211.4493640585079959 ) ) ;
#103349 = CARTESIAN_POINT ( 'NONE',  ( 10.67217592544739979, 1460.316194025420145, 206.8193158878239899 ) ) ;
#103350 = CARTESIAN_POINT ( 'NONE',  ( -25.04275794140000144, 1435.378124283050056, 135.9084131103979871 ) ) ;
#103351 = VECTOR ( 'NONE', #17453, 1000.000000000000114 ) ;
#103352 = CARTESIAN_POINT ( 'NONE',  ( 2.879956924955000108, 1516.827328999679821, 212.3743765858270081 ) ) ;
#103353 = CARTESIAN_POINT ( 'NONE',  ( -68.34315272460000301, 1379.747704235549918, 279.2339980437589588 ) ) ;
#103354 = CARTESIAN_POINT ( 'NONE',  ( -18.79700370569999635, 1444.661305230889866, 207.2600034499489823 ) ) ;
#103355 = CARTESIAN_POINT ( 'NONE',  ( -30.16752008203960500, 1524.964158026965833, 221.7255342961994700 ) ) ;
#103356 = CARTESIAN_POINT ( 'NONE',  ( -2.297629659184999618, 1516.970035769810011, 208.3868227339359862 ) ) ;
#103357 = EDGE_LOOP ( 'NONE', ( #63444, #55575, #37492, #52634 ) ) ;
#103358 = CARTESIAN_POINT ( 'NONE',  ( -26.39367551872020101, 1440.913056983640217, 211.7580267479229974 ) ) ;
#103359 = CARTESIAN_POINT ( 'NONE',  ( -2.832144297430000179, 1410.303523779030002, 232.5720248812980060 ) ) ;
#103360 = CARTESIAN_POINT ( 'NONE',  ( -36.10875963189999283, 1384.937915446980014, 235.4744139267589844 ) ) ;
#103361 = ORIENTED_EDGE ( 'NONE', *, *, #94752, .T. ) ;
#103362 = CARTESIAN_POINT ( 'NONE',  ( -14.82755886204359896, 1385.295373219239991, 219.3747924830010163 ) ) ;
#103363 = CARTESIAN_POINT ( 'NONE',  ( 11.60004869885203682, 1411.254281879943164, 135.5999999980979851 ) ) ;
#103364 = CARTESIAN_POINT ( 'NONE',  ( 12.48155824441049866, 1435.524277019780129, 150.9067716058439714 ) ) ;
#103365 = EDGE_CURVE ( 'NONE', #25738, #79870, #66227, .T. ) ;
#103366 = CARTESIAN_POINT ( 'NONE',  ( 15.64058445933870090, 1488.407880391730032, 230.9639646109729938 ) ) ;
#103367 = CARTESIAN_POINT ( 'NONE',  ( -24.40973383587160228, 1509.744644423489945, 224.4882036239870047 ) ) ;
#103368 = CARTESIAN_POINT ( 'NONE',  ( -1.674594060629999825, 1409.138563759730005, 186.6870598632980034 ) ) ;
#103369 = CARTESIAN_POINT ( 'NONE',  ( 4.414758600232289609, 1430.295245474100057, 217.5194609254549789 ) ) ;
#103370 = CARTESIAN_POINT ( 'NONE',  ( 32.38845791999500534, 1518.913060387330006, 216.1254071228445639 ) ) ;
#103372 = CARTESIAN_POINT ( 'NONE',  ( 11.13187122630000125, 1480.405616529990084, 211.3597187323589992 ) ) ;
#103371 = CARTESIAN_POINT ( 'NONE',  ( -6.550389470255000290, 1516.755758396839838, 214.1281755516169767 ) ) ;
#103373 = CARTESIAN_POINT ( 'NONE',  ( 19.58834138799999991, 1508.062712335030028, 188.7849770318979949 ) ) ;
#103375 = B_SPLINE_CURVE_WITH_KNOTS ( 'NONE', 3,
 ( #31492, #108758, #6300, #32609, #65672, #32050, #99790, #66239, #15228, #83544, #6838, #73528, #109867, #92494, #40997, #107662, #75176, #109326, #65123, #675, #70105, #51070, #34805, #84648, #67884, #94150, #77373, #59480, #110410, #131, #16867, #25279, #68437, #68993, #93591, #101993, #27506, #85200, #103094, #60589, #8487, #42661, #26394, #95815, #76816, #34254, #94709, #69546, #52728, #77917, #7945, #102540, #9596, #52181, #86863 ),
 .UNSPECIFIED., .F., .F.,
 ( 4, 2, 2, 1, 2, 2, 2, 2, 2, 2, 2, 2, 2, 2, 2, 2, 1, 1, 2, 2, 2, 2, 1, 1, 2, 2, 2, 2, 2, 4 ),
 ( 0.000000000000000000, 0.06250000000056427085, 0.09375000000084640628, 0.1093750000009878487, 0.1171875000010581952, 0.1250000000011285139, 0.1875000000010392243, 0.2187500000009074685, 0.2500000000007757128, 0.3750000000002559064, 0.4374999999998605560, 0.4999999999994652056, 0.5624999999990698551, 0.5937499999988681276, 0.6249999999986662891, 0.6874999999985312860, 0.7187499999984703347, 0.7343749999985430543, 0.7421874999986711741, 0.7499999999987991828, 0.8124999999987877475, 0.8437499999987821964, 0.8593749999987091437, 0.8671874999986661781, 0.8710937499986443067, 0.8749999999986225463, 0.9062499999989295230, 0.9218749999990830668, 0.9374999999992364996, 1.000000000000000000 ),
 .UNSPECIFIED. ) ;
#103374 = CARTESIAN_POINT ( 'NONE',  ( 1.708092266164999984, 1516.523379810429788, 216.8305916180169959 ) ) ;
#103376 = ORIENTED_EDGE ( 'NONE', *, *, #105503, .T. ) ;
#103377 = CARTESIAN_POINT ( 'NONE',  ( 7.891238774076772877, 1519.551704408389924, 189.5145166091761553 ) ) ;
#103378 = CARTESIAN_POINT ( 'NONE',  ( 15.69795926444620271, 1517.151704408390060, 222.7678737639049871 ) ) ;
#103379 = ORIENTED_EDGE ( 'NONE', *, *, #17874, .T. ) ;
#103380 = CARTESIAN_POINT ( 'NONE',  ( 2.523331955360000212, 1419.463757169429982, 185.1820755668979643 ) ) ;
#103381 = CARTESIAN_POINT ( 'NONE',  ( -109.1311031668469411, 1384.887895505450388, 311.2646947245262368 ) ) ;
#103382 = CARTESIAN_POINT ( 'NONE',  ( 8.274182124064189736, 1511.569910118449798, 203.2859663394350207 ) ) ;
#103383 = CARTESIAN_POINT ( 'NONE',  ( 2.839373935849999864, 1442.324148150689780, 217.6523810350290091 ) ) ;
#103384 = CARTESIAN_POINT ( 'NONE',  ( -29.99674465255699474, 1524.860077346004800, 195.9762169038188517 ) ) ;
#103385 = CARTESIAN_POINT ( 'NONE',  ( -20.69714284706251917, 1525.848196786131211, 233.9618279170393009 ) ) ;
#103386 = CARTESIAN_POINT ( 'NONE',  ( -3.709912251880000067, 1447.069507299949919, 154.3963887763979983 ) ) ;
#103387 = CARTESIAN_POINT ( 'NONE',  ( 10.79356334649999916, 1490.085259999289974, 207.2636451086090119 ) ) ;
#103388 = CARTESIAN_POINT ( 'NONE',  ( 10.04317694198510047, 1459.686705811340062, 204.8127587182970046 ) ) ;
#103389 = CARTESIAN_POINT ( 'NONE',  ( -5.001772368710000194, 1443.913060387330006, 150.4106346902979965 ) ) ;
#103390 = CARTESIAN_POINT ( 'NONE',  ( 15.84151803160000327, 1416.228840385830154, 191.3509196118980071 ) ) ;
#103392 = CARTESIAN_POINT ( 'NONE',  ( 0.5834642750313309145, 1464.825178575939844, 188.3591715439980021 ) ) ;
#103391 = CARTESIAN_POINT ( 'NONE',  ( -2.472534047699199711, 1422.360495435749954, 192.6709246226909613 ) ) ;
#103393 = CARTESIAN_POINT ( 'NONE',  ( 2.792392588003326903, 1526.382868172863937, 241.3440112565233164 ) ) ;
#103394 = VERTEX_POINT ( 'NONE', #68979 ) ;
#103395 = CARTESIAN_POINT ( 'NONE',  ( -32.38845791999504797, 1512.187213306747481, 202.1182848005516348 ) ) ;
#103396 = CARTESIAN_POINT ( 'NONE',  ( 27.08643475359999897, 1507.996733211630044, 207.0060423009980184 ) ) ;
#103397 = CIRCLE ( 'NONE', #55180, 6.868727599660006788 ) ;
#103398 = EDGE_CURVE ( 'NONE', #96461, #91877, #100787, .T. ) ;
#103399 = DIRECTION ( 'NONE',  ( 0.7384854939282339270, -4.128709092058508552E-17, -0.6742693640212139572 ) ) ;
#103400 = CARTESIAN_POINT ( 'NONE',  ( 17.71193101166619854, 1522.051704408389924, 196.6727161458730109 ) ) ;
#103401 = VECTOR ( 'NONE', #62888, 1000.000000000000114 ) ;
#103402 = EDGE_CURVE ( 'NONE', #86024, #43369, #13922, .T. ) ;
#103403 = CARTESIAN_POINT ( 'NONE',  ( -10.45767044947240088, 1479.639629119470101, 210.0294207369939841 ) ) ;
#103404 = PLANE ( 'NONE',  #5527 ) ;
#103405 = CARTESIAN_POINT ( 'NONE',  ( -11.11783079367559957, 1470.257259110569976, 211.5455878590279895 ) ) ;
#103406 = AXIS2_PLACEMENT_3D ( 'NONE', #50430, #59936, #100789 ) ;
#103407 = CARTESIAN_POINT ( 'NONE',  ( -2.193888375216459963, 1486.670272915489932, 220.4458273536270099 ) ) ;
#103408 = CARTESIAN_POINT ( 'NONE',  ( 12.98226561589999939, 1414.913060387329779, 198.3280246956980193 ) ) ;
#103409 = CARTESIAN_POINT ( 'NONE',  ( -71.81454634048201058, 1383.783546078690051, 296.7712788830790487 ) ) ;
#103410 = AXIS2_PLACEMENT_3D ( 'NONE', #81188, #73360, #4505 ) ;
#103411 = CARTESIAN_POINT ( 'NONE',  ( 16.56219860610000083, 1451.518047273530101, 149.1091192963980063 ) ) ;
#103412 = CARTESIAN_POINT ( 'NONE',  ( -106.4020496450190052, 1391.913060387289988, 304.2007955189830568 ) ) ;
#103413 = CARTESIAN_POINT ( 'NONE',  ( -1.013215592032840062, 1516.657104395810165, 201.4095985828120092 ) ) ;
#103415 = ORIENTED_EDGE ( 'NONE', *, *, #7683, .F. ) ;
#103414 = CARTESIAN_POINT ( 'NONE',  ( 25.00063024130000144, 1509.786765447930065, 193.6023525624979982 ) ) ;
#103416 = CARTESIAN_POINT ( 'NONE',  ( -1.471222536434999784, 1414.913526854310021, 226.2200213458429801 ) ) ;
#103417 = CARTESIAN_POINT ( 'NONE',  ( -79.42094436850000250, 1379.292317202809954, 292.9105207063590228 ) ) ;
#103418 = CARTESIAN_POINT ( 'NONE',  ( 18.18137504628520063, 1507.546748557000001, 186.5307075251750177 ) ) ;
#103419 = ORIENTED_EDGE ( 'NONE', *, *, #60946, .F. ) ;
#103420 = ORIENTED_EDGE ( 'NONE', *, *, #109763, .F. ) ;
#103421 = CARTESIAN_POINT ( 'NONE',  ( 14.09542765070000137, 1445.387346742360023, 189.3996806953979899 ) ) ;
#103422 = B_SPLINE_CURVE_WITH_KNOTS ( 'NONE', 3,
 ( #82795, #48670, #67125, #6090, #39697, #83344, #74974, #24524, #50329 ),
 .UNSPECIFIED., .F., .F.,
 ( 4, 1, 2, 2, 4 ),
 ( 0.000000000000000000, 0.2500000000000182632, 0.3750000000000175970, 0.5000000000000169864, 1.000000000000000000 ),
 .UNSPECIFIED. ) ;
#103423 = CARTESIAN_POINT ( 'NONE',  ( -10.41132050640262996, 1517.151704408390060, 189.4661702785461728 ) ) ;
#103424 = CARTESIAN_POINT ( 'NONE',  ( 37.27029739945400166, 1438.078572600510142, 136.5691528236939973 ) ) ;
#103426 = CARTESIAN_POINT ( 'NONE',  ( -42.47347404569999441, 1448.912595586219823, 263.9447133204980105 ) ) ;
#103425 = CARTESIAN_POINT ( 'NONE',  ( 13.57505907252250310, 1412.033808172750469, 269.3590162744131931 ) ) ;
#103427 = CARTESIAN_POINT ( 'NONE',  ( 9.808562800256929393, 1435.340065754910029, 208.7021925875509964 ) ) ;
#103428 = CARTESIAN_POINT ( 'NONE',  ( -108.8600183350000066, 1381.954052101950083, 297.7238345936590349 ) ) ;
#103429 = CARTESIAN_POINT ( 'NONE',  ( -12.06466153778595540, 1435.468980856949202, 151.1548757136271774 ) ) ;
#103430 = CARTESIAN_POINT ( 'NONE',  ( -18.72407526530000155, 1458.246115540929850, 227.3156487912980026 ) ) ;
#103431 = AXIS2_PLACEMENT_3D ( 'NONE', #32010, #23603, #7360 ) ;
#103432 = EDGE_CURVE ( 'NONE', #54193, #98450, #1771, .T. ) ;
#103433 = CARTESIAN_POINT ( 'NONE',  ( 2.216568699310000223, 1409.495539288629971, 185.7088051529979964 ) ) ;
#103434 = CARTESIAN_POINT ( 'NONE',  ( 4.098401964949999865, 1424.674504371229887, 185.1777059284979998 ) ) ;
#103435 = CARTESIAN_POINT ( 'NONE',  ( -11.26681287859999969, 1433.831804755629946, 151.5577293853980052 ) ) ;
#103436 = CARTESIAN_POINT ( 'NONE',  ( 9.894254036040001310, 1435.855537113729724, 152.5794184490980001 ) ) ;
#103437 = CARTESIAN_POINT ( 'NONE',  ( -4.500000000000000000, 1448.210448412289907, 170.2811368938980081 ) ) ;
#103438 = CARTESIAN_POINT ( 'NONE',  ( -6.301803161020000488, 1452.256379489029996, 153.3432975151980031 ) ) ;
#103439 = CARTESIAN_POINT ( 'NONE',  ( 21.01415622463856891, 1522.051704408389924, 200.8719909741391803 ) ) ;
#103440 = ORIENTED_EDGE ( 'NONE', *, *, #15331, .T. ) ;
#103441 = CARTESIAN_POINT ( 'NONE',  ( -11.59117397610000033, 1507.247540214189939, 207.5195457387889917 ) ) ;
#103442 = EDGE_CURVE ( 'NONE', #58469, #38935, #49889, .T. ) ;
#103443 = CARTESIAN_POINT ( 'NONE',  ( 10.95119923923629912, 1479.297566038250125, 229.8393126471409857 ) ) ;
#103444 = CARTESIAN_POINT ( 'NONE',  ( -42.57409307820000066, 1450.173233224009891, 270.2305074514979992 ) ) ;
#103445 = CARTESIAN_POINT ( 'NONE',  ( -119.8718586775641484, 1384.899971913130003, 299.5197653927721149 ) ) ;
#103446 = CARTESIAN_POINT ( 'NONE',  ( 16.81340943980000091, 1409.500197579730184, 223.0320505808980158 ) ) ;
#103447 = EDGE_CURVE ( 'NONE', #36569, #82691, #31393, .T. ) ;
#103448 = CARTESIAN_POINT ( 'NONE',  ( -8.861333410889999485, 1384.870662623839962, 218.6848950059789729 ) ) ;
#103449 = CARTESIAN_POINT ( 'NONE',  ( 11.16733641199999916, 1453.313060387329870, 192.7512321736979857 ) ) ;
#103450 = CARTESIAN_POINT ( 'NONE',  ( -4.364199663720353506, 1509.032014613822184, 213.2377092680158341 ) ) ;
#103451 = CARTESIAN_POINT ( 'NONE',  ( -2.075457432642690225, 1421.202448102600101, 193.7464090391210334 ) ) ;
#103452 = CARTESIAN_POINT ( 'NONE',  ( -8.076961596850001257, 1418.814380367629838, 233.3636024205979993 ) ) ;
#103453 = EDGE_CURVE ( 'NONE', #107968, #47285, #40723, .T. ) ;
#103454 = CARTESIAN_POINT ( 'NONE',  ( 0.1595995995380000143, 1486.508831850330125, 181.8147405652979671 ) ) ;
#103455 = CARTESIAN_POINT ( 'NONE',  ( 3.426613460956668078, 1360.656565846701824, 210.6218459616991936 ) ) ;
#103456 = CARTESIAN_POINT ( 'NONE',  ( -46.07249033020909934, 1438.837360396860049, 268.2071385507119885 ) ) ;
#103457 = LINE ( 'NONE', #26763, #60560 ) ;
#103458 = EDGE_LOOP ( 'NONE', ( #3968, #108461, #71931, #60750 ) ) ;
#103459 = CARTESIAN_POINT ( 'NONE',  ( -8.218152191339997970, 1424.217405426100186, 209.2885718405189834 ) ) ;
#103460 = ADVANCED_FACE ( 'NONE', ( #26951 ), #52714, .T. ) ;
#103461 = ORIENTED_EDGE ( 'NONE', *, *, #9797, .F. ) ;
#103462 = CARTESIAN_POINT ( 'NONE',  ( 6.563915523884999992, 1517.184063036290127, 210.2461356256870033 ) ) ;
#103463 = DIRECTION ( 'NONE',  ( -5.980589973904019347E-17, 1.000000000000000000, -1.736889445713099699E-16 ) ) ;
#103464 = CARTESIAN_POINT ( 'NONE',  ( 19.34249370211351504, 1456.699829906176774, 224.6011546362110778 ) ) ;
#103465 = CARTESIAN_POINT ( 'NONE',  ( 7.536552308397739708, 1425.565060507700082, 212.1829400242899624 ) ) ;
#103466 = EDGE_CURVE ( 'NONE', #19775, #23739, #70120, .T. ) ;
#103467 = CARTESIAN_POINT ( 'NONE',  ( -26.56033579598179983, 1451.985519570539964, 134.9300129401310073 ) ) ;
#103468 = EDGE_LOOP ( 'NONE', ( #29270, #96933, #58049, #90153 ) ) ;
#103469 = CARTESIAN_POINT ( 'NONE',  ( 4.500000000000000000, 1411.429641636930000, 126.8043280305979863 ) ) ;
#103471 = CARTESIAN_POINT ( 'NONE',  ( -15.19269324566649892, 1513.356256558869973, 223.4054110361780090 ) ) ;
#103470 = CARTESIAN_POINT ( 'NONE',  ( -2.311632204762886111, 1525.506926151471362, 176.4384886094890987 ) ) ;
#103472 = EDGE_CURVE ( 'NONE', #50075, #46649, #1618, .T. ) ;
#103473 = CARTESIAN_POINT ( 'NONE',  ( 11.60004869885204037, 1422.941107825514564, 135.6422303046223306 ) ) ;
#103474 = CARTESIAN_POINT ( 'NONE',  ( -19.09919624993290199, 1508.457687219779928, 210.0040316747289921 ) ) ;
#103475 = CARTESIAN_POINT ( 'NONE',  ( 0.004157115712379180240, 1455.132373369690185, 215.8075664961990014 ) ) ;
#103476 = EDGE_CURVE ( 'NONE', #51303, #57781, #36762, .T. ) ;
#103477 = CARTESIAN_POINT ( 'NONE',  ( -9.235583105570428941, 1440.105707546520080, 206.5655124634290303 ) ) ;
#103478 = VERTEX_POINT ( 'NONE', #37553 ) ;
#103479 = CARTESIAN_POINT ( 'NONE',  ( -4.868932048487660147, 1409.401550909529988, 270.3706725577400221 ) ) ;
#103480 = CARTESIAN_POINT ( 'NONE',  ( -2.879318455905000018, 1516.995911393979895, 208.3865093923290033 ) ) ;
#103481 = CARTESIAN_POINT ( 'NONE',  ( 6.407815220088149744, 1418.463448909649969, 232.9647645899679844 ) ) ;
#103482 = CARTESIAN_POINT ( 'NONE',  ( -6.520293482274176711, 1509.032998982614345, 216.3821516759590509 ) ) ;
#103484 = ORIENTED_EDGE ( 'NONE', *, *, #104226, .T. ) ;
#103483 = CARTESIAN_POINT ( 'NONE',  ( -8.484789816894487302, 1365.990492769855791, 207.6218459616988241 ) ) ;
#103485 = ORIENTED_EDGE ( 'NONE', *, *, #33693, .F. ) ;
#103486 = EDGE_CURVE ( 'NONE', #80080, #52184, #91029, .T. ) ;
#103487 = CARTESIAN_POINT ( 'NONE',  ( -23.81627866638899960, 1411.112638069600280, 210.1641640956580090 ) ) ;
#103488 = DIRECTION ( 'NONE',  ( -0.02616798426359480748, 0.9993150019884422530, -0.02616798426359490809 ) ) ;
#103489 = CARTESIAN_POINT ( 'NONE',  ( 3.650560473782963555, 1424.964407230763072, 184.9206000695610896 ) ) ;
#103490 = CARTESIAN_POINT ( 'NONE',  ( -5.339448499717754260, 1406.221036493157044, 266.9498660043132077 ) ) ;
#103491 = AXIS2_PLACEMENT_3D ( 'NONE', #71573, #89968, #96171 ) ;
#103492 = CIRCLE ( 'NONE', #73073, 0.9999999999999992228 ) ;
#103493 = ADVANCED_FACE ( 'NONE', ( #89047 ), #25152, .T. ) ;
#103494 = CARTESIAN_POINT ( 'NONE',  ( -18.06981095964670203, 1413.146983966680182, 195.1848155250099808 ) ) ;
#103495 = CARTESIAN_POINT ( 'NONE',  ( -17.79320747690000104, 1415.861465824730203, 225.5139460155979805 ) ) ;
#103496 = AXIS2_PLACEMENT_3D ( 'NONE', #108625, #90156, #6711 ) ;
#103497 = CARTESIAN_POINT ( 'NONE',  ( 36.97629126828699953, 1461.966573722429985, 266.9662940315810147 ) ) ;
#103498 = CARTESIAN_POINT ( 'NONE',  ( -1.832174820364002032, 1466.979387277607429, 235.3086100617430532 ) ) ;
#103499 = CARTESIAN_POINT ( 'NONE',  ( 19.59884465730813830, 1526.382868172863937, 181.1441328703420481 ) ) ;
#103500 = CARTESIAN_POINT ( 'NONE',  ( -7.724423432224999608, 1517.122088787240045, 205.6676733166769964 ) ) ;
#103501 = ORIENTED_EDGE ( 'NONE', *, *, #31031, .T. ) ;
#103502 = CARTESIAN_POINT ( 'NONE',  ( 21.74861278406057252, 1411.032916471346880, 216.6292070377826633 ) ) ;
#103503 = CARTESIAN_POINT ( 'NONE',  ( -3.956111812109641690, 1516.693880335214544, 202.7485082001233820 ) ) ;
#103504 = CARTESIAN_POINT ( 'NONE',  ( 22.83404369579999837, 1409.737016915530148, 208.6318390177190167 ) ) ;
#103505 = EDGE_LOOP ( 'NONE', ( #84488, #6553, #47361, #34198 ) ) ;
#103506 = CARTESIAN_POINT ( 'NONE',  ( 4.833436873729850092, 1508.551704408090018, 205.8972860377909910 ) ) ;
#103507 = CARTESIAN_POINT ( 'NONE',  ( 24.32398584962239951, 1452.063651768310137, 136.1369888671689807 ) ) ;
#103508 = CARTESIAN_POINT ( 'NONE',  ( -2.716551984532820097, 1508.551704408389924, 214.0984450385660125 ) ) ;
#103509 = CARTESIAN_POINT ( 'NONE',  ( -14.90483084879999964, 1391.000798919190174, 209.4215842360250122 ) ) ;
#103510 = DIRECTION ( 'NONE',  ( -0.06728379684272094152, -0.9969860201949397593, -0.03862338952348134263 ) ) ;
#103511 = CARTESIAN_POINT ( 'NONE',  ( 17.37907441389999974, 1410.017153215830149, 192.8320702375980318 ) ) ;
#103512 = CARTESIAN_POINT ( 'NONE',  ( 17.22592482065188335, 1443.913060387329779, 162.9227486220069352 ) ) ;
#103513 = DIRECTION ( 'NONE',  ( 1.000000000000000000, 0.000000000000000000, 0.000000000000000000 ) ) ;
#103515 = CARTESIAN_POINT ( 'NONE',  ( -21.37277430946751267, 1428.837918873476156, 219.6028782859573880 ) ) ;
#103514 = CARTESIAN_POINT ( 'NONE',  ( 30.15968401513964636, 1524.412455883367556, 195.8336456173444162 ) ) ;
#103516 = CARTESIAN_POINT ( 'NONE',  ( -16.57542919120515279, 1524.538768545233779, 180.6931493670368525 ) ) ;
#103517 = B_SPLINE_CURVE_WITH_KNOTS ( 'NONE', 5,
 ( #76460, #32795, #15979, #101090, #59676, #93788, #8689, #17063, #85393, #7053, #75381, #32068, #83025, #40464, #5780, #74091, #15246, #39922 ),
 .UNSPECIFIED., .F., .F.,
 ( 6, 3, 3, 3, 3, 6 ),
 ( -66.06417000470000289, -61.46700666819999981, -43.61786061130000292, -17.15566543539999600, 15.57237739079999983, 26.25296013780000237 ),
 .UNSPECIFIED. ) ;
#103518 = DIRECTION ( 'NONE',  ( -1.000000000000000000, 0.000000000000000000, 0.000000000000000000 ) ) ;
#103519 = COLOUR_RGB ( '', 0.40784314, 0.44705882, 0.49803922) ;
#103520 = CARTESIAN_POINT ( 'NONE',  ( 5.277460848200000498, 1426.742654866309977, 191.8370381630989812 ) ) ;
#103521 = CARTESIAN_POINT ( 'NONE',  ( -4.031142389804999837, 1516.929569650079884, 214.1322689334670031 ) ) ;
#103522 = CARTESIAN_POINT ( 'NONE',  ( 17.11714618750000128, 1444.740067931809790, 162.7561046190980107 ) ) ;
#103523 = ORIENTED_EDGE ( 'NONE', *, *, #10464, .F. ) ;
#103524 = DIRECTION ( 'NONE',  ( 0.000000000000000000, 0.000000000000000000, 1.000000000000000000 ) ) ;
#103525 = DIRECTION ( 'NONE',  ( -0.9455185755993178454, 0.000000000000000000, 0.3255681544571537578 ) ) ;
#103526 = CARTESIAN_POINT ( 'NONE',  ( -16.68599179819999989, 1461.099982565929849, 230.2790296985980092 ) ) ;
#103527 = ADVANCED_FACE ( 'NONE', ( #97457 ), #51723, .T. ) ;
#103528 = CARTESIAN_POINT ( 'NONE',  ( -9857.840209715130186, 50.13405481578730161, -1086.115145476999942 ) ) ;
#103529 = ADVANCED_FACE ( 'NONE', ( #50379 ), #772, .F. ) ;
#103530 = B_SPLINE_CURVE_WITH_KNOTS ( 'NONE', 3,
 ( #93723, #103231, #17001, #25970, #59066, #33837, #86453, #60168, #68027, #35501, #69693, #17564, #26541, #60736, #18132, #9744, #61297, #51765, #95416, #52877, #87004, #10294, #16457, #8627, #44470, #51200, #42802, #70253, #27657, #55639, #11421, #45590, #104360, #45038, #54001, #80274, #36607, #106566, #71914, #64039 ),
 .UNSPECIFIED., .F., .F.,
 ( 4, 3, 3, 3, 3, 3, 3, 3, 3, 3, 3, 3, 3, 4 ),
 ( -7.724159284985280038, -7.528912261385430682, -7.285801190272390038, -7.022071646754660001, -6.736975261711270591, -6.407913920619930259, -6.017318246991619546, -5.710627735595419807, -5.447746533992479989, -5.114105914177909717, -4.732608650904720271, -4.279348212383050409, -3.608572623993069328, -3.171332707879999546 ),
 .UNSPECIFIED. ) ;
#103531 = PLANE ( 'NONE',  #51196 ) ;
#103532 = CARTESIAN_POINT ( 'NONE',  ( -4.327610416712750485, 1515.134996992939932, 208.4730697464140121 ) ) ;
#103533 = B_SPLINE_CURVE_WITH_KNOTS ( 'NONE', 3,
 ( #99763, #49389, #8869, #91387, #99208, #74595, #108732, #65096, #22487, #75149, #94530, #56687, #83516, #82978, #17804, #66757, #40969, #25666, #23052, #93983, #107633, #48295, #90824, #82438, #57260, #14105, #14665, #17249, #81867, #23616, #51442, #5735, #73500, #74045, #39878, #48854, #108174 ),
 .UNSPECIFIED., .F., .F.,
 ( 4, 3, 3, 3, 3, 3, 3, 3, 3, 3, 3, 3, 4 ),
 ( -69.20990094339998677, -67.35627552521479799, -65.67677515525750209, -64.13305301190000307, -63.72413547986320026, -62.52805632474360209, -61.28625140089109635, -60.00527021219100021, -58.62934261228799926, -57.23376785416390078, -55.62731357942359978, -53.66775153965929945, -51.68681987860000504 ),
 .UNSPECIFIED. ) ;
#103534 = CARTESIAN_POINT ( 'NONE',  ( -14.97660074559999899, 1451.660971642529830, 219.6133832206979832 ) ) ;
#103535 = CARTESIAN_POINT ( 'NONE',  ( -2.156670372940499902, 1451.947498740930087, 184.5271336820339911 ) ) ;
#103536 = CARTESIAN_POINT ( 'NONE',  ( 11.20455999689999871, 1433.617589470330131, 151.5998260058979952 ) ) ;
#103537 = CARTESIAN_POINT ( 'NONE',  ( 3.108624468949999707E-15, 1461.407663422529822, 243.9198229339980060 ) ) ;
#103538 = CARTESIAN_POINT ( 'NONE',  ( -10.57409850134300022, 1462.298722268380061, 208.7176379312979861 ) ) ;
#103539 = CARTESIAN_POINT ( 'NONE',  ( -14.46118808569999814, 1422.533245244620048, 196.3519510282989984 ) ) ;
#103540 = B_SPLINE_CURVE_WITH_KNOTS ( 'NONE', 5,
 ( #68791, #33480, #102891, #17215, #58716, #101228, #23974, #101790, #67128 ),
 .UNSPECIFIED., .F., .F.,
 ( 6, 3, 6 ),
 ( 0.000000000000000000, 0.3910644012100996103, 1.000000000000000000 ),
 .UNSPECIFIED. ) ;
#103541 = CARTESIAN_POINT ( 'NONE',  ( 11.73977902011290020, 1420.726571890000287, 199.9640281710840100 ) ) ;
#103542 = DIRECTION ( 'NONE',  ( 1.439455173507210273E-14, 1.000000000000000000, 2.465190328815660140E-31 ) ) ;
#103543 = EDGE_CURVE ( 'NONE', #99156, #96293, #66637, .T. ) ;
#103544 = CARTESIAN_POINT ( 'NONE',  ( -4.696284960629999894, 1486.251895520230164, 182.0546551604979868 ) ) ;
#103545 = CARTESIAN_POINT ( 'NONE',  ( -13.98457847890000139, 1414.635582449330059, 227.2382995055980075 ) ) ;
#103546 = CARTESIAN_POINT ( 'NONE',  ( -30.15184734697509938, 1510.043527037290005, 208.7857410632290112 ) ) ;
#103547 = AXIS2_PLACEMENT_3D ( 'NONE', #12067, #46257, #37830 ) ;
#103548 = CARTESIAN_POINT ( 'NONE',  ( 25.61862525230000287, 1449.804154363369889, 210.1382241221579932 ) ) ;
#103549 = DIRECTION ( 'NONE',  ( -0.9995237709234254808, 0.03085824620771311644, -1.986951185180850780E-13 ) ) ;
#103550 = CARTESIAN_POINT ( 'NONE',  ( 25.71670629617132064, 1436.648920519811327, 137.1099281659991220 ) ) ;
#103551 = CARTESIAN_POINT ( 'NONE',  ( -1.842963640640000067, 1515.372048646890107, 204.8601094037989867 ) ) ;
#103552 = CARTESIAN_POINT ( 'NONE',  ( 13.84583159390490081, 1499.900107518399864, 227.7510596827030156 ) ) ;
#103553 = CARTESIAN_POINT ( 'NONE',  ( -0.7360974767499980365, 1517.045004075700035, 213.1642344714070134 ) ) ;
#103554 = CARTESIAN_POINT ( 'NONE',  ( -18.18415092269999889, 1419.305676067660215, 210.3674448266889954 ) ) ;
#103555 = CARTESIAN_POINT ( 'NONE',  ( 0.1620797138729939690, 1485.018021426579935, 181.8788060555280026 ) ) ;
#103557 = ORIENTED_EDGE ( 'NONE', *, *, #48711, .T. ) ;
#103556 = CARTESIAN_POINT ( 'NONE',  ( -18.18137268718939836, 1507.546750198529935, 231.7129778879169635 ) ) ;
#103558 = CARTESIAN_POINT ( 'NONE',  ( -1.546867746950000067, 1416.839692131129823, 228.0214409762979813 ) ) ;
#103559 = VECTOR ( 'NONE', #57633, 1000.000000000000000 ) ;
#103560 = EDGE_CURVE ( 'NONE', #88662, #23187, #64208, .T. ) ;
#103561 = CARTESIAN_POINT ( 'NONE',  ( -10.24092311318542059, 1389.890054110666142, 202.1840738160088620 ) ) ;
#103562 = CARTESIAN_POINT ( 'NONE',  ( -3.008615722576569951, 1440.893621901990173, 157.1951554466570258 ) ) ;
#103564 = ORIENTED_EDGE ( 'NONE', *, *, #35346, .T. ) ;
#103563 = CARTESIAN_POINT ( 'NONE',  ( -32.22536377336270164, 1523.621879633028811, 216.8351145222434013 ) ) ;
#103565 = CARTESIAN_POINT ( 'NONE',  ( -6.670684733933529564, 1508.551704408180058, 219.2717039139770066 ) ) ;
#103566 = ORIENTED_EDGE ( 'NONE', *, *, #64461, .T. ) ;
#103567 = B_SPLINE_SURFACE_WITH_KNOTS ( 'NONE', 5, 3, ( 
 ( #106387, #80639, #108027, #4490 ),
 ( #30214, #3953, #81174, #72799 ),
 ( #3401, #106926, #73901, #64405 ),
 ( #39735, #98528, #21795, #31324 ),
 ( #88491, #105850, #90119, #81714 ),
 ( #73342, #107476, #48149, #54361 ),
 ( #82287, #11775, #65507, #86007 ),
 ( #17669, #51871, #32971, #66619 ),
 ( #66065, #22901, #82829, #9307 ),
 ( #32442, #92327, #74462, #103340 ),
 ( #35050, #24003, #31877, #57666 ),
 ( #60841, #58199, #7236, #78156 ),
 ( #99616, #67160, #49803, #75561 ),
 ( #57109, #41396, #1466, #108590 ),
 ( #6121, #109158, #100721, #91236 ),
 ( #60270, #101258, #14515, #48705 ),
 ( #6677, #40277, #43470, #94389 ),
 ( #77615, #26079, #15598, #91778 ),
 ( #100189, #23473, #927, #15056 ),
 ( #83935, #49255, #26643, #69231 ),
 ( #109696, #83376, #40831, #94966 ),
 ( #75008, #18235, #52430, #86556 ),
 ( #9852, #44020, #36715, #97719 ),
 ( #63067, #44573, #105023, #19337 ),
 ( #27212, #61393, #80926, #70907 ),
 ( #10403, #88778, #80379, #28316 ),
 ( #95514, #10966, #61949, #20440 ),
 ( #78718, #104463, #3695, #62507 ),
 ( #87113, #37823, #106126, #54649 ),
 ( #96628, #2034, #37274, #72009 ) ),
 .UNSPECIFIED., .F., .F., .F.,
 ( 6, 3, 3, 3, 3, 3, 3, 3, 3, 6 ),
 ( 4, 4 ),
 ( 0.000000000000000000, 15.39383910899999997, 27.58084801740000103, 41.39509552349999666, 65.53909258059999843, 90.91108773649999364, 117.6367619669999982, 132.4493970709999928, 144.8160795070000120, 161.8240513320000105 ),
 ( 33.63253214979999939, 34.48604544350000367 ),
 .UNSPECIFIED. ) ;
#103568 = FACE_OUTER_BOUND ( 'NONE', #16967, .T. ) ;
#103569 = CARTESIAN_POINT ( 'NONE',  ( -12.84953875605850016, 1390.894593418380055, 209.7715853971660067 ) ) ;
#103570 = CARTESIAN_POINT ( 'NONE',  ( -14.11509852220000028, 1414.913060387329779, 218.5043773088879959 ) ) ;
#103571 = CARTESIAN_POINT ( 'NONE',  ( -2.739840682029376584, 1509.032634909519629, 238.5893384668526096 ) ) ;
#103572 = ADVANCED_FACE ( 'NONE', ( #7795 ), #74897, .T. ) ;
#103573 = CARTESIAN_POINT ( 'NONE',  ( 9.093901123017769095, 1470.494570018200193, 191.1297851741429952 ) ) ;
#103574 = CARTESIAN_POINT ( 'NONE',  ( -2.608414268140000214, 1431.710115199490019, 217.1231005886490095 ) ) ;
#103575 = CARTESIAN_POINT ( 'NONE',  ( -16.25511663789999872, 1421.255025725300129, 210.0327608240260133 ) ) ;
#103576 = CARTESIAN_POINT ( 'NONE',  ( 13.80599399769999991, 1434.979619872729927, 146.4346935412979747 ) ) ;
#103577 = LINE ( 'NONE', #26879, #66939 ) ;
#103578 = CARTESIAN_POINT ( 'NONE',  ( -82.48023544352470537, 1385.167086914460015, 286.1466225573760198 ) ) ;
#103579 = CARTESIAN_POINT ( 'NONE',  ( -17.03916695150000038, 1411.910831074529824, 191.9225384856980270 ) ) ;
#103580 = CARTESIAN_POINT ( 'NONE',  ( -56.64534719470000113, 1379.747652096109960, 254.3393773118589536 ) ) ;
#103581 = ORIENTED_EDGE ( 'NONE', *, *, #17484, .T. ) ;
#103582 = AXIS2_PLACEMENT_3D ( 'NONE', #61142, #70092, #86849 ) ;
#103583 = CARTESIAN_POINT ( 'NONE',  ( -15.73147536331710050, 1409.565876699960199, 225.8795040344060112 ) ) ;
#103585 = VERTEX_POINT ( 'NONE', #51461 ) ;
#103584 = CARTESIAN_POINT ( 'NONE',  ( -7.848979634317430509, 1517.051704408389924, 202.2988320601959913 ) ) ;
#103586 = CARTESIAN_POINT ( 'NONE',  ( 7.653407898138279819, 1466.072686860559998, 215.4064835335099986 ) ) ;
#103587 = CIRCLE ( 'NONE', #21078, 1.000000000000000888 ) ;
#103588 = ORIENTED_EDGE ( 'NONE', *, *, #13773, .F. ) ;
#103589 = ADVANCED_FACE ( 'NONE', ( #105181 ), #104622, .F. ) ;
#103590 = CARTESIAN_POINT ( 'NONE',  ( 25.58984387490000145, 1507.958107147929923, 218.7218739854080241 ) ) ;
#103591 = CARTESIAN_POINT ( 'NONE',  ( -6.341401618134332452, 1363.580025761456227, 209.6218459617148824 ) ) ;
#103592 = CARTESIAN_POINT ( 'NONE',  ( -9.624884241989999367, 1493.132688955090089, 201.2649490877390122 ) ) ;
#103593 = EDGE_CURVE ( 'NONE', #62909, #42879, #90084, .T. ) ;
#103594 = CARTESIAN_POINT ( 'NONE',  ( 18.44501327497894749, 1468.322017823991700, 269.3810620050319926 ) ) ;
#103595 = DIRECTION ( 'NONE',  ( 0.5224574779878928821, 0.7067418228236548305, -0.4770263929453257834 ) ) ;
#103596 = CARTESIAN_POINT ( 'NONE',  ( 15.23211778679590545, 1430.904153654725633, 219.7804539585919770 ) ) ;
#103597 = CARTESIAN_POINT ( 'NONE',  ( 2.124286289930000127, 1417.654161064629989, 233.3475255464980194 ) ) ;
#103598 = CARTESIAN_POINT ( 'NONE',  ( -6.477828314561669742, 1516.676423271974500, 212.9199659827493463 ) ) ;
#103599 = CARTESIAN_POINT ( 'NONE',  ( -9.496501384368448484, 1440.505055584230377, 186.7254819606929175 ) ) ;
#103600 = CARTESIAN_POINT ( 'NONE',  ( -5.236338392940000475, 1368.774323667059889, 207.6218459616989946 ) ) ;
#103601 = DIRECTION ( 'NONE',  ( 1.000000000000000000, 0.000000000000000000, 0.000000000000000000 ) ) ;
#103602 = CARTESIAN_POINT ( 'NONE',  ( 0.8541212061450009774, 1457.065338652990249, 199.5100658954889923 ) ) ;
#103603 = EDGE_CURVE ( 'NONE', #3002, #19377, #98237, .T. ) ;
#103604 = CARTESIAN_POINT ( 'NONE',  ( 6.933879402874999265, 1516.560253536979872, 206.6353711893569880 ) ) ;
#103605 = CARTESIAN_POINT ( 'NONE',  ( -13.04141444983799936, 1435.645536544770039, 150.5902749682459785 ) ) ;
#103606 = B_SPLINE_SURFACE_WITH_KNOTS ( 'NONE', 5, 5, ( 
 ( #106766, #65350, #30057, #5417, #64248, #56386 ),
 ( #98370, #21643, #14351, #90518, #91068, #108430 ),
 ( #14902, #55848, #13244, #47434, #22736, #97814 ),
 ( #13793, #82117, #39577, #56939, #48543, #82681 ),
 ( #23306, #49093, #5971, #83228, #6518, #40671 ),
 ( #29512, #63704, #18072, #66457, #69072, #61239 ),
 ( #7071, #66996, #49640, #69629, #101107, #26475 ),
 ( #103751, #103172, #41228, #27053, #95353, #18613 ),
 ( #43304, #27592, #23849, #85842, #78553, #15449 ),
 ( #104302, #100568, #58041, #9141, #92178, #10235 ),
 ( #60111, #109537, #83777, #86391, #86944, #52267 ),
 ( #60670, #52813, #87514, #61777, #25913, #95901 ) ),
 .UNSPECIFIED., .F., .F., .F.,
 ( 6, 3, 3, 6 ),
 ( 6, 6 ),
 ( 18.22821421442209910, 21.75967651710000084, 24.82024664080000065, 32.41288959079599863 ),
 ( -8.204439600732860269E-05, 1.512517455850000081 ),
 .UNSPECIFIED. ) ;
#103607 = CARTESIAN_POINT ( 'NONE',  ( -2.500000000000000000, 1437.833057476529802, 157.6748628238979961 ) ) ;
#103608 = CARTESIAN_POINT ( 'NONE',  ( -7.127716695479999294E-11, 1475.057956560229968, 269.6447263235979790 ) ) ;
#103610 = ORIENTED_EDGE ( 'NONE', *, *, #108576, .F. ) ;
#103609 = CARTESIAN_POINT ( 'NONE',  ( -2.897049938759999943, 1495.303674484390058, 219.9350255916990022 ) ) ;
#103611 = EDGE_CURVE ( 'NONE', #65361, #6784, #61542, .T. ) ;
#103612 = DIRECTION ( 'NONE',  ( -0.7071067811865490160, 0.000000000000000000, 0.7071067811865461294 ) ) ;
#103613 = ORIENTED_EDGE ( 'NONE', *, *, #23746, .T. ) ;
#103614 = CARTESIAN_POINT ( 'NONE',  ( 41.56052307180000582, 1438.341700298520209, 261.5689801973979911 ) ) ;
#103615 = CARTESIAN_POINT ( 'NONE',  ( -23.79684662080000024, 1410.916736090329778, 207.4665339750179953 ) ) ;
#103617 = CARTESIAN_POINT ( 'NONE',  ( 16.81493322035340299, 1409.874137557720132, 192.4133040450060150 ) ) ;
#103616 = CARTESIAN_POINT ( 'NONE',  ( -11.34549315327149976, 1426.458520874449960, 115.9708627263430003 ) ) ;
#103618 = CARTESIAN_POINT ( 'NONE',  ( 6.950214933285000285, 1517.129577905929864, 211.9934263588270085 ) ) ;
#103619 = CARTESIAN_POINT ( 'NONE',  ( 7.683404440216066611, 1509.309260261254394, 180.0625472504430888 ) ) ;
#103620 = DIRECTION ( 'NONE',  ( -0.000000000000000000, -0.000000000000000000, 1.000000000000000000 ) ) ;
#103621 = CIRCLE ( 'NONE', #32088, 2.000007659174134922 ) ;
#103622 = CARTESIAN_POINT ( 'NONE',  ( -28.68961640089999676, 1414.662827630530046, 264.4914002609979775 ) ) ;
#103623 = CARTESIAN_POINT ( 'NONE',  ( -14.15592233437959990, 1379.713028150099944, 208.2740576972960014 ) ) ;
#103624 = CARTESIAN_POINT ( 'NONE',  ( 17.48489369962524620, 1459.987562467892076, 228.4085929379347135 ) ) ;
#103625 = CARTESIAN_POINT ( 'NONE',  ( -5.024579074340000062, 1391.800828779589892, 214.6319658655289970 ) ) ;
#103626 = CARTESIAN_POINT ( 'NONE',  ( -38.33296738232420608, 1438.937668912289837, 136.6331331180969926 ) ) ;
#103627 = ORIENTED_EDGE ( 'NONE', *, *, #38350, .F. ) ;
#103628 = CARTESIAN_POINT ( 'NONE',  ( 7.629428199119460352, 1397.829558206759884, 197.4986098258069944 ) ) ;
#103629 = CARTESIAN_POINT ( 'NONE',  ( 10.14559180641809988, 1460.375376629410084, 206.4970471914819825 ) ) ;
#103630 = EDGE_CURVE ( 'NONE', #19958, #47285, #19278, .T. ) ;
#103631 = CARTESIAN_POINT ( 'NONE',  ( -16.87366308760000067, 1458.693985979230092, 229.6006262403980145 ) ) ;
#103632 = EDGE_LOOP ( 'NONE', ( #107474, #45054 ) ) ;
#103633 = ORIENTED_EDGE ( 'NONE', *, *, #58768, .T. ) ;
#103634 = CARTESIAN_POINT ( 'NONE',  ( -14.47420009890000081, 1416.181292664740113, 214.4142689833190047 ) ) ;
#103635 = CARTESIAN_POINT ( 'NONE',  ( 9.228474993260000758, 1423.651513103620118, 196.7592343168990112 ) ) ;
#103636 = ORIENTED_EDGE ( 'NONE', *, *, #104861, .T. ) ;
#103637 = CARTESIAN_POINT ( 'NONE',  ( 0.3635313643190000166, 1421.820591800929833, 227.3960884296979827 ) ) ;
#103638 = CARTESIAN_POINT ( 'NONE',  ( -13.98359605274442785, 1416.534589811554270, 202.6245575613080803 ) ) ;
#103639 = ADVANCED_FACE ( 'NONE', ( #62101 ), #69662, .F. ) ;
#103640 = CARTESIAN_POINT ( 'NONE',  ( -2.664535259099999805E-15, 1424.786834349990158, 209.1218459616989946 ) ) ;
#103641 = CARTESIAN_POINT ( 'NONE',  ( 26.92366755636065889, 1508.479994616119484, 206.2224058939788733 ) ) ;
#103642 = CARTESIAN_POINT ( 'NONE',  ( 17.79018706778330028, 1578.884106212270126, 161.8975890202569872 ) ) ;
#103643 = CARTESIAN_POINT ( 'NONE',  ( 9.549813427814630273, 1451.221866577720220, 207.5450308176739895 ) ) ;
#103644 = PLANE ( 'NONE',  #75398 ) ;
#103645 = CARTESIAN_POINT ( 'NONE',  ( -97.83172781913290805, 1384.867102923100219, 295.7948235560999706 ) ) ;
#103646 = ORIENTED_EDGE ( 'NONE', *, *, #19379, .F. ) ;
#103647 = CARTESIAN_POINT ( 'NONE',  ( 5.002593359325000044, 1516.960844870249957, 202.5626772953570196 ) ) ;
#103648 = CARTESIAN_POINT ( 'NONE',  ( 7.337297311985000015, 1517.135701590510052, 209.8615382079770200 ) ) ;
#103649 = ORIENTED_EDGE ( 'NONE', *, *, #11781, .T. ) ;
#103650 = CARTESIAN_POINT ( 'NONE',  ( 11.86538456922300000, 1432.285977292769985, 149.9821679606649809 ) ) ;
#103651 = VECTOR ( 'NONE', #15008, 1000.000000000000000 ) ;
#103652 = CARTESIAN_POINT ( 'NONE',  ( -21.38516915558007270, 1512.187213306747481, 180.3939891059723664 ) ) ;
#103653 = ORIENTED_EDGE ( 'NONE', *, *, #108224, .T. ) ;
#103654 = CARTESIAN_POINT ( 'NONE',  ( 4.115863297784077446, 1509.032014613820820, 213.4860455958220768 ) ) ;
#103655 = CARTESIAN_POINT ( 'NONE',  ( -17.22654844235838567, 1443.913060387328869, 162.9224179604370590 ) ) ;
#103656 = CARTESIAN_POINT ( 'NONE',  ( -2.813821217502529670, 1367.641464860501173, 208.8602496609475168 ) ) ;
#103657 = CARTESIAN_POINT ( 'NONE',  ( -4.853079720760000271, 1422.238069890129964, 185.0630658123980083 ) ) ;
#103658 = CIRCLE ( 'NONE', #105433, 0.9999999999999015232 ) ;
#103659 = CARTESIAN_POINT ( 'NONE',  ( 2.255304544822630319, 1409.820689363890097, 270.0715902656349954 ) ) ;
#103660 = CARTESIAN_POINT ( 'NONE',  ( 1.959285284397550120, 1474.800623515119923, 220.3715842348549927 ) ) ;
#103661 = CARTESIAN_POINT ( 'NONE',  ( 0.5890887500919903541, 1526.382868172863937, 174.9674887555077021 ) ) ;
#103662 = CARTESIAN_POINT ( 'NONE',  ( 11.86100295819999850, 1492.894947675889853, 212.5846962613990172 ) ) ;
#103663 = CARTESIAN_POINT ( 'NONE',  ( -18.81083778160000008, 1379.661349286479890, 209.0395301435680153 ) ) ;
#103664 = CARTESIAN_POINT ( 'NONE',  ( 8.943454933915715444, 1425.008260442055644, 195.6459240983384973 ) ) ;
#103666 = CARTESIAN_POINT ( 'NONE',  ( 11.08318464053740016, 1470.184830858459918, 206.6635668760160058 ) ) ;
#103665 = CARTESIAN_POINT ( 'NONE',  ( -21.20078141540000161, 1505.634983266090103, 209.1959435100580151 ) ) ;
#103667 = CARTESIAN_POINT ( 'NONE',  ( 15.57416844496259856, 1507.336002650009959, 225.6913864299219767 ) ) ;
#103668 = CARTESIAN_POINT ( 'NONE',  ( 17.69747404500670029, 1413.849660306819715, 224.8943591048869735 ) ) ;
#103669 = CARTESIAN_POINT ( 'NONE',  ( -6.160280215534999826, 1511.773927532309926, 200.4817730439669958 ) ) ;
#103670 = VERTEX_POINT ( 'NONE', #64854 ) ;
#103671 = AXIS2_PLACEMENT_3D ( 'NONE', #44488, #78633, #36086 ) ;
#103672 = CARTESIAN_POINT ( 'NONE',  ( 18.02574679518840028, 1424.482682570480165, 224.6196048480980210 ) ) ;
#103673 = CARTESIAN_POINT ( 'NONE',  ( 41.39118081080529521, 1446.191675961305009, 135.3420714969400649 ) ) ;
#103674 = CARTESIAN_POINT ( 'NONE',  ( -3.054816033052110136, 1485.996906143959905, 182.1538611115439892 ) ) ;
#103675 =( BOUNDED_CURVE ( )  B_SPLINE_CURVE ( 3, ( #85777, #77393, #21162, #96815 ),
 .UNSPECIFIED., .F., .F. ) 
 B_SPLINE_CURVE_WITH_KNOTS ( ( 4, 4 ),
 ( 3.141592653589793116, 4.712388980384689674 ),
 .UNSPECIFIED. ) 
 CURVE ( )  GEOMETRIC_REPRESENTATION_ITEM ( )  RATIONAL_B_SPLINE_CURVE ( ( 1.000000000000000000, 0.8047378541243649375, 0.8047378541243649375, 1.000000000000000000 ) ) 
 REPRESENTATION_ITEM ( '' )  );
#103676 = CARTESIAN_POINT ( 'NONE',  ( -14.10889964140000075, 1415.677402202029953, 213.9573798837890308 ) ) ;
#103678 = EDGE_LOOP ( 'NONE', ( #96729, #28501 ) ) ;
#103677 = CARTESIAN_POINT ( 'NONE',  ( 1.059358656784129993, 1515.104045403560121, 204.7934250490989996 ) ) ;
#103679 = CARTESIAN_POINT ( 'NONE',  ( -15.87663024991563532, 1415.942772094044130, 209.7336067992691824 ) ) ;
#103680 = CARTESIAN_POINT ( 'NONE',  ( 20.21057157959999984, 1475.708668719390062, 208.1550663298600057 ) ) ;
#103681 = CARTESIAN_POINT ( 'NONE',  ( -2.339614227286648696, 1449.682732101595775, 154.4221585652428246 ) ) ;
#103682 = CARTESIAN_POINT ( 'NONE',  ( -10.92547548560405168, 1429.189822794765632, 151.1096517011108062 ) ) ;
#103683 = CARTESIAN_POINT ( 'NONE',  ( 3.375977085881459949, 1446.395221913229989, 199.5681764770490076 ) ) ;
#103684 = FACE_OUTER_BOUND ( 'NONE', #106165, .T. ) ;
#103685 = CARTESIAN_POINT ( 'NONE',  ( -1.771001175045461062, 1526.211523310372513, 240.5584728653311970 ) ) ;
#103686 = CARTESIAN_POINT ( 'NONE',  ( -15.38132089836499894, 1512.167884426309911, 221.9700943965670206 ) ) ;
#103687 = CARTESIAN_POINT ( 'NONE',  ( 11.68080434900000064, 1412.737827518229778, 229.2464092685980290 ) ) ;
#103688 = CARTESIAN_POINT ( 'NONE',  ( -8.070165105480000989, 1477.963585978789752, 216.1585797569989893 ) ) ;
#103689 = CARTESIAN_POINT ( 'NONE',  ( -15.99364927919999779, 1459.641266709229967, 228.9570266767980229 ) ) ;
#103690 = CIRCLE ( 'NONE', #82178, 14.91144628110000170 ) ;
#103691 = CARTESIAN_POINT ( 'NONE',  ( 6.546039395294999785, 1516.565291103010168, 206.8289057630870218 ) ) ;
#103692 = CARTESIAN_POINT ( 'NONE',  ( 18.10151846899999839, 1409.478927776330011, 269.5454010446980533 ) ) ;
#103693 = CARTESIAN_POINT ( 'NONE',  ( 23.06010171139999798, 1435.302639552910023, 139.4254245235980250 ) ) ;
#103694 = CARTESIAN_POINT ( 'NONE',  ( 23.77245939000000163, 1449.721689247069889, 203.1279807519480016 ) ) ;
#103695 = CARTESIAN_POINT ( 'NONE',  ( -22.72361341210000063, 1432.255922540859956, 217.6431687005280082 ) ) ;
#103696 = LINE ( 'NONE', #70139, #89262 ) ;
#103697 = CARTESIAN_POINT ( 'NONE',  ( -11.42922335629970121, 1500.819224854980121, 209.0445494102119994 ) ) ;
#103698 = CARTESIAN_POINT ( 'NONE',  ( -1.632217591109999866, 1452.043058095030119, 184.0584959782980263 ) ) ;
#103699 = CARTESIAN_POINT ( 'NONE',  ( -6.224176945601150202, 1407.473636839899882, 197.7087082607250181 ) ) ;
#103700 = CARTESIAN_POINT ( 'NONE',  ( -16.80685858420000045, 1416.624127770589894, 209.3044896098560059 ) ) ;
#103701 = VECTOR ( 'NONE', #55727, 1000.000000000000000 ) ;
#103702 = CARTESIAN_POINT ( 'NONE',  ( -13.73335268700000000, 1441.669543367469942, 188.5645195036979942 ) ) ;
#103703 = CARTESIAN_POINT ( 'NONE',  ( 18.89942246145942306, 1416.835807492850108, 210.6687153380977122 ) ) ;
#103704 = CARTESIAN_POINT ( 'NONE',  ( -30.19569990680000160, 1436.880670734120258, 136.6769221344979712 ) ) ;
#103705 = DIRECTION ( 'NONE',  ( -0.4229618813980365877, 0.9061474752402244315, -4.354426617128452806E-10 ) ) ;
#103706 = VERTEX_POINT ( 'NONE', #106276 ) ;
#103707 = CARTESIAN_POINT ( 'NONE',  ( -8.751535168777641260, 1384.847616307870112, 220.6818258576190033 ) ) ;
#103708 = CARTESIAN_POINT ( 'NONE',  ( -14.61215934965860086, 1409.423328235749977, 212.1943553262919977 ) ) ;
#103709 = B_SPLINE_SURFACE_WITH_KNOTS ( 'NONE', 2, 5, ( 
 ( #79170, #9189, #18119, #27642, #86438, #51751 ),
 ( #25957, #78600, #96505, #34384, #36595, #95401 ),
 ( #61828, #53413, #103801, #27100, #103216, #52863 ) ),
 .UNSPECIFIED., .F., .F., .F.,
 ( 3, 3 ),
 ( 6, 6 ),
 ( 1.399803019409999960, 2.016961153150000019 ),
 ( 0.000000000000000000, 1.000000000000000000 ),
 .UNSPECIFIED. ) ;
#103710 = CYLINDRICAL_SURFACE ( 'NONE', #64526, 2.000000000000001776 ) ;
#103711 = CARTESIAN_POINT ( 'NONE',  ( 20.55201027734738872, 1526.382868172863937, 236.4070436938629030 ) ) ;
#103712 = CARTESIAN_POINT ( 'NONE',  ( -21.73253653299999755, 1471.283060775529975, 269.3316831886979799 ) ) ;
#103713 = CARTESIAN_POINT ( 'NONE',  ( 29.52630218505380810, 1525.661276915132476, 196.5237718006094099 ) ) ;
#103714 = CARTESIAN_POINT ( 'NONE',  ( 0.2302574898499950007, 1419.640707946279917, 184.3378087949079998 ) ) ;
#103715 = CARTESIAN_POINT ( 'NONE',  ( -24.16750533216984564, 1444.510136686808892, 211.5893432462075339 ) ) ;
#103716 = CARTESIAN_POINT ( 'NONE',  ( -71.28397327874120037, 1384.659025300439907, 296.4637328428320302 ) ) ;
#103717 = CARTESIAN_POINT ( 'NONE',  ( -24.68077630836099701, 1437.736159206269804, 210.5119845322900005 ) ) ;
#103718 = CARTESIAN_POINT ( 'NONE',  ( 18.71502584834279759, 1425.461731811239815, 226.6158928661320147 ) ) ;
#103719 = CARTESIAN_POINT ( 'NONE',  ( 21.92460402160000044, 1509.678684430729845, 227.7046112463980023 ) ) ;
#103720 = CARTESIAN_POINT ( 'NONE',  ( 1.665334536940000025E-15, 1434.541756592460160, 155.4759165859979930 ) ) ;
#103721 = B_SPLINE_CURVE_WITH_KNOTS ( 'NONE', 3,
 ( #16856, #109316, #25268, #24168 ),
 .UNSPECIFIED., .F., .F.,
 ( 4, 4 ),
 ( 7.189030196343478827E-14, 0.002384643111680485698 ),
 .UNSPECIFIED. ) ;
#103722 = CARTESIAN_POINT ( 'NONE',  ( -10.94209231895430179, 1492.979988125699947, 207.3926202358989883 ) ) ;
#103723 = CARTESIAN_POINT ( 'NONE',  ( 4.015743051850000356, 1515.588776726489868, 208.3686727890390102 ) ) ;
#103724 = CARTESIAN_POINT ( 'NONE',  ( -9.094692777799998851, 1384.940603055749989, 199.9428207063789955 ) ) ;
#103725 = CARTESIAN_POINT ( 'NONE',  ( -22.30007645030000063, 1409.691796216729927, 207.3274002725380285 ) ) ;
#103726 = CARTESIAN_POINT ( 'NONE',  ( 14.38361772900000091, 1416.219761279530076, 196.8926598285980276 ) ) ;
#103727 = EDGE_CURVE ( 'NONE', #64952, #77609, #29562, .T. ) ;
#103728 = CARTESIAN_POINT ( 'NONE',  ( 4.875860680149999737, 1485.457236370389865, 218.7044629644089753 ) ) ;
#103729 = AXIS2_PLACEMENT_3D ( 'NONE', #41112, #51176, #15341 ) ;
#103730 = CARTESIAN_POINT ( 'NONE',  ( 10.92993424403990055, 1479.841764369919929, 208.5741803220239774 ) ) ;
#103731 = EDGE_CURVE ( 'NONE', #13291, #69131, #73230, .T. ) ;
#103732 = B_SPLINE_SURFACE_WITH_KNOTS ( 'NONE', 5, 5, ( 
 ( #29138, #30225, #63866, #63327, #19625, #97982, #21248, #36981, #89588 ),
 ( #39177, #28032, #64414, #98536, #13411, #47599, #81725, #87966, #5033 ),
 ( #62222, #11256, #108599, #83388, #16167, #67168, #31887, #7786, #41952 ),
 ( #64962, #50370, #90684, #6130, #40843, #22354, #23482, #92336, #107487 ),
 ( #22911, #92893, #7244, #15608, #99075, #49814, #31330, #32979, #40286 ),
 ( #100198, #84496, #56556, #6686, #13972, #48160, #57118, #83944, #100728 ),
 ( #91244, #41405, #101267, #30782, #82296, #24013, #75572, #5595, #66628 ),
 ( #39744, #14524, #75016, #109166, #109705, #73908, #74471, #99624, #108036 ),
 ( #65517, #32452, #48715, #82838, #66073, #58208, #57674, #91788, #15064 ),
 ( #24564, #58755, #49262, #85584, #8329, #86156, #110801, #8879, #87264 ),
 ( #95111, #43061, #42493, #86706, #52572, #77221, #94542, #43612, #9999 ),
 ( #85038, #18376, #103497, #110246, #102932, #101829, #93437, #35758, #522 ),
 ( #34647, #68285, #26235, #93995, #10558, #76105, #76650, #102393, #68831 ),
 ( #27348, #25122, #60424, #78306, #16706, #61533, #104056, #59326, #50908 ),
 ( #34093, #44169, #95663, #59868, #25676, #17260, #9448, #1622, #17815 ),
 ( #60986, #51452, #69942, #33519, #52014, #18930, #77762, #1072, #35199 ),
 ( #69386, #53127, #26799, #67721, #37417, #98410, #104614, #54781, #62092 ),
 ( #71050, #97852, #37968, #70496, #105172, #21127, #38503, #55888, #27910 ),
 ( #55334, #21682, #3841, #79425, #90007, #28463, #20581, #88913, #12760 ),
 ( #54243, #36857, #44732, #11125, #2187, #46394, #78882, #36301, #96217 ),
 ( #53696, #19494, #62656, #81059, #89466, #80525, #12199, #88369, #87837 ) ),
 .UNSPECIFIED., .F., .F., .F.,
 ( 6, 3, 3, 3, 3, 3, 6 ),
 ( 6, 3, 6 ),
 ( 23.99353787332109889, 34.04292652270000019, 49.85499997250000348, 65.66707342230000677, 82.30866304890000151, 98.98173700649999773, 143.2994570502170006 ),
 ( -0.0001774529578859669783, 1.000000000000000000, 2.000198712178860028 ),
 .UNSPECIFIED. ) ;
#103733 = CARTESIAN_POINT ( 'NONE',  ( -106.4363417272620040, 1391.913060387289988, 304.7483998906039915 ) ) ;
#103734 = CARTESIAN_POINT ( 'NONE',  ( 18.92795655249999953, 1456.152682707289841, 200.2564363106190228 ) ) ;
#103735 = CARTESIAN_POINT ( 'NONE',  ( -4.038582018629999659, 1515.598601288590089, 209.1218459616989946 ) ) ;
#103736 = CARTESIAN_POINT ( 'NONE',  ( -13.90059962652860115, 1502.276548576450068, 227.4029734404369947 ) ) ;
#103737 = CARTESIAN_POINT ( 'NONE',  ( -9.052531689720000330, 1381.507819611680134, 200.6139546878390263 ) ) ;
#103738 = CARTESIAN_POINT ( 'NONE',  ( -4.992622171949999910, 1391.631312501089951, 203.6357468861989730 ) ) ;
#103739 = CARTESIAN_POINT ( 'NONE',  ( 9.806138588316610338, 1435.794735510610053, 209.7884860958980084 ) ) ;
#103740 = AXIS2_PLACEMENT_3D ( 'NONE', #52528, #86660, #36263 ) ;
#103741 = CARTESIAN_POINT ( 'NONE',  ( -15.50017078884119925, 1420.382688314539791, 210.7385713550720254 ) ) ;
#103742 = CARTESIAN_POINT ( 'NONE',  ( 4.250000000000000000, 1516.051704408390151, 209.1218459616989946 ) ) ;
#103743 = CARTESIAN_POINT ( 'NONE',  ( -0.8933028310894340907, 1419.625179221010058, 184.8271038220919991 ) ) ;
#103744 = CARTESIAN_POINT ( 'NONE',  ( -1.712644754285000070, 1516.636036526019780, 204.1262224792070015 ) ) ;
#103745 = CARTESIAN_POINT ( 'NONE',  ( -31.12456774391182535, 1525.960063244516959, 201.1524202391566121 ) ) ;
#103746 = SURFACE_STYLE_USAGE ( .BOTH. , #69624 ) ;
#103747 = CARTESIAN_POINT ( 'NONE',  ( 17.69622264849999738, 1430.679833671289771, 213.5595385020990022 ) ) ;
#103748 = CARTESIAN_POINT ( 'NONE',  ( 2.277483798560000050, 1508.992591874329946, 237.8394411828980139 ) ) ;
#103749 = AXIS2_PLACEMENT_3D ( 'NONE', #53065, #26169, #78807 ) ;
#103750 = CARTESIAN_POINT ( 'NONE',  ( 8.117022692521160820, 1504.304627734529959, 218.0272414185070033 ) ) ;
#103751 = CARTESIAN_POINT ( 'NONE',  ( 40.04388406862929628, 1448.778234248659828, 134.9800677253420247 ) ) ;
#103753 = ORIENTED_EDGE ( 'NONE', *, *, #28360, .F. ) ;
#103752 = CARTESIAN_POINT ( 'NONE',  ( -64.31310606715069866, 1379.736843722260119, 273.6487788150259917 ) ) ;
#103754 = EDGE_CURVE ( 'NONE', #19757, #105869, #46118, .T. ) ;
#103755 = VERTEX_POINT ( 'NONE', #21135 ) ;
#103756 = CARTESIAN_POINT ( 'NONE',  ( 11.60507608815730052, 1433.884017739829915, 151.1942475904019716 ) ) ;
#103757 = CARTESIAN_POINT ( 'NONE',  ( 22.04658049762480942, 1524.075132568165373, 184.4787145761434601 ) ) ;
#103758 = ORIENTED_EDGE ( 'NONE', *, *, #43488, .T. ) ;
#103759 = CARTESIAN_POINT ( 'NONE',  ( -1.085993468421462049, 1457.203538262298252, 199.6660069001111140 ) ) ;
#103760 = CARTESIAN_POINT ( 'NONE',  ( -23.59414818020000126, 1507.884704231529895, 195.6683835580979860 ) ) ;
#103761 = DIRECTION ( 'NONE',  ( -0.000000000000000000, -1.000000000000000000, -0.000000000000000000 ) ) ;
#103763 = CARTESIAN_POINT ( 'NONE',  ( 7.214502255410000231, 1427.316505021429975, 144.1938086916980239 ) ) ;
#103762 = CARTESIAN_POINT ( 'NONE',  ( -14.69331829855070026, 1452.091493848030041, 222.9975758587799817 ) ) ;
#103764 = CARTESIAN_POINT ( 'NONE',  ( 18.87855043325079762, 1458.344546833890035, 213.8102210560949743 ) ) ;
#103765 = B_SPLINE_CURVE_WITH_KNOTS ( 'NONE', 3,
 ( #9604, #52738, #43775, #70668, #35932, #68444, #69557, #60041, #70117, #28067, #69001, #53296, #52191, #103677, #104229, #104781, #76826, #140, #26976, #34262, #94719, #61166, #684, #94160, #53865, #77381, #60598, #10166, #102547, #51627, #19093, #103104, #86320, #78482, #27518, #26406, #77925, #85764, #1232, #25840, #35369, #34814, #9063, #95282, #43233, #86872, #19661, #44339, #1796, #61703, #44904, #95825, #87437, #10732, #79052, #2355, #96383, #62256, #36470, #88005, #42669 ),
 .UNSPECIFIED., .F., .F.,
 ( 4, 3, 3, 3, 3, 3, 3, 3, 3, 3, 3, 3, 3, 3, 3, 3, 3, 3, 3, 3, 4 ),
 ( 2.324858856900000159, 2.629298819338719895, 2.933834189079979726, 3.016888080820000262, 3.323211180994739777, 3.630193766017370205, 3.937176351040000188, 4.233214320261589947, 4.526002641850889852, 4.813615658591210433, 4.970096098089999970, 5.257590953320869787, 5.548112191959639894, 5.843468099502020507, 6.019659498230000239, 6.321166958536720060, 6.626011430711340466, 6.935803168168410693, 7.053491825980000129, 7.364378125943899178, 7.657659708029999734 ),
 .UNSPECIFIED. ) ;
#103766 = CARTESIAN_POINT ( 'NONE',  ( 6.609130007410000118, 1488.167526812230108, 183.3322403809980301 ) ) ;
#103767 = CARTESIAN_POINT ( 'NONE',  ( 2.359087563130000120, 1467.696298592889889, 218.9570129866989987 ) ) ;
#103768 = CARTESIAN_POINT ( 'NONE',  ( 15.70989997510000080, 1409.628288509730055, 226.4425047134980105 ) ) ;
#103769 = CARTESIAN_POINT ( 'NONE',  ( 5.012938863775000087, 1517.051603658920158, 211.6026598552170128 ) ) ;
#103770 = CARTESIAN_POINT ( 'NONE',  ( 14.20217058005079913, 1415.778512723909898, 197.1139478086609813 ) ) ;
#103771 = CARTESIAN_POINT ( 'NONE',  ( -8.684972823652898910, 1424.385334158459727, 206.2357065455580027 ) ) ;
#103772 = CARTESIAN_POINT ( 'NONE',  ( 7.100264587344999434, 1513.939092156090055, 201.4023203369069961 ) ) ;
#103773 = ORIENTED_EDGE ( 'NONE', *, *, #15514, .F. ) ;
#103774 = CARTESIAN_POINT ( 'NONE',  ( 13.81140031233439913, 1434.980667563419956, 148.6522636971369877 ) ) ;
#103775 = CARTESIAN_POINT ( 'NONE',  ( -7.879428933958430470, 1439.609447256930025, 226.0913591242859866 ) ) ;
#103776 = B_SPLINE_CURVE_WITH_KNOTS ( 'NONE', 3,
 ( #3484, #44939, #52226, #27012, #79636, #71254, #70705, #28665, #20245, #37613, #88039, #11323, #86354, #96422 ),
 .UNSPECIFIED., .F., .F.,
 ( 4, 2, 2, 2, 2, 2, 4 ),
 ( 0.000000000000000000, 0.0005712213022518396709, 0.001142442604503679342, 0.001713663906755519013, 0.002284885209007358683, 0.003427327813511035857, 0.004569770418014713030 ),
 .UNSPECIFIED. ) ;
#103777 = ORIENTED_EDGE ( 'NONE', *, *, #89465, .T. ) ;
#103778 = ORIENTED_EDGE ( 'NONE', *, *, #13293, .F. ) ;
#103779 = CARTESIAN_POINT ( 'NONE',  ( -7.597790811225000773, 1511.735270473989885, 215.4599558679070128 ) ) ;
#103780 = CARTESIAN_POINT ( 'NONE',  ( -14.45258105951289807, 1415.677402202029953, 212.7925583759839867 ) ) ;
#103781 = CIRCLE ( 'NONE', #71610, 2.000000000000000000 ) ;
#103782 = DIRECTION ( 'NONE',  ( 0.000000000000000000, 1.000000000000000000, 0.000000000000000000 ) ) ;
#103783 = CARTESIAN_POINT ( 'NONE',  ( -6.942354311545000378, 1516.905946377369901, 216.8406094761369900 ) ) ;
#103784 = CARTESIAN_POINT ( 'NONE',  ( -0.6005281695890769544, 1465.274001425240158, 198.1349723783799845 ) ) ;
#103785 = EDGE_CURVE ( 'NONE', #1934, #52452, #26021, .T. ) ;
#103786 = CARTESIAN_POINT ( 'NONE',  ( -19.08997683846052951, 1441.125342513460055, 209.8663685049180003 ) ) ;
#103787 = CARTESIAN_POINT ( 'NONE',  ( -49.28052484613377260, 1379.685954563121641, 238.1922399297049537 ) ) ;
#103788 = CARTESIAN_POINT ( 'NONE',  ( 4.256778553939329690, 1446.547191167049959, 160.0313428239830102 ) ) ;
#103789 = EDGE_CURVE ( 'NONE', #22625, #68839, #95464, .T. ) ;
#103790 = CARTESIAN_POINT ( 'NONE',  ( 0.9272409414739999356, 1508.839993243730078, 238.3381952508979964 ) ) ;
#103791 = ORIENTED_EDGE ( 'NONE', *, *, #10991, .F. ) ;
#103792 = CARTESIAN_POINT ( 'NONE',  ( -3.268859434184999913, 1516.922519270759949, 206.6438591998669949 ) ) ;
#103793 = ORIENTED_EDGE ( 'NONE', *, *, #86265, .F. ) ;
#103794 = CARTESIAN_POINT ( 'NONE',  ( -103.6155712370580062, 1379.922240051319932, 305.0844860589629661 ) ) ;
#103795 = VECTOR ( 'NONE', #16469, 1000.000000000000000 ) ;
#103796 = CARTESIAN_POINT ( 'NONE',  ( -18.63535451609999782, 1508.532394786730038, 229.9190513451980280 ) ) ;
#103797 = ORIENTED_EDGE ( 'NONE', *, *, #18482, .F. ) ;
#103798 = CARTESIAN_POINT ( 'NONE',  ( -5.513203518415759952, 1509.038617455540134, 201.6090956557640084 ) ) ;
#103799 = CARTESIAN_POINT ( 'NONE',  ( -13.84714808919999918, 1409.396613453830014, 191.2465958026980104 ) ) ;
#103800 = CARTESIAN_POINT ( 'NONE',  ( -24.67281693759999683, 1441.610155857880045, 210.7086710232079838 ) ) ;
#103801 = CARTESIAN_POINT ( 'NONE',  ( -10.79382126600000014, 1414.913060387329779, 196.1395803457980094 ) ) ;
#103802 = CARTESIAN_POINT ( 'NONE',  ( -0.1944809589943391759, 1455.245269478617274, 218.5524001425882261 ) ) ;
#103803 = CARTESIAN_POINT ( 'NONE',  ( 26.31342956949939804, 1441.279830909470093, 137.8584465659640159 ) ) ;
#103804 = CARTESIAN_POINT ( 'NONE',  ( -96.24750340660000347, 1384.324597676740041, 310.5510276952589948 ) ) ;
#103805 = CARTESIAN_POINT ( 'NONE',  ( 17.05308613158098652, 1435.093823724508866, 146.1608033541734244 ) ) ;
#103807 = DIRECTION ( 'NONE',  ( -3.237679667471999896E-17, -1.000000000000000000, -6.999474336859099157E-17 ) ) ;
#103806 = CARTESIAN_POINT ( 'NONE',  ( 31.32995031131202524, 1523.678648413191695, 221.9013357025044115 ) ) ;
#103808 = CARTESIAN_POINT ( 'NONE',  ( 7.333070134885000257, 1516.955859323880077, 214.9008457440070003 ) ) ;
#103809 = CARTESIAN_POINT ( 'NONE',  ( -3.071818229182819771, 1428.880991415399876, 200.2728629207279880 ) ) ;
#103810 = CARTESIAN_POINT ( 'NONE',  ( 5.556441548075099490, 1511.478393686179970, 217.5010704010999802 ) ) ;
#103811 = CARTESIAN_POINT ( 'NONE',  ( 29.61947514750000110, 1509.969965907130018, 207.5603945732279954 ) ) ;
#103812 = CARTESIAN_POINT ( 'NONE',  ( 5.012317068235000228, 1517.020727862619879, 211.9902797687369969 ) ) ;
#103813 = CARTESIAN_POINT ( 'NONE',  ( 42.06232107555830169, 1440.913060387330006, 269.6487541170399709 ) ) ;
#103814 = CARTESIAN_POINT ( 'NONE',  ( -17.27690404115233846, 1486.136442936737922, 187.9034219468923368 ) ) ;
#103816 = VERTEX_POINT ( 'NONE', #3849 ) ;
#103815 = CARTESIAN_POINT ( 'NONE',  ( -83.35163594419999811, 1388.281121046439921, 288.8577119767590489 ) ) ;
#103817 = AXIS2_PLACEMENT_3D ( 'NONE', #89295, #12591, #4197 ) ;
#103818 = CARTESIAN_POINT ( 'NONE',  ( 27.70845952490000030, 1450.383243101060089, 238.1060716476980019 ) ) ;
#103819 = DIRECTION ( 'NONE',  ( 0.9996573249755574819, 0.02617694830786557875, 0.000000000000000000 ) ) ;
#103820 = CARTESIAN_POINT ( 'NONE',  ( -28.27428436538610157, 1509.900420154179983, 216.9929459379879972 ) ) ;
#103821 = CARTESIAN_POINT ( 'NONE',  ( -3.662605128175850489, 1507.447374573099978, 236.6990675022970265 ) ) ;
#103822 = CARTESIAN_POINT ( 'NONE',  ( -21.04541642230000065, 1454.767645325029889, 223.1813744721980015 ) ) ;
#103824 = CARTESIAN_POINT ( 'NONE',  ( 19.24454973920000000, 1455.981838887030108, 226.3136641516979921 ) ) ;
#103823 = CARTESIAN_POINT ( 'NONE',  ( 10.97839330989999951, 1432.873337069130002, 151.7696626780980012 ) ) ;
#103825 = CARTESIAN_POINT ( 'NONE',  ( -10.26351865721099799, 1448.707356115169887, 207.5368705317330011 ) ) ;
#103826 = CARTESIAN_POINT ( 'NONE',  ( -108.6610895849279927, 1383.759820234390190, 311.0754968279820218 ) ) ;
#103827 = ORIENTED_EDGE ( 'NONE', *, *, #13996, .F. ) ;
#103828 = CARTESIAN_POINT ( 'NONE',  ( -4.621267922064999922, 1516.830644417779922, 204.1223895416970038 ) ) ;
#103829 = CARTESIAN_POINT ( 'NONE',  ( 1.297592866489999927E-09, 1405.775964805530066, 268.4837719564979466 ) ) ;
#103830 = CIRCLE ( 'NONE', #101, 9.522913805090002626 ) ;
#103831 = CARTESIAN_POINT ( 'NONE',  ( 29.13505175353622079, 1526.073429442291854, 197.1475357601794940 ) ) ;
#103832 = CARTESIAN_POINT ( 'NONE',  ( 12.98581290379999942, 1428.689068522430034, 223.6918876029980083 ) ) ;
#103833 = CARTESIAN_POINT ( 'NONE',  ( 5.436747755899999923, 1437.112761795790220, 154.7095357218980212 ) ) ;
#103834 = CARTESIAN_POINT ( 'NONE',  ( -26.99540727154380093, 1450.681735027889999, 136.4489462876310313 ) ) ;
#103835 = CARTESIAN_POINT ( 'NONE',  ( -0.8968889248344054099, 1469.603208379229500, 219.1395986089293331 ) ) ;
#103836 = CARTESIAN_POINT ( 'NONE',  ( -42.29870041503930622, 1440.913060411070092, 262.3297496996750056 ) ) ;
#103837 = CARTESIAN_POINT ( 'NONE',  ( -26.84535680910000011, 1449.047047365870185, 136.7368231881980023 ) ) ;
#103838 = CARTESIAN_POINT ( 'NONE',  ( 4.363122647530000009, 1414.776585547029981, 163.8086717993979846 ) ) ;
#103839 = CARTESIAN_POINT ( 'NONE',  ( 1.401811570890000080, 1430.917890128589988, 199.7550729045790092 ) ) ;
#103840 = CARTESIAN_POINT ( 'NONE',  ( 11.18378284279590140, 1480.307833489839823, 211.0917726453040189 ) ) ;
#103841 = CARTESIAN_POINT ( 'NONE',  ( 1.894388308689999967, 1506.148290744889891, 221.7829938216989945 ) ) ;
#103843 = CARTESIAN_POINT ( 'NONE',  ( -42.06231979437640689, 1440.913089571769888, 269.6487552725350270 ) ) ;
#103842 = VECTOR ( 'NONE', #37084, 1000.000000000000114 ) ;
#103844 = EDGE_LOOP ( 'NONE', ( #57649, #41331, #87099, #15254, #13787, #71637, #14947, #98810 ) ) ;
#103845 = CARTESIAN_POINT ( 'NONE',  ( 0.5133626083067620582, 1410.311097044259895, 185.0719925509139898 ) ) ;
#103846 = CARTESIAN_POINT ( 'NONE',  ( 3.066664150160000268, 1486.999178531689950, 197.5625016150989950 ) ) ;
#103847 = CARTESIAN_POINT ( 'NONE',  ( 9.145085911806999590, 1467.511344352970127, 205.0022163952010317 ) ) ;
#103848 = CIRCLE ( 'NONE', #55603, 33.13701971169416538 ) ;
#103849 = CARTESIAN_POINT ( 'NONE',  ( -0.8130327484720001330, 1417.377572236629931, 235.4819850726979951 ) ) ;
#103850 = CARTESIAN_POINT ( 'NONE',  ( 5.466273243599998999, 1504.965088730989919, 220.6538119101990105 ) ) ;
#103851 = CARTESIAN_POINT ( 'NONE',  ( -31.40702543711151762, 1523.611961620354123, 196.3340613265682464 ) ) ;
#103852 = CARTESIAN_POINT ( 'NONE',  ( 8.177818021369999357, 1422.878296110979818, 213.9391550444189818 ) ) ;
#103853 = CARTESIAN_POINT ( 'NONE',  ( -15.09720442233679805, 1384.876713416460007, 219.4545074913159795 ) ) ;
#103854 = CARTESIAN_POINT ( 'NONE',  ( -18.04709463619999710, 1415.245980412329800, 207.8128127142179835 ) ) ;
#103855 = CARTESIAN_POINT ( 'NONE',  ( -10.01326719289999900, 1481.014340515889899, 205.7823630344090020 ) ) ;
#103856 = CARTESIAN_POINT ( 'NONE',  ( 7.886115920484915165, 1512.218044538973345, 206.1805372229848956 ) ) ;
#103857 = CARTESIAN_POINT ( 'NONE',  ( 5.389719913101400195, 1440.971386073809981, 154.8246291173960003 ) ) ;
#103858 = ORIENTED_EDGE ( 'NONE', *, *, #100216, .T. ) ;
#103859 = AXIS2_PLACEMENT_3D ( 'NONE', #42965, #93893, #67623 ) ;
#103860 = CARTESIAN_POINT ( 'NONE',  ( -17.03291860866149676, 1409.881251985120116, 225.5426873045980187 ) ) ;
#103861 = CARTESIAN_POINT ( 'NONE',  ( 2.446787376320000096, 1432.353341358199941, 150.2884730787980061 ) ) ;
#103862 = ORIENTED_EDGE ( 'NONE', *, *, #54949, .F. ) ;
#103863 = ORIENTED_EDGE ( 'NONE', *, *, #34397, .F. ) ;
#103864 = CARTESIAN_POINT ( 'NONE',  ( -2.975037811039999980, 1495.689967157589763, 216.9727041533189720 ) ) ;
#103865 = CARTESIAN_POINT ( 'NONE',  ( 7.501993457708461044, 1516.814304245379844, 208.6975970486373626 ) ) ;
#103867 = CARTESIAN_POINT ( 'NONE',  ( -2.932381175664569906, 1457.907782490749923, 219.3878279419139972 ) ) ;
#103866 = CARTESIAN_POINT ( 'NONE',  ( 11.09190030210000089, 1426.903748879130035, 97.30362720369791418 ) ) ;
#103868 = DIRECTION ( 'NONE',  ( -0.6736849260863841948, 0.000000000000000000, 0.7390186874254148774 ) ) ;
#103869 = CARTESIAN_POINT ( 'NONE',  ( 4.311753873931529313, 1425.506783100830035, 185.4196544955500201 ) ) ;
#103870 = CARTESIAN_POINT ( 'NONE',  ( -2.497703869279095379, 1421.154004695713866, 184.9625613379778315 ) ) ;
#103871 = CARTESIAN_POINT ( 'NONE',  ( 7.594045040249999268, 1425.546108791900224, 212.0390539736889934 ) ) ;
#103872 = CARTESIAN_POINT ( 'NONE',  ( 18.38166056949999927, 1428.164368492389940, 201.4944003551989908 ) ) ;
#103873 = CARTESIAN_POINT ( 'NONE',  ( 7.829163140769999529, 1507.896460528530042, 182.8030300680979963 ) ) ;
#103874 = CARTESIAN_POINT ( 'NONE',  ( -113.4000000000000057, 1377.020218211860083, 306.8927966156020375 ) ) ;
#103875 = CARTESIAN_POINT ( 'NONE',  ( 8.122847524725520074, 1364.881652834217903, 208.3718459617061285 ) ) ;
#103877 = ORIENTED_EDGE ( 'NONE', *, *, #7521, .F. ) ;
#103876 = CARTESIAN_POINT ( 'NONE',  ( 4.758389699129999428, 1454.760432536389999, 217.3925755712789964 ) ) ;
#103878 = VERTEX_POINT ( 'NONE', #37976 ) ;
#103879 = EDGE_CURVE ( 'NONE', #5789, #8681, #52857, .T. ) ;
#103880 = CARTESIAN_POINT ( 'NONE',  ( -41.66090858750000336, 1443.836096447190130, 135.6920785174980040 ) ) ;
#103881 = LINE ( 'NONE', #68104, #63699 ) ;
#103882 = CARTESIAN_POINT ( 'NONE',  ( -2.245209799710000009, 1471.752125626330098, 269.8658162814979846 ) ) ;
#103883 = CARTESIAN_POINT ( 'NONE',  ( -110.0629314620319974, 1384.917035430780061, 296.9512851041370141 ) ) ;
#103884 = CARTESIAN_POINT ( 'NONE',  ( -121.4211954113599745, 1309.112692017089785, 312.2430413686192310 ) ) ;
#103885 = CARTESIAN_POINT ( 'NONE',  ( 23.34540950859999953, 1507.878524956530100, 194.4697486434980078 ) ) ;
#103886 = CARTESIAN_POINT ( 'NONE',  ( 2.268748340400060126, 1476.248048840699994, 197.8527876105920029 ) ) ;
#103887 = EDGE_CURVE ( 'NONE', #36271, #74608, #72158, .T. ) ;
#103888 = CARTESIAN_POINT ( 'NONE',  ( -35.12460981859439357, 1451.531087103250002, 135.5516170584860163 ) ) ;
#103889 = CARTESIAN_POINT ( 'NONE',  ( -1.906499846882070084E-08, 1515.051704408389924, 209.1218459511669892 ) ) ;
#103890 = CARTESIAN_POINT ( 'NONE',  ( 18.02093535799999913, 1424.326836137830014, 225.1991050518980160 ) ) ;
#103891 = CARTESIAN_POINT ( 'NONE',  ( 7.818221670731199779, 1367.736483592526156, 210.6218459616991936 ) ) ;
#103892 = CARTESIAN_POINT ( 'NONE',  ( 13.75707076230000148, 1408.364212814029997, 211.9527283592179856 ) ) ;
#103893 = CARTESIAN_POINT ( 'NONE',  ( -0.7631012575699189782, 1406.777862902510151, 269.6501330761860231 ) ) ;
#103894 = CARTESIAN_POINT ( 'NONE',  ( -14.38420833757800033, 1435.582840502069757, 149.6588806134069785 ) ) ;
#103895 = ORIENTED_EDGE ( 'NONE', *, *, #69666, .F. ) ;
#103896 = CARTESIAN_POINT ( 'NONE',  ( -2.500000000000000000, 1440.913060387330006, 209.1218459616979999 ) ) ;
#103897 = CARTESIAN_POINT ( 'NONE',  ( 13.27118260120000137, 1442.692795410319832, 188.6610245367980099 ) ) ;
#103898 = ORIENTED_EDGE ( 'NONE', *, *, #83533, .F. ) ;
#103899 = ORIENTED_EDGE ( 'NONE', *, *, #2239, .F. ) ;
#103900 = CARTESIAN_POINT ( 'NONE',  ( -4.378216171020000047, 1453.707746106390005, 199.6107948432290016 ) ) ;
#103901 = CARTESIAN_POINT ( 'NONE',  ( 6.892224678239999847, 1361.632554499750086, 207.6218459616989946 ) ) ;
#103902 = CARTESIAN_POINT ( 'NONE',  ( -2.866857931135000204, 1516.951766529250108, 213.1652121904069759 ) ) ;
#103903 = CARTESIAN_POINT ( 'NONE',  ( 4.059671795525000348, 1511.437978678640093, 217.3350408236069882 ) ) ;
#103904 =( GEOMETRIC_REPRESENTATION_CONTEXT ( 3 ) GLOBAL_UNCERTAINTY_ASSIGNED_CONTEXT ( ( #59222 ) ) GLOBAL_UNIT_ASSIGNED_CONTEXT ( ( #43444, #78130, #68112 ) ) REPRESENTATION_CONTEXT ( 'NONE', 'WORKASPACE' ) );
#103905 = ORIENTED_EDGE ( 'NONE', *, *, #11687, .T. ) ;
#103906 = CARTESIAN_POINT ( 'NONE',  ( -65.41103462389999379, 1377.321258373460068, 268.8604125841590076 ) ) ;
#103907 = TOROIDAL_SURFACE ( 'NONE', #28789, 6.868727599660000571, 1.000000000000000000 ) ;
#103908 = CARTESIAN_POINT ( 'NONE',  ( -106.4561910723670053, 1378.913060387289988, 301.9552841335789708 ) ) ;
#103909 = CARTESIAN_POINT ( 'NONE',  ( 6.550389432124999800, 1516.755758396839838, 204.1155163507169732 ) ) ;
#103910 = CARTESIAN_POINT ( 'NONE',  ( -28.31645363330000009, 1509.601692267130147, 205.7529699828779997 ) ) ;
#103911 = CARTESIAN_POINT ( 'NONE',  ( -3.173602190014999991, 1510.830536680500245, 201.5621726280170094 ) ) ;
#103912 = CARTESIAN_POINT ( 'NONE',  ( 11.87502392341400004, 1433.007271648830056, 149.9804723818110119 ) ) ;
#103913 = CARTESIAN_POINT ( 'NONE',  ( -66.58891394985930390, 1384.715272088890060, 258.5866899849719971 ) ) ;
#103914 = CARTESIAN_POINT ( 'NONE',  ( 10.46269364489999987, 1491.122602117189899, 212.5073291737689942 ) ) ;
#103915 = AXIS2_PLACEMENT_3D ( 'NONE', #94880, #34964, #26562 ) ;
#103916 = CARTESIAN_POINT ( 'NONE',  ( -7.396545081224999763, 1511.069621805459974, 215.4940135707269917 ) ) ;
#103918 = ORIENTED_EDGE ( 'NONE', *, *, #38793, .F. ) ;
#103917 = CARTESIAN_POINT ( 'NONE',  ( -4.043557851940000170, 1446.816496427589982, 184.5928732699980230 ) ) ;
#103919 = CARTESIAN_POINT ( 'NONE',  ( 28.25319066630000009, 1451.926638454029899, 134.8820817050979883 ) ) ;
#103920 = CARTESIAN_POINT ( 'NONE',  ( -24.88581067337899810, 1440.913060480750119, 215.3118859389570048 ) ) ;
#103921 = CARTESIAN_POINT ( 'NONE',  ( 10.52183747938889979, 1460.134765062619863, 206.2567342059500106 ) ) ;
#103922 = CARTESIAN_POINT ( 'NONE',  ( -24.78163162830000132, 1435.369157292130012, 136.0792171752979982 ) ) ;
#103923 = VECTOR ( 'NONE', #90338, 1000.000000000000227 ) ;
#103924 = CARTESIAN_POINT ( 'NONE',  ( -1.701027861004999808, 1516.937508036699910, 211.6166039682370013 ) ) ;
#103925 = CARTESIAN_POINT ( 'NONE',  ( -68.64142316320000248, 1379.747636946170132, 279.8413332628590524 ) ) ;
#103926 = CARTESIAN_POINT ( 'NONE',  ( 8.612130213264160616, 1437.494969288449965, 211.0257522034609963 ) ) ;
#103927 = CARTESIAN_POINT ( 'NONE',  ( 5.172586535390000684, 1492.767659076290101, 188.8148697515989909 ) ) ;
#103928 = CARTESIAN_POINT ( 'NONE',  ( -5.586178488784369733, 1491.246080089150155, 185.8699216472389821 ) ) ;
#103929 = CARTESIAN_POINT ( 'NONE',  ( 0.7402208603880020554, 1516.992029636990083, 208.3685455796920110 ) ) ;
#103930 = ORIENTED_EDGE ( 'NONE', *, *, #79453, .F. ) ;
#103931 = CARTESIAN_POINT ( 'NONE',  ( 2.500000000000000000, 1439.077099669189920, 157.7246394012979920 ) ) ;
#103932 = CARTESIAN_POINT ( 'NONE',  ( -12.75379259890000050, 1412.829786118129960, 228.0544790036979919 ) ) ;
#103933 = CARTESIAN_POINT ( 'NONE',  ( -47.37590574939999755, 1384.752751010099928, 256.2773158601589785 ) ) ;
#103934 = ORIENTED_EDGE ( 'NONE', *, *, #69455, .F. ) ;
#103936 = VECTOR ( 'NONE', #4697, 1000.000000000000227 ) ;
#103935 = CARTESIAN_POINT ( 'NONE',  ( 21.83863729849015911, 1523.580204110582144, 234.9763103240493081 ) ) ;
#103937 = CARTESIAN_POINT ( 'NONE',  ( -3.630422229999999750, 1429.843096179090026, 201.6307972852089847 ) ) ;
#103938 = CARTESIAN_POINT ( 'NONE',  ( 12.05097526569999822, 1434.216276041280025, 150.6184982174980007 ) ) ;
#103939 = CARTESIAN_POINT ( 'NONE',  ( 17.73694109413560227, 1478.710361465350161, 229.1951871287480174 ) ) ;
#103940 = CARTESIAN_POINT ( 'NONE',  ( -6.774723970312340526, 1511.035127054690065, 200.8105558358980147 ) ) ;
#103941 = DIRECTION ( 'NONE',  ( -0.000000000000000000, 1.000000000000000000, -0.000000000000000000 ) ) ;
#103942 = CARTESIAN_POINT ( 'NONE',  ( -0.06620051369889999593, 1409.084365175830044, 232.6715855378979825 ) ) ;
#103943 = CARTESIAN_POINT ( 'NONE',  ( 2.879377773099999871, 1417.724437854929874, 234.4927649805979968 ) ) ;
#103945 = FACE_OUTER_BOUND ( 'NONE', #85588, .T. ) ;
#103944 = CARTESIAN_POINT ( 'NONE',  ( -3.257220640824999958, 1517.040132827679827, 214.9086836491569841 ) ) ;
#103946 = CARTESIAN_POINT ( 'NONE',  ( 18.65749896639999861, 1509.387464492230038, 187.4422726698979886 ) ) ;
#103947 = CARTESIAN_POINT ( 'NONE',  ( -1.126138146715000010, 1517.208444099459939, 216.8485306577670144 ) ) ;
#103948 = VERTEX_POINT ( 'NONE', #59201 ) ;
#103949 = CARTESIAN_POINT ( 'NONE',  ( -13.02322915955869931, 1416.825783990419950, 196.6108486074699897 ) ) ;
#103950 = CARTESIAN_POINT ( 'NONE',  ( -20.63236152680000046, 1508.913060324029857, 189.5446908899980087 ) ) ;
#103951 = ORIENTED_EDGE ( 'NONE', *, *, #24856, .F. ) ;
#103952 = CIRCLE ( 'NONE', #75363, 1.000000000000007994 ) ;
#103953 = DIRECTION ( 'NONE',  ( -6.123233995736769734E-17, -1.000000000000000000, 7.888609052210119587E-33 ) ) ;
#103954 = FACE_OUTER_BOUND ( 'NONE', #97711, .T. ) ;
#103955 = CARTESIAN_POINT ( 'NONE',  ( 5.513435553965000402, 1508.551704408389924, 202.1089243864769855 ) ) ;
#103956 = DIRECTION ( 'NONE',  ( -8.453952912920146445E-06, -0.03084653019238408483, 0.9995241325268845456 ) ) ;
#103957 = CARTESIAN_POINT ( 'NONE',  ( -32.36284091029009602, 1525.878013734320348, 199.2622049721628628 ) ) ;
#103958 = CARTESIAN_POINT ( 'NONE',  ( 2197.008826411130485, 11216.44053380570767, -1526.289979289628263 ) ) ;
#103959 = CARTESIAN_POINT ( 'NONE',  ( 18.06884258770000073, 1415.263254653229978, 210.5556769813279914 ) ) ;
#103960 = CARTESIAN_POINT ( 'NONE',  ( -18.67603340750000029, 1425.535634798130104, 226.2166979841979924 ) ) ;
#103961 = CARTESIAN_POINT ( 'NONE',  ( 16.66936639839085643, 1523.456924617336881, 180.4828114240358161 ) ) ;
#103962 = CARTESIAN_POINT ( 'NONE',  ( -14.47191459792289869, 1379.648775954749908, 208.1784578746709826 ) ) ;
#103963 = CARTESIAN_POINT ( 'NONE',  ( 5.513435558014999849, 1508.551704408389924, 216.1347675157070114 ) ) ;
#103965 = CARTESIAN_POINT ( 'NONE',  ( -19.06177424568263845, 1440.331832736574825, 209.7871912064330786 ) ) ;
#103964 = CARTESIAN_POINT ( 'NONE',  ( 11.23851827549999882, 1490.487975447490044, 204.0492753133389954 ) ) ;
#103966 = CARTESIAN_POINT ( 'NONE',  ( 0.7800921441517267851, 1526.382868172863937, 241.4567505818334610 ) ) ;
#103967 = EDGE_LOOP ( 'NONE', ( #46866, #24744, #29590, #9168, #96755, #57546, #86084, #37257 ) ) ;
#103968 = CARTESIAN_POINT ( 'NONE',  ( 1.551173678986830007, 1415.834070661230044, 190.5513134611869930 ) ) ;
#103969 = CARTESIAN_POINT ( 'NONE',  ( -9221.844916327461760, 50.28429875023816464, -5636.577220017842592 ) ) ;
#103970 = CARTESIAN_POINT ( 'NONE',  ( -24.32341588750000128, 1436.131012997689822, 210.7992627561380061 ) ) ;
#103971 = CARTESIAN_POINT ( 'NONE',  ( 4.098232394932746381, 1410.432529984579560, 186.0633403236960248 ) ) ;
#103972 = CARTESIAN_POINT ( 'NONE',  ( -4.107671006832890548, 1426.017999997803372, 186.1051448316069354 ) ) ;
#103973 = PRESENTATION_LAYER_ASSIGNMENT (  '', '', ( #27106 ) ) ;
#103974 = LINE ( 'NONE', #52491, #44881 ) ;
#103975 = FACE_OUTER_BOUND ( 'NONE', #48698, .T. ) ;
#103976 = CARTESIAN_POINT ( 'NONE',  ( -10.46254913605810088, 1491.357146916849842, 212.5408882096329819 ) ) ;
#103977 = CARTESIAN_POINT ( 'NONE',  ( -17.66148018635020378, 1440.150399676859934, 218.7822600330530065 ) ) ;
#103978 = CARTESIAN_POINT ( 'NONE',  ( -99.87664611743339549, 1383.764086582540131, 310.6354922946979968 ) ) ;
#103979 = CARTESIAN_POINT ( 'NONE',  ( -109.9700156609570030, 1384.452758312609831, 311.4358946100080061 ) ) ;
#103980 = CARTESIAN_POINT ( 'NONE',  ( -15.56983240930392043, 1506.527232285067157, 224.7512174644303684 ) ) ;
#103981 = CARTESIAN_POINT ( 'NONE',  ( 11.49747574013809981, 1416.913060341719984, 220.3427041143820020 ) ) ;
#103983 = EDGE_LOOP ( 'NONE', ( #45217, #55091 ) ) ;
#103982 = CARTESIAN_POINT ( 'NONE',  ( 22.97053994450000047, 1507.867546928429874, 193.7497404625980266 ) ) ;
#103984 = CARTESIAN_POINT ( 'NONE',  ( -1.441539424119999913, 1414.983771850430003, 226.5042059068979938 ) ) ;
#103985 = CARTESIAN_POINT ( 'NONE',  ( -84.09514530399998478, 1383.332197241610174, 288.0930448863589959 ) ) ;
#103986 = DIRECTION ( 'NONE',  ( -1.755985294532469921E-16, 1.000000000000000000, -1.338183447452831989E-16 ) ) ;
#103987 = ORIENTED_EDGE ( 'NONE', *, *, #77840, .T. ) ;
#103988 = ORIENTED_EDGE ( 'NONE', *, *, #9346, .T. ) ;
#103989 = CARTESIAN_POINT ( 'NONE',  ( 17.88477383430709722, 1509.485346479319787, 231.9786773698629929 ) ) ;
#103990 = CARTESIAN_POINT ( 'NONE',  ( -6.375527264914699010, 1460.280752625940067, 210.0337940185919763 ) ) ;
#103991 = CARTESIAN_POINT ( 'NONE',  ( 13.13626245617426669, 1443.056086229705443, 169.4004656986877819 ) ) ;
#103993 = CARTESIAN_POINT ( 'NONE',  ( -26.19682434950000172, 1465.282665911629920, 259.6167014773980100 ) ) ;
#103992 = CARTESIAN_POINT ( 'NONE',  ( 19.92213876099999936, 1452.807100928230057, 209.3894951820489894 ) ) ;
#103994 = CARTESIAN_POINT ( 'NONE',  ( -4.598493981323799495, 1495.170853321719960, 197.6879014759489905 ) ) ;
#103995 = CARTESIAN_POINT ( 'NONE',  ( -109.1848878950000028, 1384.511724394249995, 297.1380044401590226 ) ) ;
#103996 = AXIS2_PLACEMENT_3D ( 'NONE', #77962, #24769, #51119 ) ;
#103997 = CARTESIAN_POINT ( 'NONE',  ( 26.88792401699999957, 1508.603612559529893, 206.2262326685279845 ) ) ;
#103998 = CARTESIAN_POINT ( 'NONE',  ( -19.83538623540000145, 1485.649277471630057, 190.4852910309980132 ) ) ;
#103999 = CARTESIAN_POINT ( 'NONE',  ( 2.641394305209999960, 1409.510112843430079, 185.8263422457980028 ) ) ;
#104000 = CARTESIAN_POINT ( 'NONE',  ( 5.950109296629999989, 1421.372702594429938, 186.2244564570979719 ) ) ;
#104001 = CARTESIAN_POINT ( 'NONE',  ( -6.017144072120000686, 1442.258634816289941, 154.7968030204980039 ) ) ;
#104002 = CARTESIAN_POINT ( 'NONE',  ( 8.234565746623669469, 1434.603406620469741, 205.5025735347319937 ) ) ;
#104003 = CYLINDRICAL_SURFACE ( 'NONE', #64508, 2.000000000000000000 ) ;
#104004 = CARTESIAN_POINT ( 'NONE',  ( -11.79257184573279993, 1490.424927523380120, 209.6468054329459960 ) ) ;
#104005 = DIRECTION ( 'NONE',  ( -1.000000000000000000, 0.000000000000000000, 0.000000000000000000 ) ) ;
#104006 = ORIENTED_EDGE ( 'NONE', *, *, #101368, .T. ) ;
#104007 = CARTESIAN_POINT ( 'NONE',  ( -11.98355723010000062, 1507.902190792990041, 208.7310628602519955 ) ) ;
#104008 = CARTESIAN_POINT ( 'NONE',  ( 20.42677715031149788, 1475.927527670890186, 217.8974877716310061 ) ) ;
#104009 = CARTESIAN_POINT ( 'NONE',  ( -39.10257508149999950, 1457.313645690129988, 270.0008335182980090 ) ) ;
#104010 = DIRECTION ( 'NONE',  ( 0.7414773880254775795, -1.225281874271768203E-16, 0.6709778558543607607 ) ) ;
#104011 =( BOUNDED_SURFACE ( )  B_SPLINE_SURFACE ( 2, 1, ( 
 ( #79237, #28825 ),
 ( #61902, #29357 ),
 ( #88734, #89271 ),
 ( #88184, #104976 ),
 ( #4176, #12568 ),
 ( #79791, #54057 ),
 ( #46748, #37225 ),
 ( #46197, #80880 ),
 ( #11476, #63022 ),
 ( #38308, #80332 ),
 ( #28264, #45098 ) ),
 .UNSPECIFIED., .T., .F., .F. ) 
 B_SPLINE_SURFACE_WITH_KNOTS ( ( 3, 2, 2, 2, 2, 3 ),
 ( 2, 2 ),
 ( 1.721761971665859647, 3.141592653589790007, 4.712388980384689674, 6.283185307179590673, 7.853981633974480125, 8.004947278845451208 ),
 ( -17.86299485559450062, 35.72598970969769994 ),
 .UNSPECIFIED. ) 
 GEOMETRIC_REPRESENTATION_ITEM ( )  RATIONAL_B_SPLINE_SURFACE ( (
 ( 0.9491121336701279221, 0.9491121336701279221),
 ( 0.7352560790313750205, 0.7352560790313750205),
 ( 1.000000000000000000, 1.000000000000000000),
 ( 0.7071067811865510144, 0.7071067811865510144),
 ( 1.000000000000000000, 1.000000000000000000),
 ( 0.7071067811865510144, 0.7071067811865510144),
 ( 1.000000000000000000, 1.000000000000000000),
 ( 0.7071067811865510144, 0.7071067811865510144),
 ( 1.000000000000000000, 1.000000000000000000),
 ( 0.9718507021551759939, 0.9718507021551759939),
 ( 0.9491121336701279221, 0.9491121336701279221) ) ) 
 REPRESENTATION_ITEM ( '' )  SURFACE ( )  );
#104012 = CARTESIAN_POINT ( 'NONE',  ( 17.63079482879999915, 1410.452322071830167, 223.6591261867980052 ) ) ;
#104013 = FACE_OUTER_BOUND ( 'NONE', #50365, .T. ) ;
#104014 = AXIS2_PLACEMENT_3D ( 'NONE', #66130, #14021, #7292 ) ;
#104015 = DIRECTION ( 'NONE',  ( 0.000000000000000000, 1.000000000000000000, 0.000000000000000000 ) ) ;
#104016 = CARTESIAN_POINT ( 'NONE',  ( -20.60448988230000111, 1484.737042837089803, 209.1218459616989946 ) ) ;
#104017 = CARTESIAN_POINT ( 'NONE',  ( -2.804945344961504716, 1516.554483488290998, 201.4122858543795189 ) ) ;
#104018 = CARTESIAN_POINT ( 'NONE',  ( -6.279660886640000328, 1416.867457637430107, 231.6963788028980105 ) ) ;
#104019 = CARTESIAN_POINT ( 'NONE',  ( -1.108701933971497633, 1484.799112515838033, 182.1781186121703513 ) ) ;
#104020 = CARTESIAN_POINT ( 'NONE',  ( -5.209651373121763740, 1358.975734498126940, 209.6218459617033432 ) ) ;
#104021 = CARTESIAN_POINT ( 'NONE',  ( -44.70539842100279770, 1432.153755970550264, 268.2536652372499475 ) ) ;
#104022 = CARTESIAN_POINT ( 'NONE',  ( -2.499999999990000443, 1434.166392531650217, 184.3332466033980097 ) ) ;
#104023 = ORIENTED_EDGE ( 'NONE', *, *, #102328, .T. ) ;
#104024 = CARTESIAN_POINT ( 'NONE',  ( -9.255392140700001491, 1423.205578550119753, 209.4023171091370159 ) ) ;
#104025 = ORIENTED_EDGE ( 'NONE', *, *, #35739, .T. ) ;
#104026 = CARTESIAN_POINT ( 'NONE',  ( 2.493697040924999886, 1516.977201124959947, 210.2401991861970032 ) ) ;
#104027 = CARTESIAN_POINT ( 'NONE',  ( -7.437974795490000623, 1473.518143733989973, 200.3716835635890163 ) ) ;
#104028 = CARTESIAN_POINT ( 'NONE',  ( -3.369085047521843457, 1470.161991784903194, 218.6691817296217835 ) ) ;
#104029 = CARTESIAN_POINT ( 'NONE',  ( -4.487249792034999629, 1509.038615934239942, 212.6094383991670043 ) ) ;
#104030 = CIRCLE ( 'NONE', #7477, 1.000000000000000666 ) ;
#104031 = CARTESIAN_POINT ( 'NONE',  ( 2.204495346684369750, 1495.683245216109981, 221.2628089792190167 ) ) ;
#104032 = VERTEX_POINT ( 'NONE', #92772 ) ;
#104033 = CARTESIAN_POINT ( 'NONE',  ( -16.19086242769280304, 1409.478452467050147, 225.0103265570539861 ) ) ;
#104035 = CARTESIAN_POINT ( 'NONE',  ( -15.06905043960169976, 1513.645442089240078, 223.6837085688980267 ) ) ;
#104034 = CARTESIAN_POINT ( 'NONE',  ( -11.81780673814840021, 1517.151704408390060, 222.7166774759110126 ) ) ;
#104036 = CIRCLE ( 'NONE', #89737, 3.000000000000002665 ) ;
#104037 = CARTESIAN_POINT ( 'NONE',  ( 1.800204229380000243, 1413.682656150029970, 232.3423579875980067 ) ) ;
#104038 = CARTESIAN_POINT ( 'NONE',  ( -11.44665353847253186, 1425.798163151176823, 139.1345268192609126 ) ) ;
#104039 = CARTESIAN_POINT ( 'NONE',  ( 6.153332312239999879, 1471.680546255089894, 217.2442593896689971 ) ) ;
#104040 = CARTESIAN_POINT ( 'NONE',  ( -9.490149457628850982, 1439.534074077459991, 207.9559815647490097 ) ) ;
#104041 = ORIENTED_EDGE ( 'NONE', *, *, #1576, .F. ) ;
#104042 = CARTESIAN_POINT ( 'NONE',  ( -1.800556938495289971, 1410.057666395089882, 269.8656564991380264 ) ) ;
#104043 = CARTESIAN_POINT ( 'NONE',  ( 0.7374508827770021036, 1516.978425811520083, 207.9881927911069965 ) ) ;
#104044 = CARTESIAN_POINT ( 'NONE',  ( 7.833511190420000325, 1418.000725493129949, 231.1317660673979901 ) ) ;
#104045 = LINE ( 'NONE', #1608, #91260 ) ;
#104047 = VERTEX_POINT ( 'NONE', #32329 ) ;
#104046 = CARTESIAN_POINT ( 'NONE',  ( -8.016541010710112047, 1366.397902625823463, 207.6218459616988241 ) ) ;
#104048 = EDGE_LOOP ( 'NONE', ( #59383, #36083, #49104, #90240, #19498 ) ) ;
#104049 = CARTESIAN_POINT ( 'NONE',  ( -22.57316855434390135, 1409.701313687740139, 209.4509182103790010 ) ) ;
#104050 = EDGE_CURVE ( 'NONE', #15491, #92642, #107554, .T. ) ;
#104051 = CARTESIAN_POINT ( 'NONE',  ( -0.2723609444870630503, 1409.428891713289886, 185.2334270307050019 ) ) ;
#104052 = CARTESIAN_POINT ( 'NONE',  ( 3.651998852415098362, 1424.315861867868080, 184.2127881604313586 ) ) ;
#104053 = CARTESIAN_POINT ( 'NONE',  ( -28.90443088959890261, 1413.811766471930923, 266.6320645011991814 ) ) ;
#104054 = CARTESIAN_POINT ( 'NONE',  ( -20.62644837504292283, 1436.449369547013475, 144.7505193540382322 ) ) ;
#104055 = CARTESIAN_POINT ( 'NONE',  ( -20.78701115710000025, 1430.788020833330165, 221.2610285622980086 ) ) ;
#104056 = CARTESIAN_POINT ( 'NONE',  ( 32.91329245024750350, 1465.287215665440044, 268.8838783738780194 ) ) ;
#104057 = CARTESIAN_POINT ( 'NONE',  ( -11.35998449626690032, 1391.913060387289988, 207.0982575650849924 ) ) ;
#104058 = CARTESIAN_POINT ( 'NONE',  ( 8.739359048380000772, 1447.264120250649967, 186.1039452748980239 ) ) ;
#104059 = CARTESIAN_POINT ( 'NONE',  ( 6.934528529765000116, 1516.588006113850042, 206.2478870805069846 ) ) ;
#104060 = ORIENTED_EDGE ( 'NONE', *, *, #27771, .T. ) ;
#104061 = DIRECTION ( 'NONE',  ( 0.02616798426359480748, 0.9993150019884422530, -0.02616798426359490809 ) ) ;
#104062 = CARTESIAN_POINT ( 'NONE',  ( 1.530052826864370052, 1452.704406626560058, 183.4894965714629791 ) ) ;
#104063 = CARTESIAN_POINT ( 'NONE',  ( 22.96024162530000368, 1409.741098516330112, 208.8471077697990097 ) ) ;
#104064 = ORIENTED_EDGE ( 'NONE', *, *, #42395, .T. ) ;
#104065 = CARTESIAN_POINT ( 'NONE',  ( 3.117394561335599779, 1508.880976916049804, 204.6292040151590186 ) ) ;
#104066 = CARTESIAN_POINT ( 'NONE',  ( 26.39039547659079687, 1451.532858036890048, 136.1253493193630106 ) ) ;
#104067 = CARTESIAN_POINT ( 'NONE',  ( 16.09743769923632328, 1409.475195298647122, 225.1611831289835379 ) ) ;
#104068 = CARTESIAN_POINT ( 'NONE',  ( -16.33138198470000191, 1386.615434968630098, 200.5875628059090161 ) ) ;
#104069 = CARTESIAN_POINT ( 'NONE',  ( -14.10024896163066188, 1390.294839404160484, 211.8274166821641984 ) ) ;
#104070 = CARTESIAN_POINT ( 'NONE',  ( 18.81211946219999831, 1410.932182625230098, 194.9082043907980051 ) ) ;
#104071 = CARTESIAN_POINT ( 'NONE',  ( 27.73716673060003757, 1444.324653571829003, 175.8274728504979976 ) ) ;
#104072 = CARTESIAN_POINT ( 'NONE',  ( 2.606044709233462875, 1439.644608576006249, 183.4134873266624766 ) ) ;
#104074 = CARTESIAN_POINT ( 'NONE',  ( -19.49500888343222371, 1425.635160192849980, 223.3892665050759945 ) ) ;
#104073 = CARTESIAN_POINT ( 'NONE',  ( 1.103328532679999974, 1417.357629882630135, 234.6276851089980084 ) ) ;
#104075 = CARTESIAN_POINT ( 'NONE',  ( 0.7396591144891080383, 1450.952091773529901, 181.9981990658489792 ) ) ;
#104076 = AXIS2_PLACEMENT_3D ( 'NONE', #32815, #101112, #24408 ) ;
#104077 = FACE_OUTER_BOUND ( 'NONE', #7235, .T. ) ;
#104078 = CARTESIAN_POINT ( 'NONE',  ( -8.834712661419999336, 1383.770682883139898, 218.4951700419789802 ) ) ;
#104079 = CARTESIAN_POINT ( 'NONE',  ( 7.721907888235000073, 1517.026025493960105, 214.1263215447669950 ) ) ;
#104080 = CARTESIAN_POINT ( 'NONE',  ( 2.691689582132314573, 1524.775785348137561, 241.8132190896513407 ) ) ;
#104081 = ORIENTED_EDGE ( 'NONE', *, *, #57074, .T. ) ;
#104082 = CARTESIAN_POINT ( 'NONE',  ( -17.42683798559999886, 1417.851019997039884, 207.0376866630389827 ) ) ;
#104083 = CARTESIAN_POINT ( 'NONE',  ( 19.90023153800532185, 1526.278758871497303, 235.2784539741592198 ) ) ;
#104084 = CARTESIAN_POINT ( 'NONE',  ( -0.5133638609672289688, 1410.311096993930050, 233.1717005261690190 ) ) ;
#104085 = EDGE_CURVE ( 'NONE', #32037, #52548, #78502, .T. ) ;
#104086 = CARTESIAN_POINT ( 'NONE',  ( -9829.078716724869082, 2833.596074015789782, -1083.720023828399917 ) ) ;
#104087 = EDGE_CURVE ( 'NONE', #58183, #44415, #83915, .T. ) ;
#104088 = CARTESIAN_POINT ( 'NONE',  ( 1.182417329582052812, 1421.364694982859646, 193.7605960035091925 ) ) ;
#104089 = ADVANCED_FACE ( 'NONE', ( #7666 ), #33403, .T. ) ;
#104090 = CARTESIAN_POINT ( 'NONE',  ( 0.3175620880625033005, 1506.436298843700342, 231.1045490282727144 ) ) ;
#104091 = VECTOR ( 'NONE', #40762, 1000.000000000000114 ) ;
#104092 = CARTESIAN_POINT ( 'NONE',  ( -20.41675352909999930, 1440.913060387330006, 219.6133834379979817 ) ) ;
#104093 = CARTESIAN_POINT ( 'NONE',  ( 5.319460837823512200, 1475.837047823878947, 266.9611527779425728 ) ) ;
#104094 = ADVANCED_FACE ( 'NONE', ( #83823 ), #16772, .T. ) ;
#104095 = CARTESIAN_POINT ( 'NONE',  ( 11.79714158089999998, 1433.102084680620010, 150.6246159734980097 ) ) ;
#104096 = CARTESIAN_POINT ( 'NONE',  ( 19.02913997099999932, 1445.216574189620133, 214.3676144204279694 ) ) ;
#104098 = EDGE_CURVE ( 'NONE', #92019, #82365, #27432, .T. ) ;
#104097 = CARTESIAN_POINT ( 'NONE',  ( -9.991880054531121047, 1461.400997162919793, 210.8424979650880005 ) ) ;
#104099 = CARTESIAN_POINT ( 'NONE',  ( -17.57139056652149733, 1418.330242804019917, 206.9610443431660087 ) ) ;
#104100 = CARTESIAN_POINT ( 'NONE',  ( 22.81156273903739873, 1507.439214557190098, 209.9480014011130038 ) ) ;
#104101 = CARTESIAN_POINT ( 'NONE',  ( -2.738357795398948635, 1525.795403383247276, 177.3070688927101060 ) ) ;
#104102 = CARTESIAN_POINT ( 'NONE',  ( -12.21452983799999892, 1486.126195478929958, 184.5549420154979998 ) ) ;
#104103 = CARTESIAN_POINT ( 'NONE',  ( 8.704405229141865874, 1398.171440019795000, 199.4642630465137358 ) ) ;
#104104 = CARTESIAN_POINT ( 'NONE',  ( -29.60289517418189931, 1509.946814196759988, 211.8389432164699713 ) ) ;
#104105 = AXIS2_PLACEMENT_3D ( 'NONE', #65822, #107251, #55222 ) ;
#104106 = CARTESIAN_POINT ( 'NONE',  ( 20.10054293860000030, 1449.792076505040086, 223.0884697793979967 ) ) ;
#104107 = DIRECTION ( 'NONE',  ( -1.000000000000000000, 0.000000000000000000, 0.000000000000000000 ) ) ;
#104108 = CARTESIAN_POINT ( 'NONE',  ( -41.66135440509999910, 1443.796918820770088, 135.6885369501979994 ) ) ;
#104109 = CARTESIAN_POINT ( 'NONE',  ( -19.53142348151149932, 1383.854072636070214, 220.5763941096860208 ) ) ;
#104110 = CARTESIAN_POINT ( 'NONE',  ( -13.90059966380340128, 1502.276548245260074, 227.4029733933120099 ) ) ;
#104111 = CARTESIAN_POINT ( 'NONE',  ( 5.784638319815000429, 1516.939574742129935, 213.7356083271170064 ) ) ;
#104112 = ADVANCED_FACE ( 'NONE', ( #42370 ), #107923, .T. ) ;
#104113 = CARTESIAN_POINT ( 'NONE',  ( -14.93837056410000130, 1416.023439710309958, 212.9159407817990086 ) ) ;
#104114 = CARTESIAN_POINT ( 'NONE',  ( 0.1680335629641069861, 1481.486285909129947, 182.0305442892730241 ) ) ;
#104116 = VERTEX_POINT ( 'NONE', #91124 ) ;
#104115 = FACE_OUTER_BOUND ( 'NONE', #8971, .T. ) ;
#104117 = CARTESIAN_POINT ( 'NONE',  ( 6.922360974429970794E-17, 1415.677402202029953, 209.1218459616989946 ) ) ;
#104118 = CARTESIAN_POINT ( 'NONE',  ( -10.11238584568503462, 1389.734820954164434, 201.9902729080233996 ) ) ;
#104119 = CARTESIAN_POINT ( 'NONE',  ( -4.504196618690000875, 1474.524975280490025, 198.6118189482990033 ) ) ;
#104121 = ORIENTED_EDGE ( 'NONE', *, *, #109055, .F. ) ;
#104120 = CARTESIAN_POINT ( 'NONE',  ( -38.71265708134060191, 1449.925712785010091, 134.0999999982089719 ) ) ;
#104122 = CARTESIAN_POINT ( 'NONE',  ( -5.156516201845800396, 1508.551704408389924, 219.6384978436439894 ) ) ;
#104123 = ORIENTED_EDGE ( 'NONE', *, *, #96009, .T. ) ;
#104124 = ADVANCED_FACE ( 'NONE', ( #14400 ), #36633, .F. ) ;
#104125 = CARTESIAN_POINT ( 'NONE',  ( -14.49971677770000156, 1379.923539855790068, 208.5574997035849947 ) ) ;
#104126 = CARTESIAN_POINT ( 'NONE',  ( -16.56387270879999818, 1416.216596894629902, 216.8457408595079983 ) ) ;
#104127 = CARTESIAN_POINT ( 'NONE',  ( -3.289824944146642505, 1509.047015717335171, 238.5027799606278620 ) ) ;
#104128 = EDGE_CURVE ( 'NONE', #40412, #101907, #83840, .T. ) ;
#104129 = CARTESIAN_POINT ( 'NONE',  ( 4.967684734197839624, 1469.890600053420030, 189.7939087450779994 ) ) ;
#104130 = DIRECTION ( 'NONE',  ( 0.9858563016923833633, 0.000000000000000000, 0.1675928173085483863 ) ) ;
#104131 = CARTESIAN_POINT ( 'NONE',  ( -11.06960323243380095, 1471.418000880429872, 206.7781049577790213 ) ) ;
#104132 = CARTESIAN_POINT ( 'NONE',  ( 14.59686494579730009, 1409.422794143049941, 212.2812494645380355 ) ) ;
#104133 = CARTESIAN_POINT ( 'NONE',  ( -10.53295592549999959, 1391.913060387289988, 204.1405351054689845 ) ) ;
#104134 = CARTESIAN_POINT ( 'NONE',  ( -87.47238879921440002, 1385.184608911460145, 290.8447695388430247 ) ) ;
#104135 = CARTESIAN_POINT ( 'NONE',  ( -17.81798938879999739, 1417.753250616630112, 193.2359899303979773 ) ) ;
#104136 = CARTESIAN_POINT ( 'NONE',  ( -32.86470158750949366, 1523.580203803270933, 201.0415738342975089 ) ) ;
#104137 = VERTEX_POINT ( 'NONE', #43494 ) ;
#104138 = EDGE_CURVE ( 'NONE', #75798, #94093, #57091, .T. ) ;
#104139 = CARTESIAN_POINT ( 'NONE',  ( 10.96545847595860046, 1490.902137392429950, 209.8197085273070002 ) ) ;
#104141 = VERTEX_POINT ( 'NONE', #51321 ) ;
#104140 = CARTESIAN_POINT ( 'NONE',  ( -18.46871759262399948, 1509.558002187349757, 227.6992299154879902 ) ) ;
#104142 = CARTESIAN_POINT ( 'NONE',  ( 8.833925975006069464, 1465.118606178020173, 213.5047465619319951 ) ) ;
#104143 = ORIENTED_EDGE ( 'NONE', *, *, #104265, .T. ) ;
#104144 = DIRECTION ( 'NONE',  ( 0.7414773880254614813, -0.000000000000000000, -0.6709778558543786353 ) ) ;
#104145 = CARTESIAN_POINT ( 'NONE',  ( 6.424778925410263852, 1362.739727695628744, 210.6218459617142003 ) ) ;
#104146 = CARTESIAN_POINT ( 'NONE',  ( -11.95607891459999905, 1433.549464727329905, 149.8823818600980076 ) ) ;
#104147 = CARTESIAN_POINT ( 'NONE',  ( 28.81246749003422636, 1509.921441786180822, 215.1936146894269370 ) ) ;
#104148 = CARTESIAN_POINT ( 'NONE',  ( -32.41382812665785451, 1525.581535527370079, 220.2604433702386189 ) ) ;
#104149 = CARTESIAN_POINT ( 'NONE',  ( 2.560697147539999996, 1397.364458149729899, 221.9069322208979997 ) ) ;
#104150 = CARTESIAN_POINT ( 'NONE',  ( 2.158915719780000408, 1417.717804633830156, 234.2951490207980214 ) ) ;
#104151 = DIRECTION ( 'NONE',  ( -1.776356839400250859E-15, 0.000000000000000000, -1.000000000000000000 ) ) ;
#104152 = CARTESIAN_POINT ( 'NONE',  ( -0.5113759145960000696, 1452.167377557530017, 183.2820360629980030 ) ) ;
#104153 = CARTESIAN_POINT ( 'NONE',  ( -8.624710350811819026, 1367.191948709361895, 210.6218459616991936 ) ) ;
#104154 = DIRECTION ( 'NONE',  ( 0.000000000000000000, 0.000000000000000000, 1.000000000000000000 ) ) ;
#104155 = CARTESIAN_POINT ( 'NONE',  ( -16.17567887616449696, 1459.146938910900644, 230.7169172525407532 ) ) ;
#104156 = CARTESIAN_POINT ( 'NONE',  ( 1.701027822874999984, 1516.937508036699910, 206.6270879340970055 ) ) ;
#104157 = B_SPLINE_CURVE_WITH_KNOTS ( 'NONE', 3,
 ( #43967, #94917, #877, #42302, #51823, #44521, #69181, #35002, #86507, #85962, #9802, #78108, #59128, #76455, #18733, #1410, #68631, #102733, #9262, #43421, #1985, #110609, #67529, #51255, #101629, #24918, #59671, #33891, #102199, #25478, #85388, #20940, #55692, #105530, #97668, #28820, #63017, #96576, #61896 ),
 .UNSPECIFIED., .F., .F.,
 ( 4, 2, 2, 1, 1, 1, 1, 2, 2, 2, 2, 1, 1, 1, 1, 2, 2, 2, 2, 1, 1, 1, 2, 2, 4 ),
 ( 0.000000000000000000, 0.1249999999992091604, 0.1874999999988137267, 0.2187499999986127763, 0.2343749999985210719, 0.2421874999984882926, 0.2460937499984814925, 0.2480468749984781063, 0.2499999999984747201, 0.3749999999988570254, 0.4374999999990452637, 0.4687499999991468491, 0.4843749999991899258, 0.4921874999992034705, 0.4960937499992135735, 0.4980468749992186805, 0.4999999999992237321, 0.6249999999993625099, 0.6874999999994277911, 0.7187499999994527711, 0.7343749999994535482, 0.7421874999994576561, 0.7460937499994595434, 0.7499999999994614308, 1.000000000000000000 ),
 .UNSPECIFIED. ) ;
#104158 = DIRECTION ( 'NONE',  ( 0.05030786423734002338, 0.002305672611446700927, 0.9987310962765134636 ) ) ;
#104159 = DIRECTION ( 'NONE',  ( -0.000000000000000000, -1.000000000000000000, -0.000000000000000000 ) ) ;
#104160 = CARTESIAN_POINT ( 'NONE',  ( 40.97060334260000047, 1457.521043316630085, 269.1083649037979626 ) ) ;
#104162 = ORIENTED_EDGE ( 'NONE', *, *, #103476, .F. ) ;
#104161 = CARTESIAN_POINT ( 'NONE',  ( -2.318462068020000100, 1495.571024868690074, 220.0861427028989965 ) ) ;
#104163 = LINE ( 'NONE', #85698, #13363 ) ;
#104164 = VERTEX_POINT ( 'NONE', #87709 ) ;
#104165 = CARTESIAN_POINT ( 'NONE',  ( 19.53786426059019021, 1512.187213306747481, 181.5239794925693388 ) ) ;
#104166 = CARTESIAN_POINT ( 'NONE',  ( -27.39000294650000100, 1488.691910936830027, 208.6711224243079812 ) ) ;
#104168 = CARTESIAN_POINT ( 'NONE',  ( 16.78176103308070211, 1409.746178557840040, 192.6058444741499898 ) ) ;
#104167 = CARTESIAN_POINT ( 'NONE',  ( -10.01040736821559918, 1425.213511949329813, 95.14036416481241076 ) ) ;
#104169 = CARTESIAN_POINT ( 'NONE',  ( 7.724732408895000013, 1517.133889586189980, 212.3822030989969960 ) ) ;
#104170 = B_SPLINE_CURVE_WITH_KNOTS ( 'NONE', 3,
 ( #73334, #39159, #5576, #109149, #49245, #81706, #39726, #32432, #49793, #55988, #5012, #6668, #100714, #90111, #15047, #90666, #13394, #73892, #31867, #100180, #23994, #31315, #65498, #47581, #64945, #108018, #23463, #56538, #15589, #58190, #83926, #74999, #13950, #107468, #92318, #30766, #57657, #99059, #22338, #48139, #99607, #22891, #7228, #57101, #91226, #14506, #48696, #75553, #109687, #91769, #6112, #40269, #74453, #66056, #108580, #34078, #35738, #76091, #43595, #68271, #67704 ),
 .UNSPECIFIED., .F., .F.,
 ( 4, 3, 3, 3, 3, 3, 3, 3, 3, 3, 3, 3, 3, 3, 3, 3, 3, 3, 3, 3, 4 ),
 ( -62.49762447071550042, -60.33300340686220409, -58.10206884789899817, -55.86175009356129806, -53.61759029967220158, -51.36985323930030489, -49.12223441177160055, -46.87661061982559829, -44.63480547542509669, -42.40295230826649941, -40.17980702489999345, -38.04092854621969622, -35.81788295326150262, -33.58648471440059780, -31.35170678149719947, -29.11424439197629965, -26.87748251352680029, -24.64329050055170001, -22.41346991023220170, -20.19442837096610077, -17.98520087693835023 ),
 .UNSPECIFIED. ) ;
#104171 = CARTESIAN_POINT ( 'NONE',  ( -21.31406882940000358, 1471.311257370629846, 207.5959200529579789 ) ) ;
#104172 = B_SPLINE_CURVE_WITH_KNOTS ( 'NONE', 3,
 ( #54149, #94442, #981, #18839, #19956, #70962 ),
 .UNSPECIFIED., .F., .F.,
 ( 4, 2, 4 ),
 ( -1.508484740986450134, -0.7560090653526220228, -0.005718497747917217211 ),
 .UNSPECIFIED. ) ;
#104173 = CARTESIAN_POINT ( 'NONE',  ( -31.95512683309999957, 1438.870446863360030, 244.1805851191980139 ) ) ;
#104174 = CARTESIAN_POINT ( 'NONE',  ( 16.01892750471949611, 1509.475672623540049, 233.8163314141949911 ) ) ;
#104175 = DIRECTION ( 'NONE',  ( -0.7414773880254711402, 0.000000000000000000, -0.6709778558543678662 ) ) ;
#104176 = CARTESIAN_POINT ( 'NONE',  ( -5.249808435119999395, 1391.918258567789962, 214.5638896842290251 ) ) ;
#104177 = CARTESIAN_POINT ( 'NONE',  ( 30.81588940880000038, 1451.836835031929922, 135.2403377932980106 ) ) ;
#104178 = VERTEX_POINT ( 'NONE', #102271 ) ;
#104179 = CARTESIAN_POINT ( 'NONE',  ( 6.240881287431440327, 1397.787785794319916, 220.5258607916529741 ) ) ;
#104180 = CARTESIAN_POINT ( 'NONE',  ( 9.611691241550468945, 1460.529588664869834, 206.0549884057099916 ) ) ;
#104181 = CARTESIAN_POINT ( 'NONE',  ( -16.96763829480000041, 1458.557240647530080, 230.2736757858980354 ) ) ;
#104182 = ORIENTED_EDGE ( 'NONE', *, *, #99531, .T. ) ;
#104183 = EDGE_LOOP ( 'NONE', ( #110129, #15132, #20146, #22708 ) ) ;
#104184 = B_SPLINE_CURVE_WITH_KNOTS ( 'NONE', 5,
 ( #29676, #30778, #100194, #91783, #65511, #81178, #22905, #15060, #56000 ),
 .UNSPECIFIED., .F., .F.,
 ( 6, 3, 6 ),
 ( 0.000000000000000000, 0.5456913010464850000, 1.000000000000000000 ),
 .UNSPECIFIED. ) ;
#104185 = CARTESIAN_POINT ( 'NONE',  ( -29.24402035022065505, 1509.934316807730966, 211.7409440427389882 ) ) ;
#104186 = CARTESIAN_POINT ( 'NONE',  ( -3.199225686647339639, 1428.849802092149957, 155.3746640963260006 ) ) ;
#104187 = EDGE_CURVE ( 'NONE', #2114, #33795, #87457, .T. ) ;
#104188 = EDGE_LOOP ( 'NONE', ( #54281, #47428, #81576, #74634 ) ) ;
#104189 = CARTESIAN_POINT ( 'NONE',  ( -1.365868668549999887, 1417.499497643730137, 185.3003514764980082 ) ) ;
#104190 = CARTESIAN_POINT ( 'NONE',  ( -5.924352395060029863, 1419.506400887321433, 194.9066959792404532 ) ) ;
#104191 = DIRECTION ( 'NONE',  ( 0.9417419115949053898, -0.3363363969979660806, -9.559255346349042767E-16 ) ) ;
#104192 = CARTESIAN_POINT ( 'NONE',  ( 12.47681624269289280, 1420.546772247846320, 200.4723319259569791 ) ) ;
#104193 = CARTESIAN_POINT ( 'NONE',  ( 1.422913744236389944, 1420.921243867379872, 183.0214009822149990 ) ) ;
#104194 = CARTESIAN_POINT ( 'NONE',  ( 10.40178565224220009, 1451.751389650100009, 207.5054792126090035 ) ) ;
#104195 = CARTESIAN_POINT ( 'NONE',  ( -3.337824073649999779, 1502.591014432890006, 230.2741237628989950 ) ) ;
#104196 = DIRECTION ( 'NONE',  ( -0.000000000000000000, -1.000000000000000000, -0.000000000000000000 ) ) ;
#104197 = ORIENTED_EDGE ( 'NONE', *, *, #9459, .T. ) ;
#104198 = CARTESIAN_POINT ( 'NONE',  ( 5.777745395274999751, 1516.908489800550115, 202.5639360494670029 ) ) ;
#104199 = CARTESIAN_POINT ( 'NONE',  ( 3.462835627365000057, 1517.038650117239968, 210.2415636864969883 ) ) ;
#104200 = ORIENTED_EDGE ( 'NONE', *, *, #109177, .T. ) ;
#104201 = CARTESIAN_POINT ( 'NONE',  ( 11.86589750230659845, 1432.321833896879980, 149.9823969317070009 ) ) ;
#104202 = EDGE_CURVE ( 'NONE', #41641, #52311, #11401, .T. ) ;
#104203 = CARTESIAN_POINT ( 'NONE',  ( 13.21142979970633391, 1444.695576628558683, 187.3344715631244242 ) ) ;
#104204 = EDGE_LOOP ( 'NONE', ( #105236, #69464, #28707, #72570 ) ) ;
#104205 = DIRECTION ( 'NONE',  ( 5.980589973904019347E-17, -1.000000000000000000, 1.736889445713099699E-16 ) ) ;
#104206 = CARTESIAN_POINT ( 'NONE',  ( -7.144831657780449596, 1508.449369756350052, 219.6178892270350218 ) ) ;
#104207 = CARTESIAN_POINT ( 'NONE',  ( 2.879160622090000121, 1507.714518183930068, 236.0305531890979864 ) ) ;
#104208 = CARTESIAN_POINT ( 'NONE',  ( -9.489078762094210973, 1470.877762335149782, 213.0725583738820035 ) ) ;
#104209 = CARTESIAN_POINT ( 'NONE',  ( -4.746199047880000244, 1421.572606312730159, 185.9709308222979871 ) ) ;
#104210 = CARTESIAN_POINT ( 'NONE',  ( 4.101683555128318837, 1410.534017730810092, 269.3367430748480160 ) ) ;
#104211 = CARTESIAN_POINT ( 'NONE',  ( 9.146237114798470458, 1449.998848199699978, 208.1168068718100130 ) ) ;
#104212 = CARTESIAN_POINT ( 'NONE',  ( -109.9438493645591990, 1383.878411725401293, 297.0368449378275386 ) ) ;
#104213 = CARTESIAN_POINT ( 'NONE',  ( -2.457346683533450094, 1422.331128196689860, 192.7387433577370075 ) ) ;
#104214 = CARTESIAN_POINT ( 'NONE',  ( -16.47481425009999967, 1379.657961281789767, 208.5229944698799898 ) ) ;
#104215 = CARTESIAN_POINT ( 'NONE',  ( 8.332319144487495777, 1424.430118509189697, 195.7440745982989654 ) ) ;
#104217 = CARTESIAN_POINT ( 'NONE',  ( 9.887881744141459706, 1469.108246522290074, 203.7125116724459986 ) ) ;
#104216 = CARTESIAN_POINT ( 'NONE',  ( -13.48450404919999990, 1503.201074756489788, 208.7146732095060031 ) ) ;
#104218 = CARTESIAN_POINT ( 'NONE',  ( -68.50706126866759860, 1379.747743051572343, 280.0840774304766683 ) ) ;
#104219 = CARTESIAN_POINT ( 'NONE',  ( 17.86527779738699806, 1419.284960752339884, 225.0523055677910236 ) ) ;
#104220 = B_SPLINE_CURVE_WITH_KNOTS ( 'NONE', 3,
 ( #38685, #73412, #98038, #72860 ),
 .UNSPECIFIED., .F., .F.,
 ( 4, 4 ),
 ( 0.000000000000000000, 0.0002960034161023847310 ),
 .UNSPECIFIED. ) ;
#104221 = CARTESIAN_POINT ( 'NONE',  ( -4.644703737721179060, 1496.617562890359977, 216.2902365695769902 ) ) ;
#104222 = VERTEX_POINT ( 'NONE', #96086 ) ;
#104223 = CARTESIAN_POINT ( 'NONE',  ( 6.850948851990000144, 1425.447270609629868, 224.8635561661979807 ) ) ;
#104224 = CARTESIAN_POINT ( 'NONE',  ( 22.62861454470000311, 1507.212883763329955, 209.7205631874760172 ) ) ;
#104225 = CARTESIAN_POINT ( 'NONE',  ( -18.40343465886419949, 1525.402221411349274, 179.8532301504590407 ) ) ;
#104226 = EDGE_CURVE ( 'NONE', #33840, #35724, #76829, .T. ) ;
#104227 = DIRECTION ( 'NONE',  ( 0.000000000000000000, 1.000000000000000000, 0.000000000000000000 ) ) ;
#104228 = CARTESIAN_POINT ( 'NONE',  ( -14.37783120989999830, 1415.677402202029953, 213.0868688017489774 ) ) ;
#104230 = ORIENTED_EDGE ( 'NONE', *, *, #120, .F. ) ;
#104229 = CARTESIAN_POINT ( 'NONE',  ( 0.9886889294276358653, 1515.109643008290050, 204.7935716275389950 ) ) ;
#104231 = DIRECTION ( 'NONE',  ( -0.000000000000000000, -1.000000000000000000, -0.000000000000000000 ) ) ;
#104232 = CARTESIAN_POINT ( 'NONE',  ( -24.68922764939999936, 1444.388416874039876, 210.7939770334679963 ) ) ;
#104233 = EDGE_CURVE ( 'NONE', #2577, #32822, #14139, .T. ) ;
#104234 = CARTESIAN_POINT ( 'NONE',  ( -1.251355130419650408, 1450.749714363028261, 154.2555256373233590 ) ) ;
#104235 = CARTESIAN_POINT ( 'NONE',  ( 0.3255681544576509712, 1547.051704408389924, 210.0673645372983174 ) ) ;
#104236 = CARTESIAN_POINT ( 'NONE',  ( 11.75640697503499865, 1511.791180387469922, 224.3022927925669876 ) ) ;
#104237 = CARTESIAN_POINT ( 'NONE',  ( 5.369951645833737963, 1422.353275737341164, 139.3006397450932070 ) ) ;
#104238 = CARTESIAN_POINT ( 'NONE',  ( 14.24650394540639908, 1509.423839838560298, 235.0732898097659813 ) ) ;
#104239 = LINE ( 'NONE', #28077, #52077 ) ;
#104240 = CARTESIAN_POINT ( 'NONE',  ( -12.54268436849999979, 1408.913060387329779, 221.6645303301980050 ) ) ;
#104241 = CARTESIAN_POINT ( 'NONE',  ( 14.50036989130000009, 1415.083979989329919, 227.9808212963979770 ) ) ;
#104242 = EDGE_CURVE ( 'NONE', #104222, #9164, #29420, .T. ) ;
#104243 = CARTESIAN_POINT ( 'NONE',  ( -10.89975107439999924, 1480.485161721690019, 212.5137882077189886 ) ) ;
#104244 = CARTESIAN_POINT ( 'NONE',  ( -16.50128791789999738, 1460.031619852429912, 228.4944370095979878 ) ) ;
#104245 = CARTESIAN_POINT ( 'NONE',  ( -5.787477032644999575, 1517.070197312179971, 206.2521524731670013 ) ) ;
#104246 = CARTESIAN_POINT ( 'NONE',  ( 46.15245612160000377, 1438.899492667230106, 268.2044261578979558 ) ) ;
#104247 = CARTESIAN_POINT ( 'NONE',  ( -32.36284091028927890, 1525.878013734321257, 218.9814869512302096 ) ) ;
#104248 = CARTESIAN_POINT ( 'NONE',  ( -21.38516915557943321, 1522.382868172863937, 237.8497028174240313 ) ) ;
#104249 = CARTESIAN_POINT ( 'NONE',  ( 18.93814215579999782, 1469.163538426630112, 190.4333472056979986 ) ) ;
#104250 = EDGE_CURVE ( 'NONE', #43874, #94269, #85928, .T. ) ;
#104251 = CARTESIAN_POINT ( 'NONE',  ( -22.98928886499999891, 1433.123621001740048, 215.0581590339280069 ) ) ;
#104252 = CARTESIAN_POINT ( 'NONE',  ( -12.28856626983460032, 1377.626870450839988, 208.3294650349379822 ) ) ;
#104253 = CARTESIAN_POINT ( 'NONE',  ( -15.68560381450000207, 1410.853898355630008, 226.7268320013979803 ) ) ;
#104254 = CARTESIAN_POINT ( 'NONE',  ( -11.41402561306639996, 1500.969831351809944, 208.5831151434670119 ) ) ;
#104255 = CARTESIAN_POINT ( 'NONE',  ( -1.403723453710000069, 1451.693831228530144, 183.8452497173979907 ) ) ;
#104256 = CARTESIAN_POINT ( 'NONE',  ( -22.91663120903140083, 1507.606285602550088, 207.6071078552859888 ) ) ;
#104257 = CARTESIAN_POINT ( 'NONE',  ( -16.31919663280000066, 1416.362649511440168, 209.6296053043620020 ) ) ;
#104258 = CARTESIAN_POINT ( 'NONE',  ( -12.57157822410000136, 1441.286360236680139, 188.0308888572979811 ) ) ;
#104259 = CARTESIAN_POINT ( 'NONE',  ( -7.557748306139269623, 1384.394157022499940, 219.0612169397370224 ) ) ;
#104260 = CARTESIAN_POINT ( 'NONE',  ( -29.17524271230000110, 1436.412047157749839, 136.6555645778979908 ) ) ;
#104261 = DIRECTION ( 'NONE',  ( 0.4978433412588781914, 0.000000000000000000, 0.8672669759446606230 ) ) ;
#104262 = ORIENTED_EDGE ( 'NONE', *, *, #44206, .T. ) ;
#104263 = CARTESIAN_POINT ( 'NONE',  ( 5.650234563753527617, 1510.510563522158918, 216.6707982693055499 ) ) ;
#104264 = CARTESIAN_POINT ( 'NONE',  ( -14.35947579292080079, 1409.414504331519765, 213.2202510431029907 ) ) ;
#104265 = EDGE_CURVE ( 'NONE', #75704, #71877, #49288, .T. ) ;
#104266 = CARTESIAN_POINT ( 'NONE',  ( 29.86461515634908892, 1525.960063244516959, 197.2746849027934957 ) ) ;
#104267 = CARTESIAN_POINT ( 'NONE',  ( 2.375285482014719999E-15, 1391.913060387289988, 209.1218459572589836 ) ) ;
#104268 = CARTESIAN_POINT ( 'NONE',  ( -46.27885839279999658, 1446.077177910260161, 267.5894350431979660 ) ) ;
#104269 = CARTESIAN_POINT ( 'NONE',  ( -4.987078454554999318, 1508.551704408389924, 205.6342535004969818 ) ) ;
#104270 = CARTESIAN_POINT ( 'NONE',  ( 0.1825647296195060110, 1419.920266353400166, 184.0904206890710100 ) ) ;
#104271 = EDGE_CURVE ( 'NONE', #93687, #76760, #43320, .T. ) ;
#104272 = CARTESIAN_POINT ( 'NONE',  ( -26.71144765010000199, 1509.845844693529898, 221.0617760641979999 ) ) ;
#104273 = CARTESIAN_POINT ( 'NONE',  ( -62.63025033776229122, 1384.685893630349938, 285.2374344412770029 ) ) ;
#104274 = B_SPLINE_SURFACE_WITH_KNOTS ( 'NONE', 5, 5, ( 
 ( #12393, #28657, #72330, #102710, #71244, #60770, #17037, #54439, #62862 ),
 ( #88572, #69160, #11855, #60202, #51234, #46028, #94894, #8662, #80156 ),
 ( #3477, #71807, #18169, #105927, #94321, #42840, #29206, #43398, #63395 ),
 ( #852, #34979, #86484, #43946, #78089, #1392, #20780, #54980, #89105 ),
 ( #5660, #55523, #72868, #98045, #48222, #64484, #89650, #56616, #49319 ),
 ( #15129, #82362, #107556, #12936, #38692, #47117, #73420, #107003, #83445 ),
 ( #82903, #39808, #30291, #31395, #23543, #21319, #22413, #91853, #108099 ),
 ( #65575, #65018, #22979, #98599, #99136, #73968, #81244, #21863, #90751 ),
 ( #56062, #4559, #90189, #40347, #47663, #13473, #81790, #14590, #5093 ),
 ( #14030, #57735, #30842, #99687, #39246, #57184, #91308, #48778, #6195 ),
 ( #40898, #74528, #6740, #106460, #108659, #29744, #31947, #66141, #100264 ),
 ( #63932, #94605, #34157, #17881, #52079, #24081, #75079, #84004, #68343 ),
 ( #25183, #93497, #59937, #67778, #59386, #94054, #43122, #102449, #33585 ),
 ( #92954, #85101, #77281, #84556, #92393, #101890, #58270, #101329, #60485 ),
 ( #86211, #15666, #75630, #16768, #8390, #49870, #41470, #66684, #50971 ) ),
 .UNSPECIFIED., .F., .F., .F.,
 ( 6, 3, 3, 3, 6 ),
 ( 6, 3, 6 ),
 ( 25.13132725520000221, 26.41639650289999963, 27.94257249489999850, 28.70566049089999794, 29.46874848689999737 ),
 ( 0.000000000000000000, 1.000000000000000000, 2.000000000000000000 ),
 .UNSPECIFIED. ) ;
#104275 = CARTESIAN_POINT ( 'NONE',  ( -18.05670876470880160, 1384.947303455109932, 201.1907562702159851 ) ) ;
#104276 = CARTESIAN_POINT ( 'NONE',  ( 17.59745923480189944, 1424.099926364739986, 226.7452899292189841 ) ) ;
#104277 = CARTESIAN_POINT ( 'NONE',  ( 12.18581598819999989, 1415.088016306429836, 220.9247494550979809 ) ) ;
#104278 = CARTESIAN_POINT ( 'NONE',  ( 14.55732100150000008, 1474.168784421129885, 223.9170786068980021 ) ) ;
#104279 = CARTESIAN_POINT ( 'NONE',  ( -25.96374710035300026, 1482.712064823979972, 211.2547906125309964 ) ) ;
#104280 = DIRECTION ( 'NONE',  ( 0.4436356471204840890, 0.000000000000000000, 0.8962072375315819350 ) ) ;
#104281 = FACE_OUTER_BOUND ( 'NONE', #91381, .T. ) ;
#104282 = CARTESIAN_POINT ( 'NONE',  ( -22.74730998069999544, 1409.707413955830134, 207.2976303262279885 ) ) ;
#104283 = CARTESIAN_POINT ( 'NONE',  ( 17.97082668629999702, 1416.218047894730262, 208.7667250827289820 ) ) ;
#104284 = FACE_OUTER_BOUND ( 'NONE', #17264, .T. ) ;
#104285 = CARTESIAN_POINT ( 'NONE',  ( 11.74549576979310039, 1479.261940693859970, 208.3477357056440269 ) ) ;
#104286 = CARTESIAN_POINT ( 'NONE',  ( -106.4029571836669987, 1391.913060387289988, 304.3198526369590127 ) ) ;
#104287 = CARTESIAN_POINT ( 'NONE',  ( 10.60563969924810124, 1451.919000108789987, 190.2093396595549848 ) ) ;
#104288 = CARTESIAN_POINT ( 'NONE',  ( -7.260542987912549151, 1508.878901734200099, 215.8879478474800067 ) ) ;
#104289 = B_SPLINE_SURFACE_WITH_KNOTS ( 'NONE', 5, 5, ( 
 ( #48755, #100765, #22954, #31924, #48198, #5636, #82336, #108636, #108076 ),
 ( #41444, #109739, #82878, #33020, #66662, #83425, #22392, #100239, #58792 ),
 ( #40877, #75056, #23519, #24054, #58248, #64997, #39786, #67207, #31371 ),
 ( #65554, #99664, #91828, #101305, #24599, #92931, #50408, #91284, #57712 ),
 ( #6172, #7821, #92371, #73395, #30821, #15643, #15106, #49298, #6721 ),
 ( #109205, #17296, #8366, #1659, #86190, #8922, #17855, #85074, #53162 ),
 ( #87304, #51492, #42534, #52608, #94032, #34132, #77799, #69980, #103537 ),
 ( #86744, #76687, #68871, #76141, #93472, #102973, #9482, #25159, #59363 ),
 ( #22586, #94579, #77258, #95150, #26271, #61027, #95700, #67755, #43097 ),
 ( #10036, #85623, #35236, #60461, #43646, #52055, #68320, #1109, #102428 ),
 ( #69424, #26840, #104096, #110285, #41991, #18410, #33561, #44207, #78350 ),
 ( #25711, #35796, #27387, #61566, #18967, #101866, #16742, #557, #50949 ) ),
 .UNSPECIFIED., .F., .F., .F.,
 ( 6, 3, 3, 6 ),
 ( 6, 3, 6 ),
 ( 0.000000000000000000, 17.84603210599999912, 40.51038747020000130, 67.03953034199999195 ),
 ( -7.105427357600000794E-15, 42.18180435250000215, 84.36360870500000431 ),
 .UNSPECIFIED. ) ;
#104290 = CARTESIAN_POINT ( 'NONE',  ( -5.385728839570650628, 1432.176526655569887, 154.6052246632760045 ) ) ;
#104292 = CARTESIAN_POINT ( 'NONE',  ( -8.672272362719999350, 1384.150546597180210, 199.9472511214389954 ) ) ;
#104291 = DIRECTION ( 'NONE',  ( 1.755985294532464991E-16, -1.000000000000000000, 1.338183447452830017E-16 ) ) ;
#104293 = CARTESIAN_POINT ( 'NONE',  ( -4.994701126379999856, 1391.710704567790117, 203.7548416175590091 ) ) ;
#104294 = FACE_OUTER_BOUND ( 'NONE', #82920, .T. ) ;
#104295 = CARTESIAN_POINT ( 'NONE',  ( -11.37189650340000213, 1489.740153703190117, 212.1629306840389972 ) ) ;
#104296 = CARTESIAN_POINT ( 'NONE',  ( -23.76631617309999811, 1425.856202520030138, 210.9077545568479763 ) ) ;
#104297 = CARTESIAN_POINT ( 'NONE',  ( -2.109090801651389846, 1421.166307101949997, 183.8085686438699895 ) ) ;
#104298 = CARTESIAN_POINT ( 'NONE',  ( -5.008848238024999233, 1516.858456333729919, 204.1217621043670079 ) ) ;
#104299 = CARTESIAN_POINT ( 'NONE',  ( -3.565162963136402574, 1440.799174861838537, 156.6581779582986087 ) ) ;
#104300 = CARTESIAN_POINT ( 'NONE',  ( -18.68342712143339668, 1486.059792560550022, 189.1570398102469994 ) ) ;
#104301 = CARTESIAN_POINT ( 'NONE',  ( 1.415932851160000006, 1507.678098756430018, 236.8296152846979794 ) ) ;
#104302 = CARTESIAN_POINT ( 'NONE',  ( 41.39120048966680088, 1446.191622651899934, 135.3419589341729932 ) ) ;
#104304 = EDGE_LOOP ( 'NONE', ( #59877, #61262, #80890, #11248 ) ) ;
#104303 = CARTESIAN_POINT ( 'NONE',  ( -59.60612636626729710, 1379.726987694469926, 264.7824669088110454 ) ) ;
#104305 = ORIENTED_EDGE ( 'NONE', *, *, #93379, .T. ) ;
#104306 = CARTESIAN_POINT ( 'NONE',  ( 11.96031942147230076, 1433.620261006660030, 150.1736231411599647 ) ) ;
#104307 = CARTESIAN_POINT ( 'NONE',  ( -21.03123196678649975, 1507.789098018889945, 192.1781278620359785 ) ) ;
#104308 = VERTEX_POINT ( 'NONE', #41434 ) ;
#104309 = DIRECTION ( 'NONE',  ( -1.755985294532469921E-16, 1.000000000000000000, -1.338183447452831989E-16 ) ) ;
#104310 = CARTESIAN_POINT ( 'NONE',  ( -109.3078499810000039, 1384.937516855040030, 311.2645914332589427 ) ) ;
#104312 = CARTESIAN_POINT ( 'NONE',  ( -0.1372456665499999784, 1508.561285218730063, 180.3391500124980098 ) ) ;
#104311 = CARTESIAN_POINT ( 'NONE',  ( 9.042313521169999646, 1416.851343894929869, 218.1641597260979779 ) ) ;
#104313 = DIRECTION ( 'NONE',  ( -0.7384854939282339270, 0.000000000000000000, 0.6742693640212139572 ) ) ;
#104314 = CARTESIAN_POINT ( 'NONE',  ( -23.92105762916159861, 1452.077756819290016, 137.0200261151539962 ) ) ;
#104315 = CARTESIAN_POINT ( 'NONE',  ( -105.7942479044789934, 1378.913060387259975, 304.2294709827049815 ) ) ;
#104316 = CARTESIAN_POINT ( 'NONE',  ( 16.66255704860000009, 1410.427173532229972, 226.4839786049979864 ) ) ;
#104317 = CARTESIAN_POINT ( 'NONE',  ( 2.492443650904999863, 1516.793978928989873, 212.3737347995770222 ) ) ;
#104318 = CARTESIAN_POINT ( 'NONE',  ( 38.36650730338939752, 1437.217469518439884, 134.0999999970779868 ) ) ;
#104319 = CARTESIAN_POINT ( 'NONE',  ( -7.547148334389939706, 1424.043885779579796, 208.8816623809889848 ) ) ;
#104320 = CARTESIAN_POINT ( 'NONE',  ( 18.53437515553029868, 1509.560294966549918, 227.6602647230590151 ) ) ;
#104321 = ORIENTED_EDGE ( 'NONE', *, *, #12130, .F. ) ;
#104322 = CARTESIAN_POINT ( 'NONE',  ( 13.76875196565650050, 1434.979433280920148, 148.6886221399630017 ) ) ;
#104323 = CARTESIAN_POINT ( 'NONE',  ( -6.312270842414640093, 1439.251699911259948, 226.7179307010800073 ) ) ;
#104324 = ORIENTED_EDGE ( 'NONE', *, *, #21536, .F. ) ;
#104325 = ORIENTED_EDGE ( 'NONE', *, *, #108950, .F. ) ;
#104326 = ORIENTED_EDGE ( 'NONE', *, *, #99663, .T. ) ;
#104327 = CARTESIAN_POINT ( 'NONE',  ( -7.538480533405000017, 1511.326779185850000, 215.2911934950269881 ) ) ;
#104328 = CARTESIAN_POINT ( 'NONE',  ( -0.7017359387820000238, 1466.348790855930019, 235.5986157078980057 ) ) ;
#104329 = EDGE_CURVE ( 'NONE', #110178, #50084, #12556, .T. ) ;
#104330 = CARTESIAN_POINT ( 'NONE',  ( 21.07099741623147438, 1450.946020818080342, 144.3761871749956640 ) ) ;
#104331 = DIRECTION ( 'NONE',  ( 0.000000000000000000, 1.000000000000000000, 0.000000000000000000 ) ) ;
#104332 = CARTESIAN_POINT ( 'NONE',  ( 0.4668132112965759917, 1465.514551817379925, 198.1226951640539937 ) ) ;
#104333 = CARTESIAN_POINT ( 'NONE',  ( -19.01838096944922540, 1443.067311164506009, 211.2996751566819569 ) ) ;
#104334 = CARTESIAN_POINT ( 'NONE',  ( -58.69971502816261477, 1379.720317519436549, 258.4395855553975707 ) ) ;
#104335 = CARTESIAN_POINT ( 'NONE',  ( 4.221567158387570018, 1446.221985844579876, 169.5782296013129837 ) ) ;
#104336 =( BOUNDED_SURFACE ( )  B_SPLINE_SURFACE ( 3, 2, ( 
 ( #40889, #57176, #57725 ),
 ( #67223, #24070, #84546 ),
 ( #40339, #75071, #41458 ),
 ( #66675, #8380, #33033 ),
 ( #73961, #91843, #83995 ),
 ( #42004, #109219, #109755 ),
 ( #92384, #15121, #7835 ),
 ( #76152, #101321, #101881 ),
 ( #32505, #100779, #59376 ),
 ( #108091, #83437, #108651 ) ),
 .UNSPECIFIED., .F., .F., .F. ) 
 B_SPLINE_SURFACE_WITH_KNOTS ( ( 4, 2, 2, 2, 4 ),
 ( 3, 3 ),
 ( 1.570796326794896558, 1.963495408493620697, 2.356194490192344837, 2.748893571891068976, 3.141592653589793116 ),
 ( 0.000000000000000000, 1.000000000000000000 ),
 .UNSPECIFIED. ) 
 GEOMETRIC_REPRESENTATION_ITEM ( )  RATIONAL_B_SPLINE_SURFACE ( (
 ( 1.000000000000000000, 0.7071067811865857644, 1.000000000000000000),
 ( 1.000000000000000000, 0.7166207884818905915, 1.000000000000000000),
 ( 1.000000000000000000, 0.7259222650911381081, 1.000000000000000000),
 ( 1.000000000000000000, 0.7428408967926047879, 1.000000000000000000),
 ( 1.000000000000000000, 0.7504512394524444074, 1.000000000000000000),
 ( 1.000000000000000000, 0.7630177051950547407, 1.000000000000000000),
 ( 1.000000000000000000, 0.7679730451973306726, 1.000000000000000000),
 ( 1.000000000000000000, 0.7746454561797161409, 1.000000000000000000),
 ( 1.000000000000000000, 0.7763684247035325114, 1.000000000000000000),
 ( 1.000000000000000000, 0.7763623250684303922, 1.000000000000000000) ) ) 
 REPRESENTATION_ITEM ( '' )  SURFACE ( )  );
#104337 = CARTESIAN_POINT ( 'NONE',  ( 0.4361291165900000322, 1508.823583087030102, 238.3913694569979782 ) ) ;
#104338 = ORIENTED_EDGE ( 'NONE', *, *, #24961, .F. ) ;
#104339 = CARTESIAN_POINT ( 'NONE',  ( -7.724732447025000504, 1517.133889586189980, 205.8614888033369823 ) ) ;
#104340 = EDGE_LOOP ( 'NONE', ( #56793, #110624, #84630, #6963 ) ) ;
#104341 = CARTESIAN_POINT ( 'NONE',  ( 33.01805644497149927, 1440.913060387330006, 257.7170065347000332 ) ) ;
#104342 = EDGE_CURVE ( 'NONE', #73262, #58610, #8773, .T. ) ;
#104343 = CARTESIAN_POINT ( 'NONE',  ( -15.09146821900000113, 1507.698585867829934, 185.0194906632980008 ) ) ;
#104344 = ORIENTED_EDGE ( 'NONE', *, *, #28225, .F. ) ;
#104345 = CARTESIAN_POINT ( 'NONE',  ( -7.266089503534879590, 1509.032013814719903, 202.3522253410079941 ) ) ;
#104346 = CARTESIAN_POINT ( 'NONE',  ( -14.94350077410000033, 1410.807377667530091, 190.7174140115980094 ) ) ;
#104347 = CARTESIAN_POINT ( 'NONE',  ( -46.84911848401252144, 1379.681085501543976, 239.8728125796529298 ) ) ;
#104348 = CARTESIAN_POINT ( 'NONE',  ( -24.38264615309999783, 1441.634144454579882, 211.3700308316280143 ) ) ;
#104349 = CARTESIAN_POINT ( 'NONE',  ( -3.955240613149759721, 1433.657955356159846, 217.8573778194910062 ) ) ;
#104350 = CARTESIAN_POINT ( 'NONE',  ( 0.0002665247232048016256, 1396.263874589266152, 196.9886544196637885 ) ) ;
#104351 = CARTESIAN_POINT ( 'NONE',  ( -11.87563350447849864, 1433.006677213540115, 147.6591432354780125 ) ) ;
#104352 = CARTESIAN_POINT ( 'NONE',  ( -27.68841619517039732, 1441.378412040929788, 137.2953534901809860 ) ) ;
#104354 = CARTESIAN_POINT ( 'NONE',  ( 8.091207885150058843, 1435.785749346069906, 206.2618432467970138 ) ) ;
#104353 = CARTESIAN_POINT ( 'NONE',  ( 2.902322711624676882E-15, 1518.913060387330006, 232.8211094035767985 ) ) ;
#104355 = CARTESIAN_POINT ( 'NONE',  ( -6.937965698444999774, 1516.732530461250008, 214.1275461716370216 ) ) ;
#104356 = CARTESIAN_POINT ( 'NONE',  ( -2.356903266504112082, 1525.394057003702756, 241.9297787646439417 ) ) ;
#104357 = CARTESIAN_POINT ( 'NONE',  ( 6.127742252161359815, 1511.645100227929788, 217.9168819886610038 ) ) ;
#104358 = CARTESIAN_POINT ( 'NONE',  ( 28.04637368570000078, 1508.608406896529914, 208.0794640871779677 ) ) ;
#104359 = CARTESIAN_POINT ( 'NONE',  ( -3.446942109845000157, 1516.842852731759876, 212.3891375753969726 ) ) ;
#104360 = CARTESIAN_POINT ( 'NONE',  ( -11.61827763164220073, 1482.582230581700060, 206.5199852600759982 ) ) ;
#104361 = CARTESIAN_POINT ( 'NONE',  ( -18.14031316878698163, 1486.179785434160522, 188.5896102339170284 ) ) ;
#104363 = ORIENTED_EDGE ( 'NONE', *, *, #55112, .T. ) ;
#104362 = CARTESIAN_POINT ( 'NONE',  ( -87.55914429599999949, 1389.463764338810051, 294.7984051320589742 ) ) ;
#104364 = CARTESIAN_POINT ( 'NONE',  ( -16.50400130224727135, 1525.907212628473872, 236.2546788475582105 ) ) ;
#104365 = CARTESIAN_POINT ( 'NONE',  ( 27.17992431449999913, 1457.024587824730133, 248.2870168946980129 ) ) ;
#104366 = EDGE_CURVE ( 'NONE', #36878, #15971, #100231, .T. ) ;
#104367 = CARTESIAN_POINT ( 'NONE',  ( 30.37359097063835733, 1526.143142182266274, 216.9284661788419442 ) ) ;
#104368 = CARTESIAN_POINT ( 'NONE',  ( -11.84242369139999873, 1431.324257919750153, 147.6543138610979895 ) ) ;
#104369 = CARTESIAN_POINT ( 'NONE',  ( -7.338679992370000349, 1507.281025754529992, 235.5381382512980224 ) ) ;
#104370 = EDGE_CURVE ( 'NONE', #109192, #36569, #53498, .T. ) ;
#104371 = CARTESIAN_POINT ( 'NONE',  ( -19.02557409639999975, 1456.564017630530088, 227.5201806683979839 ) ) ;
#104372 = EDGE_CURVE ( 'NONE', #38904, #57731, #101977, .T. ) ;
#104374 = CARTESIAN_POINT ( 'NONE',  ( 19.74623141760000067, 1455.440022657330019, 226.3245780267980081 ) ) ;
#104373 = CARTESIAN_POINT ( 'NONE',  ( -17.99954540876850118, 1410.904693920620048, 195.2564682659330231 ) ) ;
#104375 = CARTESIAN_POINT ( 'NONE',  ( -8.931373544893890681, 1449.107262902880166, 211.1739995703599959 ) ) ;
#104376 = CARTESIAN_POINT ( 'NONE',  ( -105.4614100663400080, 1378.948680768060058, 305.4850396033990023 ) ) ;
#104377 = ORIENTED_EDGE ( 'NONE', *, *, #104518, .T. ) ;
#104378 = CARTESIAN_POINT ( 'NONE',  ( 1.705466410464999916, 1517.120861839400050, 204.1076508302870138 ) ) ;
#104379 = CARTESIAN_POINT ( 'NONE',  ( -9.242820708772759630, 1508.434507021560194, 219.0621371396210009 ) ) ;
#104380 = DIRECTION ( 'NONE',  ( -0.2054769195713184726, -5.792241587466808811E-16, -0.9786619618251657382 ) ) ;
#104381 = ADVANCED_FACE ( 'NONE', ( #549 ), #43639, .F. ) ;
#104382 = CARTESIAN_POINT ( 'NONE',  ( 40.06163307034069732, 1457.034817765570097, 269.9895890114499934 ) ) ;
#104383 = CARTESIAN_POINT ( 'NONE',  ( 5.414082080120000917, 1435.477060051989838, 154.6761060569980089 ) ) ;
#104384 = CARTESIAN_POINT ( 'NONE',  ( -39.67220881037469837, 1448.134517022349883, 136.4399726006329843 ) ) ;
#104385 = CARTESIAN_POINT ( 'NONE',  ( 17.70437741359999961, 1453.580057579390086, 200.5051001409389926 ) ) ;
#104386 = B_SPLINE_CURVE_WITH_KNOTS ( 'NONE', 5,
 ( #98463, #54296, #38021, #97364, #82213, #71671 ),
 .UNSPECIFIED., .F., .F.,
 ( 6, 6 ),
 ( -1.999998997246040133, -9.600809889320771617E-07 ),
 .UNSPECIFIED. ) ;
#104387 = CARTESIAN_POINT ( 'NONE',  ( -40.34049200596960105, 1440.913060404669977, 259.7628775194000355 ) ) ;
#104388 = CARTESIAN_POINT ( 'NONE',  ( 37.01672902516649799, 1449.531401005109956, 136.2926409833710295 ) ) ;
#104389 = CARTESIAN_POINT ( 'NONE',  ( 2.351380987493629338, 1449.654710599547343, 154.4274086630604188 ) ) ;
#104390 = B_SPLINE_CURVE_WITH_KNOTS ( 'NONE', 5,
 ( #13695, #91538, #30520, #109450, #74748, #21546, #32179, #83136, #47881 ),
 .UNSPECIFIED., .F., .F.,
 ( 6, 3, 6 ),
 ( 429.1212792279999917, 432.6128460950000090, 434.2407011939999961 ),
 .UNSPECIFIED. ) ;
#104391 = CARTESIAN_POINT ( 'NONE',  ( -0.5241100996639990184, 1430.162173504289967, 199.7031367948490015 ) ) ;
#104392 = CARTESIAN_POINT ( 'NONE',  ( 14.43289921540000087, 1509.539432541030010, 235.4218729623979982 ) ) ;
#104393 = CARTESIAN_POINT ( 'NONE',  ( 26.86204993032690069, 1508.007394616730153, 206.2315948942269870 ) ) ;
#104394 = CARTESIAN_POINT ( 'NONE',  ( -4.290508147089998836, 1515.379315998089851, 209.4884831641960261 ) ) ;
#104395 = EDGE_LOOP ( 'NONE', ( #98469, #49930, #3124, #20319 ) ) ;
#104396 = CARTESIAN_POINT ( 'NONE',  ( 18.83964618864519380, 1526.382868172863937, 185.4251846830098316 ) ) ;
#104397 = TOROIDAL_SURFACE ( 'NONE', #66852, 11.99982860380000105, 0.5000000000000000000 ) ;
#104398 = CARTESIAN_POINT ( 'NONE',  ( -0.1939829864129989923, 1486.063949427190209, 197.1933270691990003 ) ) ;
#104399 = CARTESIAN_POINT ( 'NONE',  ( 3.238173812045069599, 1465.056324971090135, 199.8094274036559739 ) ) ;
#104400 = CARTESIAN_POINT ( 'NONE',  ( -0.2153814148640000037, 1475.836819236129941, 266.9611412552980028 ) ) ;
#104401 = CARTESIAN_POINT ( 'NONE',  ( 1.247882275640000094, 1499.086922831090078, 200.6750384717489908 ) ) ;
#104402 = FACE_OUTER_BOUND ( 'NONE', #101609, .T. ) ;
#104403 = EDGE_CURVE ( 'NONE', #52385, #61381, #63368, .T. ) ;
#104404 = CARTESIAN_POINT ( 'NONE',  ( 8.719508408019999379, 1427.931009161789916, 212.3464450776189949 ) ) ;
#104405 = CARTESIAN_POINT ( 'NONE',  ( -16.53951191381450059, 1384.872637633759950, 219.7923600667549806 ) ) ;
#104406 = B_SPLINE_SURFACE_WITH_KNOTS ( 'NONE', 5, 5, ( 
 ( #92901, #76113, #110253, #83951, #33527, #8336, #29416, #63615, #55206, #4769, #77769, #3706 ),
 ( #95670, #1629, #26806, #1080, #35206, #98278, #89335, #89880, #69393, #64160, #53134, #78314 ),
 ( #12631, #46808, #13150, #103504, #38913, #60993, #46264, #73095, #97732, #27356, #80938, #21554 ),
 ( #4236, #95119, #86714, #17822, #47335, #37836, #81463, #10006, #72022, #107234, #55765, #72546 ),
 ( #94549, #30525, #106677, #52023, #38371, #86163, #9455, #43621, #106138, #29968, #18383, #52580 ),
 ( #35765, #44177, #69949, #104063, #61540, #87272, #21003, #18939, #10565, #80392, #31624, #41689 ),
 ( #91542, #13699, #48457, #47886, #82023, #14819, #23216, #65256, #6979, #82595, #31074, #83681 ),
 ( #41130, #108340, #49006, #98833, #39487, #92632, #22092, #90978, #32733, #65801, #73658, #66367 ),
 ( #75848, #90420, #83142, #6436, #5885, #75311, #99922, #23767, #57416, #24319, #66913, #109454 ),
 ( #15363, #57954, #56292, #64717, #40581, #32183, #74753, #40031, #101022, #15905, #58503, #108890 ),
 ( #100486, #92087, #49555, #50106, #84231, #7533, #5327, #99367, #109998, #107790, #22640, #56846 ),
 ( #14266, #74213, #78610, #59602, #27108, #9739, #52871, #68022, #69689, #94853, #25965, #86999 ) ),
 .UNSPECIFIED., .F., .F., .F.,
 ( 6, 3, 3, 6 ),
 ( 6, 3, 3, 6 ),
 ( 6.292816022300000256, 6.725418754890000628, 7.590624220079999596, 8.366051734470000056 ),
 ( 0.000000000000000000, 0.3341520964660000259, 1.002456289399999978, 1.447932314210000015 ),
 .UNSPECIFIED. ) ;
#104407 = CARTESIAN_POINT ( 'NONE',  ( -17.60960321790000194, 1415.041103191630100, 207.7251207467879794 ) ) ;
#104408 = CARTESIAN_POINT ( 'NONE',  ( 8.759801967190000482, 1450.891143041990063, 191.6269498783990173 ) ) ;
#104409 = CARTESIAN_POINT ( 'NONE',  ( 26.68215560010769849, 1436.749144562530091, 136.7846546353530073 ) ) ;
#104411 = EDGE_CURVE ( 'NONE', #96120, #79540, #68702, .T. ) ;
#104410 = CARTESIAN_POINT ( 'NONE',  ( -8.242998637256569339, 1396.200912243170023, 201.7549567842249871 ) ) ;
#104412 = CARTESIAN_POINT ( 'NONE',  ( -16.19081144212590218, 1409.478450687899795, 225.0102812049649970 ) ) ;
#104413 = CARTESIAN_POINT ( 'NONE',  ( 4.926829097150000614, 1435.943783413959864, 150.1744789664979862 ) ) ;
#104414 = VERTEX_POINT ( 'NONE', #30122 ) ;
#104415 = CARTESIAN_POINT ( 'NONE',  ( -22.52564151159999639, 1509.699673122230024, 190.3321270482979912 ) ) ;
#104416 = CARTESIAN_POINT ( 'NONE',  ( -13.58246093890570094, 1508.543141741580030, 210.2041360783450159 ) ) ;
#104417 = CARTESIAN_POINT ( 'NONE',  ( 2.038646110889678287, 1525.960063244516959, 177.0579350083066004 ) ) ;
#104419 = CARTESIAN_POINT ( 'NONE',  ( -9.797288353148440265, 1438.442783550709919, 210.7140074991049801 ) ) ;
#104418 = DIRECTION ( 'NONE',  ( 0.000000000000000000, 0.000000000000000000, -1.000000000000000000 ) ) ;
#104420 = AXIS2_PLACEMENT_3D ( 'NONE', #49121, #65926, #32836 ) ;
#104421 = LINE ( 'NONE', #27714, #34297 ) ;
#104422 = CARTESIAN_POINT ( 'NONE',  ( -9.467068884459999722, 1450.246902653889947, 204.4311477998990085 ) ) ;
#104423 = CARTESIAN_POINT ( 'NONE',  ( -109.9853818454200081, 1384.675995219419974, 311.4496462838500292 ) ) ;
#104424 = CARTESIAN_POINT ( 'NONE',  ( 7.755601986420000316, 1424.473492849049990, 212.0082642979490117 ) ) ;
#104425 = CARTESIAN_POINT ( 'NONE',  ( -19.34949465300000071, 1446.106505183189938, 200.0047805777890062 ) ) ;
#104427 = DIRECTION ( 'NONE',  ( -5.980589973904019347E-17, 1.000000000000000000, -1.736889445713099699E-16 ) ) ;
#104426 = B_SPLINE_CURVE_WITH_KNOTS ( 'NONE', 3,
 ( #102022, #93081, #85227, #75206, #24215, #100916, #16896, #41595, #57319, #83576, #91986, #7430, #33723, #58401, #58949, #32638, #66815, #68465, #49996, #92526, #51102, #67915 ),
 .UNSPECIFIED., .F., .F.,
 ( 4, 3, 3, 3, 3, 3, 3, 4 ),
 ( 6.826668448630000685E-15, 1.142757973758999901, 2.309653782353159990, 3.228996148453810111, 3.979625921832550262, 5.138688428070659953, 5.803026787480529691, 6.457992286039999641 ),
 .UNSPECIFIED. ) ;
#104428 = CARTESIAN_POINT ( 'NONE',  ( 7.883543492515000750, 1512.115618635729788, 206.1708866102069919 ) ) ;
#104429 = CARTESIAN_POINT ( 'NONE',  ( -109.5441724319999963, 1378.085199107079916, 306.7703179349799711 ) ) ;
#104430 = CARTESIAN_POINT ( 'NONE',  ( 9.532517564039318714, 1366.286862064878051, 210.6218459616987957 ) ) ;
#104432 = ORIENTED_EDGE ( 'NONE', *, *, #26767, .F. ) ;
#104431 = FACE_OUTER_BOUND ( 'NONE', #71716, .T. ) ;
#104433 = VERTEX_POINT ( 'NONE', #5483 ) ;
#104434 = FACE_OUTER_BOUND ( 'NONE', #77729, .T. ) ;
#104435 = CARTESIAN_POINT ( 'NONE',  ( 1.435309881534390097, 1482.888641461259795, 235.7288509090289779 ) ) ;
#104436 = DIRECTION ( 'NONE',  ( -0.7067700376992160916, 0.03085825578589865628, -0.7067700346367981057 ) ) ;
#104437 = FACE_OUTER_BOUND ( 'NONE', #94799, .T. ) ;
#104438 = CARTESIAN_POINT ( 'NONE',  ( -119.3423021147281418, 1306.483669372790018, 300.9755515165800830 ) ) ;
#104439 = FACE_OUTER_BOUND ( 'NONE', #74569, .T. ) ;
#104440 = CARTESIAN_POINT ( 'NONE',  ( -2.509809942567690300, 1464.411809687589994, 199.2066022212569862 ) ) ;
#104441 = CARTESIAN_POINT ( 'NONE',  ( 21.56891739610000158, 1409.666263584230137, 206.3502057800680234 ) ) ;
#104442 = CARTESIAN_POINT ( 'NONE',  ( -2.500000000000000000, 1448.335391685370041, 163.4888273390829738 ) ) ;
#104443 = CARTESIAN_POINT ( 'NONE',  ( 9.823147811128091433, 1396.256092269869896, 214.2094273585269946 ) ) ;
#104444 = CARTESIAN_POINT ( 'NONE',  ( 13.63315086529999931, 1408.072387522930057, 211.9251830309279967 ) ) ;
#104445 = CARTESIAN_POINT ( 'NONE',  ( -3.836741580020079923, 1405.826033084110122, 267.8481700188149830 ) ) ;
#104446 = CARTESIAN_POINT ( 'NONE',  ( -14.13194304323140038, 1435.227729348820048, 149.3555327301409932 ) ) ;
#104447 = ORIENTED_EDGE ( 'NONE', *, *, #88720, .F. ) ;
#104448 = CARTESIAN_POINT ( 'NONE',  ( 0.000000000000000000, 1526.382868172863937, 209.1218459616979999 ) ) ;
#104449 = CARTESIAN_POINT ( 'NONE',  ( 21.37468300741550919, 1525.408337840050308, 233.4084488120059859 ) ) ;
#104450 = ORIENTED_EDGE ( 'NONE', *, *, #81750, .T. ) ;
#104451 = ORIENTED_EDGE ( 'NONE', *, *, #31807, .T. ) ;
#104452 = CARTESIAN_POINT ( 'NONE',  ( -22.75273496409615603, 1523.382868172864164, 183.6728937936775310 ) ) ;
#104453 = CARTESIAN_POINT ( 'NONE',  ( -7.173827098650000345, 1361.757975858899954, 207.6218459616989946 ) ) ;
#104454 = CARTESIAN_POINT ( 'NONE',  ( 2.489617538345000103, 1516.665179208830068, 214.1178407578070164 ) ) ;
#104455 = CARTESIAN_POINT ( 'NONE',  ( 3.279658019245000222, 1511.011611623900080, 216.6862599316969806 ) ) ;
#104456 = ORIENTED_EDGE ( 'NONE', *, *, #3739, .F. ) ;
#104457 = CARTESIAN_POINT ( 'NONE',  ( 4.924481260220000323, 1423.601678417960102, 208.0358385729389852 ) ) ;
#104458 = CARTESIAN_POINT ( 'NONE',  ( -72.27662900180000349, 1374.712643069990008, 284.7775436206590598 ) ) ;
#104459 = CARTESIAN_POINT ( 'NONE',  ( -105.9291394038200025, 1378.913060387309770, 303.1458921680629715 ) ) ;
#104460 = CARTESIAN_POINT ( 'NONE',  ( 1.121950743945000051, 1517.123342927159911, 204.1084165760470057 ) ) ;
#104461 = CARTESIAN_POINT ( 'NONE',  ( 10.46269364489999987, 1491.122602117189899, 212.5073291737689942 ) ) ;
#104462 = DIRECTION ( 'NONE',  ( 0.9455185755993177343, 0.000000000000000000, -0.3255681544571540909 ) ) ;
#104463 = CARTESIAN_POINT ( 'NONE',  ( -106.7755317029999986, 1385.123395227499941, 297.1212035911590306 ) ) ;
#104464 = CARTESIAN_POINT ( 'NONE',  ( -52.23400470469020007, 1384.630035204419983, 228.9130027668180105 ) ) ;
#104465 = CARTESIAN_POINT ( 'NONE',  ( -0.7526715882979990724, 1516.710624944440042, 201.4081970979170251 ) ) ;
#104466 = CARTESIAN_POINT ( 'NONE',  ( -4.193343561389999863, 1409.059495171729850, 231.0986301954980036 ) ) ;
#104468 = ORIENTED_EDGE ( 'NONE', *, *, #90745, .F. ) ;
#104467 = CARTESIAN_POINT ( 'NONE',  ( -11.92849872888365681, 1511.839858410421130, 194.1166199672483970 ) ) ;
#104469 = DIRECTION ( 'NONE',  ( -1.836970198721029688E-16, -1.000000000000000000, 0.000000000000000000 ) ) ;
#104470 = CARTESIAN_POINT ( 'NONE',  ( 2.999854732238141697, 1441.831681250876045, 217.8331532270901221 ) ) ;
#104471 = CONICAL_SURFACE ( 'NONE', #95522, 4.000000000000003553, 0.3430239404209998177 ) ;
#104472 = CARTESIAN_POINT ( 'NONE',  ( -8.746836412960000473, 1384.203074880319946, 218.5235076343190030 ) ) ;
#104473 = DIRECTION ( 'NONE',  ( -1.000000000000000000, 0.000000000000000000, 0.000000000000000000 ) ) ;
#104474 = CARTESIAN_POINT ( 'NONE',  ( -25.44254861969999837, 1435.672616488330050, 136.5529500328979964 ) ) ;
#104475 = CARTESIAN_POINT ( 'NONE',  ( -6.934528567894999718, 1516.588006113850042, 211.9958048218269937 ) ) ;
#104476 = B_SPLINE_CURVE_WITH_KNOTS ( 'NONE', 3,
 ( #16169, #34649, #41954, #26801, #85041, #68833, #60426, #50372, #110248, #84498, #50910, #8331, #52574, #60988, #33522, #18378, #17817, #7246, #1075, #94544, #7788, #86158, #75574, #77764, #109707, #67171, #101270, #25678, #24567, #76108, #67723, #101831, #42495, #59870, #34095, #93998, #96219, #18933, #88915, #45286, #3843, #105737, #71617, #28465, #54783 ),
 .UNSPECIFIED., .F., .F.,
 ( 4, 2, 2, 1, 1, 2, 2, 2, 2, 1, 1, 1, 1, 2, 2, 2, 2, 2, 2, 2, 2, 1, 1, 1, 2, 2, 4 ),
 ( 0.000000000000000000, 0.1249999999994212130, 0.1874999999990521748, 0.2187499999989441779, 0.2343749999988924970, 0.2421874999988680721, 0.2499999999988436472, 0.3749999999997821742, 0.4375000000003342326, 0.4687500000005341838, 0.4843750000007066570, 0.4921875000007929768, 0.4960937500009067747, 0.4980468750009636736, 0.5000000000010205170, 0.5625000000007670531, 0.5937500000007199796, 0.6093750000006320500, 0.6250000000005442313, 0.6875000000005638823, 0.7187500000005786482, 0.7343750000005859757, 0.7421875000004842793, 0.7460937500005387912, 0.7480468750005661027, 0.7500000000005933032, 1.000000000000000000 ),
 .UNSPECIFIED. ) ;
#104477 = CARTESIAN_POINT ( 'NONE',  ( -66.59180496469998900, 1379.743803986980083, 275.7189149213589872 ) ) ;
#104478 = AXIS2_PLACEMENT_3D ( 'NONE', #59542, #67958, #110482 ) ;
#104479 = B_SPLINE_CURVE_WITH_KNOTS ( 'NONE', 3,
 ( #62067, #105712, #104031, #87810, #88893, #78280, #18905, #70469, #54762, #46368, #45813, #78852, #1592, #9974, #28995, #18353, #2711, #86678, #63181, #80505, #96192, #79947, #20024, #44703, #71026, #52546, #35730, #104589, #27884, #44145, #69918, #54219, #88345, #72129, #61508, #19467, #2162 ),
 .UNSPECIFIED., .F., .F.,
 ( 4, 3, 3, 3, 3, 3, 3, 3, 3, 3, 3, 3, 4 ),
 ( -13.74231060008099981, -13.66514189682659897, -12.92929132305900097, -12.11627204603709984, -11.30376823848880008, -10.44046530963600006, -9.415415393832899937, -8.316051554799299694, -7.441798631434849653, -6.496218934871920148, -5.648106363132958663, -4.910580565460959335, -4.218056259389999951 ),
 .UNSPECIFIED. ) ;
#104480 = CARTESIAN_POINT ( 'NONE',  ( 0.009664285302395179966, 1508.316642170103023, 237.8215122148098999 ) ) ;
#104481 = FACE_OUTER_BOUND ( 'NONE', #101292, .T. ) ;
#104482 = CARTESIAN_POINT ( 'NONE',  ( 18.08349198060839313, 1410.907708222537167, 193.6100829980179583 ) ) ;
#104483 = CARTESIAN_POINT ( 'NONE',  ( -4.612671377915000370, 1516.783665406140017, 209.8782801844560026 ) ) ;
#104484 = VERTEX_POINT ( 'NONE', #72175 ) ;
#104485 = DIRECTION ( 'NONE',  ( 0.7257729707430152777, -3.515610711370605188E-08, 0.6879342955100125057 ) ) ;
#104486 = CARTESIAN_POINT ( 'NONE',  ( 5.487972679035699741, 1440.608688546609983, 154.7779097438309748 ) ) ;
#104487 = CARTESIAN_POINT ( 'NONE',  ( -17.46768317430000295, 1384.870099884450156, 219.9576826991589940 ) ) ;
#104488 = ORIENTED_EDGE ( 'NONE', *, *, #92401, .T. ) ;
#104489 = CARTESIAN_POINT ( 'NONE',  ( -19.48484630070749901, 1385.278268516279923, 220.7194127531260222 ) ) ;
#104490 = CARTESIAN_POINT ( 'NONE',  ( -2.981671477319999930, 1430.762427285789954, 201.3088114122890033 ) ) ;
#104491 = CARTESIAN_POINT ( 'NONE',  ( 12.72506363647149996, 1434.731722876650110, 149.9707054014059793 ) ) ;
#104492 = EDGE_CURVE ( 'NONE', #74455, #96281, #28459, .T. ) ;
#104493 = PRODUCT ( 'Grinder Body', 'Grinder Body', '', ( #49376 ) ) ;
#104494 = CARTESIAN_POINT ( 'NONE',  ( 15.34910765019810164, 1478.706085042730138, 230.6431425157049944 ) ) ;
#104495 = CARTESIAN_POINT ( 'NONE',  ( -22.38397194849720151, 1509.390755197840008, 226.7792598521729985 ) ) ;
#104496 = CARTESIAN_POINT ( 'NONE',  ( -2.193532793379999735, 1410.364270746530110, 186.3820960473979937 ) ) ;
#104497 = CARTESIAN_POINT ( 'NONE',  ( 4.987078416414999715, 1508.551704408389924, 212.6094384009469707 ) ) ;
#104498 = CARTESIAN_POINT ( 'NONE',  ( -0.1069634773768380065, 1420.455459563880140, 182.7125832242149954 ) ) ;
#104500 = CARTESIAN_POINT ( 'NONE',  ( -2.919622620539999769, 1419.522956624030030, 186.2043862055979844 ) ) ;
#104499 = CARTESIAN_POINT ( 'NONE',  ( -2.483322492024999661, 1517.139039350860003, 215.6851008610869940 ) ) ;
#104501 = CARTESIAN_POINT ( 'NONE',  ( -5.858855997866009524, 1391.912605642699873, 215.0838203321740139 ) ) ;
#104502 = CARTESIAN_POINT ( 'NONE',  ( -107.4307047400000101, 1391.913060387289988, 300.8770155100590387 ) ) ;
#104503 = ORIENTED_EDGE ( 'NONE', *, *, #32448, .F. ) ;
#104504 = CARTESIAN_POINT ( 'NONE',  ( -11.73069774347650096, 1414.913057862230062, 197.7037919276860123 ) ) ;
#104505 = CARTESIAN_POINT ( 'NONE',  ( -16.20888296009999863, 1485.913060386929828, 186.2979123506979988 ) ) ;
#104506 = ORIENTED_EDGE ( 'NONE', *, *, #97397, .F. ) ;
#104507 = CARTESIAN_POINT ( 'NONE',  ( 3.410503593230000074, 1419.799443580629941, 185.4204322456980094 ) ) ;
#104508 = EDGE_CURVE ( 'NONE', #33349, #27375, #105761, .T. ) ;
#104509 = B_SPLINE_CURVE_WITH_KNOTS ( 'NONE', 5,
 ( #8401, #37, #109779, #25747, #67792, #34717 ),
 .UNSPECIFIED., .F., .F.,
 ( 6, 6 ),
 ( 0.000000000000000000, 0.09439357723473694450 ),
 .UNSPECIFIED. ) ;
#104510 = CARTESIAN_POINT ( 'NONE',  ( -21.83550407203936672, 1523.678648413191695, 183.2743720722710634 ) ) ;
#104511 = CARTESIAN_POINT ( 'NONE',  ( 7.683752556684630086, 1511.083508941950186, 203.3594437696220041 ) ) ;
#104512 = CARTESIAN_POINT ( 'NONE',  ( 2.801853610880000289, 1442.344586916589833, 217.6656895430990062 ) ) ;
#104513 = CARTESIAN_POINT ( 'NONE',  ( -26.35583388131840010, 1508.014892778499870, 201.5454125265999892 ) ) ;
#104514 = CARTESIAN_POINT ( 'NONE',  ( -271.2574215431060338, 11216.44053380568585, -1816.021012422609601 ) ) ;
#104515 = CARTESIAN_POINT ( 'NONE',  ( 18.34708879960000161, 1415.579607672129896, 210.0281939247909975 ) ) ;
#104516 = CARTESIAN_POINT ( 'NONE',  ( -17.72811920550000053, 1424.454094666429910, 227.0280627830979938 ) ) ;
#104517 = CARTESIAN_POINT ( 'NONE',  ( -22.01249284969999920, 1435.265941330599844, 141.1946398826979703 ) ) ;
#104518 = EDGE_CURVE ( 'NONE', #90367, #58486, #26773, .T. ) ;
#104519 = CARTESIAN_POINT ( 'NONE',  ( -5.534100668969379910, 1464.371862158079921, 199.5915835189479992 ) ) ;
#104520 = CARTESIAN_POINT ( 'NONE',  ( 17.88646199680000137, 1428.770680955329908, 191.8789351869980067 ) ) ;
#104522 = CARTESIAN_POINT ( 'NONE',  ( -18.98465183149178159, 1439.320828499731761, 210.1502228767389227 ) ) ;
#104521 = CARTESIAN_POINT ( 'NONE',  ( 9.374206578739999074, 1489.420254891390186, 201.2494609442489946 ) ) ;
#104523 = CARTESIAN_POINT ( 'NONE',  ( -9.220992939474999872, 1511.932705841380084, 197.3648029957670076 ) ) ;
#104524 = EDGE_LOOP ( 'NONE', ( #52923, #97391, #37530, #46450 ) ) ;
#104525 = CARTESIAN_POINT ( 'NONE',  ( 8.613178118295000019, 1512.860712383139798, 206.8726288444870249 ) ) ;
#104526 = CARTESIAN_POINT ( 'NONE',  ( 25.24387641800000281, 1469.171074702029955, 206.7381186227779892 ) ) ;
#104527 = CARTESIAN_POINT ( 'NONE',  ( -11.90126295645609922, 1433.308378356310186, 149.9471753442728641 ) ) ;
#104528 = CARTESIAN_POINT ( 'NONE',  ( -2.454075143049999852, 1484.161599711790132, 198.7041245505990048 ) ) ;
#104529 = CARTESIAN_POINT ( 'NONE',  ( -1.925297167936410148, 1517.051704408389924, 187.5582988455250018 ) ) ;
#104530 = CARTESIAN_POINT ( 'NONE',  ( -10.50583156713009991, 1480.154605857860133, 208.5861483567410062 ) ) ;
#104531 = B_SPLINE_SURFACE_WITH_KNOTS ( 'NONE', 5, 5, ( 
 ( #22675, #30557, #57982, #32214, #5356, #64745 ),
 ( #23246, #23792, #99951, #32757, #66394, #90452 ),
 ( #47367, #57444, #109480, #38940, #107816, #58532 ),
 ( #74782, #99396, #4795, #49582, #39515, #92117 ),
 ( #48484, #83712, #107261, #6462, #66940, #73690 ),
 ( #100514, #5915, #7007, #41165, #31105, #101048 ),
 ( #75339, #24348, #81493, #91570, #73120, #49036 ),
 ( #98858, #83171, #56875, #56321, #40061, #13730 ),
 ( #47915, #65284, #91005, #14295, #82623, #74241 ),
 ( #1378, #84802, #17586, #94307, #60188, #102157 ),
 ( #26561, #50669, #25439, #51220, #69146, #93744 ),
 ( #68591, #42268, #51785, #292, #76985, #92658 ) ),
 .UNSPECIFIED., .F., .F., .F.,
 ( 6, 3, 3, 6 ),
 ( 6, 6 ),
 ( 75.80574312749999422, 89.42327280100001019, 103.1886234069999944, 121.4516539489999900 ),
 ( 0.000000000000000000, 2.000000000000000000 ),
 .UNSPECIFIED. ) ;
#104532 = CARTESIAN_POINT ( 'NONE',  ( 7.500000000000000000, 1391.913060387289988, 209.1218459616989946 ) ) ;
#104533 = CARTESIAN_POINT ( 'NONE',  ( -18.77070031028269881, 1509.608129496780066, 185.4799149847799811 ) ) ;
#104534 = CARTESIAN_POINT ( 'NONE',  ( -11.52230023899750044, 1489.339508248780248, 213.1482211750440001 ) ) ;
#104535 = CARTESIAN_POINT ( 'NONE',  ( -16.61337778659050102, 1463.629532367329830, 220.4655059527940182 ) ) ;
#104536 = CARTESIAN_POINT ( 'NONE',  ( -88.49165759785731211, 1383.771278392089926, 307.9869884267500311 ) ) ;
#104537 = CARTESIAN_POINT ( 'NONE',  ( -109.9093271260659890, 1384.056711624799846, 311.3953200952379348 ) ) ;
#104538 = DIRECTION ( 'NONE',  ( 0.8672669759446693938, 6.017873532443186100E-15, 0.4978433412588624818 ) ) ;
#104540 = ADVANCED_FACE ( 'NONE', ( #4400 ), #71508, .F. ) ;
#104539 = CARTESIAN_POINT ( 'NONE',  ( 15.94345596297699963, 1409.469818137940138, 225.2684692625209948 ) ) ;
#104542 = ORIENTED_EDGE ( 'NONE', *, *, #12582, .T. ) ;
#104541 = CARTESIAN_POINT ( 'NONE',  ( 24.87051451770000199, 1509.771876611130210, 194.6077560229979895 ) ) ;
#104543 = CARTESIAN_POINT ( 'NONE',  ( -17.63310548600473027, 1460.277549070645819, 228.1886722138392543 ) ) ;
#104544 = CARTESIAN_POINT ( 'NONE',  ( -69.46418562150000753, 1379.235091224930102, 280.3187033645589850 ) ) ;
#104545 = CARTESIAN_POINT ( 'NONE',  ( 20.47964310962990098, 1509.616076180499931, 230.4126872671060084 ) ) ;
#104546 = VERTEX_POINT ( 'NONE', #37993 ) ;
#104547 = VERTEX_POINT ( 'NONE', #54805 ) ;
#104548 = CARTESIAN_POINT ( 'NONE',  ( 18.29057181139999955, 1416.237488680629895, 209.4384559441829765 ) ) ;
#104549 = DIRECTION ( 'NONE',  ( 0.000000000000000000, 0.000000000000000000, 1.000000000000000000 ) ) ;
#104550 = CARTESIAN_POINT ( 'NONE',  ( 13.51726861618126385, 1443.820864582427475, 169.3508485337632976 ) ) ;
#104552 = CARTESIAN_POINT ( 'NONE',  ( -32.18001708380000281, 1459.550822088330051, 259.4130758622980011 ) ) ;
#104551 = CARTESIAN_POINT ( 'NONE',  ( 20.52471789389999657, 1470.812340170629795, 209.1688890340030014 ) ) ;
#104553 = AXIS2_PLACEMENT_3D ( 'NONE', #95533, #28334, #60288 ) ;
#104554 = CARTESIAN_POINT ( 'NONE',  ( -4.473177171425660070, 1495.214931084829914, 197.6378604175340001 ) ) ;
#104555 = CARTESIAN_POINT ( 'NONE',  ( -109.8932579119999957, 1384.895258862230094, 297.0235774065590135 ) ) ;
#104556 = CARTESIAN_POINT ( 'NONE',  ( 26.91030929520000115, 1509.852789098830044, 199.4984680808380233 ) ) ;
#104557 = CARTESIAN_POINT ( 'NONE',  ( 18.81609481059999922, 1456.479165729590022, 204.5196734937790097 ) ) ;
#104558 = CARTESIAN_POINT ( 'NONE',  ( 13.75903288890000198, 1409.893112510430001, 191.3057356182980016 ) ) ;
#104559 = CARTESIAN_POINT ( 'NONE',  ( 4.209031965520000362, 1421.916286089330242, 184.3722572684980037 ) ) ;
#104561 = CARTESIAN_POINT ( 'NONE',  ( -7.259422120870000050, 1440.164841281420195, 154.1325279538980055 ) ) ;
#104560 = CIRCLE ( 'NONE', #56288, 32.13701971169416538 ) ;
#104562 = CARTESIAN_POINT ( 'NONE',  ( 10.72974958539999868, 1437.118219821549928, 152.1700466173979862 ) ) ;
#104563 = CARTESIAN_POINT ( 'NONE',  ( -13.82453468407210018, 1421.936557082180116, 203.7229994192829849 ) ) ;
#104564 = CARTESIAN_POINT ( 'NONE',  ( -3.017631988560000256, 1452.807682356229861, 152.5478258260980340 ) ) ;
#104565 = CARTESIAN_POINT ( 'NONE',  ( -4.363122647530000009, 1418.913060387330006, 172.2701767054979882 ) ) ;
#104566 = VERTEX_POINT ( 'NONE', #20607 ) ;
#104567 = CARTESIAN_POINT ( 'NONE',  ( -4.240940644606780552, 1509.032041130069956, 212.8662740090449859 ) ) ;
#104568 = CARTESIAN_POINT ( 'NONE',  ( 9.890535630430530745, 1492.213485579389953, 188.4030009006890225 ) ) ;
#104569 = CARTESIAN_POINT ( 'NONE',  ( -42.71995277159999915, 1443.972229192440182, 270.1998966713979939 ) ) ;
#104570 = CARTESIAN_POINT ( 'NONE',  ( 7.503571368420000276, 1422.857534295030064, 195.6852864414989881 ) ) ;
#104571 = CARTESIAN_POINT ( 'NONE',  ( 11.97827956719999776, 1441.604408666619975, 150.7817505876979851 ) ) ;
#104572 = CYLINDRICAL_SURFACE ( 'NONE', #68036, 2.000000000000003109 ) ;
#104573 = B_SPLINE_CURVE_WITH_KNOTS ( 'NONE', 3,
 ( #77132, #110164, #17165, #42973, #42406, #25034, #101746, #59236, #73405, #30830, #93354, #34005, #34557, #98586, #21852, #56049, #79888, #94445, #103968, #9908, #54153, #95023, #70965, #61448, #26138, #95572, #69290, #68740, #19959, #27265, #78215, #62002, #60898, #18842, #9364, #36773, #36221, #45193, #87174, #87744, #11022, #1527, #35660 ),
 .UNSPECIFIED., .F., .F.,
 ( 4, 3, 3, 3, 3, 3, 3, 3, 3, 3, 3, 3, 3, 3, 4 ),
 ( 0.7655572723410000169, 0.9910019270782730594, 1.224379706194399953, 1.462078625956309885, 1.704827365190310084, 1.793853281190000093, 2.038466590501220033, 2.281256473202240009, 2.316155491850000026, 2.583989317130000352, 2.855920918771889916, 3.139267317773660082, 3.387490792969999553, 3.680707211540199530, 3.835724788479999425 ),
 .UNSPECIFIED. ) ;
#104574 = CARTESIAN_POINT ( 'NONE',  ( 13.91344329490000042, 1453.313060387329870, 195.2084026661979976 ) ) ;
#104575 = CARTESIAN_POINT ( 'NONE',  ( 2.926631436004109688, 1410.008353746950206, 231.5604053785249903 ) ) ;
#104576 = CARTESIAN_POINT ( 'NONE',  ( 1.717348298979999965, 1508.746280155129853, 237.8324610923980060 ) ) ;
#104577 = CARTESIAN_POINT ( 'NONE',  ( -4.849515614649999584, 1416.821738697630053, 232.3035063180979876 ) ) ;
#104578 = CARTESIAN_POINT ( 'NONE',  ( -9.321551428969998554, 1460.110613089990011, 211.8159337765089845 ) ) ;
#104579 = CARTESIAN_POINT ( 'NONE',  ( 10.93866963977056983, 1362.275162845329533, 208.3718459617010978 ) ) ;
#104580 = CARTESIAN_POINT ( 'NONE',  ( -44.17901015457650260, 1430.646547340430061, 267.0395108202489496 ) ) ;
#104581 = CARTESIAN_POINT ( 'NONE',  ( -4.153907728910000152, 1436.967118409070054, 185.6199311185980036 ) ) ;
#104582 = VERTEX_POINT ( 'NONE', #29045 ) ;
#104583 = CARTESIAN_POINT ( 'NONE',  ( 25.19713807460000154, 1435.377389496489741, 135.6160520644979783 ) ) ;
#104584 = VERTEX_POINT ( 'NONE', #72705 ) ;
#104585 = CARTESIAN_POINT ( 'NONE',  ( -2.865636847234999784, 1516.815173273089840, 210.2578502442970318 ) ) ;
#104586 = CARTESIAN_POINT ( 'NONE',  ( -10.06450494029999909, 1472.332863763290106, 203.5506889703189870 ) ) ;
#104587 = CARTESIAN_POINT ( 'NONE',  ( -2.470955845399090300, 1523.580203803270933, 242.8749759691355621 ) ) ;
#104588 = CARTESIAN_POINT ( 'NONE',  ( -16.18847876140000253, 1410.409213345830040, 191.4685065236979824 ) ) ;
#104589 = CARTESIAN_POINT ( 'NONE',  ( -2.323079643848300346, 1496.857146867429947, 221.2763090542839848 ) ) ;
#104590 = ORIENTED_EDGE ( 'NONE', *, *, #41892, .F. ) ;
#104591 = CARTESIAN_POINT ( 'NONE',  ( -15.82374664200000147, 1506.811133727029983, 193.8386827112979631 ) ) ;
#104593 = CARTESIAN_POINT ( 'NONE',  ( -29.13898522074213560, 1526.069472839378477, 197.1409705599818381 ) ) ;
#104592 = CYLINDRICAL_SURFACE ( 'NONE', #69330, 1.999999999999994005 ) ;
#104594 = AXIS2_PLACEMENT_3D ( 'NONE', #74316, #31176, #22751 ) ;
#104595 = CARTESIAN_POINT ( 'NONE',  ( 2.764546554733247508, 1486.833185097884325, 219.5825234514556712 ) ) ;
#104596 = CARTESIAN_POINT ( 'NONE',  ( -16.59330332571189714, 1508.551704408389924, 213.1175702257220053 ) ) ;
#104597 = CARTESIAN_POINT ( 'NONE',  ( 18.51267884070961145, 1508.236097879769432, 188.5103842653526272 ) ) ;
#104599 = CIRCLE ( 'NONE', #56334, 0.9999999999999887867 ) ;
#104598 = CARTESIAN_POINT ( 'NONE',  ( -8.809230282280388735, 1438.685521035069996, 208.2566144035540106 ) ) ;
#104600 = ORIENTED_EDGE ( 'NONE', *, *, #9035, .F. ) ;
#104601 = CARTESIAN_POINT ( 'NONE',  ( -18.62763287599860007, 1413.086711950159952, 269.8943054501950201 ) ) ;
#104602 = CARTESIAN_POINT ( 'NONE',  ( 5.775625077365000415, 1516.745833913490060, 208.3665194962490261 ) ) ;
#104603 = CARTESIAN_POINT ( 'NONE',  ( -0.9541980962059989357, 1483.985701800989773, 201.2944015401489821 ) ) ;
#104604 = CARTESIAN_POINT ( 'NONE',  ( 9.205082684422309924, 1434.999538654240041, 207.3832038862170180 ) ) ;
#104606 = ORIENTED_EDGE ( 'NONE', *, *, #101724, .T. ) ;
#104605 = CARTESIAN_POINT ( 'NONE',  ( -4.973616640903610886, 1367.807959820899441, 207.6218459616988241 ) ) ;
#104607 = ORIENTED_EDGE ( 'NONE', *, *, #92850, .T. ) ;
#104608 = CARTESIAN_POINT ( 'NONE',  ( 45.62788796885585185, 1441.601644691920001, 268.9750038475548877 ) ) ;
#104609 = CARTESIAN_POINT ( 'NONE',  ( 2.870880155352820040, 1466.604627524899797, 219.7960964397389887 ) ) ;
#104610 = CARTESIAN_POINT ( 'NONE',  ( -22.08327125186908191, 1523.604703353109699, 233.8169256665491105 ) ) ;
#104611 = CARTESIAN_POINT ( 'NONE',  ( -0.01421524400490130000, 1408.952300071870013, 186.1308435959000178 ) ) ;
#104612 = CARTESIAN_POINT ( 'NONE',  ( -18.64275274472940325, 1415.948038441080143, 207.5714938949250268 ) ) ;
#104613 = CARTESIAN_POINT ( 'NONE',  ( -23.20509094550000029, 1425.806681453030023, 211.9918775447279984 ) ) ;
#104614 = CARTESIAN_POINT ( 'NONE',  ( 22.44355668859300224, 1471.536005699779935, 269.1117652856750055 ) ) ;
#104615 = CARTESIAN_POINT ( 'NONE',  ( -9.019884638846754399, 1465.064825884716129, 232.8089404004333574 ) ) ;
#104616 = CARTESIAN_POINT ( 'NONE',  ( 12.53380176329999784, 1445.052233945699982, 186.0874982363980052 ) ) ;
#104617 = CARTESIAN_POINT ( 'NONE',  ( -6.563254928984999736, 1517.139039350860003, 206.6385234782069915 ) ) ;
#104618 = ORIENTED_EDGE ( 'NONE', *, *, #45458, .F. ) ;
#104619 = CARTESIAN_POINT ( 'NONE',  ( -13.81919561380460060, 1452.718877875840008, 223.1176038296620163 ) ) ;
#104620 = CARTESIAN_POINT ( 'NONE',  ( 1.474324447131689864, 1482.591219605810011, 182.1827347203019940 ) ) ;
#104621 = ORIENTED_EDGE ( 'NONE', *, *, #84525, .F. ) ;
#104622 = CYLINDRICAL_SURFACE ( 'NONE', #33806, 1.999999999999999556 ) ;
#104623 = CARTESIAN_POINT ( 'NONE',  ( 26.04939065782729912, 1450.947403696690117, 136.6506608130579821 ) ) ;
#104624 = CARTESIAN_POINT ( 'NONE',  ( 11.27215015582655688, 1425.068134849736907, 138.0224606737560578 ) ) ;
#104625 = CARTESIAN_POINT ( 'NONE',  ( -37.21633441560000222, 1384.983113612510124, 210.1703949109789846 ) ) ;
#104626 = FACE_OUTER_BOUND ( 'NONE', #100418, .T. ) ;
#104627 = CARTESIAN_POINT ( 'NONE',  ( 16.71902292089999875, 1409.496901533429991, 193.2501433177980346 ) ) ;
#104628 = CARTESIAN_POINT ( 'NONE',  ( 27.73716673060003757, 1443.913060387329097, 175.8274728504979976 ) ) ;
#104629 = CARTESIAN_POINT ( 'NONE',  ( 2.579410839141357936, 1439.640988620472626, 183.3331822185549811 ) ) ;
#104631 = CARTESIAN_POINT ( 'NONE',  ( -18.88027416897331179, 1424.772622057686704, 224.4247119630791758 ) ) ;
#104630 = CARTESIAN_POINT ( 'NONE',  ( 0.2990840903870000123, 1416.120339285229875, 233.5289124774980110 ) ) ;
#104632 = DIRECTION ( 'NONE',  ( -0.2054769195713186114, -6.237798632656567355E-16, 0.9786619618251657382 ) ) ;
#104633 = CARTESIAN_POINT ( 'NONE',  ( -9.454895823979999392, 1382.479201248260097, 217.9319156271789950 ) ) ;
#104634 = CARTESIAN_POINT ( 'NONE',  ( 0.01289778877310149806, 1516.939723362869927, 214.1281058189269970 ) ) ;
#104635 = CARTESIAN_POINT ( 'NONE',  ( 26.88225067539190150, 1446.276343828759991, 137.3355637594920040 ) ) ;
#104636 = VERTEX_POINT ( 'NONE', #65415 ) ;
#104637 = DIRECTION ( 'NONE',  ( 0.000000000000000000, 1.000000000000000000, 0.000000000000000000 ) ) ;
#104638 = CARTESIAN_POINT ( 'NONE',  ( 21.33281718256677451, 1523.429859730330236, 237.7590525783467683 ) ) ;
#104639 = CARTESIAN_POINT ( 'NONE',  ( -0.4291274509555380035, 1409.251717294920127, 232.6516010116560267 ) ) ;
#104640 = EDGE_CURVE ( 'NONE', #99633, #30773, #106606, .T. ) ;
#104641 = DIRECTION ( 'NONE',  ( -0.5224574779878928821, 0.7067418228236548305, 0.4770263929453257834 ) ) ;
#104642 = CIRCLE ( 'NONE', #63597, 7.500000000000000000 ) ;
#104643 = CARTESIAN_POINT ( 'NONE',  ( 1.302691703616797758, 1421.395884623610755, 193.7699158457419344 ) ) ;
#104644 = DIRECTION ( 'NONE',  ( 0.000000000000000000, -1.000000000000000000, 0.000000000000000000 ) ) ;
#104645 = CARTESIAN_POINT ( 'NONE',  ( 7.993605777300000598E-15, 1455.844446582929777, 219.6133832206979832 ) ) ;
#104646 = CARTESIAN_POINT ( 'NONE',  ( 31.44837959398592986, 1511.187213306747708, 220.9083067115976462 ) ) ;
#104647 = CARTESIAN_POINT ( 'NONE',  ( 11.68271886119999969, 1433.062043557109973, 150.9218026163979687 ) ) ;
#104648 = CARTESIAN_POINT ( 'NONE',  ( -15.40709604279999922, 1473.361390454229877, 269.5773951781980031 ) ) ;
#104649 = B_SPLINE_SURFACE_WITH_KNOTS ( 'NONE', 5, 5, ( 
 ( #97940, #44824, #96307, #104152, #95753, #89551 ),
 ( #45916, #106355, #97402, #2821, #88461, #63288 ),
 ( #105824, #21208, #87927, #36940, #105257, #55417 ),
 ( #70040, #19586, #104701, #11747, #80609, #62750 ),
 ( #45378, #79517, #4460, #96868, #80052, #12840 ),
 ( #27438, #37500, #71706, #19017, #29102, #11214 ),
 ( #20672, #87359, #54872, #78977, #36395, #70584 ),
 ( #12283, #27996, #62181, #40250, #91204, #49225 ),
 ( #100695, #14486, #15571, #49773, #23978, #30182 ),
 ( #5555, #65479, #47561, #15026, #39704, #4989 ),
 ( #91751, #74981, #74432, #108558, #38588, #82801 ),
 ( #90089, #58173, #66591, #64374, #98497, #48115 ) ),
 .UNSPECIFIED., .F., .F., .F.,
 ( 6, 3, 3, 6 ),
 ( 6, 6 ),
 ( 22.90453168350000013, 35.06371889219999360, 67.00219837880000284, 82.96876465699999414 ),
 ( 0.000000000000000000, 2.000000000000000000 ),
 .UNSPECIFIED. ) ;
#104650 = CARTESIAN_POINT ( 'NONE',  ( 26.44889291085189953, 1440.913060394389959, 224.1891630988550048 ) ) ;
#104651 = CARTESIAN_POINT ( 'NONE',  ( -17.08916621680459969, 1420.636132269700056, 201.6183731251909990 ) ) ;
#104652 = ORIENTED_EDGE ( 'NONE', *, *, #9699, .F. ) ;
#104653 = DIRECTION ( 'NONE',  ( -1.000000000000000000, 0.000000000000000000, 0.000000000000000000 ) ) ;
#104654 = CARTESIAN_POINT ( 'NONE',  ( 23.85742997590000414, 1435.349283830410059, 137.3962418501980380 ) ) ;
#104655 = CARTESIAN_POINT ( 'NONE',  ( -7.000066174799999708, 1486.134313416229816, 182.6266077387979863 ) ) ;
#104656 = CARTESIAN_POINT ( 'NONE',  ( -1.333616551530000249, 1444.154719697190103, 199.5606640046889879 ) ) ;
#104657 = LINE ( 'NONE', #71661, #100860 ) ;
#104658 = CARTESIAN_POINT ( 'NONE',  ( 25.92853884430000377, 1469.242862523229860, 212.4557546463379936 ) ) ;
#104659 = CARTESIAN_POINT ( 'NONE',  ( -16.75463440289568950, 1420.038624242013157, 208.1824980296739227 ) ) ;
#104660 = CARTESIAN_POINT ( 'NONE',  ( -8.309064975820000143, 1507.619008861029897, 235.1729359256979990 ) ) ;
#104661 = CARTESIAN_POINT ( 'NONE',  ( -35.92588528242170298, 1383.834180000839979, 235.2311359915490243 ) ) ;
#104662 = VECTOR ( 'NONE', #31482, 1000.000000000000000 ) ;
#104663 = CARTESIAN_POINT ( 'NONE',  ( -3.224548122823300389, 1508.551704408489968, 204.2884089881570162 ) ) ;
#104664 = CARTESIAN_POINT ( 'NONE',  ( 5.516975442445060551, 1422.876349978269900, 115.6516328984649959 ) ) ;
#104666 =( BOUNDED_CURVE ( )  B_SPLINE_CURVE ( 3, ( #13195, #97220, #46850, #89920 ),
 .UNSPECIFIED., .F., .T. ) 
 B_SPLINE_CURVE_WITH_KNOTS ( ( 4, 4 ),
 ( 0.02238567329313790114, 0.6605756095507959724 ),
 .UNSPECIFIED. ) 
 CURVE ( )  GEOMETRIC_REPRESENTATION_ITEM ( )  RATIONAL_B_SPLINE_CURVE ( ( 1.000000000000000000, 0.9663464813702775658, 0.9663464813702775658, 1.000000000000000000 ) ) 
 REPRESENTATION_ITEM ( '' )  );
#104665 = CARTESIAN_POINT ( 'NONE',  ( -22.52564151159999639, 1509.699673122230024, 190.3321270482979912 ) ) ;
#104667 = CARTESIAN_POINT ( 'NONE',  ( 0.1661509758321400021, 1482.596978913680005, 181.9828288344639873 ) ) ;
#104669 = ORIENTED_EDGE ( 'NONE', *, *, #8545, .F. ) ;
#104668 = CARTESIAN_POINT ( 'NONE',  ( 16.68463225830000241, 1445.052233488290085, 162.0935120917980043 ) ) ;
#104670 = CARTESIAN_POINT ( 'NONE',  ( -0.3594932245259999659, 1451.468209969430063, 182.7573421931980135 ) ) ;
#104671 = CARTESIAN_POINT ( 'NONE',  ( -8.467296363548342697, 1387.234424845827334, 200.0078932864855972 ) ) ;
#104672 = CARTESIAN_POINT ( 'NONE',  ( -4.132631535169999815, 1476.440258689390021, 199.6218979630789931 ) ) ;
#104674 = ORIENTED_EDGE ( 'NONE', *, *, #10708, .T. ) ;
#104673 = CARTESIAN_POINT ( 'NONE',  ( -32.16538354509416564, 1524.524650307258071, 216.1007197859166808 ) ) ;
#104675 = CARTESIAN_POINT ( 'NONE',  ( -5.717689142141139769, 1508.551704408389924, 219.5099898771389917 ) ) ;
#104676 = ORIENTED_EDGE ( 'NONE', *, *, #31527, .T. ) ;
#104677 = CARTESIAN_POINT ( 'NONE',  ( -14.10038679502460113, 1390.294844427760154, 211.8274118880190144 ) ) ;
#104678 = CARTESIAN_POINT ( 'NONE',  ( 12.26996133436636249, 1416.831922870707331, 223.5794496286292485 ) ) ;
#104679 = CARTESIAN_POINT ( 'NONE',  ( 8.311290096204249522, 1511.035127054690065, 202.3471219999200059 ) ) ;
#104680 = CARTESIAN_POINT ( 'NONE',  ( -2.979756015838803229, 1368.811721020882487, 207.6609286928419067 ) ) ;
#104681 = CARTESIAN_POINT ( 'NONE',  ( -0.4792132924880010414, 1431.125656909089912, 217.6287611528490231 ) ) ;
#104682 = DIRECTION ( 'NONE',  ( -0.8672669759446604010, 0.000000000000000000, 0.4978433412588780804 ) ) ;
#104683 = CARTESIAN_POINT ( 'NONE',  ( 13.59476445004379919, 1409.387800022989950, 202.9347135095200088 ) ) ;
#104684 = CARTESIAN_POINT ( 'NONE',  ( 7.789933822538570141, 1421.055612659608187, 137.0999999980982409 ) ) ;
#104685 = CARTESIAN_POINT ( 'NONE',  ( -92.29530878936199656, 1385.199744097189978, 293.8198967544350353 ) ) ;
#104686 = CARTESIAN_POINT ( 'NONE',  ( -10.01339882083300026, 1391.913060387289988, 214.4629424297139906 ) ) ;
#104687 = CARTESIAN_POINT ( 'NONE',  ( -108.2502590933346198, 1305.913060387290216, 307.0351622366206357 ) ) ;
#104688 = VERTEX_POINT ( 'NONE', #21706 ) ;
#104689 = CARTESIAN_POINT ( 'NONE',  ( 13.51702042466233600, 1443.913060387330006, 169.3754641244197217 ) ) ;
#104691 = VERTEX_POINT ( 'NONE', #98978 ) ;
#104690 = CARTESIAN_POINT ( 'NONE',  ( -1.552364036650669687, 1414.913060595378738, 226.1349304001991527 ) ) ;
#104692 = ORIENTED_EDGE ( 'NONE', *, *, #104815, .F. ) ;
#104693 = CARTESIAN_POINT ( 'NONE',  ( 20.59684415639999955, 1507.762623716630060, 227.3081670307980175 ) ) ;
#104694 = CARTESIAN_POINT ( 'NONE',  ( -5.613600279743296895, 1362.409757668945758, 210.6218459617142003 ) ) ;
#104695 = CARTESIAN_POINT ( 'NONE',  ( -5.301602273869999493, 1495.069292928890036, 198.4488064414990163 ) ) ;
#104696 = CARTESIAN_POINT ( 'NONE',  ( 29.92046006148340709, 1462.307239681074179, 269.4699585593555753 ) ) ;
#104697 = CARTESIAN_POINT ( 'NONE',  ( 15.20184466319999927, 1507.442701412029919, 225.8641442827980086 ) ) ;
#104698 = CARTESIAN_POINT ( 'NONE',  ( 3.817422068910000021, 1397.107870743330068, 221.4612898547980251 ) ) ;
#104699 = CARTESIAN_POINT ( 'NONE',  ( 31.62138935264962569, 1525.231887713385504, 201.5806591012467663 ) ) ;
#104700 = CARTESIAN_POINT ( 'NONE',  ( 18.93704081231690139, 1430.332813895809977, 209.3856457964110120 ) ) ;
#104701 = CARTESIAN_POINT ( 'NONE',  ( -0.8731571743890000903, 1457.276952884830052, 183.1868505578979978 ) ) ;
#104702 = CARTESIAN_POINT ( 'NONE',  ( -7.984337885465997431, 1369.008371754427117, 210.6218459617030021 ) ) ;
#104703 = CARTESIAN_POINT ( 'NONE',  ( -26.36655729521032754, 1436.714562387939850, 136.8351542746285645 ) ) ;
#104704 = CARTESIAN_POINT ( 'NONE',  ( -2.494020320564999782, 1516.876240617270014, 206.8389307488369866 ) ) ;
#104705 = FACE_OUTER_BOUND ( 'NONE', #62489, .T. ) ;
#104706 = CARTESIAN_POINT ( 'NONE',  ( 16.85557976710000005, 1409.501670203030017, 194.3276026113979924 ) ) ;
#104707 = CARTESIAN_POINT ( 'NONE',  ( 2.371343438090000255, 1497.319062567490164, 197.3529125933990258 ) ) ;
#104708 = CARTESIAN_POINT ( 'NONE',  ( -0.2209949390820010184, 1494.455004241089910, 220.2892042338989995 ) ) ;
#104709 = CARTESIAN_POINT ( 'NONE',  ( 41.56283943469610165, 1444.074288271499881, 136.1757548026400002 ) ) ;
#104710 = EDGE_LOOP ( 'NONE', ( #105567, #85382, #107954, #55289 ) ) ;
#104711 = CARTESIAN_POINT ( 'NONE',  ( 33.67852062189999884, 1421.560015059330226, 261.9077681813980121 ) ) ;
#104712 = ADVANCED_FACE ( 'NONE', ( #88936 ), #48972, .T. ) ;
#104713 = CARTESIAN_POINT ( 'NONE',  ( -22.56155901339999659, 1488.679832658830264, 195.6780914239980120 ) ) ;
#104716 = CARTESIAN_POINT ( 'NONE',  ( 31.34137657934008558, 1523.382868172864164, 196.3411265156547358 ) ) ;
#104715 = AXIS2_PLACEMENT_3D ( 'NONE', #90244, #13527, #39303 ) ;
#104714 = CARTESIAN_POINT ( 'NONE',  ( 0.4607471438239999495, 1507.266167991529983, 180.9276013137979930 ) ) ;
#104717 = EDGE_CURVE ( 'NONE', #48781, #64960, #55911, .T. ) ;
#104718 = CARTESIAN_POINT ( 'NONE',  ( -2.864972154145000172, 1516.859514182039902, 212.0024388992169975 ) ) ;
#104719 = CARTESIAN_POINT ( 'NONE',  ( 11.78230151170000006, 1435.286215961589960, 224.1839025558989817 ) ) ;
#104720 = CARTESIAN_POINT ( 'NONE',  ( -22.89347097630000150, 1507.627022993330229, 208.2062336298450020 ) ) ;
#104721 = CARTESIAN_POINT ( 'NONE',  ( -5.805165550179999912, 1411.425361495129891, 255.2684082155979866 ) ) ;
#104722 = CARTESIAN_POINT ( 'NONE',  ( 19.47564118608110206, 1509.620631326759849, 231.4858733237100239 ) ) ;
#104723 = EDGE_CURVE ( 'NONE', #8750, #85013, #107387, .T. ) ;
#104724 = CARTESIAN_POINT ( 'NONE',  ( 28.57599588785479838, 1509.162863316300218, 209.4718383517779898 ) ) ;
#104725 = EDGE_CURVE ( 'NONE', #92866, #46415, #76608, .T. ) ;
#104726 = LINE ( 'NONE', #63307, #44484 ) ;
#104727 = CARTESIAN_POINT ( 'NONE',  ( 33.93392607710000419, 1451.271780568129998, 135.9464999937979997 ) ) ;
#104728 = EDGE_LOOP ( 'NONE', ( #42972, #24268, #7040 ) ) ;
#104729 = CARTESIAN_POINT ( 'NONE',  ( 3.767303529005479934, 1397.401587145810026, 196.1650422737100143 ) ) ;
#104730 = DIRECTION ( 'NONE',  ( 1.000000000000000000, -0.000000000000000000, 1.224646799147353207E-16 ) ) ;
#104731 = CARTESIAN_POINT ( 'NONE',  ( -16.61244639070000062, 1459.967033444430172, 228.4924314892979851 ) ) ;
#104732 = B_SPLINE_CURVE_WITH_KNOTS ( 'NONE', 3,
 ( #20499, #74259, #84285, #47937 ),
 .UNSPECIFIED., .F., .F.,
 ( 4, 4 ),
 ( 0.000000000000000000, 1.000000000000000000 ),
 .UNSPECIFIED. ) ;
#104733 = ORIENTED_EDGE ( 'NONE', *, *, #27359, .F. ) ;
#104734 = ORIENTED_EDGE ( 'NONE', *, *, #105505, .F. ) ;
#104735 = CARTESIAN_POINT ( 'NONE',  ( 8.857752970044110441, 1451.634138792180011, 211.8773160595700062 ) ) ;
#104736 = CARTESIAN_POINT ( 'NONE',  ( 7.991060968840001166, 1423.743734712820014, 195.9120172666990243 ) ) ;
#104737 = ORIENTED_EDGE ( 'NONE', *, *, #17976, .F. ) ;
#104738 = FACE_OUTER_BOUND ( 'NONE', #14681, .T. ) ;
#104739 = CARTESIAN_POINT ( 'NONE',  ( -6.042023989919642624, 1419.473644842602880, 194.9560967347969722 ) ) ;
#104740 = CYLINDRICAL_SURFACE ( 'NONE', #36856, 30.10786454236638576 ) ;
#104741 = CARTESIAN_POINT ( 'NONE',  ( -3.378818643640000285, 1461.193638821730019, 234.6789676215979910 ) ) ;
#104742 = CARTESIAN_POINT ( 'NONE',  ( 6.961841748697260357, 1508.551566289579796, 202.5699741863490146 ) ) ;
#104743 = VECTOR ( 'NONE', #91034, 1000.000000000000114 ) ;
#104744 = CARTESIAN_POINT ( 'NONE',  ( 10.11442602625619891, 1452.508834773780109, 209.7499184922420170 ) ) ;
#104745 = CARTESIAN_POINT ( 'NONE',  ( -12.06139973099999985, 1391.856450693919896, 210.3499673627589743 ) ) ;
#104746 = ADVANCED_FACE ( 'NONE', ( #75471 ), #31951, .T. ) ;
#104747 = CARTESIAN_POINT ( 'NONE',  ( 0.1437158803840000165, 1420.464389115830045, 182.7235331698980190 ) ) ;
#104748 = ORIENTED_EDGE ( 'NONE', *, *, #15882, .F. ) ;
#104749 = CARTESIAN_POINT ( 'NONE',  ( -5.005700239535000762, 1516.732530461250008, 202.1838802717869896 ) ) ;
#104750 = CARTESIAN_POINT ( 'NONE',  ( -6.938478822895000064, 1516.719999691880048, 209.8757167055200057 ) ) ;
#104751 = ORIENTED_EDGE ( 'NONE', *, *, #28913, .F. ) ;
#104752 = CARTESIAN_POINT ( 'NONE',  ( -10.61999372029469946, 1462.990852176999852, 206.0510140530389833 ) ) ;
#104753 = CARTESIAN_POINT ( 'NONE',  ( 1.582067810090000045E-15, 1406.443991414029824, 121.6099336315979969 ) ) ;
#104754 = ORIENTED_EDGE ( 'NONE', *, *, #28391, .F. ) ;
#104755 = CARTESIAN_POINT ( 'NONE',  ( -1.569490127089286480, 1507.974949272165532, 221.0030736985697786 ) ) ;
#104756 = CARTESIAN_POINT ( 'NONE',  ( -4.863838082751120062, 1508.339116710969847, 220.3751376775360029 ) ) ;
#104757 = CARTESIAN_POINT ( 'NONE',  ( -2.919110404717550011, 1368.384062535930070, 207.8228080779019820 ) ) ;
#104758 = EDGE_CURVE ( 'NONE', #25781, #52548, #53022, .T. ) ;
#104759 = CIRCLE ( 'NONE', #97395, 8.500000000000000000 ) ;
#104760 = CARTESIAN_POINT ( 'NONE',  ( -6.941887704655929525, 1471.020790314250007, 216.5580302958940138 ) ) ;
#104761 = CARTESIAN_POINT ( 'NONE',  ( 16.66808812225220038, 1452.330997924170106, 146.5817830544619937 ) ) ;
#104762 = CARTESIAN_POINT ( 'NONE',  ( 1.412130994944630125, 1410.254392240469997, 269.6150871368109847 ) ) ;
#104763 = CARTESIAN_POINT ( 'NONE',  ( -103.5631853459999974, 1389.967198823729859, 302.9633942972590148 ) ) ;
#104764 = CARTESIAN_POINT ( 'NONE',  ( -109.7827413208553509, 1383.386978333693150, 297.1311717743816416 ) ) ;
#104765 = EDGE_CURVE ( 'NONE', #58053, #50989, #101804, .T. ) ;
#104766 = CARTESIAN_POINT ( 'NONE',  ( 8.630513237909999802, 1492.548647927590082, 216.1639467023389898 ) ) ;
#104767 = CARTESIAN_POINT ( 'NONE',  ( -42.07298630380000048, 1379.652797345190265, 226.0105342722590080 ) ) ;
#104768 = CARTESIAN_POINT ( 'NONE',  ( 0.03226293719758020068, 1410.297897419189894, 233.2219341505459909 ) ) ;
#104770 = CARTESIAN_POINT ( 'NONE',  ( 10.69207100893769891, 1469.742000000100006, 205.4164582955250182 ) ) ;
#104769 = CARTESIAN_POINT ( 'NONE',  ( -18.20628436530000016, 1504.691793905290069, 209.0089166509420124 ) ) ;
#104771 = CARTESIAN_POINT ( 'NONE',  ( 11.02420060192179996, 1422.875103594119992, 206.9420604818759841 ) ) ;
#104772 = CARTESIAN_POINT ( 'NONE',  ( -9.906853760125690300, 1439.767124081580050, 207.7335298351040080 ) ) ;
#104773 = CARTESIAN_POINT ( 'NONE',  ( -6.946514214915000096, 1512.024017243120170, 202.0369668883770089 ) ) ;
#104774 = VERTEX_POINT ( 'NONE', #27802 ) ;
#104775 = CARTESIAN_POINT ( 'NONE',  ( 8.215650382230000152E-15, 1424.916853932230197, 224.8635561844979804 ) ) ;
#104776 = DIRECTION ( 'NONE',  ( 0.8539859765994181062, 0.000000000000000000, -0.5202960232132650686 ) ) ;
#104777 = CARTESIAN_POINT ( 'NONE',  ( -68.78023285115449426, 1385.028536229589918, 293.6602838790100236 ) ) ;
#104778 = CARTESIAN_POINT ( 'NONE',  ( -20.68299398335333095, 1525.856065479256586, 233.9549332500229468 ) ) ;
#104779 = CARTESIAN_POINT ( 'NONE',  ( 3.561968053029999748, 1506.511571253490047, 220.3681567290990131 ) ) ;
#104780 = CARTESIAN_POINT ( 'NONE',  ( -14.62125525909999979, 1415.677402202029953, 212.1284411519390289 ) ) ;
#104782 = VERTEX_POINT ( 'NONE', #69835 ) ;
#104781 = CARTESIAN_POINT ( 'NONE',  ( 0.9184306762236260635, 1515.115092018379983, 204.7937143148920143 ) ) ;
#104783 = CARTESIAN_POINT ( 'NONE',  ( -15.74969544120698117, 1415.781883517263168, 209.6858483997482665 ) ) ;
#104784 = B_SPLINE_CURVE_WITH_KNOTS ( 'NONE', 5,
 ( #71340, #54529, #61282, #46671, #74061, #73516 ),
 .UNSPECIFIED., .F., .F.,
 ( 6, 6 ),
 ( 0.000000000000000000, 1.000000000000000000 ),
 .UNSPECIFIED. ) ;
#104785 = CARTESIAN_POINT ( 'NONE',  ( -10.23213401892603436, 1472.778035024365408, 208.9421871917756448 ) ) ;
#104786 = CARTESIAN_POINT ( 'NONE',  ( -11.75869035857540013, 1519.551704408389924, 190.9442076533970010 ) ) ;
#104787 = CARTESIAN_POINT ( 'NONE',  ( 9.561942892529945226, 1436.616837100986459, 211.5588262537796709 ) ) ;
#104788 = CARTESIAN_POINT ( 'NONE',  ( 14.92730988393499914, 1514.452905717119847, 225.3342559640670117 ) ) ;
#104789 = CARTESIAN_POINT ( 'NONE',  ( -12.53380394689999910, 1442.773887138329883, 185.9733701915980078 ) ) ;
#104790 = CARTESIAN_POINT ( 'NONE',  ( 21.40227409560650074, 1509.660444267860157, 229.5162084721659994 ) ) ;
#104791 = DIRECTION ( 'NONE',  ( -0.009376423277032341561, 0.9999478196825741794, -0.004054700802289810599 ) ) ;
#104792 = CARTESIAN_POINT ( 'NONE',  ( -0.9766393796380001824, 1453.313060387329870, 229.7750655478980093 ) ) ;
#104793 = CARTESIAN_POINT ( 'NONE',  ( 16.64350137070000102, 1410.411353414630184, 226.4950628044979908 ) ) ;
#104794 = CARTESIAN_POINT ( 'NONE',  ( -19.15298488520000220, 1464.559837765089924, 213.8319524061190009 ) ) ;
#104795 = CARTESIAN_POINT ( 'NONE',  ( -16.01735770899999878, 1459.144465034730047, 229.9898643770979731 ) ) ;
#104796 = CARTESIAN_POINT ( 'NONE',  ( -6.950833568235000648, 1517.156142772249950, 206.6378959915070084 ) ) ;
#104797 = CARTESIAN_POINT ( 'NONE',  ( 39.55285272340000091, 1422.351058411129998, 267.1954752406980447 ) ) ;
#104798 = CARTESIAN_POINT ( 'NONE',  ( -32.59719044532463528, 1523.982201850120191, 217.0485567930471120 ) ) ;
#104799 = CARTESIAN_POINT ( 'NONE',  ( 19.23474158209999985, 1436.402232428999923, 146.2239547538979991 ) ) ;
#104800 = CARTESIAN_POINT ( 'NONE',  ( 21.81674547060000080, 1488.582783796430022, 193.4203703249980038 ) ) ;
#104801 = CARTESIAN_POINT ( 'NONE',  ( 29.60476317767313148, 1509.968981583988352, 207.5719681184634169 ) ) ;
#104802 = CARTESIAN_POINT ( 'NONE',  ( -10.67458942334280003, 1390.939239166159950, 215.3172498179779666 ) ) ;
#104803 = CARTESIAN_POINT ( 'NONE',  ( 12.78752278269999998, 1416.843576368729828, 222.7044122178979819 ) ) ;
#104804 = CARTESIAN_POINT ( 'NONE',  ( -15.33452496817989896, 1418.116965089579935, 203.1099089491380028 ) ) ;
#104805 = CARTESIAN_POINT ( 'NONE',  ( 25.00977876991279913, 1436.598012848749931, 137.9330263815630246 ) ) ;
#104806 = CARTESIAN_POINT ( 'NONE',  ( -16.81497685297394895, 1526.382868172864164, 183.7037134202652169 ) ) ;
#104807 = CARTESIAN_POINT ( 'NONE',  ( -16.97980319039999841, 1414.913060387329779, 208.1309929760350315 ) ) ;
#104808 = CARTESIAN_POINT ( 'NONE',  ( -12.77622632179999940, 1442.825377011449973, 186.2636718277979924 ) ) ;
#104809 = DIRECTION ( 'NONE',  ( 0.000000000000000000, 1.000000000000000000, 0.000000000000000000 ) ) ;
#104810 = CARTESIAN_POINT ( 'NONE',  ( -33.14720771140000011, 1435.654777855230122, 135.5270110727979898 ) ) ;
#104811 = CARTESIAN_POINT ( 'NONE',  ( 1.713123635352999941, 1431.453930620565643, 200.4877085583662790 ) ) ;
#104812 = ORIENTED_EDGE ( 'NONE', *, *, #24961, .T. ) ;
#104813 = CARTESIAN_POINT ( 'NONE',  ( -4.026786250540000722, 1422.913060387330006, 179.5815723472979926 ) ) ;
#104814 = CARTESIAN_POINT ( 'NONE',  ( -2.224601527347340291, 1408.990745184500156, 223.9491347404019734 ) ) ;
#104815 = EDGE_CURVE ( 'NONE', #41956, #10275, #36206, .T. ) ;
#104816 = CARTESIAN_POINT ( 'NONE',  ( -13.58886547874749873, 1508.451091720879958, 209.7742548574910302 ) ) ;
#104817 = B_SPLINE_CURVE_WITH_KNOTS ( 'NONE', 3,
 ( #62260, #54412, #37579, #12365, #38123, #29179, #104234, #88009, #61707, #27522, #19665, #87441, #63370, #28629, #97485, #86876, #96389, #2904, #2360, #103681, #88544, #28072, #19097 ),
 .UNSPECIFIED., .F., .F.,
 ( 4, 2, 2, 2, 2, 2, 2, 2, 1, 2, 2, 4 ),
 ( 0.000000000000000000, 0.1250000000000727474, 0.1875000000000847378, 0.2500000000000967559, 0.3750000000001207368, 0.5000000000001447731, 0.6250000000001687539, 0.6875000000001788569, 0.7187500000000898170, 0.7343750000001433298, 0.7500000000001967315, 1.000000000000000000 ),
 .UNSPECIFIED. ) ;
#104818 = CARTESIAN_POINT ( 'NONE',  ( 21.38516915557986309, 1522.382868172863937, 237.8497028174237471 ) ) ;
#104819 = CARTESIAN_POINT ( 'NONE',  ( -37.49400285100000474, 1461.515165505230016, 269.0078955473979931 ) ) ;
#104820 = CARTESIAN_POINT ( 'NONE',  ( -11.87772997576320044, 1481.884250532160195, 209.0415709480480189 ) ) ;
#104821 = CARTESIAN_POINT ( 'NONE',  ( 0.2406210619857520050, 1420.498996480750066, 182.8345142462969761 ) ) ;
#104822 = EDGE_CURVE ( 'NONE', #38088, #22249, #57987, .T. ) ;
#104823 = CARTESIAN_POINT ( 'NONE',  ( -26.23322848259999773, 1508.580494355830069, 216.2666545556479889 ) ) ;
#104824 = CARTESIAN_POINT ( 'NONE',  ( -79.14789062195450242, 1384.640371133850067, 303.2828232109690134 ) ) ;
#104825 = CARTESIAN_POINT ( 'NONE',  ( -28.80985028338039911, 1384.966547565240262, 204.9440933951439945 ) ) ;
#104826 = CARTESIAN_POINT ( 'NONE',  ( 17.24529142091330058, 1423.692487554319996, 227.0492506374200161 ) ) ;
#104827 = CARTESIAN_POINT ( 'NONE',  ( 21.91792426430000162, 1509.678451168530273, 227.8819284608979956 ) ) ;
#104828 = CARTESIAN_POINT ( 'NONE',  ( -3.255911231930000316, 1435.946191916090129, 155.5160642224979881 ) ) ;
#104829 = AXIS2_PLACEMENT_3D ( 'NONE', #81195, #45973, #97461 ) ;
#104830 = CARTESIAN_POINT ( 'NONE',  ( -26.89242289587770074, 1508.005886644420116, 211.7458576771490186 ) ) ;
#104831 = CARTESIAN_POINT ( 'NONE',  ( 3.906019471690000078, 1515.551703594190030, 207.6331533119790151 ) ) ;
#104832 = CARTESIAN_POINT ( 'NONE',  ( -3.666700706489999906, 1509.114858798330033, 179.5219359138980053 ) ) ;
#104833 = DIRECTION ( 'NONE',  ( 0.7636119845598413614, -0.004098122786949555049, 0.6456624059260408499 ) ) ;
#104834 = CARTESIAN_POINT ( 'NONE',  ( 13.24264731299999909, 1414.971439108430104, 197.5210417955980233 ) ) ;
#104835 = CARTESIAN_POINT ( 'NONE',  ( -12.71459596929999947, 1416.274718422629803, 195.3550244208979905 ) ) ;
#104836 = ADVANCED_FACE ( 'NONE', ( #42955 ), #45178, .F. ) ;
#104837 = CARTESIAN_POINT ( 'NONE',  ( 11.72230831049659905, 1479.187001874789985, 208.0687465664710203 ) ) ;
#104838 = CARTESIAN_POINT ( 'NONE',  ( 22.70506338740000274, 1409.705938672130060, 209.2982490380130116 ) ) ;
#104839 = CARTESIAN_POINT ( 'NONE',  ( -106.8184672166400020, 1391.913060387289988, 306.2514081895690197 ) ) ;
#104840 = CARTESIAN_POINT ( 'NONE',  ( 8.241694428620000679, 1462.303391458189935, 228.8627610174989968 ) ) ;
#104841 = CARTESIAN_POINT ( 'NONE',  ( -16.28172202780000077, 1421.049848839029892, 227.0416102452980169 ) ) ;
#104842 = B_SPLINE_CURVE_WITH_KNOTS ( 'NONE', 5,
 ( #79652, #97535, #71833, #56088, #46605, #107581 ),
 .UNSPECIFIED., .F., .F.,
 ( 6, 6 ),
 ( -168.1723206030000028, -30.75981893479999485 ),
 .UNSPECIFIED. ) ;
#104844 = CARTESIAN_POINT ( 'NONE',  ( 21.38516915557964637, 1524.726013923371283, 180.3939891059721390 ) ) ;
#104843 = CARTESIAN_POINT ( 'NONE',  ( 11.90003109757362409, 1434.915657497907659, 147.6452320157113149 ) ) ;
#104845 = CARTESIAN_POINT ( 'NONE',  ( -4.994708985280000846, 1391.711004686890192, 203.7017277140789986 ) ) ;
#104846 = DIRECTION ( 'NONE',  ( 9.624611914481800761E-06, -0.9328681587603299130, 0.3602179871667691713 ) ) ;
#104847 = CARTESIAN_POINT ( 'NONE',  ( -11.00301372470000061, 1492.094802143589959, 210.0154403701209844 ) ) ;
#104848 = CARTESIAN_POINT ( 'NONE',  ( -23.36374832350000119, 1420.923074028029987, 211.0949373619980065 ) ) ;
#104849 = CARTESIAN_POINT ( 'NONE',  ( -9.978586514389998996, 1364.539968386210148, 210.6218459616991936 ) ) ;
#104850 = CARTESIAN_POINT ( 'NONE',  ( 6.548821941055000373, 1516.688761843659904, 205.0844676760469838 ) ) ;
#104851 = ADVANCED_FACE ( 'NONE', ( #70949 ), #50780, .T. ) ;
#104852 = FACE_OUTER_BOUND ( 'NONE', #106777, .T. ) ;
#104853 = CARTESIAN_POINT ( 'NONE',  ( 5.597770706110460459, 1506.679316021459954, 219.3685166263610142 ) ) ;
#104854 = CARTESIAN_POINT ( 'NONE',  ( -12.72386900654892017, 1421.513396326319935, 210.6452810979295975 ) ) ;
#104856 = ORIENTED_EDGE ( 'NONE', *, *, #109314, .F. ) ;
#104855 = CARTESIAN_POINT ( 'NONE',  ( -67.11452714873080083, 1379.744023253179876, 278.1888607204630262 ) ) ;
#104857 = ORIENTED_EDGE ( 'NONE', *, *, #103727, .T. ) ;
#104858 = CARTESIAN_POINT ( 'NONE',  ( 26.37675685490000177, 1508.582722881630161, 216.7139244022480113 ) ) ;
#104859 = ORIENTED_EDGE ( 'NONE', *, *, #61432, .F. ) ;
#104860 = CARTESIAN_POINT ( 'NONE',  ( -105.6288035359999924, 1378.913058700080001, 304.0441401731590076 ) ) ;
#104861 = EDGE_CURVE ( 'NONE', #23879, #101207, #80419, .T. ) ;
#104862 = CARTESIAN_POINT ( 'NONE',  ( 3.156166260290000025, 1466.544008048530031, 236.1241471695980181 ) ) ;
#104864 = CARTESIAN_POINT ( 'NONE',  ( 0.2427466632179999806, 1508.856333042329879, 179.8940944152980137 ) ) ;
#104863 = CARTESIAN_POINT ( 'NONE',  ( -15.71589887163418098, 1409.995731639605310, 226.4233246076490786 ) ) ;
#104865 = DIRECTION ( 'NONE',  ( 1.593356620438984032E-14, -0.7071067811865475727, -0.7071067811865475727 ) ) ;
#104866 = EDGE_CURVE ( 'NONE', #107054, #83948, #99402, .T. ) ;
#104867 = CARTESIAN_POINT ( 'NONE',  ( 4.651532691979999967, 1488.169727963030255, 182.7049705295980004 ) ) ;
#104868 = CARTESIAN_POINT ( 'NONE',  ( -106.0563520787330134, 1378.913060388819986, 305.4990271455400261 ) ) ;
#104869 = CARTESIAN_POINT ( 'NONE',  ( 6.936014448009999889, 1409.155271349029817, 229.3511990319979930 ) ) ;
#104870 = CARTESIAN_POINT ( 'NONE',  ( 0.000000000000000000, 0.000000000000000000, 0.000000000000000000 ) ) ;
#104871 = CARTESIAN_POINT ( 'NONE',  ( 4.624099291334999862, 1516.962555622980062, 212.3771868965270073 ) ) ;
#104872 = CARTESIAN_POINT ( 'NONE',  ( 39.90438676500410509, 1438.693166630719816, 134.0999999980629980 ) ) ;
#104873 = CARTESIAN_POINT ( 'NONE',  ( -11.37749809445980098, 1422.109346327800040, 209.6141660988719764 ) ) ;
#104874 = CARTESIAN_POINT ( 'NONE',  ( 10613.67162216127690, 54.28084071072816386, 5061.882847296718865 ) ) ;
#104875 = EDGE_LOOP ( 'NONE', ( #17597, #59586, #52627, #45405, #60694 ) ) ;
#104876 = CARTESIAN_POINT ( 'NONE',  ( 14.24929417786319874, 1435.536138497730008, 149.6993440739240100 ) ) ;
#104877 = CARTESIAN_POINT ( 'NONE',  ( -17.84645756668390248, 1442.885565304640295, 215.1978005858999836 ) ) ;
#104878 = ORIENTED_EDGE ( 'NONE', *, *, #24674, .F. ) ;
#104879 = EDGE_LOOP ( 'NONE', ( #81752, #12782, #40276, #61277, #40509 ) ) ;
#104880 = VERTEX_POINT ( 'NONE', #107260 ) ;
#104881 = EDGE_CURVE ( 'NONE', #38027, #81968, #41908, .T. ) ;
#104882 = CARTESIAN_POINT ( 'NONE',  ( -7.881533630355000319, 1511.927085655870087, 215.3995285225870191 ) ) ;
#104883 = CARTESIAN_POINT ( 'NONE',  ( 16.78028216998529132, 1513.363094769292047, 196.2862811899955204 ) ) ;
#104884 = CARTESIAN_POINT ( 'NONE',  ( 24.73993050763418822, 1450.821579931246333, 138.7998613157621719 ) ) ;
#104885 = CARTESIAN_POINT ( 'NONE',  ( -8.297843638769998975, 1384.899870798449911, 218.7036046513889858 ) ) ;
#104886 = CARTESIAN_POINT ( 'NONE',  ( 10.92857027410000015, 1460.888924372889960, 208.5047761330480114 ) ) ;
#104887 = EDGE_CURVE ( 'NONE', #95667, #94338, #37490, .T. ) ;
#104888 = CARTESIAN_POINT ( 'NONE',  ( -18.53161554139801126, 1445.630398175708706, 214.4691203362832539 ) ) ;
#104889 = CARTESIAN_POINT ( 'NONE',  ( -59.11373648366758715, 1379.721719983604544, 259.3782992626888131 ) ) ;
#104890 = CARTESIAN_POINT ( 'NONE',  ( 2.768534767419999820, 1465.332393548289929, 199.5050815057789748 ) ) ;
#104891 = B_SPLINE_CURVE_WITH_KNOTS ( 'NONE', 3,
 ( #73220, #64844, #56426, #90556, #88912, #5457, #62655, #97311, #88368, #11658 ),
 .UNSPECIFIED., .F., .F.,
 ( 4, 2, 2, 2, 4 ),
 ( -0.1573215296859830081, -0.1159487415761059903, -0.07685134973319139584, -0.03820936005390598855, -7.424679884793228268E-08 ),
 .UNSPECIFIED. ) ;
#104892 = DIRECTION ( 'NONE',  ( -1.755985294532469921E-16, 1.000000000000000000, -1.338183447452831989E-16 ) ) ;
#104893 = EDGE_LOOP ( 'NONE', ( #25383, #65224, #3241, #33450 ) ) ;
#104894 = CARTESIAN_POINT ( 'NONE',  ( -2.299983615734999987, 1516.861367446839949, 206.8392230197369770 ) ) ;
#104895 = ORIENTED_EDGE ( 'NONE', *, *, #87025, .T. ) ;
#104896 = CARTESIAN_POINT ( 'NONE',  ( 29.16429843505859765, 1440.913060387330006, 250.3001267888409984 ) ) ;
#104897 = CARTESIAN_POINT ( 'NONE',  ( -0.0001095867327352822572, 1452.800716251688982, 153.1161686451791013 ) ) ;
#104898 = VERTEX_POINT ( 'NONE', #106701 ) ;
#104899 = CARTESIAN_POINT ( 'NONE',  ( 26.25908477761629811, 1449.904608170299980, 136.7328078875380015 ) ) ;
#104900 = CARTESIAN_POINT ( 'NONE',  ( -13.92984420660000033, 1410.332022920429836, 190.1904693403979820 ) ) ;
#104901 = CARTESIAN_POINT ( 'NONE',  ( -45.22866404258923012, 1379.675374582019685, 237.0192218885333659 ) ) ;
#104902 = EDGE_CURVE ( 'NONE', #90951, #41783, #49967, .T. ) ;
#104904 = CARTESIAN_POINT ( 'NONE',  ( 28.27139721233038827, 1526.382868172863937, 198.6830693683571667 ) ) ;
#104903 = CARTESIAN_POINT ( 'NONE',  ( -24.90171366719999924, 1441.078953671579939, 210.4323502101080123 ) ) ;
#104905 = CARTESIAN_POINT ( 'NONE',  ( -11.60004869885203682, 1428.983126981193436, 134.0999999980979851 ) ) ;
#104906 = CARTESIAN_POINT ( 'NONE',  ( 0.0002411117317979708972, 1396.089785486056144, 197.2899115322371131 ) ) ;
#104907 = EDGE_CURVE ( 'NONE', #94625, #81986, #28538, .T. ) ;
#104908 = CARTESIAN_POINT ( 'NONE',  ( -11.87520966259999966, 1433.007090144579934, 149.2720797894980080 ) ) ;
#104909 = CARTESIAN_POINT ( 'NONE',  ( -3.462099826290000237, 1507.707684683789921, 221.1489180092989955 ) ) ;
#104911 = CARTESIAN_POINT ( 'NONE',  ( -3.138099469817183351, 1369.928451332881878, 207.8004044997916537 ) ) ;
#104910 = CARTESIAN_POINT ( 'NONE',  ( 7.657194240169999944, 1464.005168892129859, 233.8507629060979980 ) ) ;
#104912 = CARTESIAN_POINT ( 'NONE',  ( 0.7543881828220019292, 1516.727502608469877, 215.6727161143369926 ) ) ;
#104913 = EDGE_CURVE ( 'NONE', #7633, #56404, #52353, .T. ) ;
#104914 = B_SPLINE_CURVE_WITH_KNOTS ( 'NONE', 3,
 ( #9492, #86757, #1120, #61040, #25724, #77269, #11, #18420, #103550, #69435, #26284, #25170, #61579, #35250, #51503, #26852, #567, #34146, #86201, #34693, #1670, #95711, #76150, #95163, #52068, #94043, #52620, #68884, #67766 ),
 .UNSPECIFIED., .F., .F.,
 ( 4, 2, 2, 1, 1, 2, 2, 2, 2, 2, 2, 2, 1, 2, 2, 4 ),
 ( 0.000000000000000000, 0.2500000000000895950, 0.3750000000001428302, 0.4375000000001597056, 0.4687500000001595946, 0.4843750000001595946, 0.5000000000001595390, 0.6250000000001475486, 0.6875000000001415534, 0.7187500000001406653, 0.7500000000001397771, 0.8125000000001320055, 0.8437500000001281197, 0.8593750000001226796, 0.8750000000001172396, 1.000000000000000000 ),
 .UNSPECIFIED. ) ;
#104915 = DIRECTION ( 'NONE',  ( -1.755985294532469921E-16, 1.000000000000000000, -1.338183447452831989E-16 ) ) ;
#104916 = AXIS2_PLACEMENT_3D ( 'NONE', #34336, #35440, #68514 ) ;
#104917 = B_SPLINE_CURVE_WITH_KNOTS ( 'NONE', 3,
 ( #40706, #31197, #30653, #91658, #14933, #74336, #7107, #101141, #56419, #48577, #23882, #65384, #99487 ),
 .UNSPECIFIED., .F., .F.,
 ( 4, 2, 2, 2, 1, 2, 4 ),
 ( 0.000000000000000000, 0.09521579484686493178, 0.1428236922702973977, 0.1666276409821136339, 0.1785296153381099038, 0.1844806025161973007, 0.1904315896942847253 ),
 .UNSPECIFIED. ) ;
#104918 = FACE_OUTER_BOUND ( 'NONE', #68255, .T. ) ;
#104919 = CARTESIAN_POINT ( 'NONE',  ( -16.68463225901000158, 1442.773887286389936, 162.0935120915889911 ) ) ;
#104920 = CARTESIAN_POINT ( 'NONE',  ( 7.337153768115000751, 1517.119374999550018, 212.3815752680669959 ) ) ;
#104921 = CARTESIAN_POINT ( 'NONE',  ( -20.42020019299999944, 1470.816980701829834, 209.4971671475969970 ) ) ;
#104922 = CARTESIAN_POINT ( 'NONE',  ( 18.81609481059999922, 1456.479165729590022, 204.5196734937790097 ) ) ;
#104924 = ORIENTED_EDGE ( 'NONE', *, *, #42327, .F. ) ;
#104923 = CARTESIAN_POINT ( 'NONE',  ( -103.2203533160000006, 1390.533826207339871, 304.2968465863590382 ) ) ;
#104925 = DIRECTION ( 'NONE',  ( -9.138167445698339565E-47, 1.000000000000000000, -1.836970198721029688E-16 ) ) ;
#104926 = CARTESIAN_POINT ( 'NONE',  ( 3.897123952299999576E-10, 1465.695272585530120, 240.4142140030979817 ) ) ;
#104927 = CARTESIAN_POINT ( 'NONE',  ( 29.37542415142312535, 1526.382868172864164, 217.2587022579320433 ) ) ;
#104928 = CARTESIAN_POINT ( 'NONE',  ( -15.44036390149999960, 1415.706691406219988, 208.4181337457800112 ) ) ;
#104929 = CARTESIAN_POINT ( 'NONE',  ( -12.48995958582669985, 1501.883328869510024, 211.6213070116990025 ) ) ;
#104930 = CARTESIAN_POINT ( 'NONE',  ( -19.17279900190000319, 1457.063330234229852, 226.5609651273980205 ) ) ;
#104932 = CARTESIAN_POINT ( 'NONE',  ( 2.500000000000000000, 1419.623475504530006, 147.1347451145979903 ) ) ;
#104931 = CARTESIAN_POINT ( 'NONE',  ( -21.74576665880016080, 1411.032818084173414, 201.6082284287891468 ) ) ;
#104933 = CARTESIAN_POINT ( 'NONE',  ( -0.2254851406240000189, 1434.822352678220113, 190.2673095969979897 ) ) ;
#104934 = CARTESIAN_POINT ( 'NONE',  ( -106.5378846238329942, 1381.285095380909979, 309.2529097667930387 ) ) ;
#104935 = ORIENTED_EDGE ( 'NONE', *, *, #29505, .T. ) ;
#104936 = CARTESIAN_POINT ( 'NONE',  ( 2.868433798504999910, 1517.020727862619879, 204.1095288638669842 ) ) ;
#104937 = CARTESIAN_POINT ( 'NONE',  ( 2.771812352850000494, 1405.904361742329911, 267.2318186464980272 ) ) ;
#104938 = CARTESIAN_POINT ( 'NONE',  ( -1.486478317020000217, 1515.456929490889934, 213.2968315210090111 ) ) ;
#104939 = CARTESIAN_POINT ( 'NONE',  ( 13.37887548737149856, 1473.256433280859937, 270.1124100584160033 ) ) ;
#104940 = CARTESIAN_POINT ( 'NONE',  ( 5.465008655120000114, 1438.535486872679940, 154.7353332079979964 ) ) ;
#104941 = CARTESIAN_POINT ( 'NONE',  ( -19.83635568480000089, 1467.142385457190130, 209.5260977821610027 ) ) ;
#104942 = CARTESIAN_POINT ( 'NONE',  ( -37.81805297112759945, 1440.913060389500060, 255.9894328691030410 ) ) ;
#104943 = CARTESIAN_POINT ( 'NONE',  ( -26.50175984629999704, 1446.255663087950097, 137.5973547775980137 ) ) ;
#104944 = CARTESIAN_POINT ( 'NONE',  ( 3.375977085881459949, 1446.395221913229989, 199.5681764770490076 ) ) ;
#104945 = CARTESIAN_POINT ( 'NONE',  ( 1.662851635919999849, 1431.604427083889959, 200.5143776403489824 ) ) ;
#104946 = CARTESIAN_POINT ( 'NONE',  ( -15.94166200583058490, 1416.020774055787342, 209.6543190501261620 ) ) ;
#104947 = CARTESIAN_POINT ( 'NONE',  ( 3.554299344259999938, 1505.806595535689894, 220.9721874952989822 ) ) ;
#104948 = DIRECTION ( 'NONE',  ( 0.000000000000000000, 1.000000000000000000, 0.000000000000000000 ) ) ;
#104949 = ORIENTED_EDGE ( 'NONE', *, *, #55715, .F. ) ;
#104950 = CARTESIAN_POINT ( 'NONE',  ( -43.50000000000000000, 1435.965051957929973, 271.1218459616979999 ) ) ;
#104951 = EDGE_CURVE ( 'NONE', #85993, #95247, #92663, .T. ) ;
#104953 = CARTESIAN_POINT ( 'NONE',  ( -14.38276615812611681, 1514.413060387330006, 182.7943691049868278 ) ) ;
#104952 = APPLICATION_CONTEXT ( 'automotive_design' ) ;
#104954 = CARTESIAN_POINT ( 'NONE',  ( -0.2151320649219999881, 1475.759570378829949, 269.0456880799980013 ) ) ;
#104955 = CARTESIAN_POINT ( 'NONE',  ( -13.53916864874639892, 1429.119333790580185, 222.2883575635510169 ) ) ;
#104956 = CARTESIAN_POINT ( 'NONE',  ( -27.96976557860000057, 1509.201555289429962, 210.6640596492780162 ) ) ;
#104957 = CARTESIAN_POINT ( 'NONE',  ( -3.579852315081284431, 1448.290319961710338, 184.9158413581277500 ) ) ;
#104958 = CARTESIAN_POINT ( 'NONE',  ( -14.82216926960470182, 1384.877475996390103, 219.3981822003099751 ) ) ;
#104959 = VECTOR ( 'NONE', #63946, 1000.000000000000000 ) ;
#104960 = CARTESIAN_POINT ( 'NONE',  ( -17.77615777719999812, 1415.140114695929924, 207.9728109415779898 ) ) ;
#104961 = DIRECTION ( 'NONE',  ( 0.000000000000000000, 0.000000000000000000, -1.000000000000000000 ) ) ;
#104962 = CARTESIAN_POINT ( 'NONE',  ( 26.42721169618110011, 1435.958680060049801, 136.4983543512450126 ) ) ;
#104963 = CARTESIAN_POINT ( 'NONE',  ( -9.715427105718768885, 1396.252330577819976, 214.4129421473980130 ) ) ;
#104964 = CARTESIAN_POINT ( 'NONE',  ( -15.80894304229999925, 1421.035217125530153, 227.0411593344980190 ) ) ;
#104965 = ADVANCED_FACE ( 'NONE', ( #21582 ), #32860, .F. ) ;
#104966 = CARTESIAN_POINT ( 'NONE',  ( -17.33018476747690073, 1410.462527268070062, 225.7401589819789933 ) ) ;
#104967 = CARTESIAN_POINT ( 'NONE',  ( 11.88140585900000090, 1433.447543843229823, 147.6490162021979984 ) ) ;
#104968 = VERTEX_POINT ( 'NONE', #57980 ) ;
#104969 = CARTESIAN_POINT ( 'NONE',  ( -11.40035806272144470, 1501.109170488654854, 208.2596098937023328 ) ) ;
#104970 = CARTESIAN_POINT ( 'NONE',  ( -13.58909363943140036, 1508.363827828459989, 209.7584773189200007 ) ) ;
#104971 = CARTESIAN_POINT ( 'NONE',  ( -8.348318400919996662, 1484.298477954530199, 184.3911661821975372 ) ) ;
#104973 = CARTESIAN_POINT ( 'NONE',  ( -9.978796886447030445, 1439.268830739550140, 208.9290397175849989 ) ) ;
#104972 = CARTESIAN_POINT ( 'NONE',  ( 10.81150411640000009, 1425.669232956329779, 101.9066733906980033 ) ) ;
#104974 = CARTESIAN_POINT ( 'NONE',  ( -0.3155435254770000419, 1483.118057600029942, 236.2956536266979981 ) ) ;
#104975 = ADVANCED_FACE ( 'NONE', ( #99949 ), #57443, .T. ) ;
#104976 = CARTESIAN_POINT ( 'NONE',  ( -13.51610093808350577, 1445.063428794548372, 205.0760988357350527 ) ) ;
#104977 = CARTESIAN_POINT ( 'NONE',  ( 2.872836622524999939, 1517.158319634930194, 201.3964737998670103 ) ) ;
#104978 = CARTESIAN_POINT ( 'NONE',  ( 7.957350483939999108, 1425.611849966230011, 211.5358269577189958 ) ) ;
#104980 = CARTESIAN_POINT ( 'NONE',  ( 14.17511973000000047, 1428.761297070790079, 195.0897165316990254 ) ) ;
#104979 = AXIS2_PLACEMENT_3D ( 'NONE', #101444, #18000, #42672 ) ;
#104981 = CARTESIAN_POINT ( 'NONE',  ( 2.360320924850000335, 1507.942448366130066, 181.1000475259980078 ) ) ;
#104982 = CARTESIAN_POINT ( 'NONE',  ( 7.618904756804999678, 1511.873873588870083, 206.4967791623069786 ) ) ;
#104983 = CARTESIAN_POINT ( 'NONE',  ( -54.29131571383740607, 1379.936403459110124, 253.6537993308690204 ) ) ;
#104984 = CARTESIAN_POINT ( 'NONE',  ( 10.02176186329304031, 1364.879735892739745, 210.6218459616987957 ) ) ;
#104986 = ORIENTED_EDGE ( 'NONE', *, *, #41792, .F. ) ;
#104985 = CARTESIAN_POINT ( 'NONE',  ( 7.695178307639999993, 1454.153012403389994, 215.2868595619190160 ) ) ;
#104987 = VERTEX_POINT ( 'NONE', #14294 ) ;
#104988 = CARTESIAN_POINT ( 'NONE',  ( 0.07608147880745361191, 1490.951086335209993, 236.6948437218040056 ) ) ;
#104989 = CARTESIAN_POINT ( 'NONE',  ( 3.679272716979999913, 1453.313060387329870, 228.5941172881979924 ) ) ;
#104990 = CARTESIAN_POINT ( 'NONE',  ( -1.213893508954652534, 1442.512427547091193, 200.3199665731655443 ) ) ;
#104991 =( BOUNDED_CURVE ( )  B_SPLINE_CURVE ( 3, ( #15189, #109285, #84062, #32570 ),
 .UNSPECIFIED., .F., .F. ) 
 B_SPLINE_CURVE_WITH_KNOTS ( ( 4, 4 ),
 ( 4.177675961634177426, 5.247004545667287800 ),
 .UNSPECIFIED. ) 
 CURVE ( )  GEOMETRIC_REPRESENTATION_ITEM ( )  RATIONAL_B_SPLINE_CURVE ( ( 1.000000000000000000, 0.9069598256684616722, 0.9069598256684616722, 1.000000000000000000 ) ) 
 REPRESENTATION_ITEM ( '' )  );
#104993 = CARTESIAN_POINT ( 'NONE',  ( 0.1287657911039999936, 1486.015939899330078, 182.0783122775980303 ) ) ;
#104992 = CARTESIAN_POINT ( 'NONE',  ( -8.066920486049999894, 1384.201370995469915, 218.7301529432190250 ) ) ;
#104994 = CARTESIAN_POINT ( 'NONE',  ( 21.40470761700000324, 1507.840874668130027, 191.1187993005979990 ) ) ;
#104995 = EDGE_CURVE ( 'NONE', #91781, #79695, #105443, .T. ) ;
#104996 = CARTESIAN_POINT ( 'NONE',  ( -2.603434334352570101, 1463.518582721570056, 199.6736037120420235 ) ) ;
#104997 = CARTESIAN_POINT ( 'NONE',  ( 16.66936639845652479, 1523.456872492435195, 237.7608804993219280 ) ) ;
#104998 = SURFACE_STYLE_USAGE ( .BOTH. , #79812 ) ;
#104999 = CARTESIAN_POINT ( 'NONE',  ( 3.876049381683142059, 1447.746239516663763, 184.2268197018375133 ) ) ;
#105000 = CARTESIAN_POINT ( 'NONE',  ( 3.173741429363529321, 1370.393155323753945, 210.6218459617030021 ) ) ;
#105001 = CARTESIAN_POINT ( 'NONE',  ( 12.15678282470000049, 1407.401676941830146, 215.7644370117779999 ) ) ;
#105002 = CARTESIAN_POINT ( 'NONE',  ( -1.533256472543610194, 1405.729012779230061, 267.8533381434389753 ) ) ;
#105003 = EDGE_CURVE ( 'NONE', #110691, #52986, #74058, .T. ) ;
#105004 = CARTESIAN_POINT ( 'NONE',  ( 41.66090683250000382, 1443.836063800979900, 135.6920700532980106 ) ) ;
#105005 = ORIENTED_EDGE ( 'NONE', *, *, #1154, .T. ) ;
#105006 = CARTESIAN_POINT ( 'NONE',  ( 3.919202604670000145, 1440.900018029090006, 218.2279973031590146 ) ) ;
#105007 = CARTESIAN_POINT ( 'NONE',  ( 20.88377839294442495, 1525.556090473946824, 233.6619242631579141 ) ) ;
#105008 = ORIENTED_EDGE ( 'NONE', *, *, #104913, .F. ) ;
#105009 = ORIENTED_EDGE ( 'NONE', *, *, #100474, .T. ) ;
#105010 = EDGE_CURVE ( 'NONE', #93315, #100437, #21839, .T. ) ;
#105011 = CARTESIAN_POINT ( 'NONE',  ( -3.264931758469999945, 1455.156802322290105, 200.1463041844289990 ) ) ;
#105012 = CARTESIAN_POINT ( 'NONE',  ( 5.604365146370000161, 1361.139420828410039, 207.6218459616989946 ) ) ;
#105013 = AXIS2_PLACEMENT_3D ( 'NONE', #74358, #108486, #110134 ) ;
#105014 = CARTESIAN_POINT ( 'NONE',  ( -6.550389470255000290, 1516.755758396839838, 214.1281755516169767 ) ) ;
#105015 = CARTESIAN_POINT ( 'NONE',  ( 2.701540375215000012, 1511.422242621320265, 216.6970128893269987 ) ) ;
#105016 = EDGE_CURVE ( 'NONE', #45663, #46504, #107348, .T. ) ;
#105017 = ORIENTED_EDGE ( 'NONE', *, *, #55442, .T. ) ;
#105018 = CARTESIAN_POINT ( 'NONE',  ( 0.000000000000000000, 1420.584111001019892, 209.1218459616989946 ) ) ;
#105019 = CARTESIAN_POINT ( 'NONE',  ( -101.9775983549999978, 1375.414493452870147, 301.8221755499590699 ) ) ;
#105020 = CARTESIAN_POINT ( 'NONE',  ( -105.9034084253929962, 1378.913060387329779, 303.2380501759690219 ) ) ;
#105021 = CARTESIAN_POINT ( 'NONE',  ( 4.999456390405000228, 1516.830644417779922, 204.5005780481670001 ) ) ;
#105022 = CARTESIAN_POINT ( 'NONE',  ( -12.22915601319570200, 1490.209347939349982, 209.7391394842479997 ) ) ;
#105023 = CARTESIAN_POINT ( 'NONE',  ( -92.78539381950000120, 1384.966825520919883, 294.1434271777590084 ) ) ;
#105024 = CARTESIAN_POINT ( 'NONE',  ( -2.291047527245000381, 1516.524310051880093, 201.4130759250869858 ) ) ;
#105025 = CARTESIAN_POINT ( 'NONE',  ( -5.993306093509999322, 1410.496812455530062, 231.4967973790980125 ) ) ;
#105027 = VERTEX_POINT ( 'NONE', #66938 ) ;
#105026 = CARTESIAN_POINT ( 'NONE',  ( -8.927951907720000690, 1446.111221346229968, 185.7534680273980143 ) ) ;
#105028 = ADVANCED_FACE ( 'NONE', ( #75871 ), #24818, .F. ) ;
#105029 = LINE ( 'NONE', #87690, #110146 ) ;
#105030 = CARTESIAN_POINT ( 'NONE',  ( -24.78096948487849716, 1440.913060472049892, 214.6184464147330004 ) ) ;
#105032 = CARTESIAN_POINT ( 'NONE',  ( 19.91074080903766230, 1526.211528530236592, 233.5136342147586674 ) ) ;
#105031 = AXIS2_PLACEMENT_3D ( 'NONE', #88536, #3442, #108492 ) ;
#105033 = CARTESIAN_POINT ( 'NONE',  ( 15.57930626881383063, 1506.606278689549981, 224.8356771238971703 ) ) ;
#105034 = CARTESIAN_POINT ( 'NONE',  ( -25.67043386000000282, 1436.190963422269988, 136.9403443359979917 ) ) ;
#105035 = CARTESIAN_POINT ( 'NONE',  ( 41.09353168516779675, 1432.680545450300087, 269.6304333787269911 ) ) ;
#105036 = EDGE_CURVE ( 'NONE', #69912, #53899, #35519, .T. ) ;
#105037 = CARTESIAN_POINT ( 'NONE',  ( -7.709681306425000713, 1516.559109716219837, 211.9945464874270158 ) ) ;
#105038 = CARTESIAN_POINT ( 'NONE',  ( -68.02027221699999870, 1379.746446890080051, 278.4719343715589730 ) ) ;
#105039 = AXIS2_PLACEMENT_3D ( 'NONE', #17196, #34589, #18871 ) ;
#105040 = DIRECTION ( 'NONE',  ( -0.4882662618185321102, -0.4884709562387601345, 0.7231819843448452634 ) ) ;
#105041 = CARTESIAN_POINT ( 'NONE',  ( 8.294124457724750599, 1425.422146639270068, 193.1250435841020021 ) ) ;
#105042 = CARTESIAN_POINT ( 'NONE',  ( 19.12713426963480146, 1496.834684404690051, 222.0421991225989871 ) ) ;
#105043 = CARTESIAN_POINT ( 'NONE',  ( -1.906501101195560124E-08, 1517.020990152690047, 209.1218459511669892 ) ) ;
#105044 = EDGE_LOOP ( 'NONE', ( #28428, #22119, #11778 ) ) ;
#105045 = CARTESIAN_POINT ( 'NONE',  ( -1.757532416683340148, 1451.933574871519795, 184.1885909450070073 ) ) ;
#105046 = CARTESIAN_POINT ( 'NONE',  ( -6.511472450310000326, 1415.369202044029862, 231.5173866912979861 ) ) ;
#105047 = CARTESIAN_POINT ( 'NONE',  ( -49.58793988690000276, 1384.741903095260113, 260.9101892837590526 ) ) ;
#105048 = ORIENTED_EDGE ( 'NONE', *, *, #91702, .F. ) ;
#105049 = CARTESIAN_POINT ( 'NONE',  ( -21.77341892320420058, 1385.269227909690017, 221.7389472576159903 ) ) ;
#105050 = CARTESIAN_POINT ( 'NONE',  ( -2.941234743340000346, 1429.809722365389916, 201.2044919420790166 ) ) ;
#105051 = CARTESIAN_POINT ( 'NONE',  ( 12.57300769832470166, 1478.702740668469914, 232.0245263613259965 ) ) ;
#105052 = DIRECTION ( 'NONE',  ( 0.4025563316115431389, 0.03449475076686812219, 0.9147450530333514074 ) ) ;
#105053 = DIRECTION ( 'NONE',  ( 0.4794255386042030054, 0.000000000000000000, 0.8775825618903727587 ) ) ;
#105054 = CARTESIAN_POINT ( 'NONE',  ( -0.1940356176690000156, 1409.861619114730047, 233.2114736749980182 ) ) ;
#105055 = CARTESIAN_POINT ( 'NONE',  ( -16.19492410460000187, 1409.478599598930032, 217.9908631324380224 ) ) ;
#105057 = CARTESIAN_POINT ( 'NONE',  ( -0.02062249914556560024, 1508.912340185780067, 235.3515326150290150 ) ) ;
#105056 = CARTESIAN_POINT ( 'NONE',  ( -3.452289220704999551, 1517.069378699710114, 215.6835323934670328 ) ) ;
#105058 = CYLINDRICAL_SURFACE ( 'NONE', #69320, 2.000000000000003109 ) ;
#105059 = CARTESIAN_POINT ( 'NONE',  ( 9.905209297491678555, 1468.559939475269857, 207.6655895676410069 ) ) ;
#105060 = AXIS2_PLACEMENT_3D ( 'NONE', #81929, #4149, #64064 ) ;
#105061 = ORIENTED_EDGE ( 'NONE', *, *, #80850, .T. ) ;
#105062 = CARTESIAN_POINT ( 'NONE',  ( -10.86245182433490086, 1414.913060387399810, 196.8063316368690039 ) ) ;
#105063 = CARTESIAN_POINT ( 'NONE',  ( -20.20633738500000121, 1495.113783644630075, 189.9444582722979931 ) ) ;
#105064 = ORIENTED_EDGE ( 'NONE', *, *, #49384, .F. ) ;
#105065 = CARTESIAN_POINT ( 'NONE',  ( 7.654614188889650173, 1489.887865978259924, 207.9968767246130028 ) ) ;
#105066 = CARTESIAN_POINT ( 'NONE',  ( 9.788842362726176916, 1435.966427250319612, 152.6339651303872245 ) ) ;
#105067 = CARTESIAN_POINT ( 'NONE',  ( 7.596320571148669210, 1510.929912129050081, 203.3182735752830013 ) ) ;
#105068 = CARTESIAN_POINT ( 'NONE',  ( 3.001614222390000197, 1441.369934486689999, 218.5760139890790299 ) ) ;
#105069 = CARTESIAN_POINT ( 'NONE',  ( -34.68852446352950381, 1522.382868172863937, 199.9946320047955624 ) ) ;
#105070 = CARTESIAN_POINT ( 'NONE',  ( -1970.639179128770138, -8387.357407334289746, 1.374729025600770038 ) ) ;
#105071 = CARTESIAN_POINT ( 'NONE',  ( -2.500000000000000000, 1448.989771683439812, 154.5778230850980037 ) ) ;
#105072 = CARTESIAN_POINT ( 'NONE',  ( -17.72524821669999895, 1424.247088718729856, 226.5195189683980175 ) ) ;
#105073 = CARTESIAN_POINT ( 'NONE',  ( -19.66037016059999942, 1436.416578655439935, 145.8483816223979943 ) ) ;
#105074 = CARTESIAN_POINT ( 'NONE',  ( -2.451271202390000070, 1433.447543843880112, 150.3250444719979839 ) ) ;
#105075 = CARTESIAN_POINT ( 'NONE',  ( 17.37020517850000090, 1428.766723024330076, 191.2625755937980045 ) ) ;
#105077 = CARTESIAN_POINT ( 'NONE',  ( 4.329200639848810539, 1515.074268821609849, 207.6257481534460112 ) ) ;
#105076 = CARTESIAN_POINT ( 'NONE',  ( 0.8389417669273790956, 1409.109435131980035, 232.3914498246509766 ) ) ;
#105078 = CARTESIAN_POINT ( 'NONE',  ( -19.53786426059057746, 1512.187213306747481, 181.5239794925695946 ) ) ;
#105079 = ORIENTED_EDGE ( 'NONE', *, *, #44206, .F. ) ;
#105080 = CARTESIAN_POINT ( 'NONE',  ( 14.75914027823870001, 1489.809285284449970, 193.8265667301440089 ) ) ;
#105081 = CARTESIAN_POINT ( 'NONE',  ( 23.79022469739999934, 1430.448705190130113, 207.1593330058379934 ) ) ;
#105082 = CIRCLE ( 'NONE', #106824, 9.500000000000008882 ) ;
#105083 = CARTESIAN_POINT ( 'NONE',  ( -23.94935474710000278, 1437.296773319940030, 211.9556018033580074 ) ) ;
#105084 = CARTESIAN_POINT ( 'NONE',  ( -5.301886427999999540, 1484.919761519890017, 198.4532048381990137 ) ) ;
#105085 = CARTESIAN_POINT ( 'NONE',  ( -18.51562429780000230, 1509.322649224630140, 230.4822182655979645 ) ) ;
#105086 = CARTESIAN_POINT ( 'NONE',  ( -2.471036798109852217, 1525.556089352344543, 241.2503651499576165 ) ) ;
#105087 = CARTESIAN_POINT ( 'NONE',  ( -11.14671771210699980, 1434.019356486030119, 151.6529807626459956 ) ) ;
#105088 = CARTESIAN_POINT ( 'NONE',  ( 26.79413740735880367, 1436.761939593030093, 136.7822073642480234 ) ) ;
#105089 = CARTESIAN_POINT ( 'NONE',  ( -7.559010200133819524, 1510.805212306365547, 214.6182763928821657 ) ) ;
#105090 = CARTESIAN_POINT ( 'NONE',  ( -10.22907582296480200, 1490.127153888709927, 213.4824587814819665 ) ) ;
#105091 = CARTESIAN_POINT ( 'NONE',  ( 10.99043244679999987, 1479.494642110589893, 229.8297439418990109 ) ) ;
#105092 = CARTESIAN_POINT ( 'NONE',  ( -81.76652289506799320, 1383.775734044670116, 304.7570926416640305 ) ) ;
#105093 = B_SPLINE_CURVE_WITH_KNOTS ( 'NONE', 5,
 ( #64283, #46935, #90552, #6004, #39612, #22223, #65386, #12753, #81592 ),
 .UNSPECIFIED., .F., .F.,
 ( 6, 3, 6 ),
 ( 91.71614156710000998, 91.73016858649999961, 101.6051519397803986 ),
 .UNSPECIFIED. ) ;
#105094 = CARTESIAN_POINT ( 'NONE',  ( -109.5071830355930018, 1383.951130388469892, 311.2194437626960166 ) ) ;
#105095 = DIRECTION ( 'NONE',  ( -0.3363363969979660806, 0.9417419115949053898, 0.000000000000000000 ) ) ;
#105096 = CARTESIAN_POINT ( 'NONE',  ( 4.737752338079999959, 1428.052317588289952, 215.9265451789589747 ) ) ;
#105098 = ORIENTED_EDGE ( 'NONE', *, *, #29151, .F. ) ;
#105097 = CARTESIAN_POINT ( 'NONE',  ( -18.82420833825850437, 1444.120425544869931, 209.6987789698510198 ) ) ;
#105099 = DIRECTION ( 'NONE',  ( -5.980589973904019347E-17, 1.000000000000000000, -1.736889445713099699E-16 ) ) ;
#105100 = CARTESIAN_POINT ( 'NONE',  ( -92.77130722430000276, 1383.377570089289748, 294.1770395593590024 ) ) ;
#105101 = CARTESIAN_POINT ( 'NONE',  ( 30.31052258194597115, 1523.604703353109699, 222.4930856806589929 ) ) ;
#105102 = ORIENTED_EDGE ( 'NONE', *, *, #83005, .F. ) ;
#105103 = ORIENTED_EDGE ( 'NONE', *, *, #108310, .F. ) ;
#105104 = CARTESIAN_POINT ( 'NONE',  ( 31.81407709660776817, 1522.862737210649584, 221.9534378623329474 ) ) ;
#105105 = CARTESIAN_POINT ( 'NONE',  ( -109.5353424460000014, 1384.935512065160083, 297.1231347603589938 ) ) ;
#105106 = CARTESIAN_POINT ( 'NONE',  ( 12.66098461250295593, 1442.798989634974077, 169.4635270419445305 ) ) ;
#105108 = CARTESIAN_POINT ( 'NONE',  ( -45.67178389499999724, 1440.913060392759917, 266.1886045325979921 ) ) ;
#105107 = CARTESIAN_POINT ( 'NONE',  ( 29.82646034656356093, 1419.449848292917295, 269.4689676523768753 ) ) ;
#105109 = B_SPLINE_CURVE_WITH_KNOTS ( 'NONE', 5,
 ( #27887, #62070, #70473, #78856, #11637, #2165 ),
 .UNSPECIFIED., .F., .F.,
 ( 6, 6 ),
 ( 0.000000000000000000, 1.000000000000000000 ),
 .UNSPECIFIED. ) ;
#105110 = CARTESIAN_POINT ( 'NONE',  ( 9.014726288018540146, 1435.931555954980013, 208.8389660296269881 ) ) ;
#105111 = TOROIDAL_SURFACE ( 'NONE', #56840, 1.000000000000000000, 1.000000000000000000 ) ;
#105112 = CARTESIAN_POINT ( 'NONE',  ( -11.59421085610000013, 1433.816539371060117, 151.1950375012979748 ) ) ;
#105113 = CARTESIAN_POINT ( 'NONE',  ( 11.53661564504106174, 1502.557334605151937, 209.2924327149770534 ) ) ;
#105114 = CARTESIAN_POINT ( 'NONE',  ( -19.19076381549999866, 1485.870189056229719, 189.6692896468980223 ) ) ;
#105115 = CARTESIAN_POINT ( 'NONE',  ( 22.75273496409577945, 1511.187213306747708, 183.6728937936772184 ) ) ;
#105116 = CARTESIAN_POINT ( 'NONE',  ( 4.363122647530000009, 1421.971318475729959, 183.8271339139979830 ) ) ;
#105117 = CARTESIAN_POINT ( 'NONE',  ( -9.273216395669999557, 1438.130896815179995, 153.0611341270980006 ) ) ;
#105118 = CARTESIAN_POINT ( 'NONE',  ( -9.103468112560660686, 1449.499701819690017, 210.3008494512589834 ) ) ;
#105119 = DIRECTION ( 'NONE',  ( 0.2829264727638239885, 0.3709838398322150010, 0.8844905887530780664 ) ) ;
#105120 = AXIS2_PLACEMENT_3D ( 'NONE', #11889, #80746, #87501 ) ;
#105121 = B_SPLINE_CURVE_WITH_KNOTS ( 'NONE', 5,
 ( #95970, #44477, #110558, #34405, #68578, #87011, #59618, #25978, #9750, #78623, #60177, #52883 ),
 .UNSPECIFIED., .F., .F.,
 ( 6, 3, 3, 6 ),
 ( -8.912489289850000773, -7.801458206509999549, -6.062162762939999894, -3.672001930560000460 ),
 .UNSPECIFIED. ) ;
#105122 = CARTESIAN_POINT ( 'NONE',  ( 2.596261494520225366, 1525.907212628473644, 240.7735774411713123 ) ) ;
#105124 = ORIENTED_EDGE ( 'NONE', *, *, #100983, .F. ) ;
#105123 = DIRECTION ( 'NONE',  ( -0.6736849260863841948, 0.000000000000000000, 0.7390186874254148774 ) ) ;
#105125 = VERTEX_POINT ( 'NONE', #94877 ) ;
#105126 = CARTESIAN_POINT ( 'NONE',  ( -3.788285567717010416, 1508.728291974460035, 213.4250882028100023 ) ) ;
#105127 = CARTESIAN_POINT ( 'NONE',  ( -4.179417150059999919, 1482.939659495389833, 231.1991619290989775 ) ) ;
#105128 = CARTESIAN_POINT ( 'NONE',  ( -14.76285983090000187, 1469.689762253530034, 269.6387426946980099 ) ) ;
#105129 = CARTESIAN_POINT ( 'NONE',  ( 11.16376535829999916, 1420.610325767149789, 198.7943618068990190 ) ) ;
#105130 = CARTESIAN_POINT ( 'NONE',  ( 6.558760908210000906, 1438.201672707379885, 154.7769642619979891 ) ) ;
#105131 = CARTESIAN_POINT ( 'NONE',  ( -15.51935360190000068, 1506.809279358730009, 224.7680893556980095 ) ) ;
#105132 = EDGE_CURVE ( 'NONE', #57779, #36364, #62549, .T. ) ;
#105133 = EDGE_CURVE ( 'NONE', #40151, #30075, #55215, .T. ) ;
#105134 = CARTESIAN_POINT ( 'NONE',  ( 3.444951101639869950, 1484.732918568139894, 220.4578280794839884 ) ) ;
#105135 = CARTESIAN_POINT ( 'NONE',  ( -9.649970257700001497, 1460.854139312389862, 213.4680788249189902 ) ) ;
#105136 = CARTESIAN_POINT ( 'NONE',  ( 7.671300932945157136, 1359.787265839942847, 209.6218459617033432 ) ) ;
#105137 = CARTESIAN_POINT ( 'NONE',  ( -44.85754428203180311, 1434.551014250809885, 268.9966666965190143 ) ) ;
#105138 = VERTEX_POINT ( 'NONE', #27130 ) ;
#105139 = CARTESIAN_POINT ( 'NONE',  ( -7.999790656699999225, 1424.877929483370053, 210.4221880905789988 ) ) ;
#105140 = ORIENTED_EDGE ( 'NONE', *, *, #4401, .T. ) ;
#105141 = CARTESIAN_POINT ( 'NONE',  ( 2.881325373965000214, 1517.003078582959688, 210.2407492406470055 ) ) ;
#105142 = CARTESIAN_POINT ( 'NONE',  ( -9.828024340748898524, 1446.801136768030119, 212.2328356403849909 ) ) ;
#105143 = CIRCLE ( 'NONE', #85446, 1.999999999999997780 ) ;
#105144 = CARTESIAN_POINT ( 'NONE',  ( -3.829619994797929916, 1515.551704292389786, 210.9648097401420159 ) ) ;
#105145 = CARTESIAN_POINT ( 'NONE',  ( -14.18063018520000007, 1425.417875233729774, 189.5894151879979859 ) ) ;
#105146 = ADVANCED_FACE ( 'NONE', ( #95435 ), #51808, .F. ) ;
#105147 = CARTESIAN_POINT ( 'NONE',  ( -27.02986278700840117, 1451.800463763470134, 135.6518028302020014 ) ) ;
#105148 = ORIENTED_EDGE ( 'NONE', *, *, #33180, .F. ) ;
#105149 = FACE_OUTER_BOUND ( 'NONE', #90447, .T. ) ;
#105150 = B_SPLINE_CURVE_WITH_KNOTS ( 'NONE', 3,
 ( #49608, #38426, #4823, #30584, #82081, #5385, #100537, #98335, #39542, #74809, #89933, #58009, #66421, #64213, #13210, #73716 ),
 .UNSPECIFIED., .F., .F.,
 ( 4, 3, 3, 3, 3, 4 ),
 ( -7.276681342242609318, -6.842771595400160223, -5.875983249300730016, -4.912620469295280401, -3.950810556825589792, -2.991101461899999592 ),
 .UNSPECIFIED. ) ;
#105151 = CARTESIAN_POINT ( 'NONE',  ( 1.126138108584999964, 1517.208444099459939, 201.3951612445669923 ) ) ;
#105152 = B_SPLINE_CURVE_WITH_KNOTS ( 'NONE', 5,
 ( #92938, #40882, #8371, #76693, #25164, #40332 ),
 .UNSPECIFIED., .F., .F.,
 ( 6, 6 ),
 ( 0.000000000000000000, 1.000000000000000000 ),
 .UNSPECIFIED. ) ;
#105153 = CARTESIAN_POINT ( 'NONE',  ( 9.014562907850001139, 1470.471472073790210, 213.7600426553289878 ) ) ;
#105154 = CARTESIAN_POINT ( 'NONE',  ( 8.456465142934460388, 1517.051704408389924, 223.1002094411418284 ) ) ;
#105155 = ORIENTED_EDGE ( 'NONE', *, *, #79640, .F. ) ;
#105156 = CARTESIAN_POINT ( 'NONE',  ( -25.77614403568950152, 1416.582427450090108, 269.6950798014430006 ) ) ;
#105157 = CARTESIAN_POINT ( 'NONE',  ( 7.326072144144999854, 1516.714320817460020, 208.3685457967989976 ) ) ;
#105158 = DIRECTION ( 'NONE',  ( -1.755985294532469921E-16, 1.000000000000000000, -1.338183447452831989E-16 ) ) ;
#105159 = CARTESIAN_POINT ( 'NONE',  ( 8.977976324442520806, 1435.738830198290088, 208.3991943294609825 ) ) ;
#105161 = VERTEX_POINT ( 'NONE', #45057 ) ;
#105160 = CARTESIAN_POINT ( 'NONE',  ( -8.962252599314020074, 1366.920250605834099, 210.6218459616987957 ) ) ;
#105162 = VERTEX_POINT ( 'NONE', #70271 ) ;
#105163 = B_SPLINE_CURVE_WITH_KNOTS ( 'NONE', 3,
 ( #64532, #21913, #56109, #90241, #13523, #19742 ),
 .UNSPECIFIED., .F., .F.,
 ( 4, 2, 4 ),
 ( 0.000000000000000000, 0.5000000000000000000, 1.000000000000000000 ),
 .UNSPECIFIED. ) ;
#105164 = CARTESIAN_POINT ( 'NONE',  ( 45.44342259735076084, 1444.063149475110094, 268.9800971098556488 ) ) ;
#105165 = CARTESIAN_POINT ( 'NONE',  ( 1.657276590850500053, 1467.004937341380128, 220.0645755171550206 ) ) ;
#105166 = CARTESIAN_POINT ( 'NONE',  ( -10.86110766952070605, 1438.504893499145965, 152.3919029481315874 ) ) ;
#105167 = AXIS2_PLACEMENT_3D ( 'NONE', #42878, #102746, #26040 ) ;
#105168 = CARTESIAN_POINT ( 'NONE',  ( 9.949026363403810080, 1472.637006744650307, 191.3883391339116997 ) ) ;
#105169 = EDGE_CURVE ( 'NONE', #75901, #40683, #83990, .T. ) ;
#105170 = CARTESIAN_POINT ( 'NONE',  ( -21.27157138767482891, 1506.426094410640417, 214.6803200238785791 ) ) ;
#105171 = CARTESIAN_POINT ( 'NONE',  ( -17.87298439029999741, 1430.801053286930028, 226.5401518608979927 ) ) ;
#105172 = CARTESIAN_POINT ( 'NONE',  ( 15.86377822757070000, 1474.307034152129972, 268.3909166498499985 ) ) ;
#105173 = CARTESIAN_POINT ( 'NONE',  ( 11.37414570439999828, 1415.063410501429871, 222.6977618391979945 ) ) ;
#105174 = CARTESIAN_POINT ( 'NONE',  ( 3.860674342979999896, 1447.670908790060139, 184.2423422240979960 ) ) ;
#105175 = CARTESIAN_POINT ( 'NONE',  ( 4.026777485955000735, 1516.718889242609976, 206.8247602162870180 ) ) ;
#105176 = EDGE_CURVE ( 'NONE', #26525, #32787, #71308, .T. ) ;
#105177 = VERTEX_POINT ( 'NONE', #68047 ) ;
#105178 = CARTESIAN_POINT ( 'NONE',  ( 21.10423771450547292, 1411.010697888440063, 217.9724924710270102 ) ) ;
#105179 = CARTESIAN_POINT ( 'NONE',  ( 1.517721997056749927, 1457.716913820190030, 183.2697976461230098 ) ) ;
#105180 = ORIENTED_EDGE ( 'NONE', *, *, #20964, .T. ) ;
#105181 = FACE_OUTER_BOUND ( 'NONE', #96711, .T. ) ;
#105182 = CARTESIAN_POINT ( 'NONE',  ( 25.33603192065969978, 1451.791194868420007, 136.3363360771870134 ) ) ;
#105183 = DIRECTION ( 'NONE',  ( 0.9455185755993178454, 0.000000000000000000, -0.3255681544571538688 ) ) ;
#105184 = CARTESIAN_POINT ( 'NONE',  ( -20.57369194309999827, 1389.799942534980119, 216.9804166070690030 ) ) ;
#105185 = CARTESIAN_POINT ( 'NONE',  ( -12.25810126567743907, 1388.996058220885516, 215.8687261311177963 ) ) ;
#105186 = CARTESIAN_POINT ( 'NONE',  ( 17.80440947700000365, 1409.534804066629931, 196.0485523064980100 ) ) ;
#105187 = FACE_OUTER_BOUND ( 'NONE', #51768, .T. ) ;
#105188 = CARTESIAN_POINT ( 'NONE',  ( 2.991516284728592989, 1439.674840613275364, 184.0837186423407275 ) ) ;
#105189 = CARTESIAN_POINT ( 'NONE',  ( -22.82498224624805516, 1432.425316134065952, 215.5066816192843362 ) ) ;
#105190 = CIRCLE ( 'NONE', #37256, 1.000000000000000888 ) ;
#105191 = CARTESIAN_POINT ( 'NONE',  ( -4.518180742295140181E-06, 1509.047264790930058, 179.1218459713510072 ) ) ;
#105192 = CARTESIAN_POINT ( 'NONE',  ( 15.00046832902299876, 1429.237668425022093, 197.8089893366197884 ) ) ;
#105193 = VECTOR ( 'NONE', #53766, 1000.000000000000000 ) ;
#105194 = CARTESIAN_POINT ( 'NONE',  ( -5.775236830874999505, 1516.804776704140068, 214.1294346171470124 ) ) ;
#105195 = CARTESIAN_POINT ( 'NONE',  ( 26.05330421372899963, 1447.171924260989954, 137.7989882634119851 ) ) ;
#105196 = EDGE_LOOP ( 'NONE', ( #47747, #31743, #81733, #73628 ) ) ;
#105197 = CARTESIAN_POINT ( 'NONE',  ( -7.427207796130010031, 1509.244793066193324, 179.9842687496544613 ) ) ;
#105198 = CARTESIAN_POINT ( 'NONE',  ( 21.38516915557987375, 1522.382868172863937, 237.8497028174237755 ) ) ;
#105199 = VECTOR ( 'NONE', #64328, 1000.000000000000000 ) ;
#105200 = CARTESIAN_POINT ( 'NONE',  ( -6.025152189795589308, 1484.743689720570046, 198.8560543189699956 ) ) ;
#105201 = CIRCLE ( 'NONE', #103410, 2.000000000000068390 ) ;
#105202 = CARTESIAN_POINT ( 'NONE',  ( -4.026786250540000722, 1432.413060387330006, 146.1721969590979882 ) ) ;
#105203 = CARTESIAN_POINT ( 'NONE',  ( -39.36129609902809534, 1447.182057882140043, 136.6155912094569942 ) ) ;
#105204 = AXIS2_PLACEMENT_3D ( 'NONE', #64934, #91759, #41376 ) ;
#105205 = CARTESIAN_POINT ( 'NONE',  ( -4.328687482160670008, 1515.093865522939950, 207.9272901344760101 ) ) ;
#105206 = CARTESIAN_POINT ( 'NONE',  ( -20.63825566599999917, 1456.438754565230056, 248.0989693021979861 ) ) ;
#105207 = CARTESIAN_POINT ( 'NONE',  ( -28.96738428617770111, 1526.189899547014875, 197.4412607874185142 ) ) ;
#105208 = CARTESIAN_POINT ( 'NONE',  ( 11.79531744139999994, 1433.054727169869921, 150.6259952627979999 ) ) ;
#105209 = CARTESIAN_POINT ( 'NONE',  ( -2.486951778696359749, 1446.758387635790086, 222.8330888875190112 ) ) ;
#105210 = DIRECTION ( 'NONE',  ( 0.000000000000000000, 1.000000000000000000, 0.000000000000000000 ) ) ;
#105211 = CARTESIAN_POINT ( 'NONE',  ( -21.12410134230000125, 1508.013533195929995, 227.5424588953979992 ) ) ;
#105212 = LINE ( 'NONE', #11698, #76056 ) ;
#105213 = ORIENTED_EDGE ( 'NONE', *, *, #78055, .F. ) ;
#105214 = FACE_OUTER_BOUND ( 'NONE', #74856, .T. ) ;
#105215 = CARTESIAN_POINT ( 'NONE',  ( 10.01437067453739971, 1462.389803450230147, 210.8954083920299922 ) ) ;
#105216 = CARTESIAN_POINT ( 'NONE',  ( -13.69870936760000113, 1486.370890417729925, 185.2067811559980157 ) ) ;
#105217 = CARTESIAN_POINT ( 'NONE',  ( -1.063750041850000105, 1443.513882422190136, 200.1423802087390129 ) ) ;
#105218 = DIRECTION ( 'NONE',  ( 0.000000000000000000, 0.000000000000000000, -1.000000000000000000 ) ) ;
#105219 =( GEOMETRIC_REPRESENTATION_CONTEXT ( 3 ) GLOBAL_UNCERTAINTY_ASSIGNED_CONTEXT ( ( #16604 ) ) GLOBAL_UNIT_ASSIGNED_CONTEXT ( ( #86941, #35999, #87510 ) ) REPRESENTATION_CONTEXT ( 'NONE', 'WORKASPACE' ) );
#105220 = CARTESIAN_POINT ( 'NONE',  ( 21.91488070589999992, 1449.791133979859978, 220.2443267750980169 ) ) ;
#105221 = CARTESIAN_POINT ( 'NONE',  ( -16.00178234999744831, 1420.236353625467927, 209.6595671161338714 ) ) ;
#105222 = CARTESIAN_POINT ( 'NONE',  ( -12.86131642979999867, 1509.362187453730030, 235.2891919111980030 ) ) ;
#105223 = CARTESIAN_POINT ( 'NONE',  ( -27.09553561796830223, 1383.845623832669844, 225.0950745557760229 ) ) ;
#105224 = CARTESIAN_POINT ( 'NONE',  ( -3.961741473678640268, 1508.551704408789874, 204.5769763901439831 ) ) ;
#105225 = CARTESIAN_POINT ( 'NONE',  ( 2.499943159395269898, 1419.755139738720118, 123.2722782263270034 ) ) ;
#105226 = CARTESIAN_POINT ( 'NONE',  ( 2201.413669186790685, 11221.53578756870047, -1523.112345774690311 ) ) ;
#105227 = CARTESIAN_POINT ( 'NONE',  ( 0.1672222338998649860, 1481.964487760609927, 182.0100010911949937 ) ) ;
#105229 = VERTEX_POINT ( 'NONE', #102156 ) ;
#105228 = CARTESIAN_POINT ( 'NONE',  ( -4.836530696830000586, 1489.194118352389751, 188.8927898524989928 ) ) ;
#105230 = CARTESIAN_POINT ( 'NONE',  ( -1.546949756590000113, 1416.828042686930075, 228.0209011719979912 ) ) ;
#105231 = CARTESIAN_POINT ( 'NONE',  ( -3.078458350170000024, 1381.390032981420063, 201.0850095095790095 ) ) ;
#105232 = CARTESIAN_POINT ( 'NONE',  ( -3.034145623640000178, 1440.440283128710007, 157.2495509660979849 ) ) ;
#105234 = ORIENTED_EDGE ( 'NONE', *, *, #95918, .T. ) ;
#105233 = CARTESIAN_POINT ( 'NONE',  ( -32.85805783624299892, 1523.678648413191695, 217.1983043299907763 ) ) ;
#105235 = CARTESIAN_POINT ( 'NONE',  ( -7.107506042044070327, 1508.551704404740121, 219.1601581955270035 ) ) ;
#105236 = ORIENTED_EDGE ( 'NONE', *, *, #5748, .F. ) ;
#105237 = CARTESIAN_POINT ( 'NONE',  ( -9.537890462841289718, 1388.022264309169941, 217.5086179808309907 ) ) ;
#105238 = CARTESIAN_POINT ( 'NONE',  ( -16.36865316639999790, 1414.913060387329779, 209.3429107935929778 ) ) ;
#105239 = CARTESIAN_POINT ( 'NONE',  ( 28.77729953137099983, 1509.917985831029910, 206.0039978706130057 ) ) ;
#105240 = CARTESIAN_POINT ( 'NONE',  ( -0.2964941798090010017, 1431.756287522389812, 218.2392599841689957 ) ) ;
#105241 = CARTESIAN_POINT ( 'NONE',  ( -11.16643434163729864, 1471.372555858320084, 206.7508257846899937 ) ) ;
#105242 = CARTESIAN_POINT ( 'NONE',  ( 12.46263537197410010, 1409.348265197239925, 217.3636187787240033 ) ) ;
#105243 = DIRECTION ( 'NONE',  ( 0.000000000000000000, 1.000000000000000000, -2.081668171172166620E-14 ) ) ;
#105244 = CARTESIAN_POINT ( 'NONE',  ( -105.5431657123439919, 1385.234305881529963, 296.9663787050429846 ) ) ;
#105245 = CARTESIAN_POINT ( 'NONE',  ( -16.76281960579999719, 1413.995603259130121, 191.6500452088980069 ) ) ;
#105246 = CARTESIAN_POINT ( 'NONE',  ( -32.86802468386296994, 1523.481610426287716, 201.0396662540046577 ) ) ;
#105247 = CARTESIAN_POINT ( 'NONE',  ( 10.79340562696630101, 1490.084803914939812, 207.2635531919679863 ) ) ;
#105249 = ORIENTED_EDGE ( 'NONE', *, *, #50885, .F. ) ;
#105248 = CARTESIAN_POINT ( 'NONE',  ( -1.906563618092599921E-08, 1509.051704408389924, 214.1089243866270238 ) ) ;
#105250 = EDGE_LOOP ( 'NONE', ( #10843, #86633, #29422, #107642 ) ) ;
#105251 = CARTESIAN_POINT ( 'NONE',  ( -12.15368974921969958, 1416.134159100540046, 194.7772796687779930 ) ) ;
#105252 = CARTESIAN_POINT ( 'NONE',  ( 0.3222616711803319989, 1496.639296058219998, 196.7583996707039944 ) ) ;
#105253 = CARTESIAN_POINT ( 'NONE',  ( 13.60370406562014622, 1469.851559027462599, 269.3580926999919143 ) ) ;
#105254 = CARTESIAN_POINT ( 'NONE',  ( 11.60812525217539992, 1427.544186611749865, 209.2289499687080081 ) ) ;
#105255 = CARTESIAN_POINT ( 'NONE',  ( -0.006135579268280000158, 1395.974572298630164, 220.7500239771979693 ) ) ;
#105256 = CARTESIAN_POINT ( 'NONE',  ( 31.52384642521029789, 1525.730671215508664, 201.2079779568606455 ) ) ;
#105257 = CARTESIAN_POINT ( 'NONE',  ( -0.1457309951619999711, 1455.055482580329908, 183.1213254899980143 ) ) ;
#105258 = CARTESIAN_POINT ( 'NONE',  ( -9.832966357650001044, 1364.062280235949856, 207.6218459616989946 ) ) ;
#105259 = CARTESIAN_POINT ( 'NONE',  ( -26.63837744890847858, 1436.744137532187551, 136.7910871693582919 ) ) ;
#105260 = CARTESIAN_POINT ( 'NONE',  ( 4.027051405805000428, 1516.733363207009916, 206.6306575737070261 ) ) ;
#105261 = AXIS2_PLACEMENT_3D ( 'NONE', #32401, #65473, #99582 ) ;
#105262 = CARTESIAN_POINT ( 'NONE',  ( -13.17555111980130000, 1435.420252581789782, 150.3576300310929810 ) ) ;
#105263 = CARTESIAN_POINT ( 'NONE',  ( -1.931788062849999808E-14, 1421.852999791829916, 133.5962737641980027 ) ) ;
#105264 = CARTESIAN_POINT ( 'NONE',  ( -0.8045663272259990784, 1496.574851711289966, 197.1535040705990127 ) ) ;
#105266 = CARTESIAN_POINT ( 'NONE',  ( -16.93884325354670040, 1507.634939694479954, 230.1482608329069990 ) ) ;
#105265 = VECTOR ( 'NONE', #67121, 1000.000000000000114 ) ;
#105267 = CARTESIAN_POINT ( 'NONE',  ( -103.9362963259999901, 1380.106856784760112, 301.6745611782590117 ) ) ;
#105268 = ORIENTED_EDGE ( 'NONE', *, *, #23308, .F. ) ;
#105269 = ADVANCED_FACE ( 'NONE', ( #20360 ), #34709, .T. ) ;
#105270 = VECTOR ( 'NONE', #47363, 1000.000000000000114 ) ;
#105271 = CARTESIAN_POINT ( 'NONE',  ( 37.17588053200000076, 1423.049456354930044, 264.1764833033980153 ) ) ;
#105272 = CARTESIAN_POINT ( 'NONE',  ( -26.57328462060000263, 1469.248969696529912, 208.7426067427740008 ) ) ;
#105274 = CARTESIAN_POINT ( 'NONE',  ( 3.263569602579999775E-14, 1416.961989284729952, 254.9666375902979780 ) ) ;
#105273 = CARTESIAN_POINT ( 'NONE',  ( -11.00536801767579931, 1426.523244036580081, 91.15358938771061048 ) ) ;
#105275 = CARTESIAN_POINT ( 'NONE',  ( -20.39519499389999879, 1453.159462793029888, 208.3965248203290059 ) ) ;
#105276 = CARTESIAN_POINT ( 'NONE',  ( -5.301749024289999390, 1413.741945239130018, 248.5896189572980006 ) ) ;
#105277 = CARTESIAN_POINT ( 'NONE',  ( 19.73644163875970037, 1509.633137979659978, 231.2831758493399832 ) ) ;
#105278 = EDGE_CURVE ( 'NONE', #10275, #89357, #75065, .T. ) ;
#105279 = CARTESIAN_POINT ( 'NONE',  ( 3.813631208918726312, 1447.061710304021517, 154.8462439947786038 ) ) ;
#105280 = CARTESIAN_POINT ( 'NONE',  ( 31.78276358479999786, 1451.803508859929934, 135.2120624569979839 ) ) ;
#105281 = EDGE_LOOP ( 'NONE', ( #88964, #98134, #65104, #92951 ) ) ;
#105282 = CARTESIAN_POINT ( 'NONE',  ( -2.500000000000000000, 1430.723343392929792, 157.4401612927979954 ) ) ;
#105283 = CARTESIAN_POINT ( 'NONE',  ( 14.69200427761992600, 1514.485057820107158, 225.4415873000313297 ) ) ;
#105284 = CARTESIAN_POINT ( 'NONE',  ( 14.10737876370000166, 1509.405700909230063, 234.8174633738979935 ) ) ;
#105285 = ORIENTED_EDGE ( 'NONE', *, *, #51945, .F. ) ;
#105286 = ORIENTED_EDGE ( 'NONE', *, *, #97880, .T. ) ;
#105287 = CARTESIAN_POINT ( 'NONE',  ( -29.22965625836564385, 1509.933782476033912, 211.7723397217503987 ) ) ;
#105288 = CARTESIAN_POINT ( 'NONE',  ( -23.30841755010380112, 1409.842253946060055, 208.8031150648170353 ) ) ;
#105289 = VERTEX_POINT ( 'NONE', #55658 ) ;
#105290 = CARTESIAN_POINT ( 'NONE',  ( 0.5017934223950000217, 1413.835511642630081, 184.9211686299979931 ) ) ;
#105291 = AXIS2_PLACEMENT_3D ( 'NONE', #56692, #38224, #80793 ) ;
#105292 = CARTESIAN_POINT ( 'NONE',  ( -1.376928043298434767, 1522.051704408389924, 226.4861182474958525 ) ) ;
#105293 = CARTESIAN_POINT ( 'NONE',  ( -0.02955819112566620069, 1517.151704408390060, 225.0080808726450243 ) ) ;
#105294 = CARTESIAN_POINT ( 'NONE',  ( -5.701487894879999629, 1479.768604539729949, 234.8346338655979935 ) ) ;
#105295 = CARTESIAN_POINT ( 'NONE',  ( 7.012524228414029892, 1508.551704613440052, 203.1374999936529946 ) ) ;
#105296 = VERTEX_POINT ( 'NONE', #89781 ) ;
#105297 = CARTESIAN_POINT ( 'NONE',  ( 11.43732278620000109, 1425.481241381329937, 144.1613654183979918 ) ) ;
#105298 = B_SPLINE_CURVE_WITH_KNOTS ( 'NONE', 3,
 ( #28708, #20285, #69636, #62913, #37102, #27600, #71302, #61784, #95908, #105416, #63445, #20836, #103759, #27060, #10243, #97024, #44419, #79129, #19169, #36552, #91900, #65627, #100308, #39302 ),
 .UNSPECIFIED., .F., .F.,
 ( 4, 2, 1, 1, 2, 2, 2, 2, 2, 1, 1, 2, 2, 4 ),
 ( 0.000000000000000000, 0.1249999999998059053, 0.1874999999996863065, 0.2187499999996492805, 0.2343749999996534994, 0.2499999999996577182, 0.3749999999996929123, 0.4999999999997282174, 0.6249999999997635225, 0.6874999999997812861, 0.7187499999997918332, 0.7343749999997692957, 0.7499999999997467581, 1.000000000000000000 ),
 .UNSPECIFIED. ) ;
#105299 = CARTESIAN_POINT ( 'NONE',  ( 2.330134126090000368, 1515.064792882589927, 213.4512947377390049 ) ) ;
#105300 = CARTESIAN_POINT ( 'NONE',  ( 13.84474581289999939, 1452.823898879430089, 224.2523962804980044 ) ) ;
#105301 = ORIENTED_EDGE ( 'NONE', *, *, #90717, .F. ) ;
#105302 = CARTESIAN_POINT ( 'NONE',  ( -6.945490086935000029, 1516.932669162149978, 203.3434733684869968 ) ) ;
#105303 = VERTEX_POINT ( 'NONE', #64611 ) ;
#105304 = CARTESIAN_POINT ( 'NONE',  ( 11.86490175767010058, 1432.252230835709952, 149.9817356757799871 ) ) ;
#105305 = CARTESIAN_POINT ( 'NONE',  ( 13.41855466063566560, 1444.378506783447392, 187.7774200406155387 ) ) ;
#105306 = VERTEX_POINT ( 'NONE', #13049 ) ;
#105307 = ORIENTED_EDGE ( 'NONE', *, *, #96189, .F. ) ;
#105308 = CARTESIAN_POINT ( 'NONE',  ( -1.464145755870850163, 1482.281356462570102, 182.5701915244350175 ) ) ;
#105309 = CARTESIAN_POINT ( 'NONE',  ( -17.22592482065197927, 1443.913060387330233, 162.9227486220069920 ) ) ;
#105310 = CARTESIAN_POINT ( 'NONE',  ( 5.216739650425079589, 1497.653660005760230, 197.6765241825160047 ) ) ;
#105311 = CARTESIAN_POINT ( 'NONE',  ( -4.275310502956699565, 1469.420104164370059, 218.4212499309419968 ) ) ;
#105312 = CARTESIAN_POINT ( 'NONE',  ( -4.384282716360000443, 1424.957687000730175, 186.0191632644979904 ) ) ;
#105313 = CARTESIAN_POINT ( 'NONE',  ( 0.9653168468964550275, 1409.211512109100113, 270.3713481135980032 ) ) ;
#105314 = CARTESIAN_POINT ( 'NONE',  ( -103.8055019550000111, 1389.814814112089834, 301.7479020532589971 ) ) ;
#105315 = CARTESIAN_POINT ( 'NONE',  ( -12.78813129401979864, 1502.651454227029944, 209.2144374427170135 ) ) ;
#105316 = CARTESIAN_POINT ( 'NONE',  ( -2.369178030186009920, 1422.130784306599935, 193.0786739971210011 ) ) ;
#105317 = DIRECTION ( 'NONE',  ( -0.8775825618903726477, 1.203706215242023366E-32, -0.4794255386042032829 ) ) ;
#105318 = CARTESIAN_POINT ( 'NONE',  ( 0.02577720648996629366, 1410.273974002400792, 233.2210067926105239 ) ) ;
#105320 = FACE_OUTER_BOUND ( 'NONE', #74733, .T. ) ;
#105319 = CARTESIAN_POINT ( 'NONE',  ( -12.78085885379999986, 1502.746248514790068, 208.8788078008309981 ) ) ;
#105321 = CARTESIAN_POINT ( 'NONE',  ( -63.34523448917954624, 1379.747030511724688, 271.7626510979175123 ) ) ;
#105322 = CARTESIAN_POINT ( 'NONE',  ( 17.60627508980000044, 1410.895669370830092, 224.8086596393980017 ) ) ;
#105323 = CARTESIAN_POINT ( 'NONE',  ( -7.943523479595000047, 1514.557408760799945, 202.6827084971669990 ) ) ;
#105324 = ORIENTED_EDGE ( 'NONE', *, *, #17858, .F. ) ;
#105325 = CARTESIAN_POINT ( 'NONE',  ( 28.52406123459999776, 1430.067484666330074, 255.3819207742980097 ) ) ;
#105326 = CIRCLE ( 'NONE', #19466, 1.000000000000000888 ) ;
#105327 = CARTESIAN_POINT ( 'NONE',  ( 18.64442764522555862, 1507.939506224435718, 188.5219863285041129 ) ) ;
#105328 = CARTESIAN_POINT ( 'NONE',  ( -70.89913272470511174, 1385.021051334530057, 296.0640616977649984 ) ) ;
#105329 = B_SPLINE_SURFACE_WITH_KNOTS ( 'NONE', 5, 5, ( 
 ( #109685, #93974, #92873, #50354, #84479, #36284 ),
 ( #70476, #1055, #22073, #29946, #56268, #104596 ),
 ( #11105, #53674, #78862, #2169, #27890, #9981 ),
 ( #35180, #21528, #90397, #69925, #38892, #44710 ),
 ( #89862, #55742, #106656, #62073, #64692, #81439 ),
 ( #30503, #87818, #96199, #77745, #19474, #45266 ),
 ( #79405, #86687, #107215, #4750, #52553, #47315 ),
 ( #69365, #2716, #95643, #73075, #98811, #36839 ),
 ( #103474, #10536, #43594, #13131, #26780, #72526 ) ),
 .UNSPECIFIED., .F., .F., .F.,
 ( 6, 3, 6 ),
 ( 6, 6 ),
 ( 4.387253917325519836, 7.393604636469999214, 10.39995535562450080 ),
 ( -0.001720784224481730022, 1.000000000000000000 ),
 .UNSPECIFIED. ) ;
#105330 = CARTESIAN_POINT ( 'NONE',  ( -17.61183580542381577, 1523.982201850120191, 180.5695639321406532 ) ) ;
#105331 = CARTESIAN_POINT ( 'NONE',  ( 4.498501936019999370, 1505.761609765590038, 220.2758765865989972 ) ) ;
#105332 = CARTESIAN_POINT ( 'NONE',  ( -0.4151546846821903003, 1501.977400791986611, 244.9330574173806951 ) ) ;
#105333 =( BOUNDED_CURVE ( )  B_SPLINE_CURVE ( 3, ( #6268, #40966, #39874, #23049 ),
 .UNSPECIFIED., .F., .F. ) 
 B_SPLINE_CURVE_WITH_KNOTS ( ( 4, 4 ),
 ( 4.712388980384689674, 6.283185307179586232 ),
 .UNSPECIFIED. ) 
 CURVE ( )  GEOMETRIC_REPRESENTATION_ITEM ( )  RATIONAL_B_SPLINE_CURVE ( ( 1.000000000000000000, 0.8047378541243649375, 0.8047378541243649375, 1.000000000000000000 ) ) 
 REPRESENTATION_ITEM ( '' )  );
#105335 = ORIENTED_EDGE ( 'NONE', *, *, #28345, .T. ) ;
#105334 = CARTESIAN_POINT ( 'NONE',  ( -16.76766723949620186, 1420.018926319380171, 208.3735033652980064 ) ) ;
#105336 = CARTESIAN_POINT ( 'NONE',  ( -17.24222792867009701, 1417.941613371040148, 205.1746868673990036 ) ) ;
#105337 = CARTESIAN_POINT ( 'NONE',  ( -24.59914094579999855, 1443.155180290510089, 210.8302193746780233 ) ) ;
#105338 = TOROIDAL_SURFACE ( 'NONE', #40983, 11.23850026409999892, 0.5000000000000000000 ) ;
#105339 = VECTOR ( 'NONE', #109567, 1000.000000000000114 ) ;
#105340 = DIRECTION ( 'NONE',  ( -1.000000000000000000, 0.000000000000000000, 0.000000000000000000 ) ) ;
#105341 = CARTESIAN_POINT ( 'NONE',  ( -6.409211830000000276, 1460.447398049189815, 209.7327255955039789 ) ) ;
#105342 = CARTESIAN_POINT ( 'NONE',  ( 12.84824842633499919, 1512.167884426309911, 224.5031668304669950 ) ) ;
#105343 = DIRECTION ( 'NONE',  ( 0.9965178241646045487, -2.165862640214384426E-12, -0.08338001032766965970 ) ) ;
#105344 = CARTESIAN_POINT ( 'NONE',  ( 21.91388558050159929, 1509.808238952129841, 230.0100389666999945 ) ) ;
#105345 = FACE_OUTER_BOUND ( 'NONE', #95942, .T. ) ;
#105346 = CARTESIAN_POINT ( 'NONE',  ( -0.9776412681320001408, 1475.513060387329915, 230.7453403689980007 ) ) ;
#105347 = CARTESIAN_POINT ( 'NONE',  ( 14.82212541029999819, 1417.425064580829940, 227.9176054998980021 ) ) ;
#105348 = CARTESIAN_POINT ( 'NONE',  ( -5.594770757790000992, 1475.752789105589954, 217.8971188394789920 ) ) ;
#105349 = CARTESIAN_POINT ( 'NONE',  ( -16.05553604150000169, 1459.222164567730033, 229.6221585443979905 ) ) ;
#105350 = CARTESIAN_POINT ( 'NONE',  ( -7.726331963605000297, 1517.194972660189933, 206.8303316343270239 ) ) ;
#105351 = CARTESIAN_POINT ( 'NONE',  ( 39.21111056970000419, 1422.625647128129913, 266.3742241808980111 ) ) ;
#105352 = CARTESIAN_POINT ( 'NONE',  ( -17.56180752129999689, 1409.526332219330016, 223.5690793764979958 ) ) ;
#105353 = CARTESIAN_POINT ( 'NONE',  ( 18.78564773260000109, 1435.583069123479845, 146.2005943789979767 ) ) ;
#105354 = VECTOR ( 'NONE', #63747, 1000.000000000000114 ) ;
#105355 = CARTESIAN_POINT ( 'NONE',  ( 21.29824326579999649, 1488.584156283829998, 192.5314371079979878 ) ) ;
#105356 = CARTESIAN_POINT ( 'NONE',  ( -16.57644247905169976, 1409.993773362210050, 191.9232830829909915 ) ) ;
#105357 = CARTESIAN_POINT ( 'NONE',  ( -14.17818885755020020, 1379.591559934480074, 207.8207570064110143 ) ) ;
#105359 = ADVANCED_FACE ( 'NONE', ( #47238 ), #107180, .T. ) ;
#105358 = CARTESIAN_POINT ( 'NONE',  ( -16.45001201050000006, 1423.352090360930106, 227.1126878444979980 ) ) ;
#105360 = CARTESIAN_POINT ( 'NONE',  ( 15.69795926888880189, 1521.951704408389787, 222.7678737654429995 ) ) ;
#105361 = CARTESIAN_POINT ( 'NONE',  ( -33.91368157693270291, 1437.010587976510124, 136.5611906174850105 ) ) ;
#105362 = CARTESIAN_POINT ( 'NONE',  ( -17.12015336051603853, 1526.107876515966382, 182.3088662919814738 ) ) ;
#105363 = CARTESIAN_POINT ( 'NONE',  ( -15.41720089870000088, 1415.311335408779769, 208.7885211753810211 ) ) ;
#105364 = CARTESIAN_POINT ( 'NONE',  ( -13.13758325809999938, 1443.000245701009817, 187.0090600251980106 ) ) ;
#105365 = CARTESIAN_POINT ( 'NONE',  ( -7.544733521240000407, 1384.899971913130003, 219.0877090842990071 ) ) ;
#105366 = CARTESIAN_POINT ( 'NONE',  ( 4.563201210870380109, 1455.845590638939939, 218.7168878893969861 ) ) ;
#105367 = ADVANCED_FACE ( 'NONE', ( #31518 ), #110679, .F. ) ;
#105368 = CARTESIAN_POINT ( 'NONE',  ( -30.21730347749999979, 1435.712217778030208, 136.0584395910979651 ) ) ;
#105369 = CARTESIAN_POINT ( 'NONE',  ( -6.862505600778585624, 1456.752482962994009, 227.8870320116735684 ) ) ;
#105370 = VERTEX_POINT ( 'NONE', #15790 ) ;
#105371 = CARTESIAN_POINT ( 'NONE',  ( 5.768664107876966263, 1510.557600717794685, 216.6626378734150933 ) ) ;
#105372 = CARTESIAN_POINT ( 'NONE',  ( 27.31525032189999891, 1439.464609863130136, 137.0827112581980032 ) ) ;
#105373 = CARTESIAN_POINT ( 'NONE',  ( -9.134867208606445743, 1469.981975463268327, 191.1356054705261158 ) ) ;
#105374 = ORIENTED_EDGE ( 'NONE', *, *, #79593, .T. ) ;
#105375 = CARTESIAN_POINT ( 'NONE',  ( -5.302697812188962523, 1464.205369536075750, 199.9536599677759057 ) ) ;
#105376 = CARTESIAN_POINT ( 'NONE',  ( -33.98065672744881027, 1443.501467202838512, 154.9321739644268234 ) ) ;
#105377 = CARTESIAN_POINT ( 'NONE',  ( -46.16776967539999532, 1440.913036915769908, 266.9714970989979861 ) ) ;
#105379 = CIRCLE ( 'NONE', #101750, 3.999999999999997335 ) ;
#105378 = CARTESIAN_POINT ( 'NONE',  ( -11.67232828841030035, 1481.221314557019923, 211.0847665075339989 ) ) ;
#105380 = CARTESIAN_POINT ( 'NONE',  ( 0.2567085482048540035, 1419.518028698059879, 184.4201755903200137 ) ) ;
#105381 = CARTESIAN_POINT ( 'NONE',  ( 19.00259723423673464, 1526.382868173645875, 232.9129335399838112 ) ) ;
#105382 = CARTESIAN_POINT ( 'NONE',  ( -97.12056875041480453, 1384.606167604229995, 310.4282471984710128 ) ) ;
#105383 = CARTESIAN_POINT ( 'NONE',  ( -47.06618458142209249, 1385.009314242649907, 220.9877181434370073 ) ) ;
#105384 = CARTESIAN_POINT ( 'NONE',  ( -5.014111827051360493, 1375.346567646530048, 214.7183233550310320 ) ) ;
#105385 = CARTESIAN_POINT ( 'NONE',  ( 12.95840179510000034, 1416.218047894730262, 221.5780309934980039 ) ) ;
#105386 = CARTESIAN_POINT ( 'NONE',  ( 14.22134611999999976, 1463.286284084930003, 223.7238266604979628 ) ) ;
#105387 = CARTESIAN_POINT ( 'NONE',  ( -6.910348952263761113, 1496.006749978269909, 200.2510802398396379 ) ) ;
#105388 = DIRECTION ( 'NONE',  ( -1.755985294532469921E-16, 1.000000000000000000, -1.338183447452831989E-16 ) ) ;
#105389 = CARTESIAN_POINT ( 'NONE',  ( -3.540698356210000064, 1508.270058940830040, 180.7688477407980088 ) ) ;
#105390 = CARTESIAN_POINT ( 'NONE',  ( -8.486023334060128320, 1517.151704408390060, 211.0297173932031569 ) ) ;
#105391 = CARTESIAN_POINT ( 'NONE',  ( -12.26815783919999880, 1415.553739807329976, 195.3528422598979830 ) ) ;
#105392 = CARTESIAN_POINT ( 'NONE',  ( 1.773850233349999916, 1423.360122320810206, 192.5455093738989945 ) ) ;
#105393 = CARTESIAN_POINT ( 'NONE',  ( 24.08425203100000189, 1411.115211432230126, 209.6325621231380012 ) ) ;
#105394 = CARTESIAN_POINT ( 'NONE',  ( -106.6593330254749930, 1391.913060387289988, 305.7868564143699928 ) ) ;
#105395 = B_SPLINE_CURVE_WITH_KNOTS ( 'NONE', 5,
 ( #1662, #95704, #79465, #11166, #80007, #53741 ),
 .UNSPECIFIED., .F., .F.,
 ( 6, 6 ),
 ( 0.000000000000000000, 1.000000000000000000 ),
 .UNSPECIFIED. ) ;
#105396 = CARTESIAN_POINT ( 'NONE',  ( 10.53029073209870070, 1452.309494521090073, 190.1435485275030146 ) ) ;
#105397 = CARTESIAN_POINT ( 'NONE',  ( -5.386185223340929973, 1432.347042777500064, 154.6076275972019971 ) ) ;
#105399 = CARTESIAN_POINT ( 'NONE',  ( -12.96458870010000020, 1380.564911143250129, 203.9320203105589826 ) ) ;
#105398 = FACE_OUTER_BOUND ( 'NONE', #27076, .T. ) ;
#105400 = CARTESIAN_POINT ( 'NONE',  ( 0.7091528421289999828, 1410.300367797830177, 233.1399324052979978 ) ) ;
#105401 = CARTESIAN_POINT ( 'NONE',  ( -103.0210058550480738, 1376.302340817390359, 309.8919164400330146 ) ) ;
#105402 = CARTESIAN_POINT ( 'NONE',  ( -1970.025574498409924, -8382.262153571269664, 5.165967170900809258 ) ) ;
#105403 = CARTESIAN_POINT ( 'NONE',  ( -26.80147237664635185, 1509.848988426266942, 197.2601629728074499 ) ) ;
#105404 = CARTESIAN_POINT ( 'NONE',  ( -8.232155009530000456, 1367.485244382299925, 210.6218459616991936 ) ) ;
#105405 = CARTESIAN_POINT ( 'NONE',  ( -0.7564342523539989704, 1516.783665406140017, 204.5091745923169810 ) ) ;
#105406 = CARTESIAN_POINT ( 'NONE',  ( -18.37606861500000122, 1424.967732719430160, 227.5064700491979863 ) ) ;
#105407 = CARTESIAN_POINT ( 'NONE',  ( -18.97278584537820123, 1486.247047112609835, 189.3002463451680057 ) ) ;
#105408 = CARTESIAN_POINT ( 'NONE',  ( -9.253356380629998768, 1423.298286757820051, 209.1001181959080100 ) ) ;
#105409 = CIRCLE ( 'NONE', #80390, 2.000000000000003553 ) ;
#105410 = CARTESIAN_POINT ( 'NONE',  ( -10.77418843618166377, 1422.305283220386627, 210.6378112949979311 ) ) ;
#105412 = EDGE_LOOP ( 'NONE', ( #65506, #68006, #62001, #42789 ) ) ;
#105411 = CARTESIAN_POINT ( 'NONE',  ( -68.05606538682749829, 1379.746262163739857, 279.5397730745099807 ) ) ;
#105413 = VERTEX_POINT ( 'NONE', #57316 ) ;
#105414 = CARTESIAN_POINT ( 'NONE',  ( 27.13583296430000047, 1509.164684264529797, 215.3181691316380011 ) ) ;
#105415 = EDGE_LOOP ( 'NONE', ( #65908, #18427, #64293, #46893 ) ) ;
#105416 = CARTESIAN_POINT ( 'NONE',  ( -0.2829287784654356819, 1457.550022606329549, 199.5929807864239081 ) ) ;
#105417 = CARTESIAN_POINT ( 'NONE',  ( 1.547463840030000037, 1414.913060387329779, 192.3096136973980208 ) ) ;
#105419 = CARTESIAN_POINT ( 'NONE',  ( 23.35526608410000193, 1448.827836771670036, 218.6598503475479731 ) ) ;
#105418 = CARTESIAN_POINT ( 'NONE',  ( 15.91223255370150014, 1418.658837366640000, 191.2758984395539983 ) ) ;
#105420 = CARTESIAN_POINT ( 'NONE',  ( 4.026786250540000722, 1421.741487512030062, 169.4417495807979890 ) ) ;
#105421 = VECTOR ( 'NONE', #25344, 1000.000000000000114 ) ;
#105422 = CARTESIAN_POINT ( 'NONE',  ( -25.57416082987599992, 1451.572412185829990, 136.5135885075040107 ) ) ;
#105423 = CARTESIAN_POINT ( 'NONE',  ( 8.622487674225027376, 1440.776277238063585, 153.7651958641682768 ) ) ;
#105424 = CARTESIAN_POINT ( 'NONE',  ( 13.71870890039999935, 1409.558843311929877, 227.5656532589979975 ) ) ;
#105425 = EDGE_CURVE ( 'NONE', #54104, #86029, #80578, .T. ) ;
#105426 = PRODUCT ( 'MAS-682', 'MAS-682', '', ( #21381 ) ) ;
#105427 = CARTESIAN_POINT ( 'NONE',  ( 4.623787969365000805, 1516.947419719950176, 212.5709951659769956 ) ) ;
#105428 = CARTESIAN_POINT ( 'NONE',  ( 41.63323805095519958, 1443.027121608840162, 134.0999999981200119 ) ) ;
#105429 = CARTESIAN_POINT ( 'NONE',  ( -5.778791999094319287, 1426.204447263729890, 207.0106680037629872 ) ) ;
#105430 = CARTESIAN_POINT ( 'NONE',  ( 14.35058941227343254, 1522.051704408389924, 224.2459111387558437 ) ) ;
#105431 = ORIENTED_EDGE ( 'NONE', *, *, #16760, .F. ) ;
#105432 = CARTESIAN_POINT ( 'NONE',  ( -9.299436816969999242, 1446.922293007090275, 190.6945112479990030 ) ) ;
#105433 = AXIS2_PLACEMENT_3D ( 'NONE', #102780, #83370, #26074 ) ;
#105434 = CARTESIAN_POINT ( 'NONE',  ( -1.318899170704230128, 1431.696355161669999, 200.8232092877559865 ) ) ;
#105435 = ORIENTED_EDGE ( 'NONE', *, *, #80868, .T. ) ;
#105436 = ORIENTED_EDGE ( 'NONE', *, *, #10291, .T. ) ;
#105437 = ORIENTED_EDGE ( 'NONE', *, *, #66749, .T. ) ;
#105438 = CARTESIAN_POINT ( 'NONE',  ( -7.211759849075000339, 1511.702066573629963, 215.8939835620469978 ) ) ;
#105439 = CARTESIAN_POINT ( 'NONE',  ( 16.25466701628457500, 1514.562529182973549, 194.3320297101351741 ) ) ;
#105440 = CARTESIAN_POINT ( 'NONE',  ( 15.81648005058062090, 1451.124245892486215, 149.1749219823134638 ) ) ;
#105441 = CARTESIAN_POINT ( 'NONE',  ( -3.089264994810000164, 1485.815196309429894, 182.5613893784980064 ) ) ;
#105442 = CARTESIAN_POINT ( 'NONE',  ( 3.156336099161360043, 1466.261550192479945, 198.5320301967060175 ) ) ;
#105443 = CIRCLE ( 'NONE', #12474, 2.000000000000001776 ) ;
#105444 = CARTESIAN_POINT ( 'NONE',  ( -17.39703151571873008, 1448.459128900735550, 218.4035087908428352 ) ) ;
#105445 = CARTESIAN_POINT ( 'NONE',  ( -63.17697519130717154, 1379.734402953275776, 268.4289174494917916 ) ) ;
#105446 = CARTESIAN_POINT ( 'NONE',  ( 3.153087606539999754, 1465.853416239390071, 199.3411100570189944 ) ) ;
#105447 = CARTESIAN_POINT ( 'NONE',  ( -3.424720339024999838, 1517.051704408389924, 217.6596685689069943 ) ) ;
#105448 = EDGE_LOOP ( 'NONE', ( #52270, #42017, #12883, #83822 ) ) ;
#105449 = CARTESIAN_POINT ( 'NONE',  ( 3.251611325815000342, 1516.779243033999819, 206.8234764622770001 ) ) ;
#105450 = VERTEX_POINT ( 'NONE', #23671 ) ;
#105451 = CARTESIAN_POINT ( 'NONE',  ( 32.16729354855799983, 1440.913060387330006, 256.2481582175259973 ) ) ;
#105452 = CARTESIAN_POINT ( 'NONE',  ( -15.33686075110000147, 1509.107788877129906, 184.5497581577979815 ) ) ;
#105453 = ORIENTED_EDGE ( 'NONE', *, *, #63708, .T. ) ;
#105454 = CARTESIAN_POINT ( 'NONE',  ( 26.69188107298460011, 1449.953547536330007, 136.5849450126470117 ) ) ;
#105455 = CARTESIAN_POINT ( 'NONE',  ( -14.33393486070000122, 1409.413612422530150, 192.0174323315980018 ) ) ;
#105456 = CARTESIAN_POINT ( 'NONE',  ( -57.46991821550079749, 1379.718150813474040, 260.7768847105036230 ) ) ;
#105458 = CARTESIAN_POINT ( 'NONE',  ( 19.52205342210000083, 1473.076230373790168, 204.3554439105789982 ) ) ;
#105457 = CARTESIAN_POINT ( 'NONE',  ( 21.14415186440000127, 1497.093961449289964, 210.1561521351690089 ) ) ;
#105459 = CARTESIAN_POINT ( 'NONE',  ( -7.993033103293710084, 1436.236666033240226, 214.7384163211640100 ) ) ;
#105460 = CARTESIAN_POINT ( 'NONE',  ( 13.90496272978541725, 1414.913060387330006, 217.4955100473378025 ) ) ;
#105461 = DIRECTION ( 'NONE',  ( 0.4999999999998399614, -0.7071067811867740582, 0.4999999999998399614 ) ) ;
#105462 = CARTESIAN_POINT ( 'NONE',  ( -12.06107998010000060, 1433.903545125019946, 148.5637427420979861 ) ) ;
#105464 = ADVANCED_FACE ( 'NONE', ( #99262 ), #55930, .F. ) ;
#105463 = CARTESIAN_POINT ( 'NONE',  ( -6.814218036220000663, 1508.185726375689910, 220.1716981485990061 ) ) ;
#105466 = CARTESIAN_POINT ( 'NONE',  ( 5.423836325560000837, 1437.243905350390150, 208.3828194269840139 ) ) ;
#105465 = CARTESIAN_POINT ( 'NONE',  ( 10.27415084429999936, 1462.789161984029761, 234.7156815036980220 ) ) ;
#105467 = CONICAL_SURFACE ( 'NONE', #55422, 23.60273273060006360, 1.047194910839999826 ) ;
#105468 = B_SPLINE_SURFACE_WITH_KNOTS ( 'NONE', 5, 5, ( 
 ( #86826, #26926, #35883, #44289, #86271, #70067, #1188, #104179, #53247 ),
 ( #9557, #76774, #27463, #43727, #25795, #94112, #43184, #110370, #85163 ),
 ( #61115, #33649, #42622, #90, #95230, #34767, #18494, #10117, #52690 ),
 ( #102505, #87388, #34215, #69506, #67843, #77880, #78433, #76226, #68401 ),
 ( #59994, #17383, #61651, #638, #101954, #103056, #10683, #52139, #95778 ),
 ( #19045, #59444, #17943, #25241, #26354, #93555, #35319, #8449, #51582 ),
 ( #16827, #94672, #51028, #85714, #77336, #9010, #60550, #103628, #63852 ),
 ( #81169, #80634, #3948, #44851, #89019, #96888, #104729, #20698, #97964 ),
 ( #54894, #64400, #4484, #45939, #55991, #90114, #21234, #3396, #29667 ) ),
 .UNSPECIFIED., .F., .F., .F.,
 ( 6, 3, 6 ),
 ( 6, 3, 6 ),
 ( -1.001153178291219951E-05, 19.90003809979999971, 45.10384108370000433 ),
 ( 0.000000000000000000, 1.000000000000000000, 2.000010011531780041 ),
 .UNSPECIFIED. ) ;
#105469 = CARTESIAN_POINT ( 'NONE',  ( -0.7386049428049979992, 1517.122674412569950, 215.6839400395269877 ) ) ;
#105470 = CARTESIAN_POINT ( 'NONE',  ( -1.975340820460000257, 1463.175830154689947, 228.7200063650990103 ) ) ;
#105471 = CARTESIAN_POINT ( 'NONE',  ( 5.704331096967670156, 1511.494703458840149, 217.3688750472999800 ) ) ;
#105472 = CARTESIAN_POINT ( 'NONE',  ( 28.44347333380000364, 1509.158830953930192, 208.5401038306789872 ) ) ;
#105473 = CARTESIAN_POINT ( 'NONE',  ( 2.879956924955000108, 1516.827328999679821, 212.3743765858270081 ) ) ;
#105474 = CARTESIAN_POINT ( 'NONE',  ( -18.85453636469999950, 1434.822352678670086, 209.3473311023250005 ) ) ;
#105475 = DIRECTION ( 'NONE',  ( 0.9455185755993177343, 0.000000000000000000, -0.3255681544571540909 ) ) ;
#105477 = ORIENTED_EDGE ( 'NONE', *, *, #28178, .T. ) ;
#105476 = CARTESIAN_POINT ( 'NONE',  ( -113.4000000000000057, 1390.498795466600086, 304.4869478500590390 ) ) ;
#105478 = CARTESIAN_POINT ( 'NONE',  ( 0.000000000000000000, 1452.913060387330006, 179.9625354391980068 ) ) ;
#105479 = AXIS2_PLACEMENT_3D ( 'NONE', #92289, #49210, #6634 ) ;
#105480 = CARTESIAN_POINT ( 'NONE',  ( 31.69751081770000312, 1445.012237274630024, 244.1892870184980211 ) ) ;
#105481 = CARTESIAN_POINT ( 'NONE',  ( -2.298816259811510054, 1486.462377102800019, 220.8289805423670202 ) ) ;
#105482 = FACE_OUTER_BOUND ( 'NONE', #10897, .T. ) ;
#105483 = CARTESIAN_POINT ( 'NONE',  ( 2.344512035239230130, 1516.526058368810027, 216.8306617777329848 ) ) ;
#105484 = CARTESIAN_POINT ( 'NONE',  ( -19.44003422200000131, 1456.042540789730083, 227.5400276923980130 ) ) ;
#105486 = CARTESIAN_POINT ( 'NONE',  ( 5.359829535970479952, 1422.291879003420036, 145.7409380638519849 ) ) ;
#105485 = CARTESIAN_POINT ( 'NONE',  ( -18.74957845327451622, 1410.930162482557989, 196.2665709180884051 ) ) ;
#105487 = CARTESIAN_POINT ( 'NONE',  ( -8.790791811524689692, 1448.890444021340045, 211.6766362075580048 ) ) ;
#105488 = CARTESIAN_POINT ( 'NONE',  ( -104.7456079307379895, 1380.506914483850096, 307.5456015192170298 ) ) ;
#105489 = VERTEX_POINT ( 'NONE', #39380 ) ;
#105490 = CARTESIAN_POINT ( 'NONE',  ( -1.133517003235000153, 1516.713079096360161, 204.5117660986770147 ) ) ;
#105491 = CARTESIAN_POINT ( 'NONE',  ( 0.7780366837319999673, 1405.780753921430005, 268.4835186043979434 ) ) ;
#105492 = CARTESIAN_POINT ( 'NONE',  ( 1.094850995720000109, 1515.349842019790003, 213.4046786226089978 ) ) ;
#105493 = EDGE_CURVE ( 'NONE', #92278, #55998, #87318, .T. ) ;
#105494 = CARTESIAN_POINT ( 'NONE',  ( 42.06232253459919690, 1445.825096420900081, 269.6487541258160263 ) ) ;
#105495 = ADVANCED_FACE ( 'NONE', ( #9082 ), #39230, .T. ) ;
#105496 = CARTESIAN_POINT ( 'NONE',  ( 2.478947879950000210, 1432.276406471479959, 157.5139433850980026 ) ) ;
#105497 = CARTESIAN_POINT ( 'NONE',  ( 10.75950721900864693, 1424.480083424939039, 137.8581109189600227 ) ) ;
#105498 = EDGE_CURVE ( 'NONE', #52986, #36271, #65921, .T. ) ;
#105499 = CARTESIAN_POINT ( 'NONE',  ( -43.93650039737229918, 1440.913060405460101, 264.2825071479210237 ) ) ;
#105500 = DIRECTION ( 'NONE',  ( 5.980589973904019347E-17, -1.000000000000000000, 1.736889445713099699E-16 ) ) ;
#105501 = CARTESIAN_POINT ( 'NONE',  ( 1.746243614909547714, 1450.465158970312586, 154.2919968866931981 ) ) ;
#105502 = CARTESIAN_POINT ( 'NONE',  ( 0.5599827605490009796, 1431.620283137290016, 200.5991563158890187 ) ) ;
#105503 = EDGE_CURVE ( 'NONE', #37961, #31839, #16893, .T. ) ;
#105504 = CARTESIAN_POINT ( 'NONE',  ( -31.23437356469455040, 1512.187213306747481, 196.3468678195118287 ) ) ;
#105505 = EDGE_CURVE ( 'NONE', #44004, #54639, #7201, .T. ) ;
#105506 = CARTESIAN_POINT ( 'NONE',  ( 3.628818058489999832, 1505.602008442089982, 221.3635114687990040 ) ) ;
#105507 = CARTESIAN_POINT ( 'NONE',  ( -4.038582018749999669, 1515.598601288590089, 209.4984326820579952 ) ) ;
#105508 = ORIENTED_EDGE ( 'NONE', *, *, #62202, .F. ) ;
#105509 = AXIS2_PLACEMENT_3D ( 'NONE', #62047, #105697, #1575 ) ;
#105510 = CARTESIAN_POINT ( 'NONE',  ( 5.995204332980000249E-15, 1419.211677883429957, 248.0989693021979861 ) ) ;
#105511 = EDGE_CURVE ( 'NONE', #36569, #96612, #27538, .T. ) ;
#105512 = CARTESIAN_POINT ( 'NONE',  ( 9.473794194718619721, 1468.306494430019939, 205.7209031666899648 ) ) ;
#105513 = CARTESIAN_POINT ( 'NONE',  ( -0.1062961612130000066, 1475.048391926030035, 269.6500679733979950 ) ) ;
#105514 = CARTESIAN_POINT ( 'NONE',  ( -27.77560365120000085, 1451.943158935029942, 134.8960326030979786 ) ) ;
#105515 = CARTESIAN_POINT ( 'NONE',  ( -31.03088476499778281, 1523.982201850120191, 196.3745419238244381 ) ) ;
#105516 = LINE ( 'NONE', #71400, #32391 ) ;
#105517 = CARTESIAN_POINT ( 'NONE',  ( -37.64110078237469992, 1384.797974306949982, 238.1784615367210165 ) ) ;
#105518 = AXIS2_PLACEMENT_3D ( 'NONE', #91626, #49094, #83229 ) ;
#105519 = CARTESIAN_POINT ( 'NONE',  ( -18.89905511659999959, 1416.828040475729949, 207.5748962040180174 ) ) ;
#105520 = DIRECTION ( 'NONE',  ( 1.000000000000000000, 0.000000000000000000, 0.000000000000000000 ) ) ;
#105521 = CARTESIAN_POINT ( 'NONE',  ( 26.23576681230780139, 1435.413602865789926, 135.4068554872490040 ) ) ;
#105522 = CARTESIAN_POINT ( 'NONE',  ( -9.802578310169730358, 1396.255373964939963, 214.2508701772540007 ) ) ;
#105523 = EDGE_CURVE ( 'NONE', #24414, #4089, #43249, .T. ) ;
#105524 = B_SPLINE_CURVE_WITH_KNOTS ( 'NONE', 3,
 ( #48578, #82713, #50232, #91659, #40154, #108465, #14934, #74337, #31747, #65934, #67584, #50764, #390, #35059, #103349, #16568, #60850, #101690, #103921, #93306, #75964, #84899 ),
 .UNSPECIFIED., .F., .F.,
 ( 4, 3, 3, 3, 3, 3, 3, 4 ),
 ( -7.359819275554579932, -7.141305509537970053, -6.026261691904320372, -5.186741713040009749, -5.022423404310830009, -4.324046055999499316, -3.608772125771039896, -3.013663444789999701 ),
 .UNSPECIFIED. ) ;
#105525 = CARTESIAN_POINT ( 'NONE',  ( -15.49426842564200157, 1421.633204956707914, 227.2929607267749930 ) ) ;
#105526 = CARTESIAN_POINT ( 'NONE',  ( -16.49508940950000024, 1409.737691204929888, 225.9011186669980304 ) ) ;
#105527 = CARTESIAN_POINT ( 'NONE',  ( 19.41800382249774515, 1455.667198361140663, 225.5846027043448032 ) ) ;
#105528 = ORIENTED_EDGE ( 'NONE', *, *, #41168, .T. ) ;
#105529 = CARTESIAN_POINT ( 'NONE',  ( -11.36125419377996515, 1501.596596453163556, 207.6628600452400804 ) ) ;
#105531 = EDGE_CURVE ( 'NONE', #104116, #19921, #46465, .T. ) ;
#105530 = CARTESIAN_POINT ( 'NONE',  ( -15.59606447164447651, 1415.961119725337312, 208.0309741868692299 ) ) ;
#105532 = CARTESIAN_POINT ( 'NONE',  ( -18.43641199600227765, 1485.257797375915743, 189.1831268613264854 ) ) ;
#105534 = CARTESIAN_POINT ( 'NONE',  ( -12.13495040386500001, 1511.961073825299991, 193.0130861717670143 ) ) ;
#105533 = CARTESIAN_POINT ( 'NONE',  ( 10.91367058839999871, 1425.302818804329945, 128.4898600348980153 ) ) ;
#105535 = CARTESIAN_POINT ( 'NONE',  ( 5.157704406284129827E-09, 1406.911841301380036, 222.1218459627310153 ) ) ;
#105536 = EDGE_CURVE ( 'NONE', #65282, #64454, #17666, .T. ) ;
#105537 = CARTESIAN_POINT ( 'NONE',  ( -9.064953078289999411, 1451.258683735890145, 206.8358752714689786 ) ) ;
#105538 = CIRCLE ( 'NONE', #16137, 3.999999999999997335 ) ;
#105539 = CARTESIAN_POINT ( 'NONE',  ( 7.329930013194999816, 1516.881930554049859, 201.4037113026670056 ) ) ;
#105540 = CARTESIAN_POINT ( 'NONE',  ( 7.699283328289999950, 1425.052167582540051, 211.8716563696589787 ) ) ;
#105541 = CARTESIAN_POINT ( 'NONE',  ( -9.634835741540001663, 1430.981823154709900, 148.7079730222979776 ) ) ;
#105542 = CARTESIAN_POINT ( 'NONE',  ( 5.469793405669999942, 1507.795163446829747, 181.9824978760979945 ) ) ;
#105543 = CARTESIAN_POINT ( 'NONE',  ( 7.893411082094998754, 1512.020737142380085, 206.1250608998970222 ) ) ;
#105544 = CARTESIAN_POINT ( 'NONE',  ( -55.53609276739749845, 1378.543823089900116, 260.2783981610180035 ) ) ;
#105545 = ADVANCED_FACE ( 'NONE', ( #35950 ), #35627, .F. ) ;
#105546 = CARTESIAN_POINT ( 'NONE',  ( 7.445922712514740915, 1367.935115748543922, 210.6218459616987957 ) ) ;
#105548 = VERTEX_POINT ( 'NONE', #25588 ) ;
#105547 = CARTESIAN_POINT ( 'NONE',  ( 7.213645968120000695, 1453.321438162990034, 215.1620360656989988 ) ) ;
#105549 = B_SPLINE_CURVE_WITH_KNOTS ( 'NONE', 3,
 ( #31374, #39223, #46005, #80693 ),
 .UNSPECIFIED., .F., .F.,
 ( 4, 4 ),
 ( -14.36013183198100052, -6.524295923422950061 ),
 .UNSPECIFIED. ) ;
#105550 = ORIENTED_EDGE ( 'NONE', *, *, #28297, .T. ) ;
#105551 = CARTESIAN_POINT ( 'NONE',  ( -7.536504302460000027, 1396.176240917429823, 200.3138106880579983 ) ) ;
#105552 = CARTESIAN_POINT ( 'NONE',  ( 1.189285361496680071, 1507.141006053059982, 237.0337565598269975 ) ) ;
#105553 = DIRECTION ( 'NONE',  ( 0.000000000000000000, 0.3666799630584695047, 0.9303471420343265574 ) ) ;
#105554 = CARTESIAN_POINT ( 'NONE',  ( -7.685457311955000925, 1511.037966505499980, 214.2610714211569984 ) ) ;
#105556 = CARTESIAN_POINT ( 'NONE',  ( 17.77263048209999852, 1416.284038623030028, 224.9649977725980250 ) ) ;
#105555 = CARTESIAN_POINT ( 'NONE',  ( -8.032185305569999656, 1384.475430595510034, 218.7662459373489980 ) ) ;
#105557 = CIRCLE ( 'NONE', #1822, 1.999999999999998668 ) ;
#105558 = CARTESIAN_POINT ( 'NONE',  ( 1.838213786079999856, 1410.306157565029935, 185.3985639462979975 ) ) ;
#105559 = DIRECTION ( 'NONE',  ( -0.9455185755993177343, 0.000000000000000000, 0.3255681544571540909 ) ) ;
#105560 = CARTESIAN_POINT ( 'NONE',  ( -2.130922739038390024, 1467.954349360780043, 220.0452206896550251 ) ) ;
#105561 =( NAMED_UNIT ( * ) PLANE_ANGLE_UNIT ( ) SI_UNIT ( $, .RADIAN. ) );
#105562 = CARTESIAN_POINT ( 'NONE',  ( -2.500000000000000000, 1448.365115610690054, 162.8856519709460144 ) ) ;
#105563 = DIRECTION ( 'NONE',  ( 0.000000000000000000, -0.7071067811865474617, -0.7071067811865474617 ) ) ;
#105564 = CARTESIAN_POINT ( 'NONE',  ( -27.13955216900179934, 1438.563659682299885, 136.9826056857960168 ) ) ;
#105565 = CARTESIAN_POINT ( 'NONE',  ( -1.532227443785459942, 1405.761751320050053, 267.5364479672910534 ) ) ;
#105566 = CARTESIAN_POINT ( 'NONE',  ( -27.69925886641940238, 1441.434395751479997, 137.3015763626259798 ) ) ;
#105567 = ORIENTED_EDGE ( 'NONE', *, *, #57744, .T. ) ;
#105568 = DIRECTION ( 'NONE',  ( 0.8775825618903746461, -8.693568535565067726E-32, 0.4794255386041995082 ) ) ;
#105569 = CARTESIAN_POINT ( 'NONE',  ( 12.84752083859999949, 1442.662704864849957, 187.9133791926979882 ) ) ;
#105570 = ORIENTED_EDGE ( 'NONE', *, *, #88720, .T. ) ;
#105571 = ORIENTED_EDGE ( 'NONE', *, *, #14854, .T. ) ;
#105572 = DIRECTION ( 'NONE',  ( -0.2054769195713296304, 0.000000000000000000, 0.9786619618251631847 ) ) ;
#105573 = CARTESIAN_POINT ( 'NONE',  ( -9.328535443860001664, 1363.278783432130012, 207.6218459616989946 ) ) ;
#105574 = CARTESIAN_POINT ( 'NONE',  ( -3.257220640824999958, 1517.040132827679827, 214.9086836491569841 ) ) ;
#105575 = CARTESIAN_POINT ( 'NONE',  ( 2.564633783425000146, 1511.308638870219966, 216.6940388207569868 ) ) ;
#105576 = EDGE_CURVE ( 'NONE', #33799, #76035, #60779, .T. ) ;
#105577 = ORIENTED_EDGE ( 'NONE', *, *, #65200, .F. ) ;
#105578 = CARTESIAN_POINT ( 'NONE',  ( -8.928474135859682193, 1509.321320493349958, 180.3286574278590138 ) ) ;
#105579 = CARTESIAN_POINT ( 'NONE',  ( -88.45813511300001153, 1375.507175221300258, 298.0129420291590350 ) ) ;
#105580 = EDGE_CURVE ( 'NONE', #54152, #35149, #93833, .T. ) ;
#105581 = B_SPLINE_CURVE_WITH_KNOTS ( 'NONE', 3,
 ( #48796, #5108, #20796, #98064 ),
 .UNSPECIFIED., .F., .F.,
 ( 4, 4 ),
 ( 0.000000000000000000, 0.0002960034161023848394 ),
 .UNSPECIFIED. ) ;
#105582 = CARTESIAN_POINT ( 'NONE',  ( -105.8445521485040075, 1378.913060387460064, 303.5212775329050032 ) ) ;
#105583 = CARTESIAN_POINT ( 'NONE',  ( -2.877744984375000037, 1516.723920667490120, 204.5127816287269980 ) ) ;
#105584 = AXIS2_PLACEMENT_3D ( 'NONE', #99446, #12151, #47963 ) ;
#105585 = CARTESIAN_POINT ( 'NONE',  ( -35.61911272319999711, 1440.913060387330006, 261.9797944256979463 ) ) ;
#105586 = B_SPLINE_SURFACE_WITH_KNOTS ( 'NONE', 3, 1, ( 
 ( #109788, #33605 ),
 ( #15686, #32532 ),
 ( #85672, #49892 ),
 ( #46, #85122 ),
 ( #42582, #24100 ),
 ( #66703, #94073 ) ),
 .UNSPECIFIED., .F., .F., .F.,
 ( 4, 2, 4 ),
 ( 2, 2 ),
 ( 0.000000000000000000, 0.4999999999999998890, 1.000000000000000000 ),
 ( 0.000000000000000000, 1.000000000000000000 ),
 .UNSPECIFIED. ) ;
#105587 = CARTESIAN_POINT ( 'NONE',  ( -40.71298012283864409, 1433.226053685588113, 269.6231774168464881 ) ) ;
#105588 = CARTESIAN_POINT ( 'NONE',  ( -4.434803163540000703, 1409.571684121930048, 231.8514698793979960 ) ) ;
#105589 = CIRCLE ( 'NONE', #71655, 1.000000000000000888 ) ;
#105591 = ORIENTED_EDGE ( 'NONE', *, *, #90567, .T. ) ;
#105590 = CARTESIAN_POINT ( 'NONE',  ( 2.485536755124557740, 1523.919943579690425, 175.4381630812001731 ) ) ;
#105592 = AXIS2_PLACEMENT_3D ( 'NONE', #104870, #91911, #4618 ) ;
#105593 = CARTESIAN_POINT ( 'NONE',  ( 33.52142403570000084, 1451.742483455429920, 134.7272099485979879 ) ) ;
#105594 = CARTESIAN_POINT ( 'NONE',  ( 3.007039660992123942, 1441.535621290770678, 218.1727171084023382 ) ) ;
#105595 = CARTESIAN_POINT ( 'NONE',  ( -1.465793917108519917, 1484.360957496709943, 182.4810413606819850 ) ) ;
#105597 = EDGE_CURVE ( 'NONE', #106841, #29992, #7111, .T. ) ;
#105596 = CARTESIAN_POINT ( 'NONE',  ( 15.56469051819999905, 1506.798305132829910, 225.0756798403980099 ) ) ;
#105598 = CARTESIAN_POINT ( 'NONE',  ( 29.18127911709999722, 1415.346630214729885, 269.9487154676979799 ) ) ;
#105599 = CARTESIAN_POINT ( 'NONE',  ( 6.949265646015000186, 1517.089216728169959, 212.5747629931370000 ) ) ;
#105600 = CARTESIAN_POINT ( 'NONE',  ( -65.86513797469999076, 1379.742265928139886, 274.2610620464590170 ) ) ;
#105601 = CARTESIAN_POINT ( 'NONE',  ( -11.26183798051521734, 1427.523654888847886, 223.7584288158600714 ) ) ;
#105602 = CARTESIAN_POINT ( 'NONE',  ( 9.967911316253610821, 1425.849184522710175, 194.0881941884150024 ) ) ;
#105603 = CARTESIAN_POINT ( 'NONE',  ( 19.38665828288160142, 1498.812007524589944, 221.8202318911040152 ) ) ;
#105604 = CARTESIAN_POINT ( 'NONE',  ( -1.127928371535000140, 1516.989863902050047, 209.1319708558790182 ) ) ;
#105605 = ORIENTED_EDGE ( 'NONE', *, *, #92098, .T. ) ;
#105606 = CARTESIAN_POINT ( 'NONE',  ( 4.282777390491250280, 1420.607940666440072, 185.6069246241769974 ) ) ;
#105607 = CARTESIAN_POINT ( 'NONE',  ( -1.870446701440000137, 1420.451316163830143, 233.2770772963979766 ) ) ;
#105608 = CARTESIAN_POINT ( 'NONE',  ( -102.7364941740000006, 1384.940050820800025, 311.2335147922589726 ) ) ;
#105609 = ORIENTED_EDGE ( 'NONE', *, *, #93194, .T. ) ;
#105610 = CARTESIAN_POINT ( 'NONE',  ( -36.74521059231790332, 1385.199967091270082, 236.7483831902960105 ) ) ;
#105611 = ADVANCED_FACE ( 'NONE', ( #5646 ), #99122, .F. ) ;
#105612 = CARTESIAN_POINT ( 'NONE',  ( 18.96350866050000050, 1416.837080243330092, 210.2430642888180046 ) ) ;
#105613 = CARTESIAN_POINT ( 'NONE',  ( 9.225907677606100421, 1517.151704408390060, 198.5805875773771731 ) ) ;
#105614 = EDGE_CURVE ( 'NONE', #75668, #36772, #68493, .T. ) ;
#105615 = CARTESIAN_POINT ( 'NONE',  ( 7.548872300095000654, 1510.418062979259958, 203.9404357814470075 ) ) ;
#105616 = FACE_OUTER_BOUND ( 'NONE', #107460, .T. ) ;
#105617 = CARTESIAN_POINT ( 'NONE',  ( -0.08623196090545810766, 1420.451368587459910, 182.6995769445769895 ) ) ;
#105618 = AXIS2_PLACEMENT_3D ( 'NONE', #44250, #95741, #53206 ) ;
#105620 = CARTESIAN_POINT ( 'NONE',  ( 22.08327125186925599, 1523.604703353109699, 184.4267662568470598 ) ) ;
#105619 = CARTESIAN_POINT ( 'NONE',  ( -1.123101616545000070, 1517.157901477309906, 214.9105372957470195 ) ) ;
#105621 = CARTESIAN_POINT ( 'NONE',  ( 18.97264949710000081, 1509.488247120830010, 187.2484463636980081 ) ) ;
#105622 = FACE_OUTER_BOUND ( 'NONE', #92185, .T. ) ;
#105623 = VERTEX_POINT ( 'NONE', #102302 ) ;
#105624 = CARTESIAN_POINT ( 'NONE',  ( -0.7526715882979990724, 1516.710624944440042, 201.4081970979170251 ) ) ;
#105625 = DIRECTION ( 'NONE',  ( -0.8090169943749548898, -0.000000000000000000, -0.5877852522924631451 ) ) ;
#105626 = VERTEX_POINT ( 'NONE', #58672 ) ;
#105627 = CARTESIAN_POINT ( 'NONE',  ( 21.84020450222056908, 1523.481610426287716, 234.9798068779740277 ) ) ;
#105628 = EDGE_CURVE ( 'NONE', #63483, #69179, #77795, .T. ) ;
#105629 = CARTESIAN_POINT ( 'NONE',  ( -19.68364361186289813, 1519.551704408389924, 221.2357901434498615 ) ) ;
#105630 = CARTESIAN_POINT ( 'NONE',  ( 8.423122042745829319, 1511.533951550999973, 203.4036934630460109 ) ) ;
#105631 = CARTESIAN_POINT ( 'NONE',  ( 0.07018038471609880369, 1442.854703621289900, 218.7250898028690074 ) ) ;
#105632 = CARTESIAN_POINT ( 'NONE',  ( -26.67785352284090195, 1509.032684147069858, 201.4103146283430021 ) ) ;
#105633 = AXIS2_PLACEMENT_3D ( 'NONE', #82482, #20899, #106038 ) ;
#105634 = CARTESIAN_POINT ( 'NONE',  ( -2.704720143830000367, 1447.053020115450181, 167.4681766834979726 ) ) ;
#105636 = ADVANCED_FACE ( 'NONE', ( #39229 ), #35729, .T. ) ;
#105635 = CARTESIAN_POINT ( 'NONE',  ( -17.60866373010000174, 1424.118365038330012, 226.6925037000980012 ) ) ;
#105637 = CARTESIAN_POINT ( 'NONE',  ( 16.66936639845631518, 1523.382868172864164, 180.4828114240739296 ) ) ;
#105638 = CARTESIAN_POINT ( 'NONE',  ( -4.890969413286970102, 1464.492716438699972, 199.2455826196770090 ) ) ;
#105639 = CARTESIAN_POINT ( 'NONE',  ( 19.53786426059019021, 1512.187213306747481, 179.5239794925693388 ) ) ;
#105641 = CARTESIAN_POINT ( 'NONE',  ( -18.96055153501447421, 1439.098414281957730, 210.2943801834743454 ) ) ;
#105640 = CARTESIAN_POINT ( 'NONE',  ( 0.3105706251539200324, 1408.923906415619967, 232.1808711561190250 ) ) ;
#105642 = CARTESIAN_POINT ( 'NONE',  ( -9.983709645732758986, 1472.259764172770019, 211.0763333463989966 ) ) ;
#105643 = EDGE_LOOP ( 'NONE', ( #1362, #92883, #22072, #24143 ) ) ;
#105644 = CARTESIAN_POINT ( 'NONE',  ( 7.821732060355000016, 1516.863303996349941, 216.8564630578470087 ) ) ;
#105645 = CARTESIAN_POINT ( 'NONE',  ( -14.53800271749999951, 1508.448877354789829, 216.0591006970490184 ) ) ;
#105646 = DIRECTION ( 'NONE',  ( -0.6736849260863837507, 0.000000000000000000, 0.7390186874254154326 ) ) ;
#105647 = EDGE_CURVE ( 'NONE', #32282, #13288, #5272, .T. ) ;
#105648 = CARTESIAN_POINT ( 'NONE',  ( -24.15153577330000090, 1438.063256318689810, 212.1983434544380032 ) ) ;
#105649 = DIRECTION ( 'NONE',  ( -1.755985294532469921E-16, 1.000000000000000000, -1.338183447452831989E-16 ) ) ;
#105650 = CARTESIAN_POINT ( 'NONE',  ( -18.59438479510000164, 1507.626747889230046, 229.7138951080980007 ) ) ;
#105651 = FACE_OUTER_BOUND ( 'NONE', #21563, .T. ) ;
#105652 = DIRECTION ( 'NONE',  ( 0.3096375404471009563, -0.4473880807146179417, -0.8390283063045967937 ) ) ;
#105653 = CARTESIAN_POINT ( 'NONE',  ( -24.89839821108130025, 1440.936833924440180, 210.4291215488500200 ) ) ;
#105654 = DIRECTION ( 'NONE',  ( -0.9948834766775036531, 1.294385792140559950E-15, -0.1010290445074239624 ) ) ;
#105655 = EDGE_CURVE ( 'NONE', #36202, #41783, #104573, .T. ) ;
#105656 = EDGE_CURVE ( 'NONE', #59250, #87156, #33749, .T. ) ;
#105657 = CARTESIAN_POINT ( 'NONE',  ( -8.181710101844450023, 1488.271543501559790, 217.5078058625639983 ) ) ;
#105658 = CARTESIAN_POINT ( 'NONE',  ( -16.53114558859999761, 1465.611456236089907, 220.7423132190989747 ) ) ;
#105659 = CARTESIAN_POINT ( 'NONE',  ( -77.25135237149000034, 1383.779025680539917, 301.6761197000710126 ) ) ;
#105660 = CARTESIAN_POINT ( 'NONE',  ( -109.1401334702460133, 1384.096248926530052, 311.1747910708369886 ) ) ;
#105661 =( BOUNDED_CURVE ( )  B_SPLINE_CURVE ( 3, ( #67657, #29753, #48790, #57193 ),
 .UNSPECIFIED., .F., .F. ) 
 B_SPLINE_CURVE_WITH_KNOTS ( ( 4, 4 ),
 ( 1.025211572815232008, 1.340431719809825895 ),
 .UNSPECIFIED. ) 
 CURVE ( )  GEOMETRIC_REPRESENTATION_ITEM ( )  RATIONAL_B_SPLINE_CURVE ( ( 1.000000000000000000, 0.9917368149478550388, 0.9917368149478550388, 1.000000000000000000 ) ) 
 REPRESENTATION_ITEM ( '' )  );
#105662 = CARTESIAN_POINT ( 'NONE',  ( 8.051687730190000281, 1428.206419125489901, 213.2401846629289821 ) ) ;
#105664 = ORIENTED_EDGE ( 'NONE', *, *, #50251, .T. ) ;
#105663 = CARTESIAN_POINT ( 'NONE',  ( 9.374720191569998917, 1498.531797635389921, 228.6938383677990316 ) ) ;
#105665 = AXIS2_PLACEMENT_3D ( 'NONE', #40806, #15030, #23982 ) ;
#105666 = CARTESIAN_POINT ( 'NONE',  ( -88.44418928299998583, 1380.083824802999970, 304.2210320317589662 ) ) ;
#105667 = CARTESIAN_POINT ( 'NONE',  ( 20.03226456047849879, 1509.090742603719946, 229.7466210559209969 ) ) ;
#105668 = ORIENTED_EDGE ( 'NONE', *, *, #54007, .F. ) ;
#105669 = ORIENTED_EDGE ( 'NONE', *, *, #76878, .T. ) ;
#105670 = CARTESIAN_POINT ( 'NONE',  ( 17.13018491840009716, 1414.971993471370070, 210.1258406375170011 ) ) ;
#105671 = CARTESIAN_POINT ( 'NONE',  ( 13.03597514149999981, 1508.085462669229855, 233.2284867411979974 ) ) ;
#105672 = CARTESIAN_POINT ( 'NONE',  ( 13.33697072603180622, 1443.292755780022844, 169.3747417453497235 ) ) ;
#105674 = CARTESIAN_POINT ( 'NONE',  ( -5.038677013370000068, 1466.838857908529917, 244.5742075694979860 ) ) ;
#105673 = CARTESIAN_POINT ( 'NONE',  ( 29.81586140656836292, 1419.442089572837176, 269.4688564823842398 ) ) ;
#105675 = CARTESIAN_POINT ( 'NONE',  ( -20.37201606160000367, 1506.520234984129957, 189.4987160947980271 ) ) ;
#105676 = CARTESIAN_POINT ( 'NONE',  ( -11.86277575849999977, 1433.458230554240117, 150.5156657703979874 ) ) ;
#105677 = CARTESIAN_POINT ( 'NONE',  ( 2.087496205359999912, 1487.118434918990033, 216.9290059995090019 ) ) ;
#105678 = CARTESIAN_POINT ( 'NONE',  ( -19.62677431030000008, 1486.135797666930102, 190.0069177851979987 ) ) ;
#105679 = CARTESIAN_POINT ( 'NONE',  ( 6.022115808500000611, 1410.057305242329903, 186.7793557827980067 ) ) ;
#105680 = CARTESIAN_POINT ( 'NONE',  ( 4.921337687010000295, 1421.568449892030003, 185.6518752963980035 ) ) ;
#105682 = EDGE_CURVE ( 'NONE', #89942, #72154, #3063, .T. ) ;
#105681 = CARTESIAN_POINT ( 'NONE',  ( -1.201530806679770080, 1515.093215458460008, 213.4505504663210047 ) ) ;
#105683 = CARTESIAN_POINT ( 'NONE',  ( 7.259422694309999535, 1440.164840772029947, 154.1325276865980243 ) ) ;
#105684 = CARTESIAN_POINT ( 'NONE',  ( -4.329112086532120429, 1476.833686876630054, 219.7848579265929914 ) ) ;
#105685 = AXIS2_PLACEMENT_3D ( 'NONE', #2589, #20990, #96065 ) ;
#105686 = B_SPLINE_CURVE_WITH_KNOTS ( 'NONE', 3,
 ( #78755, #59757, #60305, #94425 ),
 .UNSPECIFIED., .F., .F.,
 ( 4, 4 ),
 ( 0.000000000000000000, 1.000000000000000000 ),
 .UNSPECIFIED. ) ;
#105687 = CARTESIAN_POINT ( 'NONE',  ( -9.384832308269999146, 1452.150223719329915, 152.4418518133980172 ) ) ;
#105689 = ORIENTED_EDGE ( 'NONE', *, *, #90299, .F. ) ;
#105688 = CARTESIAN_POINT ( 'NONE',  ( 1.959285284397550120, 1474.800623515119923, 220.3715842348549927 ) ) ;
#105690 = ORIENTED_EDGE ( 'NONE', *, *, #15109, .T. ) ;
#105691 = CARTESIAN_POINT ( 'NONE',  ( -13.54199508319999978, 1506.857021832190185, 209.2226570286780145 ) ) ;
#105692 = CARTESIAN_POINT ( 'NONE',  ( 9.839796275310359164, 1492.609014552419922, 188.3573332966260239 ) ) ;
#105693 = CARTESIAN_POINT ( 'NONE',  ( -33.10222556109999914, 1460.414048409229963, 269.7553217547979898 ) ) ;
#105694 = CARTESIAN_POINT ( 'NONE',  ( -9.638115897704999213, 1517.051704408389924, 203.7504991310570119 ) ) ;
#105696 = CLOSED_SHELL ( 'NONE', ( #46609, #54994, #62697, #13313, #34357, #58981, #56614, #100886, #105495, #58502, #44028, #79553, #842, #34547, #29827, #7946, #40190, #100161, #76027, #69259, #99962, #37377, #20710, #38442, #30413, #52030, #1456, #65178, #60415, #37136, #89787, #109662, #6533, #87303, #30437, #25578, #33563, #98784, #86447, #737, #26985, #41420, #61198, #45267, #27487, #6489, #37513, #87108, #38583, #86352, #11081, #85658, #109215, #39149, #101268, #7598, #392, #66764, #86254, #18714, #45980, #11969, #69520, #46733, #76973, #91984, #11925, #2259, #98790, #3011, #63023, #45011, #49648, #73254, #22017, #74186, #28990, #19289, #79609, #82680, #67383, #3296, #17366 ) ) ;
#105695 = CARTESIAN_POINT ( 'NONE',  ( 6.484578373979999810, 1434.540925522399903, 154.7070604761979951 ) ) ;
#105697 = DIRECTION ( 'NONE',  ( -0.000000000000000000, -1.000000000000000000, -0.000000000000000000 ) ) ;
#105698 = CARTESIAN_POINT ( 'NONE',  ( 4.328264056533019932, 1515.110035495290049, 210.1077469519609906 ) ) ;
#105699 = CARTESIAN_POINT ( 'NONE',  ( 3.824257248145499943, 1484.587375475480030, 220.3370414412930245 ) ) ;
#105700 = CIRCLE ( 'NONE', #59180, 2.000000000730000949 ) ;
#105701 = CARTESIAN_POINT ( 'NONE',  ( -10.48877660729999839, 1461.381695361490074, 212.5316338973990185 ) ) ;
#105702 = CARTESIAN_POINT ( 'NONE',  ( 9.060256214184169821, 1361.711347158616718, 207.6218459616987673 ) ) ;
#105703 = CARTESIAN_POINT ( 'NONE',  ( -45.82251511589010562, 1436.720346514069888, 268.2155769059959880 ) ) ;
#105704 = ORIENTED_EDGE ( 'NONE', *, *, #28969, .F. ) ;
#105705 = CARTESIAN_POINT ( 'NONE',  ( -3.532607207562010299, 1491.098995286199852, 181.6594233187500151 ) ) ;
#105706 = EDGE_LOOP ( 'NONE', ( #100562, #102416, #81247, #69872 ) ) ;
#105707 = CARTESIAN_POINT ( 'NONE',  ( -2.476170635034999901, 1516.819260244609950, 210.8389306816469855 ) ) ;
#105708 = CIRCLE ( 'NONE', #86018, 1.500000000000001332 ) ;
#105709 = CARTESIAN_POINT ( 'NONE',  ( -0.5890887500919903541, 1526.382868172863937, 243.2762031678882977 ) ) ;
#105710 = CARTESIAN_POINT ( 'NONE',  ( -20.61551574950000187, 1508.364577319530099, 190.3819664504979983 ) ) ;
#105711 = CARTESIAN_POINT ( 'NONE',  ( -15.55320418710000041, 1425.421141778929950, 190.3538950101980163 ) ) ;
#105712 = CARTESIAN_POINT ( 'NONE',  ( 2.220665158331510014, 1495.679845400359909, 221.2599143071639958 ) ) ;
#105713 = ORIENTED_EDGE ( 'NONE', *, *, #9714, .F. ) ;
#105714 = CARTESIAN_POINT ( 'NONE',  ( -2.664386649677787045, 1523.844782250835124, 176.1122499388616234 ) ) ;
#105715 = B_SPLINE_CURVE_WITH_KNOTS ( 'NONE', 5,
 ( #83075, #33212, #24254, #92026, #76329, #58989 ),
 .UNSPECIFIED., .F., .F.,
 ( 6, 6 ),
 ( 0.000000000000000000, 1.000000000000000000 ),
 .UNSPECIFIED. ) ;
#105716 = CARTESIAN_POINT ( 'NONE',  ( 1.709384572955000126, 1517.224900789629828, 201.7820965968870155 ) ) ;
#105717 = TOROIDAL_SURFACE ( 'NONE', #82451, 8.800000000000000711, 1.000000000000000000 ) ;
#105718 = DIRECTION ( 'NONE',  ( 2.041467857569999829E-16, -1.000000000000000000, 5.573852046271030309E-16 ) ) ;
#105719 = CARTESIAN_POINT ( 'NONE',  ( -9.934732886592909651, 1439.684679282129991, 207.9389421599310026 ) ) ;
#105720 = ORIENTED_EDGE ( 'NONE', *, *, #97304, .F. ) ;
#105721 = CARTESIAN_POINT ( 'NONE',  ( -19.35248331488120144, 1411.084690813580210, 270.2222661304289772 ) ) ;
#105722 = CARTESIAN_POINT ( 'NONE',  ( 0.7533003524100010395, 1516.992029636990083, 209.8620668306199946 ) ) ;
#105723 = CARTESIAN_POINT ( 'NONE',  ( 3.620601295783090201, 1417.932068788450124, 233.8910581729880391 ) ) ;
#105724 = CARTESIAN_POINT ( 'NONE',  ( 0.000000000000000000, 1518.913060387330006, 209.1218459616979999 ) ) ;
#105726 = VERTEX_POINT ( 'NONE', #45751 ) ;
#105725 = CARTESIAN_POINT ( 'NONE',  ( -5.962554884090152996, 1367.290268553626447, 210.6218459617142003 ) ) ;
#105727 = VERTEX_POINT ( 'NONE', #103395 ) ;
#105728 = CARTESIAN_POINT ( 'NONE',  ( 45.62376250662960331, 1441.740454976975570, 268.9751154461204692 ) ) ;
#105729 = CARTESIAN_POINT ( 'NONE',  ( -1.565479927690150097, 1467.839058700010128, 220.1279929306939778 ) ) ;
#105730 = CARTESIAN_POINT ( 'NONE',  ( -8.178500771994089646, 1441.152429774469965, 153.9860759686779943 ) ) ;
#105731 = CARTESIAN_POINT ( 'NONE',  ( -0.006923030120857438796, 1408.920737911269953, 186.3147001159109948 ) ) ;
#105732 = CIRCLE ( 'NONE', #57466, 29.84605316870980829 ) ;
#105733 = DIRECTION ( 'NONE',  ( 0.4436356471204865315, 1.250495761681361773E-32, 0.8962072375315807138 ) ) ;
#105734 = CARTESIAN_POINT ( 'NONE',  ( -18.07596433670000025, 1430.799689938030269, 226.2266804869980206 ) ) ;
#105735 = CARTESIAN_POINT ( 'NONE',  ( -14.20204669740000014, 1416.837080256030276, 221.7382503415979897 ) ) ;
#105736 = CARTESIAN_POINT ( 'NONE',  ( 11.95871496589999872, 1415.628674276829770, 223.2763524143979907 ) ) ;
#105737 = CARTESIAN_POINT ( 'NONE',  ( -17.37024900971054109, 1422.638029353652428, 226.5732080476987562 ) ) ;
#105738 = CARTESIAN_POINT ( 'NONE',  ( 0.7353365397730019515, 1516.995911393979895, 206.2425275143270085 ) ) ;
#105739 = EDGE_LOOP ( 'NONE', ( #43710, #53464, #35443, #6675 ) ) ;
#105740 = CARTESIAN_POINT ( 'NONE',  ( -2.918137311410000212, 1438.508781642889971, 227.5106010738990108 ) ) ;
#105741 = DIRECTION ( 'NONE',  ( 3.828568698926946970E-16, 0.000000000000000000, -1.000000000000000000 ) ) ;
#105742 = ORIENTED_EDGE ( 'NONE', *, *, #4401, .F. ) ;
#105743 = CARTESIAN_POINT ( 'NONE',  ( 4.562141516099857519, 1457.338505932022372, 228.3743572140680556 ) ) ;
#105744 = ADVANCED_FACE ( 'NONE', ( #11574 ), #70406, .F. ) ;
#105745 = CARTESIAN_POINT ( 'NONE',  ( 23.96827632182870005, 1452.076072134780134, 136.6874999515719935 ) ) ;
#105746 = FACE_OUTER_BOUND ( 'NONE', #47784, .T. ) ;
#105747 = CARTESIAN_POINT ( 'NONE',  ( -38.50281909529999780, 1385.190821792449924, 239.3058332809590070 ) ) ;
#105748 = DIRECTION ( 'NONE',  ( 0.9965074780645594155, -0.004098122787112013637, -0.08340294689657867799 ) ) ;
#105749 = CARTESIAN_POINT ( 'NONE',  ( 20.11149129760000065, 1409.615369146429884, 200.2383580101779899 ) ) ;
#105750 = CARTESIAN_POINT ( 'NONE',  ( -4.054154399340952786, 1446.253642567111228, 170.5365981393944992 ) ) ;
#105751 = CARTESIAN_POINT ( 'NONE',  ( 17.31558285710000078, 1410.013623662029886, 225.5276143365979920 ) ) ;
#105752 = CARTESIAN_POINT ( 'NONE',  ( 10.27511161340000001, 1489.668981243689814, 204.7180042823989936 ) ) ;
#105753 = CARTESIAN_POINT ( 'NONE',  ( 19.44117294853580091, 1456.941945407359981, 224.4539793896520052 ) ) ;
#105754 = CARTESIAN_POINT ( 'NONE',  ( 2.500000000000270450, 1439.222450974139974, 159.1124396249019810 ) ) ;
#105755 = CARTESIAN_POINT ( 'NONE',  ( -3.258474617075000079, 1517.083030555940013, 215.6838419306269827 ) ) ;
#105756 = CARTESIAN_POINT ( 'NONE',  ( 3.302453616664800418, 1524.523992613103019, 241.8698019156646239 ) ) ;
#105757 = ORIENTED_EDGE ( 'NONE', *, *, #70167, .F. ) ;
#105758 = CARTESIAN_POINT ( 'NONE',  ( -17.09418616900000032, 1417.376006423840181, 206.9664283537690039 ) ) ;
#105759 = PRESENTATION_LAYER_ASSIGNMENT (  '', '', ( #9198 ) ) ;
#105760 = CARTESIAN_POINT ( 'NONE',  ( 19.63708787179898962, 1526.382868172863937, 234.8228066531187324 ) ) ;
#105761 = LINE ( 'NONE', #80549, #41078 ) ;
#105762 = CARTESIAN_POINT ( 'NONE',  ( 11.90008666459999986, 1434.920851464509951, 147.6452002888979962 ) ) ;
#105763 = CARTESIAN_POINT ( 'NONE',  ( -38.67142060801120351, 1448.149028305610045, 136.4729251882360188 ) ) ;
#105764 = CARTESIAN_POINT ( 'NONE',  ( 10.85931684761558458, 1424.796817104864203, 138.1961031260640311 ) ) ;
#105765 = CARTESIAN_POINT ( 'NONE',  ( 1.930776842151626926, 1417.106403351838935, 232.9720933022255167 ) ) ;
#105766 = CARTESIAN_POINT ( 'NONE',  ( -3.721063415729999695E-09, 1475.837061091930082, 266.9611530633980010 ) ) ;
#105768 = ADVANCED_FACE ( 'NONE', ( #28369 ), #91857, .F. ) ;
#105767 = CARTESIAN_POINT ( 'NONE',  ( 11.13931297870000137, 1433.088362659679888, 151.6441982395979835 ) ) ;
#105769 = DIRECTION ( 'NONE',  ( 0.000000000000000000, 0.000000000000000000, 1.000000000000000000 ) ) ;
#105770 = CARTESIAN_POINT ( 'NONE',  ( -9.519777939162850089, 1460.017017711900053, 210.6312322783699926 ) ) ;
#105771 = CARTESIAN_POINT ( 'NONE',  ( 5.371346801045000063, 1520.551704408390151, 199.4837300725270097 ) ) ;
#105772 = CARTESIAN_POINT ( 'NONE',  ( -32.16776790210110448, 1524.538969332612623, 202.1449104801618262 ) ) ;
#105773 = ORIENTED_EDGE ( 'NONE', *, *, #22093, .T. ) ;
#105774 = EDGE_CURVE ( 'NONE', #39998, #89473, #30279, .T. ) ;
#105775 = CARTESIAN_POINT ( 'NONE',  ( 22.68012700155740191, 1507.275789587059990, 209.7693291172490149 ) ) ;
#105776 = CARTESIAN_POINT ( 'NONE',  ( -6.391938905018056616, 1508.551704408390151, 202.1089245808659882 ) ) ;
#105777 = EDGE_CURVE ( 'NONE', #77212, #85181, #98873, .T. ) ;
#105778 = DIRECTION ( 'NONE',  ( -1.000000000000000000, 0.000000000000000000, 0.000000000000000000 ) ) ;
#105779 = CIRCLE ( 'NONE', #19990, 1.999999999999998668 ) ;
#105780 = CARTESIAN_POINT ( 'NONE',  ( -6.742045582256606551, 1509.032357776622348, 202.0097237844711344 ) ) ;
#105781 = CARTESIAN_POINT ( 'NONE',  ( 1.894852802010000170, 1507.091060773529989, 236.3260084363980127 ) ) ;
#105782 = EDGE_CURVE ( 'NONE', #80633, #68673, #54703, .T. ) ;
#105783 = CARTESIAN_POINT ( 'NONE',  ( -16.83198307403168315, 1526.000688113731940, 235.9162354437811473 ) ) ;
#105784 = CARTESIAN_POINT ( 'NONE',  ( -11.99699175549999985, 1508.052959061330057, 233.6129359570980171 ) ) ;
#105785 = CARTESIAN_POINT ( 'NONE',  ( -23.21699021137670016, 1383.850094297019950, 222.3556410448979932 ) ) ;
#105786 = CARTESIAN_POINT ( 'NONE',  ( -2.487920634212330118, 1508.551704408389924, 204.1347675177020164 ) ) ;
#105787 = CARTESIAN_POINT ( 'NONE',  ( 10.68290885440000082, 1409.286115784929962, 219.9879125262980040 ) ) ;
#105788 = CARTESIAN_POINT ( 'NONE',  ( 0.000000000000000000, 1512.187213306747481, 209.1218459616979999 ) ) ;
#105789 = CARTESIAN_POINT ( 'NONE',  ( -113.4000000000000057, 1305.733110638860126, 304.2218459572590064 ) ) ;
#105791 = VERTEX_POINT ( 'NONE', #89380 ) ;
#105790 = CARTESIAN_POINT ( 'NONE',  ( -10.29630665101337073, 1435.300287559097114, 152.3007955122366184 ) ) ;
#105792 = CARTESIAN_POINT ( 'NONE',  ( -1.216112039750000040, 1452.488429528330016, 183.6485174699979837 ) ) ;
#105793 = VECTOR ( 'NONE', #85893, 1000.000000000000000 ) ;
#105794 = CARTESIAN_POINT ( 'NONE',  ( -9.222898088157986507, 1388.549295314689516, 200.8262261746918114 ) ) ;
#105795 = CARTESIAN_POINT ( 'NONE',  ( -3.023153272364219823, 1440.625623213970130, 157.2242917382399980 ) ) ;
#105797 = ORIENTED_EDGE ( 'NONE', *, *, #42568, .T. ) ;
#105796 = CARTESIAN_POINT ( 'NONE',  ( -17.15013451049770055, 1414.913057819779851, 207.6647986024049999 ) ) ;
#105798 = CARTESIAN_POINT ( 'NONE',  ( 10.99044919668839881, 1479.494726248550023, 229.8297398567180210 ) ) ;
#105799 = ORIENTED_EDGE ( 'NONE', *, *, #12007, .F. ) ;
#105800 =( BOUNDED_CURVE ( )  B_SPLINE_CURVE ( 3, ( #18571, #104811, #52766, #86905 ),
 .UNSPECIFIED., .F., .T. ) 
 B_SPLINE_CURVE_WITH_KNOTS ( ( 4, 4 ),
 ( 1.021828243325141994, 2.119764315462445037 ),
 .UNSPECIFIED. ) 
 CURVE ( )  GEOMETRIC_REPRESENTATION_ITEM ( )  RATIONAL_B_SPLINE_CURVE ( ( 1.000000000000000000, 0.9020423082557569305, 0.9020423082557569305, 1.000000000000000000 ) ) 
 REPRESENTATION_ITEM ( '' )  );
#105801 = CARTESIAN_POINT ( 'NONE',  ( -10.63240336516950002, 1387.911495707119911, 217.3146354632350210 ) ) ;
#105802 = CARTESIAN_POINT ( 'NONE',  ( 7.708815788408339920, 1516.526058372639909, 206.7773338513199803 ) ) ;
#105803 = CARTESIAN_POINT ( 'NONE',  ( 3.138931148605959913E-16, 1391.413060387289988, 209.1218459616989946 ) ) ;
#105804 = CARTESIAN_POINT ( 'NONE',  ( -3.034926079678203159, 1369.200812461396481, 210.6218459616991936 ) ) ;
#105805 = CARTESIAN_POINT ( 'NONE',  ( -1.233464473149999963, 1431.858984285389852, 217.8324935667789930 ) ) ;
#105806 = CARTESIAN_POINT ( 'NONE',  ( -10.21667613351959858, 1472.322293331309993, 207.1512473758539841 ) ) ;
#105807 = CARTESIAN_POINT ( 'NONE',  ( 13.48456462084389962, 1409.383951757389923, 215.5448620521310090 ) ) ;
#105808 = DIRECTION ( 'NONE',  ( 0.000000000000000000, 0.000000000000000000, 1.000000000000000000 ) ) ;
#105809 = CARTESIAN_POINT ( 'NONE',  ( -97.97442128001588912, 1385.215631988479799, 295.8423678355109701 ) ) ;
#105810 = EDGE_CURVE ( 'NONE', #23280, #17035, #22987, .T. ) ;
#105811 = CARTESIAN_POINT ( 'NONE',  ( -19.12773309319999981, 1463.218120443330008, 191.1290552211980014 ) ) ;
#105812 = CARTESIAN_POINT ( 'NONE',  ( -68.67274465469999711, 1379.748163774529985, 279.9618448723590518 ) ) ;
#105813 = VECTOR ( 'NONE', #54126, 1000.000000000000000 ) ;
#105814 = CARTESIAN_POINT ( 'NONE',  ( 11.88070671566089942, 1491.927040624079837, 209.1634875332829893 ) ) ;
#105815 = ORIENTED_EDGE ( 'NONE', *, *, #92146, .T. ) ;
#105816 = ORIENTED_EDGE ( 'NONE', *, *, #84859, .F. ) ;
#105817 = ADVANCED_FACE ( 'NONE', ( #107011 ), #110777, .T. ) ;
#105818 = CARTESIAN_POINT ( 'NONE',  ( -12.00789815305109975, 1415.778512723939912, 194.9196753816330272 ) ) ;
#105819 = CARTESIAN_POINT ( 'NONE',  ( 2.350390795498939589, 1497.086630012390287, 196.9446188252720162 ) ) ;
#105820 = CARTESIAN_POINT ( 'NONE',  ( 30.03297113387935013, 1462.224093527517880, 269.4711606006897568 ) ) ;
#105821 = CARTESIAN_POINT ( 'NONE',  ( -29.78220350812331318, 1524.382868172863937, 221.7347658002330775 ) ) ;
#105822 = CARTESIAN_POINT ( 'NONE',  ( 5.071972357519999974, 1397.441751889229863, 221.0975735167979792 ) ) ;
#105823 = CARTESIAN_POINT ( 'NONE',  ( 30.90487439922552682, 1525.907212628473644, 201.8101144455178257 ) ) ;
#105824 = CARTESIAN_POINT ( 'NONE',  ( -1.441435333030000043, 1455.080611006229901, 183.7350912959979894 ) ) ;
#105825 = CARTESIAN_POINT ( 'NONE',  ( -10.75152334329300174, 1366.170224226380697, 207.6218459616987673 ) ) ;
#105826 = CARTESIAN_POINT ( 'NONE',  ( -26.28247728721726162, 1436.705573956322723, 136.8563548585942726 ) ) ;
#105827 = CARTESIAN_POINT ( 'NONE',  ( 6.933616821004999764, 1516.548716157039962, 206.8295387017270173 ) ) ;
#105828 = CARTESIAN_POINT ( 'NONE',  ( -13.10870366159999989, 1435.054409783779874, 149.9910397837979872 ) ) ;
#105829 = CARTESIAN_POINT ( 'NONE',  ( -8.315526934679999371, 1385.338042180710090, 218.6773504991989796 ) ) ;
#105830 = CARTESIAN_POINT ( 'NONE',  ( 1.342027776509999937, 1416.827520077930103, 190.1634478202980176 ) ) ;
#105831 = CARTESIAN_POINT ( 'NONE',  ( 2.144608228480000101, 1498.044160227690099, 197.8976463139989903 ) ) ;
#105832 = CARTESIAN_POINT ( 'NONE',  ( -15.97576971693890080, 1477.217383298640016, 229.1973553141059767 ) ) ;
#105833 = CARTESIAN_POINT ( 'NONE',  ( 33.28034951413926734, 1522.862737210650039, 200.8029765415138286 ) ) ;
#105834 = ORIENTED_EDGE ( 'NONE', *, *, #68911, .T. ) ;
#105835 = CARTESIAN_POINT ( 'NONE',  ( 7.571416212307459759, 1423.019345442000031, 195.7264161909869813 ) ) ;
#105836 = CARTESIAN_POINT ( 'NONE',  ( -26.99303384999999977, 1488.687911585429902, 206.6276365953079903 ) ) ;
#105838 = FACE_OUTER_BOUND ( 'NONE', #19800, .T. ) ;
#105837 = CARTESIAN_POINT ( 'NONE',  ( -9.971616305214038078, 1425.233230934379890, 92.74877973774999873 ) ) ;
#105839 = CARTESIAN_POINT ( 'NONE',  ( 1.716045945209999868, 1509.007693206030126, 179.5167849949980052 ) ) ;
#105840 = CARTESIAN_POINT ( 'NONE',  ( -26.00754374319999940, 1427.792721086330175, 240.2274373024979752 ) ) ;
#105841 = CARTESIAN_POINT ( 'NONE',  ( 20.59987592950000135, 1509.677367935830262, 230.5839143914980127 ) ) ;
#105842 = CARTESIAN_POINT ( 'NONE',  ( 0.9825367709745502776, 1415.585804587858775, 233.1616798236157990 ) ) ;
#105843 = CARTESIAN_POINT ( 'NONE',  ( 33.14937533060000163, 1451.602147045430002, 135.6094880980980122 ) ) ;
#105844 = ORIENTED_EDGE ( 'NONE', *, *, #93976, .F. ) ;
#105845 = CARTESIAN_POINT ( 'NONE',  ( -5.386516158502840490, 1432.363696384169998, 154.6077582407299928 ) ) ;
#105846 = CARTESIAN_POINT ( 'NONE',  ( 13.06910704241984966, 1513.473960729436385, 225.9112088208277953 ) ) ;
#105847 = CARTESIAN_POINT ( 'NONE',  ( 19.63722818094939981, 1517.051704408389924, 218.2362632588020119 ) ) ;
#105848 = ORIENTED_EDGE ( 'NONE', *, *, #5732, .F. ) ;
#105849 = ORIENTED_EDGE ( 'NONE', *, *, #63675, .F. ) ;
#105850 = CARTESIAN_POINT ( 'NONE',  ( -16.33316124910000156, 1384.804537353890055, 200.5738954341890121 ) ) ;
#105851 = CARTESIAN_POINT ( 'NONE',  ( 4.997202291739998969, 1423.732852402740264, 194.0938664950990074 ) ) ;
#105852 = VERTEX_POINT ( 'NONE', #30851 ) ;
#105853 = AXIS2_PLACEMENT_3D ( 'NONE', #110481, #68504, #67956 ) ;
#105854 = CARTESIAN_POINT ( 'NONE',  ( -0.7163550209979999694, 1413.835382546030132, 184.9556001181979923 ) ) ;
#105855 = CARTESIAN_POINT ( 'NONE',  ( -5.812939435032099311, 1419.537318060671623, 194.8608174217619649 ) ) ;
#105856 = CARTESIAN_POINT ( 'NONE',  ( 0.3483522942510000053, 1452.334144580529937, 183.2984807459980061 ) ) ;
#105857 = CARTESIAN_POINT ( 'NONE',  ( -1.072720051239999917, 1489.064677756729907, 236.4182509688979792 ) ) ;
#105858 = CARTESIAN_POINT ( 'NONE',  ( -1.288405174186285418, 1419.848498354222329, 185.1203288673806924 ) ) ;
#105859 = EDGE_LOOP ( 'NONE', ( #98400, #16435, #81263, #40434, #53207, #18682, #37142, #96995 ) ) ;
#105860 = CARTESIAN_POINT ( 'NONE',  ( 11.63661014589999887, 1425.864895317229866, 144.1626081066980021 ) ) ;
#105861 = CARTESIAN_POINT ( 'NONE',  ( -12.31551432481460040, 1414.913060387399810, 219.9842977860079998 ) ) ;
#105862 = CARTESIAN_POINT ( 'NONE',  ( 14.86247180250000000, 1485.705779184129824, 225.2758283624980038 ) ) ;
#105863 = ORIENTED_EDGE ( 'NONE', *, *, #44902, .T. ) ;
#105864 = CARTESIAN_POINT ( 'NONE',  ( -1.131796848745000084, 1516.659138130710289, 203.3488676535569937 ) ) ;
#105865 = ORIENTED_EDGE ( 'NONE', *, *, #22789, .F. ) ;
#105866 = CARTESIAN_POINT ( 'NONE',  ( 11.86444742414140130, 1432.220480012309963, 149.9811424069689849 ) ) ;
#105867 = CARTESIAN_POINT ( 'NONE',  ( 12.72342974552460682, 1445.008495287113647, 186.4128679283859356 ) ) ;
#105868 = ORIENTED_EDGE ( 'NONE', *, *, #26363, .T. ) ;
#105869 = VERTEX_POINT ( 'NONE', #48789 ) ;
#105870 = CARTESIAN_POINT ( 'NONE',  ( -18.18137283769999968, 1507.546748828630143, 231.7129783355979669 ) ) ;
#105871 = CARTESIAN_POINT ( 'NONE',  ( -29.82178186784418727, 1526.306647125542440, 216.9179131060151633 ) ) ;
#105872 = FACE_OUTER_BOUND ( 'NONE', #4326, .T. ) ;
#105873 = CARTESIAN_POINT ( 'NONE',  ( -8.603211701180001114, 1469.317673379189955, 216.5015782100589945 ) ) ;
#105874 = DIRECTION ( 'NONE',  ( 0.6987313624946034363, 0.07895079864675673409, -0.7110142434997167582 ) ) ;
#105875 = CARTESIAN_POINT ( 'NONE',  ( 0.9866695707572261664, 1407.933421795380127, 270.2925939168970331 ) ) ;
#105876 = CARTESIAN_POINT ( 'NONE',  ( -4.146782895030730387, 1426.018316030089863, 186.1121555109529879 ) ) ;
#105877 = CARTESIAN_POINT ( 'NONE',  ( 19.53786426059019021, 1512.187213306747481, 181.5239794925693388 ) ) ;
#105878 = CARTESIAN_POINT ( 'NONE',  ( -19.94575122458989469, 1509.638991226211601, 231.0845654444641468 ) ) ;
#105879 = CARTESIAN_POINT ( 'NONE',  ( 0.03112280646364588149, 1410.164110630448931, 233.2100737522354734 ) ) ;
#105881 = CARTESIAN_POINT ( 'NONE',  ( -105.5476282266839974, 1391.479847970690116, 304.9206647878619947 ) ) ;
#105880 = CARTESIAN_POINT ( 'NONE',  ( -13.39453303099999992, 1503.483788606090002, 208.7029727493389828 ) ) ;
#105882 = CARTESIAN_POINT ( 'NONE',  ( 11.70359515955249918, 1422.053249383299999, 207.2442419415079655 ) ) ;
#105883 = CARTESIAN_POINT ( 'NONE',  ( -24.95049239925220164, 1509.561083361290002, 222.7521736304589979 ) ) ;
#105884 = CARTESIAN_POINT ( 'NONE',  ( -7.266995445965000577, 1512.686126173209914, 202.3407130533369980 ) ) ;
#105885 = VERTEX_POINT ( 'NONE', #99695 ) ;
#105886 = CARTESIAN_POINT ( 'NONE',  ( 10.04572263670000076, 1417.623152644130187, 255.3819207803980191 ) ) ;
#105887 = CIRCLE ( 'NONE', #7557, 1.000000000000000000 ) ;
#105888 = B_SPLINE_CURVE_WITH_KNOTS ( 'NONE', 4,
 ( #32149, #5856, #108305, #109968, #50072 ),
 .UNSPECIFIED., .F., .F.,
 ( 5, 5 ),
 ( 1.967616199060000071, 3.613988937050000239 ),
 .UNSPECIFIED. ) ;
#105889 = CARTESIAN_POINT ( 'NONE',  ( 18.67054467737644075, 1509.506033878418975, 187.1506692568550534 ) ) ;
#105890 = CARTESIAN_POINT ( 'NONE',  ( -59.61868368084140002, 1385.068020327440081, 280.3090023487520170 ) ) ;
#105891 = CARTESIAN_POINT ( 'NONE',  ( -8.888758267720000106, 1385.314821192629779, 218.6605176881890031 ) ) ;
#105892 = DIRECTION ( 'NONE',  ( 0.000000000000000000, 0.000000000000000000, 1.000000000000000000 ) ) ;
#105893 = CARTESIAN_POINT ( 'NONE',  ( -14.77171694839999994, 1415.677402209299999, 212.1703745851490055 ) ) ;
#105894 = AXIS2_PLACEMENT_3D ( 'NONE', #58458, #15857, #67980 ) ;
#105896 = VERTEX_POINT ( 'NONE', #64492 ) ;
#105895 = CARTESIAN_POINT ( 'NONE',  ( -15.77795547941580168, 1420.228508977689899, 210.6635392844780199 ) ) ;
#105897 = CARTESIAN_POINT ( 'NONE',  ( -15.88245123595834585, 1415.955066226697454, 209.7358280198473039 ) ) ;
#105898 = CARTESIAN_POINT ( 'NONE',  ( 12.71038982811789886, 1507.471771741610155, 233.3404631503599944 ) ) ;
#105899 = DIRECTION ( 'NONE',  ( 0.000000000000000000, 0.000000000000000000, 1.000000000000000000 ) ) ;
#105901 = EDGE_CURVE ( 'NONE', #65085, #29403, #8492, .T. ) ;
#105900 = CARTESIAN_POINT ( 'NONE',  ( 1.069043333538070017, 1430.790655322590055, 199.7345386470830135 ) ) ;
#105902 = CARTESIAN_POINT ( 'NONE',  ( 15.01814799273499901, 1514.214451716350140, 223.8476172842669882 ) ) ;
#105903 = CARTESIAN_POINT ( 'NONE',  ( -12.30608628080000067, 1442.741623762909967, 186.5150421474980078 ) ) ;
#105904 = CARTESIAN_POINT ( 'NONE',  ( 19.38267550565620212, 1509.603095404120040, 231.8230532176900169 ) ) ;
#105905 = CARTESIAN_POINT ( 'NONE',  ( 7.914828484685850540, 1459.913996726710138, 203.2501674748179994 ) ) ;
#105906 = CARTESIAN_POINT ( 'NONE',  ( 12.63095811414796898, 1434.552017584898522, 149.3952382085417696 ) ) ;
#105907 = CARTESIAN_POINT ( 'NONE',  ( 15.96415235769999974, 1412.748275509629821, 227.0251384850979832 ) ) ;
#105908 = CARTESIAN_POINT ( 'NONE',  ( -5.463886630600000238, 1476.963513525689905, 218.4976191159190080 ) ) ;
#105909 = CARTESIAN_POINT ( 'NONE',  ( -21.33281718256813875, 1523.429859730331145, 237.7590525783452335 ) ) ;
#105910 = CARTESIAN_POINT ( 'NONE',  ( -1.136814071995000175, 1516.854133554269993, 206.8377924607469822 ) ) ;
#105911 = CARTESIAN_POINT ( 'NONE',  ( 45.97783906840000157, 1436.874426342759989, 266.9777547047980306 ) ) ;
#105912 = CARTESIAN_POINT ( 'NONE',  ( -17.93887750940000103, 1409.704405018330135, 223.7856054849979728 ) ) ;
#105913 = CARTESIAN_POINT ( 'NONE',  ( 16.37332010780000147, 1435.060612807570124, 147.2880571655980191 ) ) ;
#105914 = CARTESIAN_POINT ( 'NONE',  ( 26.86204967519999798, 1508.007394501330054, 206.2315949059079969 ) ) ;
#105915 = CARTESIAN_POINT ( 'NONE',  ( 29.77439797945870126, 1509.998809754348486, 209.4099699424615153 ) ) ;
#105916 = EDGE_CURVE ( 'NONE', #27462, #41473, #42851, .T. ) ;
#105917 = CARTESIAN_POINT ( 'NONE',  ( -12.28062996578079868, 1378.241810724349989, 208.0559987543549880 ) ) ;
#105918 = CARTESIAN_POINT ( 'NONE',  ( -23.58453086489999961, 1470.876928620230046, 266.7402721287979830 ) ) ;
#105919 = CYLINDRICAL_SURFACE ( 'NONE', #78097, 33.13701971169416538 ) ;
#105920 = CYLINDRICAL_SURFACE ( 'NONE', #9841, 2.000000000000003553 ) ;
#105921 = DIRECTION ( 'NONE',  ( 5.980589973904019347E-17, -1.000000000000000000, 1.736889445713099699E-16 ) ) ;
#105922 = CARTESIAN_POINT ( 'NONE',  ( -14.37237490289999897, 1409.238075345830111, 207.8572050715280000 ) ) ;
#105923 = FACE_OUTER_BOUND ( 'NONE', #92148, .T. ) ;
#105924 = CARTESIAN_POINT ( 'NONE',  ( -12.51292156319999904, 1441.547097317919906, 187.9392280838980014 ) ) ;
#105925 = EDGE_CURVE ( 'NONE', #86024, #27781, #88511, .T. ) ;
#105926 = CARTESIAN_POINT ( 'NONE',  ( -7.551930971255839786, 1384.476535447399783, 219.0683411548229742 ) ) ;
#105927 = CARTESIAN_POINT ( 'NONE',  ( 12.91340936269999951, 1434.774317664089949, 146.7590612318980163 ) ) ;
#105928 = CARTESIAN_POINT ( 'NONE',  ( -34.11564357272870041, 1435.688851149340280, 134.0999999980979851 ) ) ;
#105929 = DIRECTION ( 'NONE',  ( 0.000000000000000000, 0.000000000000000000, 1.000000000000000000 ) ) ;
#105930 = ORIENTED_EDGE ( 'NONE', *, *, #61681, .F. ) ;
#105931 = CARTESIAN_POINT ( 'NONE',  ( 6.372167600494999640, 1511.069621805459974, 216.5183910133270047 ) ) ;
#105932 = CARTESIAN_POINT ( 'NONE',  ( 40.13864028269999551, 1442.238426966730003, 136.9590191442979972 ) ) ;
#105933 = CARTESIAN_POINT ( 'NONE',  ( 18.46438756856120023, 1509.557851009430124, 186.5303332237980101 ) ) ;
#105934 = B_SPLINE_CURVE_WITH_KNOTS ( 'NONE', 5,
 ( #97669, #88730, #70860, #89267, #104971, #55146, #106613, #88180, #71417, #20941, #28260, #11472, #45093, #46743, #37220, #105532, #80875, #28821 ),
 .UNSPECIFIED., .F., .F.,
 ( 6, 3, 3, 3, 3, 6 ),
 ( 0.000000000000000000, 0.3094080260441300911, 0.6147993323560541068, 0.7644424561903261361, 0.8931847307547668979, 1.000000000000000000 ),
 .UNSPECIFIED. ) ;
#105935 = CARTESIAN_POINT ( 'NONE',  ( -13.59236974158869948, 1508.248953138170009, 209.5387658739280141 ) ) ;
#105936 = CARTESIAN_POINT ( 'NONE',  ( -12.31949146158819985, 1378.253793448930082, 209.5105130821430066 ) ) ;
#105937 = CARTESIAN_POINT ( 'NONE',  ( -26.99778882349999876, 1469.302995409530013, 268.7552990114980389 ) ) ;
#105938 = CARTESIAN_POINT ( 'NONE',  ( -30.11857922865454640, 1525.055427061272439, 196.5532548484356141 ) ) ;
#105939 = LINE ( 'NONE', #3488, #104959 ) ;
#105940 = CARTESIAN_POINT ( 'NONE',  ( -28.51853658599999974, 1509.908949629729932, 214.4930692104080094 ) ) ;
#105941 = CARTESIAN_POINT ( 'NONE',  ( -0.8945946638535250406, 1417.298095655010002, 235.8147265033050246 ) ) ;
#105942 = CARTESIAN_POINT ( 'NONE',  ( -31.77495577332650001, 1384.972186697860025, 206.5720684459180063 ) ) ;
#105943 = CARTESIAN_POINT ( 'NONE',  ( 17.89572889415259738, 1423.787865911519930, 225.8712852353089886 ) ) ;
#105944 = CARTESIAN_POINT ( 'NONE',  ( 21.33071589520000089, 1509.431526492729972, 227.7332358683979976 ) ) ;
#105945 = CARTESIAN_POINT ( 'NONE',  ( 15.38768853080000198, 1495.932765146430029, 224.1785865777980291 ) ) ;
#105946 = DIRECTION ( 'NONE',  ( -0.3282391760791590340, 0.000000000000000000, -0.9445946449598763284 ) ) ;
#105948 = ORIENTED_EDGE ( 'NONE', *, *, #38350, .T. ) ;
#105947 = CARTESIAN_POINT ( 'NONE',  ( -8.568313719024999386, 1512.631076693560090, 197.0179983452670172 ) ) ;
#105949 = CARTESIAN_POINT ( 'NONE',  ( -109.6574261609999894, 1384.907292521180125, 311.3230475462589766 ) ) ;
#105950 = CARTESIAN_POINT ( 'NONE',  ( 1.427985284410939970, 1474.785119020410093, 235.3823680754540248 ) ) ;
#105951 = EDGE_CURVE ( 'NONE', #17368, #68158, #55532, .T. ) ;
#105952 = DIRECTION ( 'NONE',  ( 0.1425040565888799349, 0.3680151204241798868, -0.9188348409779036885 ) ) ;
#105953 = CARTESIAN_POINT ( 'NONE',  ( -12.44601730950000018, 1416.547221147930031, 194.7757989389979798 ) ) ;
#105954 = CARTESIAN_POINT ( 'NONE',  ( 0.000000000000000000, 1401.254281879943164, 134.0999999980979851 ) ) ;
#105955 = CARTESIAN_POINT ( 'NONE',  ( 23.94687154950000263, 1411.110112760130050, 210.2130935636480160 ) ) ;
#105956 = CARTESIAN_POINT ( 'NONE',  ( -12.40096745299999981, 1434.347023119479900, 149.5501479441980166 ) ) ;
#105957 = CARTESIAN_POINT ( 'NONE',  ( 19.11847670520000264, 1460.287704656489950, 220.2677159749989926 ) ) ;
#105958 = DIRECTION ( 'NONE',  ( -1.755985294532469921E-16, 1.000000000000000000, -1.338183447452831989E-16 ) ) ;
#105960 = LINE ( 'NONE', #81825, #21759 ) ;
#105959 = CARTESIAN_POINT ( 'NONE',  ( -11.86923217650000062, 1432.580379542929904, 150.3965903535979862 ) ) ;
#105961 = DIRECTION ( 'NONE',  ( -0.1541492146682660325, 0.06142059477871750911, -0.9861366691053453648 ) ) ;
#105962 = CARTESIAN_POINT ( 'NONE',  ( -122.4487580624616498, 1378.528619065190014, 299.2784868977504402 ) ) ;
#105963 = LINE ( 'NONE', #29241, #41897 ) ;
#105964 = CARTESIAN_POINT ( 'NONE',  ( -22.53878282410000011, 1411.058442784730232, 212.0450770655079964 ) ) ;
#105965 = CARTESIAN_POINT ( 'NONE',  ( -9.936738324549999390, 1364.340818343089950, 210.6218459616991936 ) ) ;
#105966 = CARTESIAN_POINT ( 'NONE',  ( -7.722536802824999214, 1517.050041317280147, 204.5049460973469877 ) ) ;
#105967 = CARTESIAN_POINT ( 'NONE',  ( 13.37406854550570046, 1507.496451373729997, 233.0472692220099873 ) ) ;
#105968 = CARTESIAN_POINT ( 'NONE',  ( -15.45533207179999913, 1484.705735421829786, 187.3543539206980029 ) ) ;
#105969 = CIRCLE ( 'NONE', #91643, 1.999999999999998668 ) ;
#105970 = CARTESIAN_POINT ( 'NONE',  ( -8.316672828268760753, 1425.055149638239982, 204.9623390585310005 ) ) ;
#105971 = CARTESIAN_POINT ( 'NONE',  ( -4.282792884661109412, 1440.970302453239810, 156.0836163958929887 ) ) ;
#105973 = ORIENTED_EDGE ( 'NONE', *, *, #48403, .T. ) ;
#105972 = CARTESIAN_POINT ( 'NONE',  ( -67.34501255021619670, 1379.744579630669932, 278.5325692663910218 ) ) ;
#105974 = ORIENTED_EDGE ( 'NONE', *, *, #79453, .T. ) ;
#105975 = CARTESIAN_POINT ( 'NONE',  ( 28.39970178019999736, 1509.598990362429959, 212.0559822206679996 ) ) ;
#105976 = ORIENTED_EDGE ( 'NONE', *, *, #50233, .T. ) ;
#105977 = CARTESIAN_POINT ( 'NONE',  ( -105.0454790209999913, 1379.237143502780100, 304.6380415787589868 ) ) ;
#105978 = CARTESIAN_POINT ( 'NONE',  ( -109.1320112420000044, 1384.953741877089897, 311.2644403302589353 ) ) ;
#105979 = SHAPE_REPRESENTATION ( 'Crank Arm', ( #21632 ), #46788 ) ;
#105981 = CARTESIAN_POINT ( 'NONE',  ( 15.73136618761820316, 1409.565780267800164, 192.3644800552150116 ) ) ;
#105980 = CARTESIAN_POINT ( 'NONE',  ( 0.7484295816749999553, 1428.043997280830126, 101.8807690336980016 ) ) ;
#105982 = CARTESIAN_POINT ( 'NONE',  ( 11.89522282729999958, 1434.541161981840105, 151.0452005854980086 ) ) ;
#105983 = CARTESIAN_POINT ( 'NONE',  ( -24.83308109816510267, 1451.807016045359887, 136.9460679876989957 ) ) ;
#105984 = CARTESIAN_POINT ( 'NONE',  ( 9.998927153253520217, 1439.449791891414179, 152.9676570072420247 ) ) ;
#105985 = CARTESIAN_POINT ( 'NONE',  ( 4.324697132450000758, 1409.231835851730011, 230.8572462717979761 ) ) ;
#105986 = CARTESIAN_POINT ( 'NONE',  ( 12.54808185004130117, 1501.100271328960162, 211.1771682979919831 ) ) ;
#105987 = CARTESIAN_POINT ( 'NONE',  ( 4.042729802795000715, 1516.919782530640077, 212.3762473738369749 ) ) ;
#105988 = CARTESIAN_POINT ( 'NONE',  ( 40.66293689370180431, 1439.821779689370032, 134.0999999980979851 ) ) ;
#105989 = DIRECTION ( 'NONE',  ( -0.000000000000000000, -1.000000000000000000, -0.000000000000000000 ) ) ;
#105990 = VERTEX_POINT ( 'NONE', #6204 ) ;
#105991 = CARTESIAN_POINT ( 'NONE',  ( -9.771935530151019123, 1448.872218581839888, 190.8346833224969998 ) ) ;
#105992 = CARTESIAN_POINT ( 'NONE',  ( -4.363122647529283249, 1407.471318475732005, 137.0999999980979851 ) ) ;
#105993 = ORIENTED_EDGE ( 'NONE', *, *, #25444, .T. ) ;
#105994 = ORIENTED_EDGE ( 'NONE', *, *, #108679, .F. ) ;
#105995 = ORIENTED_EDGE ( 'NONE', *, *, #1741, .T. ) ;
#105996 = CARTESIAN_POINT ( 'NONE',  ( -6.563811449735000636, 1514.071098020780028, 216.7756948377870003 ) ) ;
#105997 = CARTESIAN_POINT ( 'NONE',  ( 16.51878312702331186, 1514.214507863231120, 194.7969773782033656 ) ) ;
#105998 = CYLINDRICAL_SURFACE ( 'NONE', #18814, 2.000000000000003553 ) ;
#105999 = CARTESIAN_POINT ( 'NONE',  ( -8.023395094369998759, 1384.908845605290026, 218.7875321875989982 ) ) ;
#106000 = CARTESIAN_POINT ( 'NONE',  ( 9.855320986769999791, 1462.478457361989967, 210.0130851932640041 ) ) ;
#106001 = CARTESIAN_POINT ( 'NONE',  ( -18.42693662763718265, 1445.993580523349237, 214.9599593228655294 ) ) ;
#106002 = CARTESIAN_POINT ( 'NONE',  ( -63.87106590895305658, 1379.736345038605350, 269.9222812701415251 ) ) ;
#106003 = CARTESIAN_POINT ( 'NONE',  ( -0.4967503101659990206, 1463.947305906790007, 199.2992579264090125 ) ) ;
#106004 = CARTESIAN_POINT ( 'NONE',  ( 6.250809056239999606, 1416.216596894529857, 191.9478012161979734 ) ) ;
#106005 = ORIENTED_EDGE ( 'NONE', *, *, #48382, .T. ) ;
#106006 =( BOUNDED_SURFACE ( )  B_SPLINE_SURFACE ( 3, 2, ( 
 ( #56459, #49718, #109073 ),
 ( #65981, #22259, #4934 ),
 ( #39078, #57023, #90593 ),
 ( #41306, #30692, #39651 ) ),
 .UNSPECIFIED., .F., .F., .F. ) 
 B_SPLINE_SURFACE_WITH_KNOTS ( ( 4, 4 ),
 ( 3, 3 ),
 ( 0.000000000000000000, 0.0002960034161023847852 ),
 ( 0.000000000000000000, 1.000000000000000000 ),
 .UNSPECIFIED. ) 
 GEOMETRIC_REPRESENTATION_ITEM ( )  RATIONAL_B_SPLINE_SURFACE ( (
 ( 1.000000000000000000, 0.8070209408750051994, 1.000000000000000000),
 ( 1.000000000000000000, 0.8071723757218238759, 1.000000000000000000),
 ( 1.000000000000000000, 0.8072480346917746408, 1.000000000000000000),
 ( 1.000000000000000000, 0.8072480644198114508, 1.000000000000000000) ) ) 
 REPRESENTATION_ITEM ( '' )  SURFACE ( )  );
#106007 = CARTESIAN_POINT ( 'NONE',  ( -7.726331963605000297, 1517.194972660189933, 206.8303316343270239 ) ) ;
#106008 = ORIENTED_EDGE ( 'NONE', *, *, #91905, .F. ) ;
#106009 = CARTESIAN_POINT ( 'NONE',  ( 32.33557200478939819, 1440.913060387330006, 256.5466809373250499 ) ) ;
#106010 = CARTESIAN_POINT ( 'NONE',  ( -13.92523054340000144, 1509.057792502929715, 183.7758903212979931 ) ) ;
#106011 = ORIENTED_EDGE ( 'NONE', *, *, #49453, .F. ) ;
#106012 = CARTESIAN_POINT ( 'NONE',  ( -0.2694122152484670352, 1452.981480044009913, 183.2530805241289897 ) ) ;
#106013 = CARTESIAN_POINT ( 'NONE',  ( -15.12468517189999950, 1409.607859681430000, 191.4574115868979902 ) ) ;
#106014 = CARTESIAN_POINT ( 'NONE',  ( -17.47298132753811117, 1508.456142919008016, 212.6551300565776899 ) ) ;
#106016 = DIRECTION ( 'NONE',  ( -1.000000000000000000, -2.249639673992789970E-32, -1.224646799147350002E-16 ) ) ;
#106015 = CARTESIAN_POINT ( 'NONE',  ( -24.49695175729999974, 1441.051797180180074, 210.9974392583980034 ) ) ;
#106017 = CARTESIAN_POINT ( 'NONE',  ( -6.052777691587611031, 1434.867522108110052, 216.6696794239180122 ) ) ;
#106018 = CARTESIAN_POINT ( 'NONE',  ( 0.0002641894870882123352, 1396.493308979614994, 196.7136476201564506 ) ) ;
#106019 = CARTESIAN_POINT ( 'NONE',  ( 0.1075625203479999986, 1405.989059426929998, 266.9611530679979978 ) ) ;
#106020 = CARTESIAN_POINT ( 'NONE',  ( -12.40420594909999963, 1434.420026268609945, 148.5638390392980170 ) ) ;
#106021 = CARTESIAN_POINT ( 'NONE',  ( -7.239307611560000133, 1509.020652858989934, 218.9550108994890252 ) ) ;
#106023 = CARTESIAN_POINT ( 'NONE',  ( 18.14949073579999705, 1432.344282874789997, 211.8258969992290019 ) ) ;
#106022 = CARTESIAN_POINT ( 'NONE',  ( 15.68557540059999766, 1410.853897593529837, 191.5168599455980143 ) ) ;
#106024 = CARTESIAN_POINT ( 'NONE',  ( 1.709358663124999955, 1516.542957540330008, 216.0554336257470140 ) ) ;
#106025 = CARTESIAN_POINT ( 'NONE',  ( -3.330134203884999700, 1515.051704408389924, 213.4516374609670208 ) ) ;
#106026 = CARTESIAN_POINT ( 'NONE',  ( 5.912727970548059986, 1510.598356033829987, 216.6556934984580209 ) ) ;
#106027 = CARTESIAN_POINT ( 'NONE',  ( 3.101757698284638209, 1466.831514544163610, 219.0062985612876503 ) ) ;
#106028 = CARTESIAN_POINT ( 'NONE',  ( 5.787476994515000861, 1517.070197312179971, 211.9915394291670054 ) ) ;
#106029 = CARTESIAN_POINT ( 'NONE',  ( -22.00315959520000320, 1506.810797421130019, 209.3571658142759873 ) ) ;
#106030 = CARTESIAN_POINT ( 'NONE',  ( -2.745154014197499937, 1419.769956470485113, 137.0999999980979851 ) ) ;
#106032 = ORIENTED_EDGE ( 'NONE', *, *, #79455, .F. ) ;
#106031 = CARTESIAN_POINT ( 'NONE',  ( -2.218918642439999811, 1431.115532562089811, 203.8893404030790180 ) ) ;
#106033 = CARTESIAN_POINT ( 'NONE',  ( 8.598884471655001249, 1512.314860040240092, 206.8869224911269953 ) ) ;
#106034 = CARTESIAN_POINT ( 'NONE',  ( 30.28727320069999962, 1444.847842080569990, 240.1330978332979669 ) ) ;
#106035 = CARTESIAN_POINT ( 'NONE',  ( -16.78608357809999774, 1458.775951820630098, 230.6691475833980007 ) ) ;
#106036 = CARTESIAN_POINT ( 'NONE',  ( -14.61826233789999918, 1415.850734755279973, 204.4424076310489795 ) ) ;
#106037 = CARTESIAN_POINT ( 'NONE',  ( 1.802538876310000093, 1411.735565077730143, 232.2550115084980007 ) ) ;
#106038 = DIRECTION ( 'NONE',  ( 0.03206272707449610987, 0.004242270441052224499, 0.9994768554969400975 ) ) ;
#106040 = CARTESIAN_POINT ( 'NONE',  ( -17.04532912216366825, 1522.051704408389924, 196.9538555332918293 ) ) ;
#106039 = CARTESIAN_POINT ( 'NONE',  ( -24.66664643669999890, 1470.078893469029936, 215.2854056718580296 ) ) ;
#106041 = CARTESIAN_POINT ( 'NONE',  ( -10.29850490222790071, 1448.590037845560119, 207.7852207394710149 ) ) ;
#106042 = CARTESIAN_POINT ( 'NONE',  ( -105.7945529881810103, 1378.894406107679970, 306.4862516817319715 ) ) ;
#106043 = VERTEX_POINT ( 'NONE', #74536 ) ;
#106044 = CARTESIAN_POINT ( 'NONE',  ( 4.998515157294999511, 1516.787536375099990, 205.0819486540370065 ) ) ;
#106045 = CARTESIAN_POINT ( 'NONE',  ( 2.110729450650000061, 1405.810983166630194, 268.4819085761979522 ) ) ;
#106046 = CARTESIAN_POINT ( 'NONE',  ( 1.118758552039999854, 1515.569725561690120, 213.0929468739089714 ) ) ;
#106047 = CARTESIAN_POINT ( 'NONE',  ( 30.17003485434790022, 1463.451681519390149, 269.4565801611439610 ) ) ;
#106048 = CARTESIAN_POINT ( 'NONE',  ( -0.8391973868109434687, 1463.415940303041452, 199.3702334271763164 ) ) ;
#106049 = CARTESIAN_POINT ( 'NONE',  ( 10.57441464843243750, 1423.877695273033623, 137.4726654012514189 ) ) ;
#106050 = CARTESIAN_POINT ( 'NONE',  ( -9.996566840449769842, 1446.992630724909986, 211.6934593223399759 ) ) ;
#106051 = CARTESIAN_POINT ( 'NONE',  ( -3.220674670777950332, 1433.265635011049881, 218.1214075741529825 ) ) ;
#106052 = CARTESIAN_POINT ( 'NONE',  ( 0.3109538050990010016, 1430.738335933489907, 200.0544679982990033 ) ) ;
#106053 = CARTESIAN_POINT ( 'NONE',  ( -21.41971086555066606, 1511.187213306747708, 233.0798096144383749 ) ) ;
#106054 = CARTESIAN_POINT ( 'NONE',  ( -22.07691437628720266, 1523.843263703804041, 184.4448114610363518 ) ) ;
#106055 = CARTESIAN_POINT ( 'NONE',  ( 14.35058941227343077, 1517.151704408390060, 224.2459111387558437 ) ) ;
#106056 = VERTEX_POINT ( 'NONE', #63940 ) ;
#106057 = CARTESIAN_POINT ( 'NONE',  ( -34.84383443810000358, 1427.856177413630121, 265.6112249940979950 ) ) ;
#106058 = CARTESIAN_POINT ( 'NONE',  ( 11.13982123801030077, 1470.272549761619985, 206.9150573627110248 ) ) ;
#106059 = CARTESIAN_POINT ( 'NONE',  ( -0.7786989082230000303, 1476.104488692030145, 267.8537809120979887 ) ) ;
#106060 = CARTESIAN_POINT ( 'NONE',  ( 10.73171637939167233, 1424.977692942605472, 138.8095723872937413 ) ) ;
#106061 = CARTESIAN_POINT ( 'NONE',  ( -28.04637438780000025, 1508.608407033030062, 210.1642266462579869 ) ) ;
#106062 = CARTESIAN_POINT ( 'NONE',  ( -3.065717400587616215, 1448.273177092793958, 184.5346825199581815 ) ) ;
#106063 = CARTESIAN_POINT ( 'NONE',  ( -40.87587467545650100, 1384.783584316470069, 243.6885206019040027 ) ) ;
#106064 = CARTESIAN_POINT ( 'NONE',  ( 12.15645370196850017, 1491.542819424739946, 207.2681566586209954 ) ) ;
#106065 = CARTESIAN_POINT ( 'NONE',  ( -10.12198797759999991, 1482.055157405490036, 205.4868429776790038 ) ) ;
#106066 = CARTESIAN_POINT ( 'NONE',  ( 26.81253513141949796, 1435.745391332569852, 136.2312305098039928 ) ) ;
#106067 = CARTESIAN_POINT ( 'NONE',  ( -8.906481764856058803, 1396.224081584079840, 215.6780524493100017 ) ) ;
#106068 = CARTESIAN_POINT ( 'NONE',  ( -15.05245933179999973, 1421.043214595429845, 227.1190893059979885 ) ) ;
#106069 = CARTESIAN_POINT ( 'NONE',  ( 19.28951026099334598, 1455.968020544745059, 225.2216972307680010 ) ) ;
#106070 = EDGE_LOOP ( 'NONE', ( #101548, #101417, #105948, #90801, #74604 ) ) ;
#106071 = CARTESIAN_POINT ( 'NONE',  ( -11.40679451554845336, 1501.041746466157065, 208.3891828855351491 ) ) ;
#106072 = CARTESIAN_POINT ( 'NONE',  ( 2.193535739449999689, 1410.364270874430076, 231.8615948999980105 ) ) ;
#106073 = CARTESIAN_POINT ( 'NONE',  ( -5.144873395449999443, 1502.885538352589947, 229.8910404859989853 ) ) ;
#106075 = CARTESIAN_POINT ( 'NONE',  ( -12.18811182046500008, 1511.857118786289902, 193.8586218496669744 ) ) ;
#106074 = CARTESIAN_POINT ( 'NONE',  ( 10.45694972170000092, 1425.379544169830069, 99.60600324669779582 ) ) ;
#106076 = B_SPLINE_CURVE_WITH_KNOTS ( 'NONE', 3,
 ( #37649, #107052, #81287, #105971, #63438, #97556, #79121, #53938, #96458, #30337, #2429, #20830, #55025, #64528, #56105, #90236, #36544, #70742, #28142, #62333, #108147, #14638, #23026, #49358, #75121, #99180, #91358, #48823, #57777, #83487, #30885, #39296, #7344, #58311, #73468, #22460, #5705, #107602, #91895, #66728, #65065, #65620, #32553, #6238, #57228, #56661, #6781, #90795, #15172, #81835, #82947, #40389, #14078, #31437, #48267, #40944, #82412, #39851 ),
 .UNSPECIFIED., .F., .F.,
 ( 4, 3, 3, 3, 3, 3, 3, 3, 3, 3, 3, 3, 3, 3, 3, 3, 3, 3, 3, 4 ),
 ( -71.37784974196719645, -71.16605863430530121, -69.93410874380388975, -68.73248683439000217, -67.54973204371560769, -66.39512066597440310, -65.25685987814000555, -64.13305301190000307, -63.25887383612570147, -62.19532168835289809, -61.12456690189929986, -60.04779693945010166, -58.95843042468590056, -57.85897264479999791, -57.12128301158499966, -55.97157416834189547, -54.78165593109999776, -54.16598274440690375, -52.96632159195399936, -51.70433921739999761 ),
 .UNSPECIFIED. ) ;
#106077 = DIRECTION ( 'NONE',  ( 5.980589973904019347E-17, -1.000000000000000000, 1.736889445713099699E-16 ) ) ;
#106078 = CARTESIAN_POINT ( 'NONE',  ( 4.322220531106200525, 1423.873566462119925, 183.7070391214139988 ) ) ;
#106079 = ADVANCED_FACE ( 'NONE', ( #108667 ), #94609, .T. ) ;
#106080 = CARTESIAN_POINT ( 'NONE',  ( -0.7526715882979990724, 1516.710624944440042, 201.4081970979170251 ) ) ;
#106081 = CARTESIAN_POINT ( 'NONE',  ( 7.490627823309999656, 1426.027613909420097, 212.3458724979089709 ) ) ;
#106082 = CARTESIAN_POINT ( 'NONE',  ( 13.84583145400000070, 1499.900106662689723, 227.7510597354990125 ) ) ;
#106083 = CARTESIAN_POINT ( 'NONE',  ( 1.625726771530000114, 1508.862184707429833, 180.0252976342979991 ) ) ;
#106084 = CARTESIAN_POINT ( 'NONE',  ( 7.774021405044999611, 1512.205735116489905, 206.2993818420169987 ) ) ;
#106085 = CARTESIAN_POINT ( 'NONE',  ( -50.14845714630110507, 1380.010081755269994, 242.5009527263639768 ) ) ;
#106086 = CARTESIAN_POINT ( 'NONE',  ( 7.770954596407177561, 1365.285754389724843, 209.6218459617148824 ) ) ;
#106087 = B_SPLINE_CURVE_WITH_KNOTS ( 'NONE', 3,
 ( #86626, #9920, #69305, #53615, #88294, #95585, #103980, #45766, #44091, #87757, #11039 ),
 .UNSPECIFIED., .F., .F.,
 ( 4, 2, 1, 2, 2, 4 ),
 ( 0.000000000000000000, 0.2499999999997748468, 0.3749999999997812861, 0.4374999999997651878, 0.4999999999997490896, 1.000000000000000000 ),
 .UNSPECIFIED. ) ;
#106089 = EDGE_LOOP ( 'NONE', ( #101243, #37368, #41937, #87969 ) ) ;
#106088 = CARTESIAN_POINT ( 'NONE',  ( 3.313501335607582643, 1397.551704408390151, 215.1871694724064810 ) ) ;
#106090 = ORIENTED_EDGE ( 'NONE', *, *, #51843, .F. ) ;
#106091 = CARTESIAN_POINT ( 'NONE',  ( -14.34064213879999983, 1445.290870928000004, 188.7064315755980033 ) ) ;
#106092 = CARTESIAN_POINT ( 'NONE',  ( -14.27906159650000006, 1409.411696205929957, 191.9865084241980071 ) ) ;
#106093 = CARTESIAN_POINT ( 'NONE',  ( 19.44117294853580091, 1456.941945407359981, 224.4539793896520052 ) ) ;
#106094 = CARTESIAN_POINT ( 'NONE',  ( -8.100204470725000050, 1511.336728379370243, 213.6607147150270123 ) ) ;
#106096 = CARTESIAN_POINT ( 'NONE',  ( -21.50860586580829903, 1505.511036766189818, 209.4816256532819807 ) ) ;
#106095 = CARTESIAN_POINT ( 'NONE',  ( -8.018637776459998534, 1384.752548399070065, 218.7860119703690032 ) ) ;
#106097 = CARTESIAN_POINT ( 'NONE',  ( 4.473648201620000542, 1410.299799965830061, 186.1951180057979798 ) ) ;
#106098 = FILL_AREA_STYLE ('',( #28846 ) ) ;
#106099 = CARTESIAN_POINT ( 'NONE',  ( -39.34713282899999598, 1447.269474492200061, 136.6009879164979850 ) ) ;
#106100 =( LENGTH_UNIT ( ) NAMED_UNIT ( * ) SI_UNIT ( .MILLI., .METRE. ) );
#106101 = CARTESIAN_POINT ( 'NONE',  ( 41.20351939146799936, 1440.849798643580016, 135.3869769205820148 ) ) ;
#106102 = CARTESIAN_POINT ( 'NONE',  ( 3.005276066430516035, 1369.205039411270036, 210.6218459616991936 ) ) ;
#106103 = DIRECTION ( 'NONE',  ( 6.123233995736769734E-17, 1.000000000000000000, 1.124819836996399911E-32 ) ) ;
#106104 = CARTESIAN_POINT ( 'NONE',  ( -2.277971195341919941, 1406.541924822740157, 269.4972091294530401 ) ) ;
#106105 = CARTESIAN_POINT ( 'NONE',  ( 40.70885980849999441, 1444.084951190109905, 137.1037942526980089 ) ) ;
#106106 = EDGE_LOOP ( 'NONE', ( #30755, #92732, #35035, #58865, #58016 ) ) ;
#106107 = CARTESIAN_POINT ( 'NONE',  ( -16.50400130224782558, 1525.907212628473644, 181.9890130758379598 ) ) ;
#106108 = CARTESIAN_POINT ( 'NONE',  ( 12.19742149640000051, 1441.220184892860061, 188.3545874510979843 ) ) ;
#106109 = ORIENTED_EDGE ( 'NONE', *, *, #38482, .T. ) ;
#106110 = ORIENTED_EDGE ( 'NONE', *, *, #100138, .F. ) ;
#106111 = CARTESIAN_POINT ( 'NONE',  ( 19.53786426059039982, 1511.187213306747708, 237.7197124308265188 ) ) ;
#106112 = CARTESIAN_POINT ( 'NONE',  ( -14.63759143169999888, 1461.861471536829868, 229.3720751777979956 ) ) ;
#106113 = CARTESIAN_POINT ( 'NONE',  ( -2.288357445734999995, 1517.116049120239950, 214.9102823043970147 ) ) ;
#106114 = CARTESIAN_POINT ( 'NONE',  ( 4.826478482935000258, 1511.220390575160081, 217.0108025382170069 ) ) ;
#106115 = B_SPLINE_SURFACE_WITH_KNOTS ( 'NONE', 5, 5, ( 
 ( #53870, #53300, #46552, #79600, #36474, #70672 ),
 ( #80687, #44343, #62833, #3998, #26982, #96947 ),
 ( #61171, #95286, #18548, #10170, #78486, #1800 ),
 ( #35937, #95829, #5068, #72305, #81219, #31369 ),
 ( #22390, #90724, #57158, #64995, #13446, #29720 ),
 ( #74505, #30818, #47637, #90165, #82334, #108634 ) ),
 .UNSPECIFIED., .F., .F., .F.,
 ( 6, 6 ),
 ( 6, 6 ),
 ( 10.65476131940000037, 18.78936860560000000 ),
 ( 0.000000000000000000, 0.5000000000000000000 ),
 .UNSPECIFIED. ) ;
#106116 = ORIENTED_EDGE ( 'NONE', *, *, #82253, .F. ) ;
#106117 = CARTESIAN_POINT ( 'NONE',  ( -5.976455546807909691, 1509.218656960890030, 179.5797749763599995 ) ) ;
#106118 = CARTESIAN_POINT ( 'NONE',  ( -87.43041093610000303, 1374.577971548089863, 299.9734862988590294 ) ) ;
#106119 = ADVANCED_FACE ( 'NONE', ( #65026 ), #14950, .T. ) ;
#106120 = EDGE_CURVE ( 'NONE', #53131, #100441, #32501, .T. ) ;
#106121 = ADVANCED_FACE ( 'NONE', ( #66693 ), #93682, .T. ) ;
#106122 = CARTESIAN_POINT ( 'NONE',  ( 2.859824348760000134, 1416.824060884729988, 226.9682156876980059 ) ) ;
#106123 = CARTESIAN_POINT ( 'NONE',  ( -4.622842882315000068, 1516.901952101700090, 205.0913314195169903 ) ) ;
#106124 = CARTESIAN_POINT ( 'NONE',  ( -12.18560036526529977, 1490.059793347699951, 210.2795501257769786 ) ) ;
#106125 = EDGE_CURVE ( 'NONE', #79128, #103755, #20117, .T. ) ;
#106127 = EDGE_CURVE ( 'NONE', #80584, #83258, #69898, .T. ) ;
#106126 = CARTESIAN_POINT ( 'NONE',  ( -109.9987473190000031, 1385.017600419090058, 297.1692069989590550 ) ) ;
#106128 = CARTESIAN_POINT ( 'NONE',  ( -2.947857299329999847, 1409.016001832629854, 231.5025266905979890 ) ) ;
#106130 = ORIENTED_EDGE ( 'NONE', *, *, #94794, .F. ) ;
#106129 = CARTESIAN_POINT ( 'NONE',  ( -29.86461515634926656, 1525.960063244517187, 197.2746849027940925 ) ) ;
#106131 = CARTESIAN_POINT ( 'NONE',  ( -14.53515913103558610, 1435.864451241055349, 149.7571230983877228 ) ) ;
#106132 = CARTESIAN_POINT ( 'NONE',  ( -26.65848496185190086, 1440.913060438550019, 225.2196237981240188 ) ) ;
#106133 = CARTESIAN_POINT ( 'NONE',  ( 20.21023357682329546, 1526.107880201381477, 233.6897414230651293 ) ) ;
#106134 = CARTESIAN_POINT ( 'NONE',  ( 18.51068734469999910, 1475.362681785890118, 218.3399159096489939 ) ) ;
#106135 = CARTESIAN_POINT ( 'NONE',  ( 39.15206306312100537, 1428.692637880929851, 269.5910580954339935 ) ) ;
#106136 = CARTESIAN_POINT ( 'NONE',  ( 2.878693249144999466, 1516.766397346390022, 213.1495431961470217 ) ) ;
#106137 = CARTESIAN_POINT ( 'NONE',  ( -67.47186131060000491, 1379.745269727820187, 277.3594581318590144 ) ) ;
#106138 = CARTESIAN_POINT ( 'NONE',  ( 23.81949531699999767, 1410.711204269130121, 208.1966712349829720 ) ) ;
#106139 = CARTESIAN_POINT ( 'NONE',  ( 0.01313586619463304531, 1507.980182440329145, 237.5914718841819990 ) ) ;
#106140 = CARTESIAN_POINT ( 'NONE',  ( 14.99555783611850046, 1427.394895963429917, 198.9768735146830068 ) ) ;
#106141 = CARTESIAN_POINT ( 'NONE',  ( -18.80013642706989785, 1505.319320522869930, 222.5373253066319990 ) ) ;
#106142 = CARTESIAN_POINT ( 'NONE',  ( -1.122033430074999893, 1516.972341476009888, 209.8777854684929878 ) ) ;
#106143 = ORIENTED_EDGE ( 'NONE', *, *, #84265, .F. ) ;
#106144 = CARTESIAN_POINT ( 'NONE',  ( 4.179007317879920080, 1421.587745001310168, 184.8346002776440002 ) ) ;
#106146 = EDGE_CURVE ( 'NONE', #85181, #27055, #40870, .T. ) ;
#106145 = CARTESIAN_POINT ( 'NONE',  ( -0.4639000096230000425, 1415.383732484729990, 233.3963766452980053 ) ) ;
#106147 = CARTESIAN_POINT ( 'NONE',  ( -109.9987472809999929, 1384.694936393889975, 311.2694678342589896 ) ) ;
#106148 = ORIENTED_EDGE ( 'NONE', *, *, #23577, .T. ) ;
#106149 = CARTESIAN_POINT ( 'NONE',  ( -20.12001630530539842, 1385.275803444980056, 220.9734419276739743 ) ) ;
#106150 = CARTESIAN_POINT ( 'NONE',  ( -2.634252018550000241, 1429.123518628689908, 200.1269094519890075 ) ) ;
#106151 = EDGE_CURVE ( 'NONE', #52007, #66425, #53768, .T. ) ;
#106152 = CARTESIAN_POINT ( 'NONE',  ( -20.60174636844089946, 1508.366643450050105, 228.3235642671120047 ) ) ;
#106153 = CARTESIAN_POINT ( 'NONE',  ( -3.562576982599999997, 1500.604443063090002, 230.1476615162989958 ) ) ;
#106154 = EDGE_CURVE ( 'NONE', #74686, #33810, #83152, .T. ) ;
#106155 = CARTESIAN_POINT ( 'NONE',  ( 20.21728935790000037, 1475.862786327189951, 209.1218459616989946 ) ) ;
#106156 = CARTESIAN_POINT ( 'NONE',  ( 0.1236923762493960105, 1420.459419726229953, 182.7104392795739898 ) ) ;
#106157 = AXIS2_PLACEMENT_3D ( 'NONE', #56006, #100731, #90130 ) ;
#106159 = CARTESIAN_POINT ( 'NONE',  ( -16.43661047864564040, 1416.852979121301360, 207.9780681923153338 ) ) ;
#106158 = CARTESIAN_POINT ( 'NONE',  ( 1.709358663124999955, 1516.542957540330008, 216.0554336257470140 ) ) ;
#106160 = CARTESIAN_POINT ( 'NONE',  ( 19.28053483500000098, 1508.539880148729935, 188.4639099547979981 ) ) ;
#106161 = CARTESIAN_POINT ( 'NONE',  ( 9.923128685616420697, 1469.055232010309965, 207.6288126312279871 ) ) ;
#106162 = ORIENTED_EDGE ( 'NONE', *, *, #9658, .T. ) ;
#106163 = CARTESIAN_POINT ( 'NONE',  ( 1.709384572955000126, 1517.224900789629828, 201.7820965968870155 ) ) ;
#106164 = CARTESIAN_POINT ( 'NONE',  ( 10.40804279477580074, 1480.934692010039953, 207.3742714289850255 ) ) ;
#106165 = EDGE_LOOP ( 'NONE', ( #23455, #101203, #53272, #104006, #108228, #5319, #96257, #8130 ) ) ;
#106166 = CARTESIAN_POINT ( 'NONE',  ( 11.60004869885205459, 1426.637431749262760, 134.7518136753569706 ) ) ;
#106167 = CARTESIAN_POINT ( 'NONE',  ( 10.36367428452916428, 1435.180720288839666, 152.2397717789484375 ) ) ;
#106168 = CARTESIAN_POINT ( 'NONE',  ( 8.179170872261016356, 1424.126445343982823, 195.8532290842973680 ) ) ;
#106169 = CARTESIAN_POINT ( 'NONE',  ( -0.5923098205000010275, 1443.101676972689802, 218.7159598536189833 ) ) ;
#106170 = CARTESIAN_POINT ( 'NONE',  ( -27.48965073337759790, 1509.741665821160041, 201.0942380509760028 ) ) ;
#106171 = CARTESIAN_POINT ( 'NONE',  ( -3.133278228710000501, 1446.922685362290167, 159.4827083638979843 ) ) ;
#106172 = CARTESIAN_POINT ( 'NONE',  ( -18.48615752410000113, 1425.307041905530014, 226.5289461057980134 ) ) ;
#106173 = CARTESIAN_POINT ( 'NONE',  ( -15.20520707470000232, 1435.028465714059848, 147.6080287230979877 ) ) ;
#106174 = CARTESIAN_POINT ( 'NONE',  ( -19.58905257500000019, 1465.550414696789858, 206.2240342260589898 ) ) ;
#106175 = CARTESIAN_POINT ( 'NONE',  ( 17.92485922270000032, 1509.539010264429862, 186.7667139844979829 ) ) ;
#106177 = CARTESIAN_POINT ( 'NONE',  ( -17.28825620729984536, 1433.649598815182799, 216.8113180210153246 ) ) ;
#106176 = CARTESIAN_POINT ( 'NONE',  ( 7.407046107680000269, 1488.581653516390134, 199.5623810922690211 ) ) ;
#106178 = CARTESIAN_POINT ( 'NONE',  ( 2.383407846124329765, 1522.906363951597314, 243.2919566057095153 ) ) ;
#106179 = ORIENTED_EDGE ( 'NONE', *, *, #106886, .F. ) ;
#106180 = CARTESIAN_POINT ( 'NONE',  ( -9.103468112560660686, 1449.499701819690017, 210.3008494512589834 ) ) ;
#106181 = CARTESIAN_POINT ( 'NONE',  ( 14.49568591477500057, 1514.921196705999819, 224.3246435558060057 ) ) ;
#106182 = CARTESIAN_POINT ( 'NONE',  ( 3.827327165375219664, 1424.046157828239984, 183.3886487722830054 ) ) ;
#106183 = CARTESIAN_POINT ( 'NONE',  ( 11.24351695115020000, 1470.448214870340053, 207.4320293865459917 ) ) ;
#106184 = CARTESIAN_POINT ( 'NONE',  ( -2.812370349340000519, 1484.074845783890169, 198.7990170648990045 ) ) ;
#106185 = CARTESIAN_POINT ( 'NONE',  ( -15.77133272873888714, 1418.153095964348040, 203.3734822495675019 ) ) ;
#106186 = CARTESIAN_POINT ( 'NONE',  ( -2.966648571466143025, 1425.987482934672926, 185.4283574743214444 ) ) ;
#106187 = CARTESIAN_POINT ( 'NONE',  ( 15.53391875520000021, 1431.113060387329824, 219.7242127505980136 ) ) ;
#106188 = CARTESIAN_POINT ( 'NONE',  ( 26.81573205290009554, 1435.593033338389205, 136.1631037710002943 ) ) ;
#106189 = CARTESIAN_POINT ( 'NONE',  ( 5.063479484552349419, 1494.517360836430043, 219.5241837424580353 ) ) ;
#106190 = CARTESIAN_POINT ( 'NONE',  ( -10.25580389252270130, 1489.562374261269724, 214.0502075833479978 ) ) ;
#106191 = CARTESIAN_POINT ( 'NONE',  ( -20.43379408400000230, 1466.940146741789931, 211.2182734472289951 ) ) ;
#106192 = CARTESIAN_POINT ( 'NONE',  ( -90.89540613257170776, 1383.769753454369948, 308.8054560215319952 ) ) ;
#106193 = CARTESIAN_POINT ( 'NONE',  ( -109.9358763820779927, 1384.187282608590067, 311.4119166190040460 ) ) ;
#106194 = CARTESIAN_POINT ( 'NONE',  ( 6.200611228269999664, 1427.799628982990043, 214.6497469830689795 ) ) ;
#106196 = VERTEX_POINT ( 'NONE', #27974 ) ;
#106195 = CARTESIAN_POINT ( 'NONE',  ( 1.026847439679999807, 1494.050500615490137, 217.3813169612789977 ) ) ;
#106197 = CARTESIAN_POINT ( 'NONE',  ( -97.71463903750000668, 1379.367587121119868, 302.5561533006589912 ) ) ;
#106198 = CARTESIAN_POINT ( 'NONE',  ( -0.4770279523499595942, 1415.729984941675639, 233.4079075601304964 ) ) ;
#106199 = ORIENTED_EDGE ( 'NONE', *, *, #83387, .T. ) ;
#106200 = ORIENTED_EDGE ( 'NONE', *, *, #56503, .T. ) ;
#106201 = CARTESIAN_POINT ( 'NONE',  ( 17.36791971707869919, 1414.972329067380088, 210.3611080999600063 ) ) ;
#106202 = CARTESIAN_POINT ( 'NONE',  ( -109.8947400899999991, 1384.917309675210163, 297.0284544140590128 ) ) ;
#106203 = CARTESIAN_POINT ( 'NONE',  ( 13.51610093808349333, 1443.885067043062236, 169.3501091255430140 ) ) ;
#106205 = CARTESIAN_POINT ( 'NONE',  ( -10.82132306919999998, 1467.865346123229983, 250.5360043744979635 ) ) ;
#106204 = CARTESIAN_POINT ( 'NONE',  ( 41.03828203346069614, 1434.252829246168858, 269.6293022805288615 ) ) ;
#106206 = CARTESIAN_POINT ( 'NONE',  ( 9.273082254300890170, 1436.468110177680273, 210.7387439683169816 ) ) ;
#106207 = CARTESIAN_POINT ( 'NONE',  ( -11.88086828319999988, 1433.529714312930082, 150.4967080263980108 ) ) ;
#106208 = EDGE_CURVE ( 'NONE', #103319, #59275, #64363, .T. ) ;
#106209 = CARTESIAN_POINT ( 'NONE',  ( -23.59335433706185015, 1519.551704408389924, 209.8811657366039185 ) ) ;
#106210 = CARTESIAN_POINT ( 'NONE',  ( -19.36887732249999772, 1485.900336442130083, 189.8252615598980242 ) ) ;
#106211 = CARTESIAN_POINT ( 'NONE',  ( 7.147354835452560451, 1466.396680852790041, 215.9969464199629954 ) ) ;
#106212 = CARTESIAN_POINT ( 'NONE',  ( 13.04207579039999843, 1409.368499709730031, 192.3005086496980027 ) ) ;
#106213 = EDGE_CURVE ( 'NONE', #29227, #108746, #28539, .T. ) ;
#106214 = CARTESIAN_POINT ( 'NONE',  ( 5.609660757850000401, 1424.149675858230012, 185.9623400711979855 ) ) ;
#106215 = CARTESIAN_POINT ( 'NONE',  ( 1.351910739691850161, 1515.082829241050149, 213.4508224384909738 ) ) ;
#106216 = CARTESIAN_POINT ( 'NONE',  ( 7.981991770210000503, 1441.362204039569860, 154.1152756057979900 ) ) ;
#106217 = CARTESIAN_POINT ( 'NONE',  ( -9.137858907971150302, 1479.061965924570131, 216.3904244229409812 ) ) ;
#106218 = CARTESIAN_POINT ( 'NONE',  ( 34.09113935470853818, 1523.429859730330008, 198.4929744671651974 ) ) ;
#106220 = VERTEX_POINT ( 'NONE', #55947 ) ;
#106219 = CARTESIAN_POINT ( 'NONE',  ( -1.213043055954409927E-09, 1413.218559050369777, 250.1013962713409740 ) ) ;
#106221 = ORIENTED_EDGE ( 'NONE', *, *, #20821, .T. ) ;
#106222 = CARTESIAN_POINT ( 'NONE',  ( -11.86472222573770097, 1432.239683487029879, 149.9815285707079795 ) ) ;
#106223 = CARTESIAN_POINT ( 'NONE',  ( -17.72465096253550243, 1488.214251129269996, 195.0958863970620030 ) ) ;
#106224 = CARTESIAN_POINT ( 'NONE',  ( -15.21920960299999948, 1471.332176259930065, 270.4035064524979930 ) ) ;
#106225 = DIRECTION ( 'NONE',  ( 0.9846671174924281900, -0.1149361401860498344, -0.1312263365650570279 ) ) ;
#106226 = CARTESIAN_POINT ( 'NONE',  ( -104.3512419375385036, 1378.528619065190242, 309.1652050167673451 ) ) ;
#106227 = DIRECTION ( 'NONE',  ( 1.224646799147350002E-16, -1.836970198721029688E-16, -1.000000000000000000 ) ) ;
#106228 = EDGE_CURVE ( 'NONE', #47709, #35907, #59004, .T. ) ;
#106229 = CARTESIAN_POINT ( 'NONE',  ( 0.2546547860042029932, 1451.330736227379930, 182.4946635726779789 ) ) ;
#106230 = CARTESIAN_POINT ( 'NONE',  ( -13.12457881600000142, 1420.616264208729945, 228.4003993496980058 ) ) ;
#106231 = CARTESIAN_POINT ( 'NONE',  ( -30.04349656869200302, 1524.760046179776054, 222.3147819414557489 ) ) ;
#106232 = CARTESIAN_POINT ( 'NONE',  ( -1.243940167669593144, 1484.627497658113271, 182.2780586529670757 ) ) ;
#106233 = CARTESIAN_POINT ( 'NONE',  ( 8.863526962015209065, 1360.372185508180110, 209.6218459617033432 ) ) ;
#106234 = CARTESIAN_POINT ( 'NONE',  ( -45.58440001455219459, 1437.147777294319894, 268.7645413928499920 ) ) ;
#106235 = ORIENTED_EDGE ( 'NONE', *, *, #8949, .F. ) ;
#106236 = CARTESIAN_POINT ( 'NONE',  ( -3.540559338901060116, 1498.522212189139964, 181.3435358006369995 ) ) ;
#106237 = VECTOR ( 'NONE', #5179, 1000.000000000000000 ) ;
#106238 = ORIENTED_EDGE ( 'NONE', *, *, #59039, .F. ) ;
#106239 = VERTEX_POINT ( 'NONE', #99567 ) ;
#106240 = CARTESIAN_POINT ( 'NONE',  ( 5.013274961385000061, 1517.068517094990057, 211.4089302402969963 ) ) ;
#106241 = CARTESIAN_POINT ( 'NONE',  ( -9.413255646274679478, 1447.050163675619842, 212.1529317657590070 ) ) ;
#106242 = CARTESIAN_POINT ( 'NONE',  ( -22.52609270580000000, 1509.699688878229836, 190.3721637121980166 ) ) ;
#106243 = CARTESIAN_POINT ( 'NONE',  ( -9.065232144620001264, 1410.393916203129947, 188.0587484761979908 ) ) ;
#106244 = CIRCLE ( 'NONE', #52545, 2.000000000000004441 ) ;
#106245 = CARTESIAN_POINT ( 'NONE',  ( 2.500020115319840031, 1419.382923540379807, 144.1035841389490031 ) ) ;
#106246 = B_SPLINE_SURFACE_WITH_KNOTS ( 'NONE', 5, 5, ( 
 ( #7682, #6588, #24466, #8771, #33417, #84395 ),
 ( #67065, #41839, #93881, #85473, #23913, #32345 ),
 ( #25015, #67613, #42953, #75994, #101171, #15511 ),
 ( #101725, #77113, #16063, #74912, #58108, #51339 ),
 ( #58655, #32876, #110144, #420, #8220, #50266 ),
 ( #68179, #68722, #26119, #50796, #59216, #42386 ) ),
 .UNSPECIFIED., .F., .F., .F.,
 ( 6, 6 ),
 ( 6, 6 ),
 ( 28.60746992390000187, 29.16358567150000169 ),
 ( 106.3256099500000005, 116.2484248749999978 ),
 .UNSPECIFIED. ) ;
#106247 = ORIENTED_EDGE ( 'NONE', *, *, #106934, .F. ) ;
#106248 = EDGE_CURVE ( 'NONE', #47608, #103079, #75232, .T. ) ;
#106249 = EDGE_CURVE ( 'NONE', #21883, #91721, #16036, .T. ) ;
#106250 = CARTESIAN_POINT ( 'NONE',  ( -3.260378293205000055, 1516.582197289609894, 201.4115600944169842 ) ) ;
#106251 = CARTESIAN_POINT ( 'NONE',  ( 18.47399034927997974, 1509.320896583164085, 187.7622940969008027 ) ) ;
#106252 = CARTESIAN_POINT ( 'NONE',  ( -24.94190653805079805, 1384.544460101560162, 203.2666405366809954 ) ) ;
#106253 = ORIENTED_EDGE ( 'NONE', *, *, #38968, .T. ) ;
#106254 = CARTESIAN_POINT ( 'NONE',  ( -28.62992350010170028, 1415.197349097820052, 269.9536374735400273 ) ) ;
#106255 = CARTESIAN_POINT ( 'NONE',  ( 2.882077220935269857, 1416.276656370609999, 231.8998151304730015 ) ) ;
#106256 = CARTESIAN_POINT ( 'NONE',  ( -33.91369114349999592, 1451.728768196330066, 134.7155300131979914 ) ) ;
#106258 = EDGE_LOOP ( 'NONE', ( #75904, #49888, #46508, #3527 ) ) ;
#106257 = CARTESIAN_POINT ( 'NONE',  ( -8.121924544136929214, 1364.961891190665483, 208.3718459617061285 ) ) ;
#106259 = EDGE_LOOP ( 'NONE', ( #15469, #52292, #103420, #92878 ) ) ;
#106260 = CARTESIAN_POINT ( 'NONE',  ( 45.53497092200698404, 1443.217213248229655, 268.9775536060090531 ) ) ;
#106261 = EDGE_CURVE ( 'NONE', #52986, #42748, #106334, .T. ) ;
#106262 = CARTESIAN_POINT ( 'NONE',  ( 11.32255167084790060, 1471.391268690820198, 210.6326086776350053 ) ) ;
#106263 = CARTESIAN_POINT ( 'NONE',  ( -13.80240444773970054, 1436.220381468010146, 150.3462313445339760 ) ) ;
#106264 = CARTESIAN_POINT ( 'NONE',  ( -1.808737601750000090, 1485.212291732630092, 182.6011977753979920 ) ) ;
#106265 = EDGE_CURVE ( 'NONE', #63893, #20461, #78657, .T. ) ;
#106266 = CARTESIAN_POINT ( 'NONE',  ( -3.750000000000000000, 1512.051704408390151, 209.1218459616989946 ) ) ;
#106267 = CARTESIAN_POINT ( 'NONE',  ( -20.59277739099999849, 1435.768631358810126, 222.2025041439979987 ) ) ;
#106268 = CARTESIAN_POINT ( 'NONE',  ( -14.21664609989999839, 1423.493515736829977, 222.0584263151980053 ) ) ;
#106269 = CARTESIAN_POINT ( 'NONE',  ( -0.7357022321859555403, 1467.091276340035392, 235.5366063015856923 ) ) ;
#106270 = CARTESIAN_POINT ( 'NONE',  ( 5.965627396590000409, 1445.982822326609949, 182.9131883685979858 ) ) ;
#106271 = CARTESIAN_POINT ( 'NONE',  ( 1.701027822874999984, 1516.937508036699910, 206.6270879340970055 ) ) ;
#106272 = VERTEX_POINT ( 'NONE', #63804 ) ;
#106273 = CARTESIAN_POINT ( 'NONE',  ( -33.91369104892859809, 1435.681798505350116, 135.6928025923940027 ) ) ;
#106274 = CARTESIAN_POINT ( 'NONE',  ( -20.98707344033122979, 1454.832818946160842, 223.2596928627122281 ) ) ;
#106275 = ORIENTED_EDGE ( 'NONE', *, *, #42966, .F. ) ;
#106276 = CARTESIAN_POINT ( 'NONE',  ( 0.7162863658319988946, 1429.709265593189912, 217.4063670190490143 ) ) ;
#106277 = CARTESIAN_POINT ( 'NONE',  ( 24.88920569565430085, 1451.596982390830135, 137.4451123274170072 ) ) ;
#106278 = DIRECTION ( 'NONE',  ( 0.5877852522924673639, 0.000000000000000000, -0.8090169943749514481 ) ) ;
#106279 = CARTESIAN_POINT ( 'NONE',  ( -9.122696901847419326, 1384.513827595119892, 199.9705375801759999 ) ) ;
#106280 = CARTESIAN_POINT ( 'NONE',  ( 19.26695685190000162, 1409.750441825429789, 197.0538186098980020 ) ) ;
#106281 = CARTESIAN_POINT ( 'NONE',  ( 21.54410709489999931, 1409.665397185129905, 207.6797030671280027 ) ) ;
#106282 = CARTESIAN_POINT ( 'NONE',  ( 7.150360480941603036, 1512.239113741272149, 216.2200089361317339 ) ) ;
#106283 = CARTESIAN_POINT ( 'NONE',  ( -14.08191331708516358, 1379.630701899112864, 211.6533031874265873 ) ) ;
#106284 = EDGE_CURVE ( 'NONE', #55990, #15017, #68618, .T. ) ;
#106285 = CARTESIAN_POINT ( 'NONE',  ( 0.5266315203254070543, 1450.894659745209992, 181.6127199232379894 ) ) ;
#106286 = CARTESIAN_POINT ( 'NONE',  ( 2.500000000000000000, 1439.621710183279902, 168.1588810856449925 ) ) ;
#106287 = CARTESIAN_POINT ( 'NONE',  ( -6.937965698444999774, 1516.732530461250008, 214.1275461716370216 ) ) ;
#106288 = ADVANCED_FACE ( 'NONE', ( #48092 ), #49874, .T. ) ;
#106289 = ORIENTED_EDGE ( 'NONE', *, *, #28798, .T. ) ;
#106290 = CARTESIAN_POINT ( 'NONE',  ( 7.714278200979600264, 1516.734659492849914, 208.4225296901069839 ) ) ;
#106291 = LINE ( 'NONE', #31232, #30197 ) ;
#106292 = CARTESIAN_POINT ( 'NONE',  ( -2.696156926760000072, 1448.260832249920213, 184.2611194951979883 ) ) ;
#106293 = B_SPLINE_CURVE_WITH_KNOTS ( 'NONE', 5,
 ( #25577, #77663, #9356, #50806, #69282, #92800, #86060, #76550, #975, #43520, #17716, #42964 ),
 .UNSPECIFIED., .F., .F.,
 ( 6, 3, 3, 6 ),
 ( 0.000000000000000000, 0.3787668335507043960, 0.7575336671025384438, 1.000000000000000000 ),
 .UNSPECIFIED. ) ;
#106294 = B_SPLINE_CURVE_WITH_KNOTS ( 'NONE', 3,
 ( #63774, #30695, #46973, #80561, #71087, #3876, #105772, #81095, #97890, #98988 ),
 .UNSPECIFIED., .F., .F.,
 ( 4, 2, 2, 2, 4 ),
 ( 0.000000000000000000, 0.0007189769279725866536, 0.001437953855945173307, 0.002156930783917760178, 0.002875907711890346614 ),
 .UNSPECIFIED. ) ;
#106295 = FACE_OUTER_BOUND ( 'NONE', #94051, .T. ) ;
#106296 =( BOUNDED_CURVE ( )  B_SPLINE_CURVE ( 3, ( #6351, #15279, #68485, #60084 ),
 .UNSPECIFIED., .F., .T. ) 
 B_SPLINE_CURVE_WITH_KNOTS ( ( 4, 4 ),
 ( 2.498705433189824632, 2.510790977241040167 ),
 .UNSPECIFIED. ) 
 CURVE ( )  GEOMETRIC_REPRESENTATION_ITEM ( )  RATIONAL_B_SPLINE_CURVE ( ( 1.000000000000000000, 0.9999878283391195888, 0.9999878283391195888, 1.000000000000000000 ) ) 
 REPRESENTATION_ITEM ( '' )  );
#106297 = CARTESIAN_POINT ( 'NONE',  ( -39.20581607928339452, 1447.436852605690092, 136.5770680602419986 ) ) ;
#106298 = DIRECTION ( 'NONE',  ( 0.000000000000000000, 1.000000000000000000, 0.000000000000000000 ) ) ;
#106299 = CARTESIAN_POINT ( 'NONE',  ( -22.03465957474591619, 1512.187213306747481, 182.8300405912331144 ) ) ;
#106300 = CARTESIAN_POINT ( 'NONE',  ( 17.83740504339754551, 1423.668137810906956, 225.9714325268276696 ) ) ;
#106301 = CARTESIAN_POINT ( 'NONE',  ( 11.21649392120000144, 1433.156491609380282, 151.5728939339980172 ) ) ;
#106302 = CARTESIAN_POINT ( 'NONE',  ( -43.35454757139999771, 1452.005318730930185, 269.0376331129979803 ) ) ;
#106303 = CARTESIAN_POINT ( 'NONE',  ( 31.53547013313849590, 1440.913060383619950, 242.8798340245609779 ) ) ;
#106304 = CYLINDRICAL_SURFACE ( 'NONE', #19765, 0.4999999999999909517 ) ;
#106305 = CARTESIAN_POINT ( 'NONE',  ( 10.52399048938390003, 1498.970143501030179, 202.0357175427869834 ) ) ;
#106306 = VERTEX_POINT ( 'NONE', #74959 ) ;
#106307 = CIRCLE ( 'NONE', #2676, 1.000000000000000888 ) ;
#106308 = CARTESIAN_POINT ( 'NONE',  ( 12.37499353609999986, 1445.063428794549964, 206.9242620747189960 ) ) ;
#106309 = CARTESIAN_POINT ( 'NONE',  ( -19.40696031517546771, 1485.597849508721538, 189.9130132395831367 ) ) ;
#106310 = CARTESIAN_POINT ( 'NONE',  ( -1.912903644472999432, 1526.104292489133059, 240.8844628569841575 ) ) ;
#106311 = CARTESIAN_POINT ( 'NONE',  ( 11.96299724475220039, 1501.580462394789947, 211.5588274086130127 ) ) ;
#106312 = AXIS2_PLACEMENT_3D ( 'NONE', #38801, #88682, #79732 ) ;
#106313 = AXIS2_PLACEMENT_3D ( 'NONE', #39287, #21902, #64519 ) ;
#106314 = CARTESIAN_POINT ( 'NONE',  ( -5.013435694540000043, 1375.426148861440197, 214.7180213005390215 ) ) ;
#106315 = CARTESIAN_POINT ( 'NONE',  ( -16.10723672499999992, 1509.418792458129928, 232.5337701105979988 ) ) ;
#106316 = CARTESIAN_POINT ( 'NONE',  ( -28.27275148466259935, 1383.844209727440102, 226.1197677515999942 ) ) ;
#106317 = CARTESIAN_POINT ( 'NONE',  ( -2.487923244941209866, 1508.731373123109961, 204.5668975639180189 ) ) ;
#106318 = CARTESIAN_POINT ( 'NONE',  ( 9.515252399970000496, 1407.295241224529946, 218.7370609393180132 ) ) ;
#106319 = B_SPLINE_CURVE_WITH_KNOTS ( 'NONE', 3,
 ( #42720, #17476, #9112, #7453, #25332, #101487, #42164, #24774 ),
 .UNSPECIFIED., .F., .F.,
 ( 4, 2, 2, 4 ),
 ( 0.000000000000000000, 0.5000000000000000000, 0.7500000000000000000, 1.000000000000000000 ),
 .UNSPECIFIED. ) ;
#106320 = CARTESIAN_POINT ( 'NONE',  ( 173.8335085727406693, 1526.382868172863937, 317.3879012941853830 ) ) ;
#106321 = CARTESIAN_POINT ( 'NONE',  ( 1.484869686569999958, 1466.691734608930119, 234.9721188785979962 ) ) ;
#106323 = EDGE_LOOP ( 'NONE', ( #93030, #70302 ) ) ;
#106322 = CARTESIAN_POINT ( 'NONE',  ( -4.840660725190000235, 1489.193457555089935, 188.8938074394989997 ) ) ;
#106324 = CARTESIAN_POINT ( 'NONE',  ( -1.453301145269999983, 1450.656428793419991, 182.0378587995979842 ) ) ;
#106325 = B_SPLINE_CURVE_WITH_KNOTS ( 'NONE', 5,
 ( #13583, #47769, #39362, #107672, #22522, #30957 ),
 .UNSPECIFIED., .F., .F.,
 ( 6, 6 ),
 ( 0.000000000000000000, 1.000000000000000000 ),
 .UNSPECIFIED. ) ;
#106326 = CARTESIAN_POINT ( 'NONE',  ( -30.57150941279999756, 1379.881520546990032, 222.4328286988589980 ) ) ;
#106327 = CARTESIAN_POINT ( 'NONE',  ( -3.072929113039999827, 1475.870006633390176, 199.1238679828490206 ) ) ;
#106329 = ORIENTED_EDGE ( 'NONE', *, *, #94114, .T. ) ;
#106328 = CARTESIAN_POINT ( 'NONE',  ( -31.30542570072097064, 1525.651285554137075, 216.2805821473968422 ) ) ;
#106330 = CARTESIAN_POINT ( 'NONE',  ( 20.75864866223560057, 1455.056248125270031, 207.3304711268599760 ) ) ;
#106331 = ORIENTED_EDGE ( 'NONE', *, *, #36043, .T. ) ;
#106332 = CARTESIAN_POINT ( 'NONE',  ( -9.567963333730000741, 1388.728411291870088, 217.1955492302289770 ) ) ;
#106333 = CARTESIAN_POINT ( 'NONE',  ( -4.848919996459999382, 1489.192135936889827, 188.8958457811990002 ) ) ;
#106334 = LINE ( 'NONE', #29620, #89444 ) ;
#106335 = EDGE_CURVE ( 'NONE', #27879, #53764, #103275, .T. ) ;
#106336 = CARTESIAN_POINT ( 'NONE',  ( 4.025649270539999769, 1466.171376325889923, 219.4115622680990043 ) ) ;
#106337 = CARTESIAN_POINT ( 'NONE',  ( 20.29125555118498525, 1509.661241771571213, 187.4025316824865968 ) ) ;
#106338 = CARTESIAN_POINT ( 'NONE',  ( 14.88243897759089940, 1409.432766608349993, 207.8795444941929986 ) ) ;
#106339 = DIRECTION ( 'NONE',  ( -2.275957200481568541E-15, -0.7071067811865475727, -0.7071067811865475727 ) ) ;
#106340 = CARTESIAN_POINT ( 'NONE',  ( -90.92127573589050371, 1385.195597713360030, 293.1101517920880042 ) ) ;
#106341 = CARTESIAN_POINT ( 'NONE',  ( -19.68344085950000277, 1478.176749358629877, 191.0788175296980000 ) ) ;
#106342 = CARTESIAN_POINT ( 'NONE',  ( -68.74147317429999759, 1379.748081684489989, 280.1371050876589948 ) ) ;
#106343 = CARTESIAN_POINT ( 'NONE',  ( 11.46179980149750044, 1491.526194067609822, 208.8062879593289836 ) ) ;
#106344 = VERTEX_POINT ( 'NONE', #77159 ) ;
#106345 = ORIENTED_EDGE ( 'NONE', *, *, #81894, .T. ) ;
#106346 = VECTOR ( 'NONE', #76493, 1000.000000000000114 ) ;
#106348 = CIRCLE ( 'NONE', #58090, 30.13701971169416183 ) ;
#106347 = CARTESIAN_POINT ( 'NONE',  ( -12.23023785423269949, 1416.449138231070037, 194.7027724284880037 ) ) ;
#106349 = CARTESIAN_POINT ( 'NONE',  ( 2.041914512376249657, 1497.024681018629963, 196.8943108031110114 ) ) ;
#106350 = EDGE_CURVE ( 'NONE', #104484, #83093, #95253, .T. ) ;
#106351 = CARTESIAN_POINT ( 'NONE',  ( -5.185116111308140457E-10, 1466.995839566859786, 244.9882531609609941 ) ) ;
#106352 = CARTESIAN_POINT ( 'NONE',  ( -20.12529541769230335, 1492.488775349680054, 190.8351265624610278 ) ) ;
#106353 = CARTESIAN_POINT ( 'NONE',  ( 4.606757942329999800, 1396.134574633329976, 219.8862302532979811 ) ) ;
#106354 = CARTESIAN_POINT ( 'NONE',  ( 21.33942550552290029, 1477.920013592180112, 209.7103284805230032 ) ) ;
#106355 = CARTESIAN_POINT ( 'NONE',  ( -1.183503983870000109, 1453.587766892330137, 183.5423389305979924 ) ) ;
#106356 = CARTESIAN_POINT ( 'NONE',  ( -9.657355732011760452, 1366.083296228048084, 210.6218459616991936 ) ) ;
#106357 = CARTESIAN_POINT ( 'NONE',  ( -26.30168575793273433, 1436.707617520661415, 136.8511971899106925 ) ) ;
#106358 = EDGE_CURVE ( 'NONE', #7780, #40166, #50133, .T. ) ;
#106359 = CARTESIAN_POINT ( 'NONE',  ( 1.715743480078970019E-15, 1374.913060387289988, 209.1218459572589836 ) ) ;
#106360 = CARTESIAN_POINT ( 'NONE',  ( -4.045182518055000287, 1517.057265928030120, 207.4180663268770104 ) ) ;
#106361 = CARTESIAN_POINT ( 'NONE',  ( 11.58602478873720010, 1433.820729704430050, 151.2070532014469961 ) ) ;
#106362 = CARTESIAN_POINT ( 'NONE',  ( -13.84400707361050209, 1436.103923087979865, 150.2928912686649880 ) ) ;
#106363 = CARTESIAN_POINT ( 'NONE',  ( -8.871284928439999717, 1385.205931087319868, 218.6719299737089841 ) ) ;
#106364 = B_SPLINE_SURFACE_WITH_KNOTS ( 'NONE', 5, 5, ( 
 ( #109502, #7581, #8670, #83194, #102184, #68073 ),
 ( #58005, #51242, #84823, #32778, #108394, #101617 ),
 ( #31675, #65856, #66962, #99975, #92141, #108948 ),
 ( #16503, #91591, #59113, #85376, #15414, #101071 ),
 ( #41736, #50161, #50692, #49605, #24369, #58555 ),
 ( #8124, #14866, #15958, #49058, #75895, #110047 ) ),
 .UNSPECIFIED., .F., .F., .F.,
 ( 6, 6 ),
 ( 6, 6 ),
 ( 5.893388375705330695, 9.819929736144670684 ),
 ( 0.000000000000000000, 0.5002947206946709580 ),
 .UNSPECIFIED. ) ;
#106365 = DIRECTION ( 'NONE',  ( 0.000000000000000000, 1.000000000000000000, 0.000000000000000000 ) ) ;
#106366 = CARTESIAN_POINT ( 'NONE',  ( 1.707874834880000137, 1497.186644415389765, 197.2309891130989854 ) ) ;
#106367 = DIRECTION ( 'NONE',  ( -0.7384854939282345931, 0.000000000000000000, 0.6742693640212131800 ) ) ;
#106368 = VERTEX_POINT ( 'NONE', #54181 ) ;
#106369 = CARTESIAN_POINT ( 'NONE',  ( 34.21460435970000447, 1436.526926586619993, 250.0133502344980059 ) ) ;
#106370 = CARTESIAN_POINT ( 'NONE',  ( -27.02980867449999991, 1488.688182089229940, 206.7943278652880110 ) ) ;
#106372 = CARTESIAN_POINT ( 'NONE',  ( -1.135155600555850075, 1507.593744725489842, 232.0500749651639865 ) ) ;
#106371 = CARTESIAN_POINT ( 'NONE',  ( 1.453785988909999771, 1502.021732069830023, 181.3354227047979919 ) ) ;
#106373 = CARTESIAN_POINT ( 'NONE',  ( 21.03310440807343440, 1506.473666149375049, 202.6084271311502505 ) ) ;
#106374 = CARTESIAN_POINT ( 'NONE',  ( -28.01490336850000062, 1440.913060392510033, 231.6874816156980046 ) ) ;
#106375 = CARTESIAN_POINT ( 'NONE',  ( 0.8991927417389989907, 1486.143869282489959, 220.2726218139989953 ) ) ;
#106376 = ADVANCED_FACE ( 'NONE', ( #87772 ), #35138, .T. ) ;
#106377 = CARTESIAN_POINT ( 'NONE',  ( 20.12874795999999833, 1473.837606016890049, 209.1218459616989946 ) ) ;
#106378 = CARTESIAN_POINT ( 'NONE',  ( 33.54166316889999422, 1451.286620755330205, 135.9569810539979926 ) ) ;
#106379 = ORIENTED_EDGE ( 'NONE', *, *, #23299, .T. ) ;
#106380 = DIRECTION ( 'NONE',  ( -0.6450708608674635691, -0.04363816414198488230, 0.7628756747269024308 ) ) ;
#106381 = CARTESIAN_POINT ( 'NONE',  ( -17.68237282055029880, 1517.051704408389924, 205.6847408665509818 ) ) ;
#106382 = EDGE_CURVE ( 'NONE', #100544, #81391, #107259, .T. ) ;
#106383 = CARTESIAN_POINT ( 'NONE',  ( 11.74018743070000070, 1509.402761548730041, 236.7672879654979852 ) ) ;
#106384 = ORIENTED_EDGE ( 'NONE', *, *, #42673, .F. ) ;
#106385 = ORIENTED_EDGE ( 'NONE', *, *, #32444, .F. ) ;
#106386 = AXIS2_PLACEMENT_3D ( 'NONE', #5590, #31881, #108031 ) ;
#106387 = CARTESIAN_POINT ( 'NONE',  ( -1.973729821559999912E-15, 1384.913060387289988, 199.6218459572590120 ) ) ;
#106388 = CARTESIAN_POINT ( 'NONE',  ( -23.72940098905899831, 1410.154294345949893, 208.7747630995070267 ) ) ;
#106389 = ADVANCED_FACE ( 'NONE', ( #69879 ), #76716, .T. ) ;
#106390 = VERTEX_POINT ( 'NONE', #65328 ) ;
#106391 = CARTESIAN_POINT ( 'NONE',  ( -4.367915676912749845, 1447.898270802109892, 190.6350657527499948 ) ) ;
#106392 = FACE_OUTER_BOUND ( 'NONE', #21103, .T. ) ;
#106393 = CIRCLE ( 'NONE', #27676, 4.004156303888216861 ) ;
#106394 = EDGE_CURVE ( 'NONE', #32555, #105138, #54730, .T. ) ;
#106395 = CARTESIAN_POINT ( 'NONE',  ( -2.386325087049999905, 1470.484332729530024, 235.3385911319980153 ) ) ;
#106396 = CARTESIAN_POINT ( 'NONE',  ( 16.56816485274985951, 1526.186458717543701, 235.6095862221665129 ) ) ;
#106397 = ORIENTED_EDGE ( 'NONE', *, *, #15824, .F. ) ;
#106398 = CARTESIAN_POINT ( 'NONE',  ( 11.73700276120000119, 1426.696009609329849, 144.1682878317980112 ) ) ;
#106399 = CARTESIAN_POINT ( 'NONE',  ( -12.86384817108250189, 1415.089948427370018, 220.8168020335180017 ) ) ;
#106400 = CARTESIAN_POINT ( 'NONE',  ( 0.3823997583379999954, 1418.629108576230010, 184.6943103907979946 ) ) ;
#106401 = ORIENTED_EDGE ( 'NONE', *, *, #72317, .F. ) ;
#106402 = CARTESIAN_POINT ( 'NONE',  ( -3.457266643525000127, 1516.691414181030041, 203.3491180233569935 ) ) ;
#106403 = ORIENTED_EDGE ( 'NONE', *, *, #70186, .T. ) ;
#106404 = CARTESIAN_POINT ( 'NONE',  ( 10.96111033800959866, 1480.941108277019794, 213.4869506453160000 ) ) ;
#106405 = CARTESIAN_POINT ( 'NONE',  ( 1.847634001515719993, 1478.089546411300262, 198.8590795898780073 ) ) ;
#106406 = ORIENTED_EDGE ( 'NONE', *, *, #65112, .T. ) ;
#106407 = EDGE_LOOP ( 'NONE', ( #68978, #75446, #54017, #59164 ) ) ;
#106408 = CARTESIAN_POINT ( 'NONE',  ( -11.87327837476540005, 1482.014171357300029, 208.6019633461839931 ) ) ;
#106409 = CARTESIAN_POINT ( 'NONE',  ( -32.28466283162165240, 1512.187213306747481, 199.0684425896249081 ) ) ;
#106410 = CARTESIAN_POINT ( 'NONE',  ( -22.70509189929999749, 1409.705932116229860, 208.9454376012710100 ) ) ;
#106411 = CARTESIAN_POINT ( 'NONE',  ( -8.593317962150289091, 1470.520629101329860, 214.8006129900909968 ) ) ;
#106412 = CARTESIAN_POINT ( 'NONE',  ( -108.2039566672529958, 1378.913060387289988, 299.7295690038039879 ) ) ;
#106413 = CARTESIAN_POINT ( 'NONE',  ( 8.725351515859999907, 1420.892103511989944, 196.4178243839989761 ) ) ;
#106414 = ADVANCED_FACE ( 'NONE', ( #98351 ), #15864, .F. ) ;
#106415 = CARTESIAN_POINT ( 'NONE',  ( -2.853004531550470180, 1476.255805782230254, 220.2301807339150059 ) ) ;
#106416 = CARTESIAN_POINT ( 'NONE',  ( 11.14671379024469999, 1434.019377051509991, 151.6529839732360188 ) ) ;
#106417 = CARTESIAN_POINT ( 'NONE',  ( -2.249664798384999997, 1512.877808311729950, 200.5082201411669871 ) ) ;
#106419 = CARTESIAN_POINT ( 'NONE',  ( 16.45537802140000139, 1489.466917449630046, 194.2445904713979985 ) ) ;
#106418 = CARTESIAN_POINT ( 'NONE',  ( -12.63597620429999857, 1503.239529842989896, 208.6558503650219905 ) ) ;
#106420 = CARTESIAN_POINT ( 'NONE',  ( -57.01644491674332471, 1379.744987729992772, 259.4421383630754576 ) ) ;
#106421 = CARTESIAN_POINT ( 'NONE',  ( -24.15206955952350043, 1508.556946117430016, 222.3774010852600043 ) ) ;
#106422 = ADVANCED_FACE ( 'NONE', ( #102202 ), #109770, .T. ) ;
#106423 = CARTESIAN_POINT ( 'NONE',  ( -6.844666251345000063, 1512.637906871299947, 201.1997175912570128 ) ) ;
#106424 = ORIENTED_EDGE ( 'NONE', *, *, #106120, .F. ) ;
#106425 = CARTESIAN_POINT ( 'NONE',  ( 21.34957048960000137, 1432.854863361970047, 234.3916895697979612 ) ) ;
#106426 = FACE_OUTER_BOUND ( 'NONE', #109807, .T. ) ;
#106427 = CARTESIAN_POINT ( 'NONE',  ( -86.82655498892479784, 1384.976974444049802, 307.5220928825150395 ) ) ;
#106428 = AXIS2_PLACEMENT_3D ( 'NONE', #74592, #7369, #82975 ) ;
#106429 = CARTESIAN_POINT ( 'NONE',  ( 5.328644995739999501, 1505.167604692990153, 220.2736030611989975 ) ) ;
#106430 = ADVANCED_FACE ( 'NONE', ( #54465 ), #77640, .F. ) ;
#106431 = CARTESIAN_POINT ( 'NONE',  ( -15.22121264530000140, 1415.857004583649996, 211.5998937619590095 ) ) ;
#106433 = ORIENTED_EDGE ( 'NONE', *, *, #24836, .T. ) ;
#106432 = CARTESIAN_POINT ( 'NONE',  ( -17.33843278754439865, 1419.406148393270087, 207.7041131039349864 ) ) ;
#106434 = CARTESIAN_POINT ( 'NONE',  ( 16.81223226430000039, 1414.913060387329779, 210.6693098017280192 ) ) ;
#106435 = DIRECTION ( 'NONE',  ( -0.4999999999998399614, -0.7071067811867740582, 0.4999999999998399614 ) ) ;
#106436 = CARTESIAN_POINT ( 'NONE',  ( -113.9202960232132540, 1392.913060387289988, 303.3678599806595457 ) ) ;
#106437 = CARTESIAN_POINT ( 'NONE',  ( 0.5650653572531030289, 1430.599530611739965, 199.7038102876320238 ) ) ;
#106438 = CARTESIAN_POINT ( 'NONE',  ( 15.00364256283500097, 1514.335759350750095, 225.2363441599670182 ) ) ;
#106439 = DIRECTION ( 'NONE',  ( 0.000000000000000000, 1.000000000000000000, 0.000000000000000000 ) ) ;
#106440 = CIRCLE ( 'NONE', #47381, 1.999999999999997780 ) ;
#106441 = CARTESIAN_POINT ( 'NONE',  ( 6.468780810475760035, 1509.138952694780073, 179.6697712966799827 ) ) ;
#106442 = CARTESIAN_POINT ( 'NONE',  ( -41.66193840216117650, 1443.744945820009661, 136.1277624208983639 ) ) ;
#106443 = CARTESIAN_POINT ( 'NONE',  ( 32.85805783624304155, 1523.678648413191695, 201.0453875934054508 ) ) ;
#106444 = CARTESIAN_POINT ( 'NONE',  ( 15.81240911520000125, 1417.427885388930008, 227.3441162537980347 ) ) ;
#106445 = CARTESIAN_POINT ( 'NONE',  ( -11.18076303840566332, 1517.051704408389924, 213.9857921429048417 ) ) ;
#106446 = CARTESIAN_POINT ( 'NONE',  ( 1.700706776364999895, 1516.923170579120097, 206.8211163054370161 ) ) ;
#106447 = CARTESIAN_POINT ( 'NONE',  ( 41.16455037149999896, 1425.337515733230020, 266.3184770345980041 ) ) ;
#106448 = CARTESIAN_POINT ( 'NONE',  ( -18.55304899770000304, 1410.484400192730163, 223.7713282511979855 ) ) ;
#106449 = CARTESIAN_POINT ( 'NONE',  ( 22.35103205260000081, 1436.090882114679971, 142.4834648293980024 ) ) ;
#106450 = CARTESIAN_POINT ( 'NONE',  ( -0.9044168070210000243, 1418.675475465229965, 228.1103104084980373 ) ) ;
#106451 = CARTESIAN_POINT ( 'NONE',  ( 5.379930311655070518, 1430.658779919180006, 154.4493466840170015 ) ) ;
#106452 = CARTESIAN_POINT ( 'NONE',  ( -37.54398636633066388, 1461.570449753633966, 266.4251595816978124 ) ) ;
#106453 = CARTESIAN_POINT ( 'NONE',  ( -14.26437337564139973, 1416.738556469530067, 203.2135512967790021 ) ) ;
#106454 = CARTESIAN_POINT ( 'NONE',  ( -38.86240415199999632, 1439.430083176099970, 136.6726061590980237 ) ) ;
#106455 = CARTESIAN_POINT ( 'NONE',  ( 0.2086211941929050073, 1458.123855251709983, 183.0335782383330070 ) ) ;
#106456 = CARTESIAN_POINT ( 'NONE',  ( -9.967857204701429552, 1407.622385665449883, 200.5556886166019979 ) ) ;
#106457 = CARTESIAN_POINT ( 'NONE',  ( -11.73070209449999979, 1414.913060387329779, 197.7037767505979957 ) ) ;
#106458 = CARTESIAN_POINT ( 'NONE',  ( 18.72690275718901987, 1526.278758871497985, 182.1127646906432744 ) ) ;
#106459 = CARTESIAN_POINT ( 'NONE',  ( -28.04361090164860215, 1509.087630844720024, 210.7243009158079872 ) ) ;
#106460 = CARTESIAN_POINT ( 'NONE',  ( 12.91288853569999873, 1434.774381388219808, 149.4778850478979848 ) ) ;
#106461 = CARTESIAN_POINT ( 'NONE',  ( -38.01446494613939819, 1436.977963748669936, 134.0999999969440069 ) ) ;
#106462 = CARTESIAN_POINT ( 'NONE',  ( 3.851527341300000185, 1440.290862272119966, 184.6363558007980146 ) ) ;
#106463 = ORIENTED_EDGE ( 'NONE', *, *, #73425, .F. ) ;
#106464 = CARTESIAN_POINT ( 'NONE',  ( 3.556995324409999881, 1476.475065048189890, 198.0947962222990100 ) ) ;
#106465 = CARTESIAN_POINT ( 'NONE',  ( 40.31826125219999568, 1443.160130861930156, 137.0614306859980047 ) ) ;
#106466 = CARTESIAN_POINT ( 'NONE',  ( -11.29172267060000046, 1491.552985758590012, 207.2028609495190210 ) ) ;
#106467 = CARTESIAN_POINT ( 'NONE',  ( 2.203005645500000220, 1464.498845408490070, 202.4205385530689796 ) ) ;
#106468 = DIRECTION ( 'NONE',  ( 0.5117323852940846018, 0.8591449038673432126, 0.000000000000000000 ) ) ;
#106469 = CARTESIAN_POINT ( 'NONE',  ( -31.53040958840000485, 1466.256159665430005, 268.9167898976980382 ) ) ;
#106470 = CARTESIAN_POINT ( 'NONE',  ( -11.85463470256620155, 1481.688684073870036, 209.6797579912160074 ) ) ;
#106471 = CARTESIAN_POINT ( 'NONE',  ( -16.66231036550682276, 1523.604703353109699, 237.7554842931448036 ) ) ;
#106472 = CARTESIAN_POINT ( 'NONE',  ( -26.15182807060000059, 1509.826302347529918, 220.8502595356980009 ) ) ;
#106473 = CARTESIAN_POINT ( 'NONE',  ( -94.45993641895300641, 1384.611044289900065, 309.9217182750660413 ) ) ;
#106474 = CARTESIAN_POINT ( 'NONE',  ( -30.26357380513479711, 1384.969279520580130, 205.7050507507260022 ) ) ;
#106475 = CARTESIAN_POINT ( 'NONE',  ( -12.24102064520350019, 1490.576295553370073, 208.4712049614670093 ) ) ;
#106476 = CARTESIAN_POINT ( 'NONE',  ( 20.86040077210000021, 1508.959081887729781, 227.6602567232980050 ) ) ;
#106477 = CARTESIAN_POINT ( 'NONE',  ( -29.40921901757340251, 1509.877385649660027, 208.6169211888969812 ) ) ;
#106478 = CARTESIAN_POINT ( 'NONE',  ( -3.347801439296141712, 1523.382868172864164, 176.1543725841967500 ) ) ;
#106480 = ORIENTED_EDGE ( 'NONE', *, *, #21508, .F. ) ;
#106479 = CARTESIAN_POINT ( 'NONE',  ( 0.5065993652445669460, 1412.370428418450047, 184.9838650198409766 ) ) ;
#106481 = CARTESIAN_POINT ( 'NONE',  ( -13.77715290559999950, 1508.637939534930183, 184.0711877140979880 ) ) ;
#106482 = B_SPLINE_CURVE_WITH_KNOTS ( 'NONE', 5,
 ( #7239, #49806, #17810, #67164, #52010, #16163, #41399, #17255, #34643, #40834, #32974, #85578, #6680, #15601, #76644, #101261, #50902, #33513 ),
 .UNSPECIFIED., .F., .F.,
 ( 6, 3, 3, 3, 3, 6 ),
 ( -75.86994138869999915, -60.45619974110000072, -46.86861349480000172, -18.08975840989999284, -6.500000000000000000, -0.4214913904880006612 ),
 .UNSPECIFIED. ) ;
#106484 = DIRECTION ( 'NONE',  ( 0.000000000000000000, 0.000000000000000000, -1.000000000000000000 ) ) ;
#106483 = CIRCLE ( 'NONE', #74294, 23.99999935407219454 ) ;
#106485 = DIRECTION ( 'NONE',  ( 0.9980844203940678616, -0.06184550950381709211, 0.001619481661242269796 ) ) ;
#106486 = CARTESIAN_POINT ( 'NONE',  ( -12.62835224979999893, 1416.067629290630066, 195.5863397732979934 ) ) ;
#106487 = CARTESIAN_POINT ( 'NONE',  ( -31.34137657934000387, 1501.977400791986611, 221.9025654077414345 ) ) ;
#106488 = CARTESIAN_POINT ( 'NONE',  ( 23.24624089760000345, 1410.220001169729812, 212.0510662298279954 ) ) ;
#106489 = B_SPLINE_SURFACE_WITH_KNOTS ( 'NONE', 5, 5, ( 
 ( #34441, #51241, #76440, #26580, #27151, #69167, #36107, #1399, #52916 ),
 ( #70293, #861, #1971, #42289, #102719, #60777, #26013, #60209, #94902 ),
 ( #110595, #104404, #78095, #18176, #33879, #17606, #87048, #27698, #86492 ),
 ( #103272, #25463, #43953, #35538, #44508, #69733, #78655, #16502, #95455 ),
 ( #94328, #50691, #102183, #77010, #84822, #8123, #93766, #17045, #103852 ),
 ( #18720, #51806, #34987, #85375, #43406, #20927, #13071, #3079, #63004 ) ),
 .UNSPECIFIED., .F., .F., .F.,
 ( 6, 6 ),
 ( 6, 3, 6 ),
 ( 9.791992066980000686, 13.21653623010000089 ),
 ( 0.000000000000000000, 1.500000000000000000, 3.000000000000000000 ),
 .UNSPECIFIED. ) ;
#106490 = DIRECTION ( 'NONE',  ( 0.9125304618754029873, 0.000000000000000000, 0.4090087482554177756 ) ) ;
#106491 = CARTESIAN_POINT ( 'NONE',  ( -18.47517316556379896, 1466.235620594650072, 200.8822777731460008 ) ) ;
#106492 = CARTESIAN_POINT ( 'NONE',  ( -7.878537825433329367, 1517.151704408390060, 218.1850669711710111 ) ) ;
#106494 = CARTESIAN_POINT ( 'NONE',  ( -13.26994390069999952, 1379.834384431509989, 206.1416992256990000 ) ) ;
#106493 = CARTESIAN_POINT ( 'NONE',  ( -11.57799723109999945, 1432.441865831549876, 151.1964732625980048 ) ) ;
#106495 = CARTESIAN_POINT ( 'NONE',  ( -10.49767883750000053, 1382.256743515189783, 217.7001910593189677 ) ) ;
#106496 = CARTESIAN_POINT ( 'NONE',  ( -124.1574587856609071, 1375.179104070688936, 298.3450194382701852 ) ) ;
#106497 = CARTESIAN_POINT ( 'NONE',  ( 1970.025574498409924, -8382.262153571269664, 413.0777247525010125 ) ) ;
#106498 = CARTESIAN_POINT ( 'NONE',  ( -23.87304943890000075, 1435.754597106050142, 211.2923954554679824 ) ) ;
#106499 = CARTESIAN_POINT ( 'NONE',  ( -0.7618909056620021270, 1360.403425203259985, 210.6218459616991936 ) ) ;
#106500 = CARTESIAN_POINT ( 'NONE',  ( -0.01327408612949850138, 1516.939877939420057, 205.6663500982469941 ) ) ;
#106501 = CARTESIAN_POINT ( 'NONE',  ( -17.37601589566219928, 1485.496354615790096, 188.4150023406379830 ) ) ;
#106502 = CARTESIAN_POINT ( 'NONE',  ( -9.199049879260000395, 1422.949100153850168, 210.5804414222690184 ) ) ;
#106503 = CARTESIAN_POINT ( 'NONE',  ( -12.08007700854662225, 1421.774748355924658, 210.6450025019371139 ) ) ;
#106505 = ORIENTED_EDGE ( 'NONE', *, *, #46749, .T. ) ;
#106504 = CARTESIAN_POINT ( 'NONE',  ( -68.29979175837739547, 1379.746978049359996, 279.8462751379269662 ) ) ;
#106506 = EDGE_LOOP ( 'NONE', ( #62511, #109971, #97789, #59256 ) ) ;
#106507 = CARTESIAN_POINT ( 'NONE',  ( 28.21332323700000089, 1508.643929370829937, 209.7679031484589984 ) ) ;
#106508 = EDGE_LOOP ( 'NONE', ( #63816, #74349, #2039, #55431, #101972 ) ) ;
#106509 = FACE_OUTER_BOUND ( 'NONE', #498, .T. ) ;
#106510 = VECTOR ( 'NONE', #85935, 1000.000000000000000 ) ;
#106511 = CARTESIAN_POINT ( 'NONE',  ( -109.9852357310000031, 1384.922450477979964, 311.4561609882589437 ) ) ;
#106513 = CARTESIAN_POINT ( 'NONE',  ( 24.39988810369999683, 1444.709222782450070, 214.8827041012880272 ) ) ;
#106512 = CARTESIAN_POINT ( 'NONE',  ( 15.84085386514549931, 1416.203647188709738, 191.3516974002209849 ) ) ;
#106514 = CARTESIAN_POINT ( 'NONE',  ( -7.710967015764999211, 1516.608208975040043, 210.2506035313070072 ) ) ;
#106515 = CARTESIAN_POINT ( 'NONE',  ( -24.00451132643230068, 1452.074800784660056, 136.6367033768989927 ) ) ;
#106516 = DIRECTION ( 'NONE',  ( 0.000000000000000000, 0.5877852522921415135, -0.8090169943751884807 ) ) ;
#106517 = CARTESIAN_POINT ( 'NONE',  ( 14.70688542969999979, 1409.928487481030061, 227.4346275906979997 ) ) ;
#106519 = EDGE_CURVE ( 'NONE', #91721, #43187, #91192, .T. ) ;
#106518 = CARTESIAN_POINT ( 'NONE',  ( 10.04235571396320026, 1481.895431969530136, 213.0073720138159956 ) ) ;
#106520 = APPLICATION_PROTOCOL_DEFINITION ( 'draft international standard', 'automotive_design', 1998, #64909 ) ;
#106522 = AXIS2_PLACEMENT_3D ( 'NONE', #45830, #79963, #35195 ) ;
#106521 = CARTESIAN_POINT ( 'NONE',  ( 40.14707100556169905, 1448.397814785060064, 134.0999999982449822 ) ) ;
#106523 = CARTESIAN_POINT ( 'NONE',  ( -7.229435970709999992, 1480.743738106489900, 207.9750912412490038 ) ) ;
#106524 = VERTEX_POINT ( 'NONE', #76192 ) ;
#106525 = CARTESIAN_POINT ( 'NONE',  ( 14.52275784015550109, 1435.809058665319981, 149.7340231952910017 ) ) ;
#106526 = CARTESIAN_POINT ( 'NONE',  ( -1.196549396492360140, 1431.757418655609854, 200.8025689291640106 ) ) ;
#106527 = ORIENTED_EDGE ( 'NONE', *, *, #30221, .T. ) ;
#106528 = ORIENTED_EDGE ( 'NONE', *, *, #86399, .F. ) ;
#106529 = VERTEX_POINT ( 'NONE', #25208 ) ;
#106530 = CARTESIAN_POINT ( 'NONE',  ( 12.08338312575843787, 1410.708559485759224, 228.9665408485644491 ) ) ;
#106531 = CARTESIAN_POINT ( 'NONE',  ( 16.78772369872005754, 1513.520094853501405, 195.9605301170960843 ) ) ;
#106532 = CARTESIAN_POINT ( 'NONE',  ( 16.51877150081237389, 1451.100436498563113, 148.6701188902696344 ) ) ;
#106533 = CARTESIAN_POINT ( 'NONE',  ( -22.86388141493510062, 1452.114636054849825, 134.0999999999999943 ) ) ;
#106534 = CARTESIAN_POINT ( 'NONE',  ( -18.58116375392060249, 1445.454363348780362, 214.2320557096282130 ) ) ;
#106535 = CARTESIAN_POINT ( 'NONE',  ( -67.62101597386647711, 1379.745593051518881, 277.6608951446080482 ) ) ;
#106536 = CARTESIAN_POINT ( 'NONE',  ( -0.5893430329309989890, 1464.381058777490125, 199.1585742529190100 ) ) ;
#106537 = EDGE_CURVE ( 'NONE', #76557, #92712, #60513, .T. ) ;
#106538 = DIRECTION ( 'NONE',  ( -0.6736849260863841948, 0.000000000000000000, 0.7390186874254148774 ) ) ;
#106539 = CARTESIAN_POINT ( 'NONE',  ( 3.560382106670000102, 1415.087974639930053, 191.9480497089980133 ) ) ;
#106540 = CARTESIAN_POINT ( 'NONE',  ( -63.26676713937528973, 1384.693636663830148, 251.1880306028709811 ) ) ;
#106541 = EDGE_LOOP ( 'NONE', ( #51731, #71959, #45276, #53700 ) ) ;
#106542 = CARTESIAN_POINT ( 'NONE',  ( 6.933616821004999764, 1516.548716157039962, 206.8295387017270173 ) ) ;
#106543 = ORIENTED_EDGE ( 'NONE', *, *, #32311, .F. ) ;
#106544 = CARTESIAN_POINT ( 'NONE',  ( 30.67453579933340180, 1440.913060387330006, 253.4609548031900204 ) ) ;
#106545 = B_SPLINE_CURVE_WITH_KNOTS ( 'NONE', 5,
 ( #107143, #32093, #29880, #22002, #30435, #15270 ),
 .UNSPECIFIED., .F., .F.,
 ( 6, 6 ),
 ( 1.385794409258260110E-07, 0.5294135995224299451 ),
 .UNSPECIFIED. ) ;
#106546 = CARTESIAN_POINT ( 'NONE',  ( 11.63359383422730176, 1479.019660161769934, 207.4180740764660129 ) ) ;
#106547 = ORIENTED_EDGE ( 'NONE', *, *, #26077, .T. ) ;
#106548 = CARTESIAN_POINT ( 'NONE',  ( -0.5697989934050000649, 1450.893162568020216, 181.2886233453980083 ) ) ;
#106549 = CARTESIAN_POINT ( 'NONE',  ( -15.82667276960000180, 1410.838063423429958, 191.2287379893979846 ) ) ;
#106550 = CARTESIAN_POINT ( 'NONE',  ( -108.8494111198608323, 1383.998126889661307, 311.1481491610576882 ) ) ;
#106551 = CARTESIAN_POINT ( 'NONE',  ( -24.41186848580399982, 1440.913060429360030, 212.0284777848129920 ) ) ;
#106552 = CARTESIAN_POINT ( 'NONE',  ( -9.613420378160620672, 1438.053801520089792, 211.4783176813969874 ) ) ;
#106553 = CARTESIAN_POINT ( 'NONE',  ( 13.90221994160000030, 1436.238121858259774, 150.2928703997980051 ) ) ;
#106555 = B_SPLINE_CURVE_WITH_KNOTS ( 'NONE', 3,
 ( #65058, #4059, #79664, #38185, #56654, #55563, #81828, #13512 ),
 .UNSPECIFIED., .F., .F.,
 ( 4, 2, 2, 4 ),
 ( 0.000000000000000000, 0.001073044933456205339, 0.001609567400184348232, 0.002146089866912491342 ),
 .UNSPECIFIED. ) ;
#106554 = CARTESIAN_POINT ( 'NONE',  ( 43.71400182546053514, 1430.030204529002958, 266.2448334775871785 ) ) ;
#106556 = CARTESIAN_POINT ( 'NONE',  ( -6.164039445902147030, 1510.821818207758270, 201.6558465868637313 ) ) ;
#106557 = DIRECTION ( 'NONE',  ( -1.387778780781598557E-14, -1.000000000000000000, 0.000000000000000000 ) ) ;
#106559 = CARTESIAN_POINT ( 'NONE',  ( -10.23378643512955577, 1422.709436974594610, 137.1241386678474043 ) ) ;
#106558 = CARTESIAN_POINT ( 'NONE',  ( 8.038768963489999919, 1463.606875709430142, 235.5281748529980064 ) ) ;
#106560 = EDGE_CURVE ( 'NONE', #44996, #78702, #100819, .T. ) ;
#106561 = CARTESIAN_POINT ( 'NONE',  ( 7.331183090945000203, 1516.882217593000178, 216.0635732225570109 ) ) ;
#106562 = CARTESIAN_POINT ( 'NONE',  ( -8.320994297490690528, 1422.937291762939822, 213.3671062658739856 ) ) ;
#106563 = CARTESIAN_POINT ( 'NONE',  ( -0.1550544472294869969, 1507.335707632679942, 180.8803381700240038 ) ) ;
#106564 = CARTESIAN_POINT ( 'NONE',  ( 3.461047291624999911, 1516.858765657450249, 212.5691103191969944 ) ) ;
#106565 = CIRCLE ( 'NONE', #29412, 1.999999999999999556 ) ;
#106566 = CARTESIAN_POINT ( 'NONE',  ( -11.46886437749099841, 1482.732392890260144, 205.9150088758919708 ) ) ;
#106567 = ADVANCED_FACE ( 'NONE', ( #94080 ), #49899, .T. ) ;
#106568 = DIRECTION ( 'NONE',  ( -0.000000000000000000, -1.000000000000000000, -0.000000000000000000 ) ) ;
#106570 = ORIENTED_EDGE ( 'NONE', *, *, #4657, .T. ) ;
#106569 = CARTESIAN_POINT ( 'NONE',  ( -103.7369032989999909, 1385.230281736809957, 296.9336279125589613 ) ) ;
#106571 = CARTESIAN_POINT ( 'NONE',  ( -8.848209551960000141, 1384.890560814510081, 199.9248350966889802 ) ) ;
#106572 = CARTESIAN_POINT ( 'NONE',  ( 25.18985267090000235, 1442.566560664089820, 217.4969598497380048 ) ) ;
#106573 = CARTESIAN_POINT ( 'NONE',  ( -11.86665551350000136, 1432.374829077889899, 149.9823017929979869 ) ) ;
#106574 = CARTESIAN_POINT ( 'NONE',  ( -20.65369855650610020, 1487.044956911440067, 207.4344914902700054 ) ) ;
#106575 = CARTESIAN_POINT ( 'NONE',  ( 2.670551802009999864, 1411.760187836130171, 231.7294704944980026 ) ) ;
#106576 = DIRECTION ( 'NONE',  ( 0.9455185755993178454, 0.000000000000000000, -0.3255681544571539243 ) ) ;
#106577 = CARTESIAN_POINT ( 'NONE',  ( -9.966727850805121136, 1439.480327375449860, 208.4309914983489875 ) ) ;
#106579 = CARTESIAN_POINT ( 'NONE',  ( 2.500000000000000000, 1425.201036443130079, 155.3321294796979828 ) ) ;
#106578 = CARTESIAN_POINT ( 'NONE',  ( -22.57989227939999921, 1470.081218446630146, 221.4829011586980130 ) ) ;
#106580 = CARTESIAN_POINT ( 'NONE',  ( -2.546419266200000475, 1485.854131597229980, 182.3738517892980155 ) ) ;
#106581 = VERTEX_POINT ( 'NONE', #67808 ) ;
#106582 = CARTESIAN_POINT ( 'NONE',  ( 6.548821941055000373, 1516.688761843659904, 205.0844676760469838 ) ) ;
#106583 = CARTESIAN_POINT ( 'NONE',  ( 2.763724491000000061, 1406.126245782430033, 269.0427161091980111 ) ) ;
#106584 = CARTESIAN_POINT ( 'NONE',  ( -113.4000000000000057, 1305.913060387289988, 304.2218459572590064 ) ) ;
#106585 = AXIS2_PLACEMENT_3D ( 'NONE', #15285, #57881, #92550 ) ;
#106586 = CARTESIAN_POINT ( 'NONE',  ( 41.41036356811409291, 1451.093780838620205, 270.1893080176820376 ) ) ;
#106587 = CARTESIAN_POINT ( 'NONE',  ( -25.18563703530000097, 1452.033577648029905, 135.3787234722980202 ) ) ;
#106588 = CARTESIAN_POINT ( 'NONE',  ( 11.60004869884103407, 1423.521825948030937, 137.0424065539601770 ) ) ;
#106589 = CARTESIAN_POINT ( 'NONE',  ( -6.916803064789941224, 1439.753322365320628, 203.7544753627797149 ) ) ;
#106590 = CARTESIAN_POINT ( 'NONE',  ( -7.055457375169999601, 1459.495818635790101, 217.3326011958589845 ) ) ;
#106591 = CARTESIAN_POINT ( 'NONE',  ( -1.672144570133835995, 1451.729478148845374, 184.0944664686900296 ) ) ;
#106592 = CARTESIAN_POINT ( 'NONE',  ( -1.676215897828090107, 1450.511945644329899, 182.4451613505460159 ) ) ;
#106593 = CARTESIAN_POINT ( 'NONE',  ( -13.64809019991630024, 1415.124054205850143, 220.5687789520499962 ) ) ;
#106594 = CARTESIAN_POINT ( 'NONE',  ( -4.123245670370000227, 1515.545044289889802, 209.8706601212949749 ) ) ;
#106595 = ORIENTED_EDGE ( 'NONE', *, *, #77840, .F. ) ;
#106596 = CARTESIAN_POINT ( 'NONE',  ( 2.886579864029999753E-15, 1413.763055110029882, 262.6648722463980334 ) ) ;
#106597 = CARTESIAN_POINT ( 'NONE',  ( 2.500000000000000000, 1439.625347662450167, 166.9460400662979964 ) ) ;
#106598 = CARTESIAN_POINT ( 'NONE',  ( -0.5593523789189999151, 1476.106998426729888, 267.8539144646980503 ) ) ;
#106599 = CARTESIAN_POINT ( 'NONE',  ( -32.67729582440000513, 1451.771913520829912, 134.7516611205979871 ) ) ;
#106600 = CARTESIAN_POINT ( 'NONE',  ( -110.7631994250367029, 1305.714868215269917, 299.3952148801843691 ) ) ;
#106601 = DIRECTION ( 'NONE',  ( 1.224646799147350002E-16, -1.836970198721029688E-16, -1.000000000000000000 ) ) ;
#106602 = CARTESIAN_POINT ( 'NONE',  ( -25.61501306685740076, 1384.843999110390087, 224.1472815994760026 ) ) ;
#106603 = CARTESIAN_POINT ( 'NONE',  ( -106.1058971500000041, 1378.913060387289988, 302.5343330838589395 ) ) ;
#106604 = CARTESIAN_POINT ( 'NONE',  ( 32.22536377336281532, 1523.621879633029039, 216.8351145222429466 ) ) ;
#106605 = CARTESIAN_POINT ( 'NONE',  ( 0.2538829723067779764, 1420.503732877419907, 182.7635795570130028 ) ) ;
#106606 =( BOUNDED_CURVE ( )  B_SPLINE_CURVE ( 3, ( #97336, #3314, #39644, #3865 ),
 .UNSPECIFIED., .F., .F. ) 
 B_SPLINE_CURVE_WITH_KNOTS ( ( 4, 4 ),
 ( 4.409610437282244888, 5.070003789806990291 ),
 .UNSPECIFIED. ) 
 CURVE ( )  GEOMETRIC_REPRESENTATION_ITEM ( )  RATIONAL_B_SPLINE_CURVE ( ( 1.000000000000000000, 0.9639857291066213918, 0.9639857291066213918, 1.000000000000000000 ) ) 
 REPRESENTATION_ITEM ( '' )  );
#106607 = CARTESIAN_POINT ( 'NONE',  ( -5.750244769764350394, 1396.113863361650147, 218.5416372912760039 ) ) ;
#106608 = CARTESIAN_POINT ( 'NONE',  ( -3.244847879459100248, 1508.551704408389924, 204.2522919139599935 ) ) ;
#106609 = CARTESIAN_POINT ( 'NONE',  ( -45.60176523299999474, 1439.545916309389895, 268.9757053294979983 ) ) ;
#106610 = VERTEX_POINT ( 'NONE', #17349 ) ;
#106611 = CARTESIAN_POINT ( 'NONE',  ( -2.207969477403779912, 1436.315141507179987, 227.4839793697360051 ) ) ;
#106612 = CARTESIAN_POINT ( 'NONE',  ( -13.58088438526920072, 1508.551704407800116, 210.3100666414740090 ) ) ;
#106613 = CARTESIAN_POINT ( 'NONE',  ( -11.28228388660000014, 1484.392611670030192, 185.3973464570979957 ) ) ;
#106615 = CARTESIAN_POINT ( 'NONE',  ( -13.99234591236500158, 1513.736060322949925, 192.3918525003670084 ) ) ;
#106614 = CARTESIAN_POINT ( 'NONE',  ( 11.62090964459999931, 1426.357348742330032, 135.9230500439979892 ) ) ;
#106616 = DIRECTION ( 'NONE',  ( -0.7071067811865474617, 4.329780281177460882E-17, 0.7071067811865474617 ) ) ;
#106617 = CARTESIAN_POINT ( 'NONE',  ( -13.69967938769999982, 1380.327631092480033, 209.8719513141080029 ) ) ;
#106618 = CARTESIAN_POINT ( 'NONE',  ( -3.261007169695000041, 1516.596789218710001, 201.7991362452670216 ) ) ;
#106619 = CARTESIAN_POINT ( 'NONE',  ( 7.635296396580000255, 1426.631419723420095, 212.2123003208889997 ) ) ;
#106620 = CARTESIAN_POINT ( 'NONE',  ( -22.15968325629999924, 1485.573345355790025, 217.2083650093589995 ) ) ;
#106621 = CARTESIAN_POINT ( 'NONE',  ( 1.448678579899999930, 1507.129710292329946, 181.1126013549980200 ) ) ;
#106622 = CARTESIAN_POINT ( 'NONE',  ( 7.404094472206104172, 1512.905891558378698, 217.4471223568880021 ) ) ;
#106623 = CARTESIAN_POINT ( 'NONE',  ( -93.66127265309958716, 1377.138788487970032, 305.4911171557070020 ) ) ;
#106624 = CARTESIAN_POINT ( 'NONE',  ( 7.230203487789204964, 1365.895265398900847, 208.3718459617061285 ) ) ;
#106626 = ORIENTED_EDGE ( 'NONE', *, *, #98035, .T. ) ;
#106625 = CARTESIAN_POINT ( 'NONE',  ( 9.906408661899998691, 1453.734930172990062, 213.0153772767789917 ) ) ;
#106627 = ORIENTED_EDGE ( 'NONE', *, *, #863, .T. ) ;
#106628 = CARTESIAN_POINT ( 'NONE',  ( -8.555999076900000944, 1397.549004006330051, 199.0552853815979972 ) ) ;
#106629 = CARTESIAN_POINT ( 'NONE',  ( 2.887715917392400300, 1409.376950096379915, 231.1465570425760063 ) ) ;
#106630 = CARTESIAN_POINT ( 'NONE',  ( -7.329925260613682880, 1516.833976298084281, 201.4049670776166749 ) ) ;
#106631 = CARTESIAN_POINT ( 'NONE',  ( -6.931887347990000059, 1409.155127227530102, 188.8914258914980167 ) ) ;
#106632 = CARTESIAN_POINT ( 'NONE',  ( 1.910126501409999789E-10, 1431.113060387329824, 227.8291532366980050 ) ) ;
#106633 = CARTESIAN_POINT ( 'NONE',  ( -7.937216491484998748, 1511.802450769970164, 212.2876873266469886 ) ) ;
#106635 = CARTESIAN_POINT ( 'NONE',  ( -21.51614340397090075, 1505.638256348389859, 209.3196076299650201 ) ) ;
#106634 = CARTESIAN_POINT ( 'NONE',  ( -103.9057015030000031, 1389.915727242629828, 305.4069455405589792 ) ) ;
#106636 = CARTESIAN_POINT ( 'NONE',  ( 0.6856161522000000508, 1410.310357111729900, 185.1124255419979932 ) ) ;
#106637 = CARTESIAN_POINT ( 'NONE',  ( -37.26789664401470503, 1450.479926032020103, 135.9651663335700107 ) ) ;
#106638 = CARTESIAN_POINT ( 'NONE',  ( 41.66194080536450173, 1443.744915603149821, 136.1277488527510116 ) ) ;
#106639 = CARTESIAN_POINT ( 'NONE',  ( 33.27870177008182395, 1435.659577329578951, 135.0862789282056724 ) ) ;
#106640 = CARTESIAN_POINT ( 'NONE',  ( -27.93599228559999759, 1442.648988978950001, 137.4365311676980355 ) ) ;
#106641 = CARTESIAN_POINT ( 'NONE',  ( 10.94295718250000071, 1430.426329750230252, 151.5194551083980059 ) ) ;
#106642 = CARTESIAN_POINT ( 'NONE',  ( -0.04641543311909263059, 1519.551704408389924, 230.3502074419784265 ) ) ;
#106643 = ORIENTED_EDGE ( 'NONE', *, *, #87706, .F. ) ;
#106644 = CARTESIAN_POINT ( 'NONE',  ( 4.229500449809999729, 1423.902524512430091, 183.5234483264979986 ) ) ;
#106645 = CARTESIAN_POINT ( 'NONE',  ( 20.49599333844858151, 1525.960063244517187, 233.8638087104923216 ) ) ;
#106646 = EDGE_LOOP ( 'NONE', ( #78800, #97482, #16424, #31859 ) ) ;
#106647 = ORIENTED_EDGE ( 'NONE', *, *, #81068, .T. ) ;
#106648 = CARTESIAN_POINT ( 'NONE',  ( -17.65532971150000208, 1419.497219977419945, 207.2321558962389929 ) ) ;
#106649 = CARTESIAN_POINT ( 'NONE',  ( 5.215187551879999717, 1368.779556716650177, 207.6218459616989946 ) ) ;
#106650 = CARTESIAN_POINT ( 'NONE',  ( 15.60314760730000039, 1425.942174865029983, 212.9755122303479880 ) ) ;
#106651 = FACE_OUTER_BOUND ( 'NONE', #55936, .T. ) ;
#106652 = CARTESIAN_POINT ( 'NONE',  ( 5.006329581384999727, 1516.755758396839838, 215.6722354023569892 ) ) ;
#106653 = CARTESIAN_POINT ( 'NONE',  ( -12.31905933190130042, 1378.298490798669945, 209.5595369833839925 ) ) ;
#106654 = COLOUR_RGB ( '', 0.31764706, 0.68627451, 0.89019608) ;
#106655 = ORIENTED_EDGE ( 'NONE', *, *, #93262, .F. ) ;
#106656 = CARTESIAN_POINT ( 'NONE',  ( -17.83734749800949970, 1508.522611025080096, 211.8629472681300001 ) ) ;
#106657 = CARTESIAN_POINT ( 'NONE',  ( -5.957503935620779956, 1509.188430844039885, 179.6796226404359800 ) ) ;
#106658 = CARTESIAN_POINT ( 'NONE',  ( -62.88186284109999491, 1374.821258372890043, 270.0876510056589836 ) ) ;
#106659 = EDGE_CURVE ( 'NONE', #65282, #101005, #87619, .T. ) ;
#106660 = CARTESIAN_POINT ( 'NONE',  ( 18.12194535329999923, 1416.217772597929979, 213.0453993036479972 ) ) ;
#106661 = CARTESIAN_POINT ( 'NONE',  ( 5.773668814845000163, 1516.734985836460055, 205.0832084693769843 ) ) ;
#106662 = ORIENTED_EDGE ( 'NONE', *, *, #51476, .F. ) ;
#106663 = CARTESIAN_POINT ( 'NONE',  ( -19.70969297780000318, 1440.913060387330006, 214.9271664100980104 ) ) ;
#106664 = EDGE_CURVE ( 'NONE', #18275, #70222, #19066, .T. ) ;
#106665 = CARTESIAN_POINT ( 'NONE',  ( -29.83114707306344826, 1419.453282592096002, 269.4690146648258064 ) ) ;
#106666 = CIRCLE ( 'NONE', #38239, 93.02998377600577840 ) ;
#106667 = CARTESIAN_POINT ( 'NONE',  ( -4.781335570289999559, 1409.080028304630105, 230.4240303851980229 ) ) ;
#106669 = VERTEX_POINT ( 'NONE', #16254 ) ;
#106668 = CARTESIAN_POINT ( 'NONE',  ( -3.487133837120000024, 1431.113060387329824, 190.6407012183980214 ) ) ;
#106670 = CARTESIAN_POINT ( 'NONE',  ( 2.500000000000000000, 1419.382872273060002, 144.1054344980790063 ) ) ;
#106671 = CARTESIAN_POINT ( 'NONE',  ( -26.99520746976219954, 1440.913060419549993, 226.8119193977670136 ) ) ;
#106672 = CARTESIAN_POINT ( 'NONE',  ( -13.38802240389999909, 1383.860181226410077, 218.7963554078490063 ) ) ;
#106673 = CARTESIAN_POINT ( 'NONE',  ( 10.10526312269999849, 1471.402127165189995, 212.2219414490489839 ) ) ;
#106674 = CARTESIAN_POINT ( 'NONE',  ( 42.06226826553579912, 1436.795776192510175, 269.6487248881980463 ) ) ;
#106675 = CARTESIAN_POINT ( 'NONE',  ( -1.702406023195000007, 1516.999105586269934, 212.3918307515370145 ) ) ;
#106676 = CARTESIAN_POINT ( 'NONE',  ( -67.91765045250001265, 1379.745871413030045, 278.2920511910589880 ) ) ;
#106677 = CARTESIAN_POINT ( 'NONE',  ( 22.82834858460000049, 1409.718736107430232, 208.8015344678899794 ) ) ;
#106678 = CARTESIAN_POINT ( 'NONE',  ( 0.01851582568700120210, 1507.478319835492812, 237.4021211056988818 ) ) ;
#106679 = CARTESIAN_POINT ( 'NONE',  ( 6.179817242093199603, 1424.911203525419978, 192.2193043612860208 ) ) ;
#106680 = CARTESIAN_POINT ( 'NONE',  ( -7.718845898157540297, 1516.909122020879977, 209.2104016507690005 ) ) ;
#106681 = CARTESIAN_POINT ( 'NONE',  ( 6.951517132375000685, 1517.194816588360027, 210.2467400204669730 ) ) ;
#106682 = CARTESIAN_POINT ( 'NONE',  ( -106.5585968837300044, 1390.939245634569943, 300.3884029622149683 ) ) ;
#106683 = CARTESIAN_POINT ( 'NONE',  ( -2.801976539950000067, 1420.449080726529928, 233.0291344731980132 ) ) ;
#106684 = CARTESIAN_POINT ( 'NONE',  ( -96.24057774249999397, 1384.839338083349958, 310.5876767322589558 ) ) ;
#106685 = ORIENTED_EDGE ( 'NONE', *, *, #68675, .T. ) ;
#106686 = CARTESIAN_POINT ( 'NONE',  ( -20.43314471396830001, 1385.274570738710054, 221.1097988323519985 ) ) ;
#106687 = DIRECTION ( 'NONE',  ( -0.3090169943749382919, 0.000000000000000000, 0.9510565162951565288 ) ) ;
#106688 = CARTESIAN_POINT ( 'NONE',  ( -0.004541069570850000091, 1417.346727570329904, 235.5710176400980060 ) ) ;
#106689 = CARTESIAN_POINT ( 'NONE',  ( -2.140641997699999965, 1508.551704408389924, 220.0635241299990241 ) ) ;
#106690 = CARTESIAN_POINT ( 'NONE',  ( -32.97913964219446115, 1511.187213306747708, 197.9697544589750464 ) ) ;
#106691 = CARTESIAN_POINT ( 'NONE',  ( 11.24138533720000055, 1422.409861511610188, 204.1338940524489942 ) ) ;
#106692 = DIRECTION ( 'NONE',  ( -5.980589973904019347E-17, 1.000000000000000000, -1.736889445713099699E-16 ) ) ;
#106694 = CARTESIAN_POINT ( 'NONE',  ( 21.54116136312511998, 1523.382868172863709, 183.9310736446955445 ) ) ;
#106693 = CARTESIAN_POINT ( 'NONE',  ( -1.708747662384999977, 1517.213554313520035, 216.0740123525270064 ) ) ;
#106695 = CARTESIAN_POINT ( 'NONE',  ( 2.780672902370000088, 1460.407737242989924, 228.5579519583990020 ) ) ;
#106696 = CARTESIAN_POINT ( 'NONE',  ( 11.37695908739150141, 1470.749029468129947, 208.3696375387830244 ) ) ;
#106697 = EDGE_LOOP ( 'NONE', ( #75293, #54686, #16191, #42908 ) ) ;
#106698 = CARTESIAN_POINT ( 'NONE',  ( 7.716252052974999387, 1516.810037859429940, 202.1795012402670011 ) ) ;
#106699 = CARTESIAN_POINT ( 'NONE',  ( -16.20130421256499886, 1512.842772631639946, 220.3734026763669931 ) ) ;
#106700 = EDGE_LOOP ( 'NONE', ( #107203, #15058, #10380, #19740 ) ) ;
#106701 = CARTESIAN_POINT ( 'NONE',  ( 18.79226589730000185, 1456.307606824690083, 213.7887498653890077 ) ) ;
#106702 = CIRCLE ( 'NONE', #13729, 2.000048766321055993 ) ;
#106703 = B_SPLINE_CURVE_WITH_KNOTS ( 'NONE', 3,
 ( #29203, #89102, #80710, #4556 ),
 .UNSPECIFIED., .F., .F.,
 ( 4, 4 ),
 ( 7.189088551655727393E-14, 0.002384643111680536873 ),
 .UNSPECIFIED. ) ;
#106704 = CARTESIAN_POINT ( 'NONE',  ( 4.706522373909999502, 1426.134490744389950, 210.8435422850390069 ) ) ;
#106705 = CARTESIAN_POINT ( 'NONE',  ( 8.973660471278915196, 1425.007957488622651, 195.6894122325922467 ) ) ;
#106706 = CARTESIAN_POINT ( 'NONE',  ( 1.531308761570000065, 1442.248940191690053, 218.5680284645490019 ) ) ;
#106707 = CARTESIAN_POINT ( 'NONE',  ( -27.68503987499639862, 1509.816463871160067, 201.0194270758620121 ) ) ;
#106708 = CARTESIAN_POINT ( 'NONE',  ( -2.499999999959999997, 1447.637843966430182, 170.5315787469979796 ) ) ;
#106709 = CARTESIAN_POINT ( 'NONE',  ( -20.34455516050000057, 1426.954645372529967, 221.8177795676979827 ) ) ;
#106710 = CARTESIAN_POINT ( 'NONE',  ( -20.44161166330000157, 1485.241385972889930, 206.1012198832090121 ) ) ;
#106711 = CARTESIAN_POINT ( 'NONE',  ( -107.9045857630000000, 1389.125896740649978, 298.5296598085590176 ) ) ;
#106712 = CARTESIAN_POINT ( 'NONE',  ( 15.94624203079999702, 1509.299608116730042, 185.9453027169979862 ) ) ;
#106714 = CARTESIAN_POINT ( 'NONE',  ( -17.30083075200003151, 1433.673648912240196, 216.7777474620279463 ) ) ;
#106713 = CARTESIAN_POINT ( 'NONE',  ( -0.03277866176829110495, 1410.296501491089884, 233.2237263845800044 ) ) ;
#106715 = CARTESIAN_POINT ( 'NONE',  ( 0.4151546846839010985, 1522.906561336850928, 244.9330574173806951 ) ) ;
#106716 = ORIENTED_EDGE ( 'NONE', *, *, #28880, .T. ) ;
#106717 = DIRECTION ( 'NONE',  ( 0.06162841671618448508, -0.9961946980917499861, -0.06162841671618445039 ) ) ;
#106718 = CARTESIAN_POINT ( 'NONE',  ( -16.65377040190000102, 1508.454794883789873, 213.7212185660889929 ) ) ;
#106719 = FACE_OUTER_BOUND ( 'NONE', #72123, .T. ) ;
#106720 = CARTESIAN_POINT ( 'NONE',  ( 11.26363633646609941, 1470.487396938490065, 207.5510992998169968 ) ) ;
#106721 = CARTESIAN_POINT ( 'NONE',  ( -3.378095328389999707, 1485.354467027690134, 197.6993834011990145 ) ) ;
#106722 = CARTESIAN_POINT ( 'NONE',  ( -18.64460733019999950, 1509.564144422130084, 231.7099517930980142 ) ) ;
#106723 = CARTESIAN_POINT ( 'NONE',  ( -2.570812331889315683, 1525.317349363550647, 241.4588417251712826 ) ) ;
#106724 = AXIS2_PLACEMENT_3D ( 'NONE', #87566, #11948, #80259 ) ;
#106725 = CARTESIAN_POINT ( 'NONE',  ( -12.92150563921792461, 1442.903198327644077, 186.4433106084745759 ) ) ;
#106726 = CARTESIAN_POINT ( 'NONE',  ( -24.68077630836099701, 1437.736159206269804, 210.5119845322900005 ) ) ;
#106727 = CARTESIAN_POINT ( 'NONE',  ( 4.730876151940029750, 1493.686648256609942, 219.2027333063510071 ) ) ;
#106728 = CARTESIAN_POINT ( 'NONE',  ( -21.26809933518700291, 1485.919115173290038, 201.7808441828850050 ) ) ;
#106729 = CARTESIAN_POINT ( 'NONE',  ( -15.45647355988487881, 1415.677402202029953, 209.5466896407415618 ) ) ;
#106730 = EDGE_CURVE ( 'NONE', #89451, #7508, #79205, .T. ) ;
#106731 = CARTESIAN_POINT ( 'NONE',  ( 24.86520790779999857, 1436.144674809589787, 137.8610291600980133 ) ) ;
#106732 = CARTESIAN_POINT ( 'NONE',  ( 6.365104321110000463, 1429.227105708690033, 215.6823107352090005 ) ) ;
#106734 = ORIENTED_EDGE ( 'NONE', *, *, #67197, .F. ) ;
#106733 = DIRECTION ( 'NONE',  ( 1.224646799147353207E-16, -1.836970198721029688E-16, -1.000000000000000000 ) ) ;
#106735 = CARTESIAN_POINT ( 'NONE',  ( 29.99620953741488449, 1526.382868172863937, 198.4974435154498735 ) ) ;
#106736 = EDGE_CURVE ( 'NONE', #31004, #54528, #8361, .T. ) ;
#106737 = CARTESIAN_POINT ( 'NONE',  ( 14.86941678424950020, 1514.013728164709846, 223.9821045949209974 ) ) ;
#106738 = ORIENTED_EDGE ( 'NONE', *, *, #62580, .F. ) ;
#106739 = VERTEX_POINT ( 'NONE', #48673 ) ;
#106740 = EDGE_CURVE ( 'NONE', #44756, #237, #67967, .T. ) ;
#106741 = CARTESIAN_POINT ( 'NONE',  ( 204.2714532754875449, 1524.382868172863937, 223.7095399770875304 ) ) ;
#106742 = CARTESIAN_POINT ( 'NONE',  ( 13.28728145560000051, 1508.680272370929970, 233.3924286979980138 ) ) ;
#106743 = CARTESIAN_POINT ( 'NONE',  ( -8.359385560594374098, 1382.870626080099782, 199.9003235427358334 ) ) ;
#106745 = CARTESIAN_POINT ( 'NONE',  ( -27.90885395439999783, 1457.406260642230109, 250.2249407924980176 ) ) ;
#106744 = CARTESIAN_POINT ( 'NONE',  ( 29.95045141167489433, 1419.540663059560529, 269.4702688073739409 ) ) ;
#106746 = CARTESIAN_POINT ( 'NONE',  ( -20.32989725279999860, 1499.115995715829968, 190.6432919934979964 ) ) ;
#106747 = CARTESIAN_POINT ( 'NONE',  ( -11.14671480820000049, 1434.019355918939937, 151.6529837240979930 ) ) ;
#106748 = CARTESIAN_POINT ( 'NONE',  ( 0.000000000000000000, 1420.119835273649869, 209.1218459616989946 ) ) ;
#106749 = CARTESIAN_POINT ( 'NONE',  ( -19.06723480449999997, 1485.490520234629912, 189.6150008477979725 ) ) ;
#106750 = AXIS2_PLACEMENT_3D ( 'NONE', #109735, #34678, #50945 ) ;
#106751 = CARTESIAN_POINT ( 'NONE',  ( 8.616434899906300515, 1465.329448497550175, 213.9433383265620137 ) ) ;
#106752 = CARTESIAN_POINT ( 'NONE',  ( -2.372478608334043670, 1522.644714754858114, 243.3440112565160973 ) ) ;
#106753 = CARTESIAN_POINT ( 'NONE',  ( 0.3731951684343629561, 1515.150224411170029, 213.4490576343089856 ) ) ;
#106754 = DIRECTION ( 'NONE',  ( 1.000000000000000000, 0.000000000000000000, 0.000000000000000000 ) ) ;
#106755 = CARTESIAN_POINT ( 'NONE',  ( -11.02097544798480122, 1480.400473981879941, 213.2717396774600331 ) ) ;
#106756 = CARTESIAN_POINT ( 'NONE',  ( 0.05319939914973582928, 1362.392533002544042, 209.6218459617148824 ) ) ;
#106757 = CARTESIAN_POINT ( 'NONE',  ( 31.95643112691193366, 1526.329757971585877, 201.5629546934984262 ) ) ;
#106759 = ORIENTED_EDGE ( 'NONE', *, *, #24815, .T. ) ;
#106758 = CARTESIAN_POINT ( 'NONE',  ( 1.452038864671010018E-08, 1407.324376059620135, 264.3779639133369983 ) ) ;
#106760 = EDGE_LOOP ( 'NONE', ( #62648, #89189, #30340 ) ) ;
#106761 = CARTESIAN_POINT ( 'NONE',  ( -11.86387080393020099, 1432.180192430769921, 149.9801236230049710 ) ) ;
#106762 = CARTESIAN_POINT ( 'NONE',  ( -22.15338394760000185, 1485.967612886890038, 217.2877321619890267 ) ) ;
#106763 = CARTESIAN_POINT ( 'NONE',  ( -34.52598909179999964, 1461.996329814830005, 270.2126011320979728 ) ) ;
#106764 = CARTESIAN_POINT ( 'NONE',  ( -23.92569337129095786, 1435.916919288760027, 211.2787512685800095 ) ) ;
#106765 = CARTESIAN_POINT ( 'NONE',  ( 6.446325585610000353, 1432.345375419369930, 154.6647257196979979 ) ) ;
#106766 = CARTESIAN_POINT ( 'NONE',  ( 33.91361689144800096, 1451.728768045109973, 134.7154145114139965 ) ) ;
#106767 = CARTESIAN_POINT ( 'NONE',  ( 0.2064069609369219849, 1452.175221133040168, 183.1192452647970015 ) ) ;
#106768 = CARTESIAN_POINT ( 'NONE',  ( -12.41153351569999863, 1420.834873760830078, 229.8963213914979917 ) ) ;
#106769 = CARTESIAN_POINT ( 'NONE',  ( -16.17568633703940151, 1459.146939663510011, 230.7169128052520080 ) ) ;
#106770 = CARTESIAN_POINT ( 'NONE',  ( -6.384611937859999919, 1459.149684699189947, 217.3122905540589898 ) ) ;
#106771 = CARTESIAN_POINT ( 'NONE',  ( 9.930155807529674306, 1362.158223026690166, 210.6218459617030021 ) ) ;
#106772 = CARTESIAN_POINT ( 'NONE',  ( -27.31148204492600229, 1412.934667530339993, 269.0113653186659803 ) ) ;
#106773 = ORIENTED_EDGE ( 'NONE', *, *, #2138, .F. ) ;
#106774 = CARTESIAN_POINT ( 'NONE',  ( -3.537598770401839676, 1495.725909260799881, 181.4625765259970080 ) ) ;
#106775 = EDGE_LOOP ( 'NONE', ( #20705, #95355, #54174, #93574 ) ) ;
#106776 = AXIS2_PLACEMENT_3D ( 'NONE', #55783, #56312, #13170 ) ;
#106777 = EDGE_LOOP ( 'NONE', ( #109634, #59628, #56725, #53975 ) ) ;
#106778 = CARTESIAN_POINT ( 'NONE',  ( -3.251611363945000388, 1516.779243033999819, 211.4202154400570066 ) ) ;
#106779 = FACE_OUTER_BOUND ( 'NONE', #59482, .T. ) ;
#106781 = CARTESIAN_POINT ( 'NONE',  ( -20.61553203140000434, 1508.364800381330042, 190.3717489592980030 ) ) ;
#106780 = CARTESIAN_POINT ( 'NONE',  ( -5.771149113014999443, 1516.616791731099966, 211.6102065995370083 ) ) ;
#106782 = CARTESIAN_POINT ( 'NONE',  ( -11.77258770480000116, 1440.429812290090013, 187.7126807368979939 ) ) ;
#106783 = AXIS2_PLACEMENT_3D ( 'NONE', #17893, #28532, #77832 ) ;
#106784 = CARTESIAN_POINT ( 'NONE',  ( -15.97031451047940109, 1470.475814234120207, 228.8250343533829891 ) ) ;
#106785 = ORIENTED_EDGE ( 'NONE', *, *, #57733, .T. ) ;
#106786 = CARTESIAN_POINT ( 'NONE',  ( -26.80688184059999912, 1436.287257724250139, 136.6586291973980281 ) ) ;
#106787 = CARTESIAN_POINT ( 'NONE',  ( -4.617490504904999682, 1516.685667699390024, 201.7969310139470167 ) ) ;
#106788 = ADVANCED_FACE ( 'NONE', ( #13924 ), #48111, .T. ) ;
#106789 = CARTESIAN_POINT ( 'NONE',  ( 9.600863931830000197, 1470.542903070589773, 212.2537315410889676 ) ) ;
#106790 = CARTESIAN_POINT ( 'NONE',  ( -16.59437507809930068, 1384.525787470290197, 200.9191608993760099 ) ) ;
#106791 = CARTESIAN_POINT ( 'NONE',  ( -19.13958158392089715, 1411.674646606650185, 270.3886806677189725 ) ) ;
#106792 = CARTESIAN_POINT ( 'NONE',  ( -1.470421131539999982, 1428.420680932830237, 91.31218443469779800 ) ) ;
#106793 = CARTESIAN_POINT ( 'NONE',  ( 9.338308684742390398, 1435.342874469600019, 208.2407783485550112 ) ) ;
#106795 = EDGE_LOOP ( 'NONE', ( #76542, #46994, #4217, #99350, #102651 ) ) ;
#106794 = CARTESIAN_POINT ( 'NONE',  ( -9.351945459739999578, 1366.519103298159735, 207.6218459616989946 ) ) ;
#106796 = ORIENTED_EDGE ( 'NONE', *, *, #38349, .T. ) ;
#106797 = CARTESIAN_POINT ( 'NONE',  ( 36.90008876993807263, 1461.061631172933403, 269.2062195636714250 ) ) ;
#106798 = CARTESIAN_POINT ( 'NONE',  ( 10.95098205620359977, 1471.837422849929908, 212.3987392730099657 ) ) ;
#106799 = CARTESIAN_POINT ( 'NONE',  ( -20.68580785760000040, 1486.599620265689964, 210.1129637272439936 ) ) ;
#106800 = FACE_OUTER_BOUND ( 'NONE', #104875, .T. ) ;
#106801 = CIRCLE ( 'NONE', #37127, 1.530931026689996699 ) ;
#106802 = CARTESIAN_POINT ( 'NONE',  ( -3.255809902135000211, 1516.837969789639828, 209.8792719553279937 ) ) ;
#106803 = CARTESIAN_POINT ( 'NONE',  ( -18.67445339878970145, 1416.007771869960152, 207.5718808771989927 ) ) ;
#106804 = CARTESIAN_POINT ( 'NONE',  ( -18.94569428040000147, 1430.795004337129967, 224.8243481170979976 ) ) ;
#106805 = CARTESIAN_POINT ( 'NONE',  ( -14.76826616709999840, 1426.820312322130121, 221.7083327112979987 ) ) ;
#106806 = CARTESIAN_POINT ( 'NONE',  ( 12.39598156289999942, 1416.274718424630009, 223.4274628688980044 ) ) ;
#106807 = CARTESIAN_POINT ( 'NONE',  ( 7.985842358304999777, 1511.355055856599847, 205.0854651845669991 ) ) ;
#106808 = CARTESIAN_POINT ( 'NONE',  ( 3.445685077385000294, 1516.778761582560037, 206.6297153089269898 ) ) ;
#106809 = ORIENTED_EDGE ( 'NONE', *, *, #11168, .T. ) ;
#106810 = CARTESIAN_POINT ( 'NONE',  ( 4.487249772970000272, 1509.038615934189920, 209.1218459625970070 ) ) ;
#106811 = CARTESIAN_POINT ( 'NONE',  ( -2.446740418831741870, 1516.554415856173591, 202.0292846036045944 ) ) ;
#106812 = ORIENTED_EDGE ( 'NONE', *, *, #46140, .F. ) ;
#106813 = CARTESIAN_POINT ( 'NONE',  ( -11.15120484728000072, 1517.151704408390060, 198.0995572319588405 ) ) ;
#106814 = CARTESIAN_POINT ( 'NONE',  ( -18.89959486414000267, 1416.839692127460012, 207.5749783441650038 ) ) ;
#106815 = CARTESIAN_POINT ( 'NONE',  ( 13.79060599709999835, 1416.547221146729953, 196.3475826081979960 ) ) ;
#106816 = CARTESIAN_POINT ( 'NONE',  ( -9.092793663155459782, 1384.840586518749888, 199.9433582416939998 ) ) ;
#106817 = CARTESIAN_POINT ( 'NONE',  ( 19.28368759869999849, 1410.509001784329939, 195.8671163398980184 ) ) ;
#106818 = CARTESIAN_POINT ( 'NONE',  ( 16.68463233076019492, 1445.052233488289176, 162.0935120523188289 ) ) ;
#106819 = CARTESIAN_POINT ( 'NONE',  ( 10.10004869885234058, 1422.222932908421171, 137.0999999980978430 ) ) ;
#106820 = DIRECTION ( 'NONE',  ( 0.000000000000000000, 0.000000000000000000, -1.000000000000000000 ) ) ;
#106821 = CARTESIAN_POINT ( 'NONE',  ( 30.61443310214658453, 1523.462669333492840, 221.8243310972552536 ) ) ;
#106822 = CARTESIAN_POINT ( 'NONE',  ( 4.241818682233510884, 1441.427818084279806, 162.5168752623719968 ) ) ;
#106823 = ADVANCED_FACE ( 'NONE', ( #64921 ), #82249, .T. ) ;
#106824 = AXIS2_PLACEMENT_3D ( 'NONE', #85480, #42960, #86603 ) ;
#106825 = CARTESIAN_POINT ( 'NONE',  ( 2.500000000000300204, 1439.152015563370014, 158.1892132547360177 ) ) ;
#106826 = CARTESIAN_POINT ( 'NONE',  ( -6.550389470255000290, 1516.755758396839838, 214.1281755516169767 ) ) ;
#106827 = ORIENTED_EDGE ( 'NONE', *, *, #83746, .T. ) ;
#106828 = CARTESIAN_POINT ( 'NONE',  ( 7.710405941315919165, 1516.586783862359880, 207.7425835133209944 ) ) ;
#106829 = CARTESIAN_POINT ( 'NONE',  ( -5.062212390315069754, 1474.342205398819942, 198.8731691453010058 ) ) ;
#106830 = CARTESIAN_POINT ( 'NONE',  ( -2.696187843830000208, 1448.602801166340214, 184.2458148013979837 ) ) ;
#106831 = CARTESIAN_POINT ( 'NONE',  ( -11.43480974721719967, 1425.837050099640010, 122.9429429844429933 ) ) ;
#106832 = CARTESIAN_POINT ( 'NONE',  ( -38.37365570824950112, 1448.472291891780060, 136.4276078884599883 ) ) ;
#106833 = CARTESIAN_POINT ( 'NONE',  ( 11.60004869885203682, 1426.233066092331683, 138.1607928833331584 ) ) ;
#106834 = CARTESIAN_POINT ( 'NONE',  ( 2.514509550398654536, 1417.714408133527741, 233.7630435220257823 ) ) ;
#106835 = CARTESIAN_POINT ( 'NONE',  ( -2.500000000000000000, 1419.649642134729902, 147.2763244958979953 ) ) ;
#106836 = CARTESIAN_POINT ( 'NONE',  ( -107.1138176589999915, 1379.788324461719867, 299.4659512524589786 ) ) ;
#106837 = CARTESIAN_POINT ( 'NONE',  ( -39.27028727949999620, 1458.780602943529857, 269.1469756859979725 ) ) ;
#106838 = CARTESIAN_POINT ( 'NONE',  ( 30.82334546788949936, 1440.913060384559913, 240.8675706011379987 ) ) ;
#106839 = CARTESIAN_POINT ( 'NONE',  ( -110.0632053599999978, 1385.194747628709820, 296.9590720091590015 ) ) ;
#106840 = CARTESIAN_POINT ( 'NONE',  ( 11.74145575222949844, 1499.920360182230070, 205.7526641877259976 ) ) ;
#106841 = VERTEX_POINT ( 'NONE', #6092 ) ;
#106842 = CARTESIAN_POINT ( 'NONE',  ( 12.53380498098208840, 1442.773887284840384, 150.7612718761199062 ) ) ;
#106843 = CIRCLE ( 'NONE', #106776, 1.999999999999912514 ) ;
#106844 = DIRECTION ( 'NONE',  ( 0.000000000000000000, 0.000000000000000000, -1.000000000000000000 ) ) ;
#106845 = CARTESIAN_POINT ( 'NONE',  ( -0.6369869090064108619, 1408.970540970598222, 186.3721633967661830 ) ) ;
#106846 = CARTESIAN_POINT ( 'NONE',  ( 6.501609782144663896, 1522.051704408389924, 217.4228972380528262 ) ) ;
#106847 = EDGE_CURVE ( 'NONE', #18777, #53857, #75151, .T. ) ;
#106848 = AXIS2_PLACEMENT_3D ( 'NONE', #2119, #68767, #27290 ) ;
#106849 = CARTESIAN_POINT ( 'NONE',  ( -16.73628186595804479, 1526.382868172864164, 234.1845039693045862 ) ) ;
#106850 = CARTESIAN_POINT ( 'NONE',  ( -16.97760529929999862, 1508.233635166930071, 230.2235885397980155 ) ) ;
#106851 = CARTESIAN_POINT ( 'NONE',  ( -43.05153967746429799, 1383.823344776070144, 247.3619861808770111 ) ) ;
#106852 = EDGE_CURVE ( 'NONE', #65282, #35589, #95161, .T. ) ;
#106853 = CARTESIAN_POINT ( 'NONE',  ( -4.410745965304349703, 1508.610338743689908, 205.2563625205500273 ) ) ;
#106854 = CARTESIAN_POINT ( 'NONE',  ( -16.06428792994629973, 1414.913060387329779, 209.3174441339999987 ) ) ;
#106855 = CARTESIAN_POINT ( 'NONE',  ( -6.252266492314999979, 1511.741868877540128, 200.3335294429169835 ) ) ;
#106856 = FACE_OUTER_BOUND ( 'NONE', #59196, .T. ) ;
#106857 = EDGE_CURVE ( 'NONE', #53391, #79801, #84074, .T. ) ;
#106859 = ORIENTED_EDGE ( 'NONE', *, *, #80949, .T. ) ;
#106858 = CARTESIAN_POINT ( 'NONE',  ( -4.832616828004995924, 1508.551704408610021, 212.6094309338623418 ) ) ;
#106860 = CARTESIAN_POINT ( 'NONE',  ( -1.216452466170000024, 1450.942157347929879, 182.7783913332980035 ) ) ;
#106861 = CARTESIAN_POINT ( 'NONE',  ( -13.70246959700000033, 1380.890122814619872, 216.8472876221590013 ) ) ;
#106862 = EDGE_CURVE ( 'NONE', #50172, #32360, #91193, .T. ) ;
#106863 = CARTESIAN_POINT ( 'NONE',  ( 2.487935123020000194, 1508.551704408389924, 204.1347675455010062 ) ) ;
#106865 = EDGE_LOOP ( 'NONE', ( #54214, #57313, #4676, #85902, #105591, #78707 ) ) ;
#106864 = CARTESIAN_POINT ( 'NONE',  ( -18.18162401578809906, 1416.230844595159851, 208.9105673229449849 ) ) ;
#106866 = CARTESIAN_POINT ( 'NONE',  ( 10.75634779605130120, 1451.137958617219965, 190.3409307970749751 ) ) ;
#106867 = ORIENTED_EDGE ( 'NONE', *, *, #28546, .T. ) ;
#106868 = EDGE_CURVE ( 'NONE', #11573, #37685, #40798, .T. ) ;
#106869 = CARTESIAN_POINT ( 'NONE',  ( -8.546537168396879380, 1387.684766926490056, 218.1936297957030035 ) ) ;
#106870 = CARTESIAN_POINT ( 'NONE',  ( -18.11157384430000050, 1509.545530482630056, 231.7129783355979669 ) ) ;
#106871 = CARTESIAN_POINT ( 'NONE',  ( 3.487592431261229642, 1509.038615938009798, 213.6090957240379851 ) ) ;
#106873 = ADVANCED_FACE ( 'NONE', ( #52529 ), #69340, .T. ) ;
#106872 = CARTESIAN_POINT ( 'NONE',  ( -4.885449122210000716, 1463.524425562389752, 200.4816631501890072 ) ) ;
#106874 = DIRECTION ( 'NONE',  ( -0.6736849260863841948, 0.000000000000000000, 0.7390186874254148774 ) ) ;
#106875 = CARTESIAN_POINT ( 'NONE',  ( 2.470168522032202940, 1523.481610118012441, 242.8787258960491897 ) ) ;
#106876 = AXIS2_PLACEMENT_3D ( 'NONE', #73252, #65421, #81088 ) ;
#106877 = DIRECTION ( 'NONE',  ( -0.8775825618903725367, 0.000000000000000000, -0.4794255386042032829 ) ) ;
#106878 = CARTESIAN_POINT ( 'NONE',  ( 8.731332846349999954, 1459.404707344790040, 227.0651519182989944 ) ) ;
#106879 = DIRECTION ( 'NONE',  ( -1.577721810442025012E-32, -1.000000000000000000, 6.123233995736769734E-17 ) ) ;
#106880 = CARTESIAN_POINT ( 'NONE',  ( -18.31748438839999693, 1452.000482346729996, 190.7950199775980025 ) ) ;
#106881 = CARTESIAN_POINT ( 'NONE',  ( -68.77339414690014507, 1379.748013015986317, 280.2450576337279813 ) ) ;
#106882 = DIRECTION ( 'NONE',  ( -9.500021872036790217E-47, 1.000000000000000000, -1.836970198721029688E-16 ) ) ;
#106883 = ORIENTED_EDGE ( 'NONE', *, *, #33158, .T. ) ;
#106884 = VERTEX_POINT ( 'NONE', #44128 ) ;
#106886 = EDGE_CURVE ( 'NONE', #26163, #73589, #48074, .T. ) ;
#106885 = CARTESIAN_POINT ( 'NONE',  ( 19.33418355719911474, 1523.342713519622976, 239.2327152390723484 ) ) ;
#106887 = CARTESIAN_POINT ( 'NONE',  ( -2.581689387682173376, 1419.606464184852484, 137.0999999981000883 ) ) ;
#106888 = CARTESIAN_POINT ( 'NONE',  ( -12.48312717700000007, 1434.436312747890042, 149.9522253733979937 ) ) ;
#106889 = B_SPLINE_CURVE_WITH_KNOTS ( 'NONE', 5,
 ( #6556, #107358, #6003, #73781, #15482, #22222, #101142, #39611, #7651, #66495, #100601, #58624, #92755, #56420, #90551 ),
 .UNSPECIFIED., .F., .F.,
 ( 6, 3, 3, 3, 6 ),
 ( 0.000000000000000000, 0.3703688121675461908, 0.5769812935202122128, 0.8426640375833164276, 1.000000000000000000 ),
 .UNSPECIFIED. ) ;
#106890 = CARTESIAN_POINT ( 'NONE',  ( -5.215130879758570953E-10, 1468.939591304350188, 251.0785144346289712 ) ) ;
#106891 = CARTESIAN_POINT ( 'NONE',  ( -20.38352471697730195, 1500.853033034210057, 190.5928454434599928 ) ) ;
#106892 = FACE_OUTER_BOUND ( 'NONE', #30652, .T. ) ;
#106893 = CARTESIAN_POINT ( 'NONE',  ( -109.4097255559999979, 1385.247472506640179, 311.2758024732589774 ) ) ;
#106894 = ADVANCED_FACE ( 'NONE', ( #36264 ), #92774, .T. ) ;
#106895 = CARTESIAN_POINT ( 'NONE',  ( -7.670153693721269761, 1511.304111283970087, 215.1254345037010012 ) ) ;
#106896 = CARTESIAN_POINT ( 'NONE',  ( -9.516636888329999877, 1366.309137899869938, 207.6218459616989946 ) ) ;
#106897 = PLANE ( 'NONE',  #101919 ) ;
#106898 = DIRECTION ( 'NONE',  ( 0.000000000000000000, 1.000000000000000000, 0.000000000000000000 ) ) ;
#106899 = EDGE_CURVE ( 'NONE', #75707, #30117, #17867, .T. ) ;
#106900 = CARTESIAN_POINT ( 'NONE',  ( -1.137296688934999800, 1516.908147884120126, 207.4199954749970232 ) ) ;
#106901 = CARTESIAN_POINT ( 'NONE',  ( -9.033366821045200723, 1447.304030695519941, 212.0885462952919909 ) ) ;
#106902 = CARTESIAN_POINT ( 'NONE',  ( 11.94888771486709977, 1433.583934366519998, 150.1820132112760007 ) ) ;
#106903 = CARTESIAN_POINT ( 'NONE',  ( -13.42182309979999921, 1435.162926645730067, 149.8212854273980099 ) ) ;
#106904 = CARTESIAN_POINT ( 'NONE',  ( -8.863675502250000449, 1385.133167759019898, 218.6777116865889923 ) ) ;
#106905 = CYLINDRICAL_SURFACE ( 'NONE', #31893, 0.4999999999999909517 ) ;
#106906 = CARTESIAN_POINT ( 'NONE',  ( 19.32254953540159903, 1466.487181286699979, 226.4358010736329732 ) ) ;
#106907 = LINE ( 'NONE', #45926, #56891 ) ;
#106908 = EDGE_CURVE ( 'NONE', #43261, #107214, #50050, .T. ) ;
#106909 = ORIENTED_EDGE ( 'NONE', *, *, #28761, .T. ) ;
#106910 = CARTESIAN_POINT ( 'NONE',  ( 28.66942460980000007, 1426.582479900129783, 248.2467662509980073 ) ) ;
#106911 = CARTESIAN_POINT ( 'NONE',  ( -28.24200347660000077, 1508.135538546330281, 208.7967122801030087 ) ) ;
#106913 = CARTESIAN_POINT ( 'NONE',  ( 13.15726447020000123, 1414.996442546130083, 197.7616625855980033 ) ) ;
#106912 = CARTESIAN_POINT ( 'NONE',  ( 1.515335126600000137, 1458.417426270730175, 183.2389660611979991 ) ) ;
#106914 = CARTESIAN_POINT ( 'NONE',  ( 21.27157138040592343, 1506.426094406462198, 203.5633718702692079 ) ) ;
#106915 = CARTESIAN_POINT ( 'NONE',  ( -1.271605103970000069E-07, 1420.650940017329958, 220.7242732315979765 ) ) ;
#106916 = CARTESIAN_POINT ( 'NONE',  ( 1.969630537620000066, 1485.776228655490058, 220.0997983293990217 ) ) ;
#106917 = CARTESIAN_POINT ( 'NONE',  ( -4.994701136659999818, 1391.710704960489920, 214.4888430591489907 ) ) ;
#106918 = CARTESIAN_POINT ( 'NONE',  ( -18.90749324119999741, 1416.833018152629847, 208.2176376215240055 ) ) ;
#106919 = EDGE_LOOP ( 'NONE', ( #84224, #62525, #1153, #100829 ) ) ;
#106920 = CARTESIAN_POINT ( 'NONE',  ( -2.500000000000000000, 1432.344429588900084, 157.4943015532979871 ) ) ;
#106921 = DIRECTION ( 'NONE',  ( -0.9455185755993178454, 0.000000000000000000, 0.3255681544571537578 ) ) ;
#106922 = CARTESIAN_POINT ( 'NONE',  ( 2.919540490770000218, 1509.015012987830232, 238.5603143811979976 ) ) ;
#106923 = ORIENTED_EDGE ( 'NONE', *, *, #77087, .T. ) ;
#106924 = ORIENTED_EDGE ( 'NONE', *, *, #24375, .T. ) ;
#106925 = CIRCLE ( 'NONE', #96152, 0.9999999999999976685 ) ;
#106926 = CARTESIAN_POINT ( 'NONE',  ( -6.355004503990000053, 1384.784618782699908, 199.7177247563389813 ) ) ;
#106927 = CARTESIAN_POINT ( 'NONE',  ( -23.03290791463370013, 1409.747221716589820, 208.9467762737129988 ) ) ;
#106928 = ORIENTED_EDGE ( 'NONE', *, *, #20324, .F. ) ;
#106929 = CARTESIAN_POINT ( 'NONE',  ( 3.487585214244389942, 1508.551704408389924, 204.2892321559630204 ) ) ;
#106930 = CARTESIAN_POINT ( 'NONE',  ( 15.72751745975079984, 1517.051704408389924, 206.8816388537309763 ) ) ;
#106931 = VECTOR ( 'NONE', #89952, 1000.000000000000114 ) ;
#106932 = CIRCLE ( 'NONE', #13967, 2.000000000000003553 ) ;
#106933 = CARTESIAN_POINT ( 'NONE',  ( -9.739009285419999884, 1489.054442968930061, 233.7183489316979887 ) ) ;
#106934 = EDGE_CURVE ( 'NONE', #102270, #79909, #29712, .T. ) ;
#106935 = CARTESIAN_POINT ( 'NONE',  ( 16.69297358003969123, 1526.382868172864164, 234.5473741529541201 ) ) ;
#106936 = VERTEX_POINT ( 'NONE', #31713 ) ;
#106937 = AXIS2_PLACEMENT_3D ( 'NONE', #19154, #79114, #88613 ) ;
#106938 = CARTESIAN_POINT ( 'NONE',  ( 11.63663615270000129, 1425.864876078829866, 144.1644678884979953 ) ) ;
#106939 = CARTESIAN_POINT ( 'NONE',  ( -12.51099735422430115, 1416.825783990419950, 222.1450751212599926 ) ) ;
#106940 = EDGE_CURVE ( 'NONE', #80100, #19422, #69808, .T. ) ;
#106941 = CARTESIAN_POINT ( 'NONE',  ( -0.1681676274470000065, 1420.473121337229941, 182.7663689088979879 ) ) ;
#106942 =( BOUNDED_CURVE ( )  B_SPLINE_CURVE ( 3, ( #64946, #48697, #31316, #98521 ),
 .UNSPECIFIED., .F., .F. ) 
 B_SPLINE_CURVE_WITH_KNOTS ( ( 4, 4 ),
 ( 0.3089224742796055079, 0.9578869033099139951 ),
 .UNSPECIFIED. ) 
 CURVE ( )  GEOMETRIC_REPRESENTATION_ITEM ( )  RATIONAL_B_SPLINE_CURVE ( ( 1.000000000000000000, 0.9652106218856630893, 0.9652106218856630893, 1.000000000000000000 ) ) 
 REPRESENTATION_ITEM ( '' )  );
#106943 = CARTESIAN_POINT ( 'NONE',  ( -7.333070173014999860, 1516.955859323880077, 203.3428461583270064 ) ) ;
#106944 = ORIENTED_EDGE ( 'NONE', *, *, #69262, .T. ) ;
#106945 = CARTESIAN_POINT ( 'NONE',  ( 9.188387156589639559, 1482.188622616660041, 216.5467321156359901 ) ) ;
#106946 = CARTESIAN_POINT ( 'NONE',  ( 13.33831059585898160, 1443.295405362211341, 187.7819447126144325 ) ) ;
#106947 = ORIENTED_EDGE ( 'NONE', *, *, #51184, .T. ) ;
#106948 = ORIENTED_EDGE ( 'NONE', *, *, #20631, .T. ) ;
#106950 = B_SPLINE_CURVE_WITH_KNOTS ( 'NONE', 3,
 ( #104768, #35919, #61690, #62242, #105318, #61152, #95812, #63348, #52177, #53850, #97466, #52725, #87987, #11275, #10152, #9593, #1782, #105879, #45438, #29160, #13990, #20735, #29702, #90703, #47076, #12344, #63886, #3983, #46535, #72826, #89058, #74489, #22933, #90147, #106959, #38651, #30801, #57138, #30244, #38107, #13429, #64979, #47619, #72285, #82859, #21271, #81201, #22373, #89606, #54930, #5051, #81744, #56022, #39196, #107511, #73373, #80669, #5613 ),
 .UNSPECIFIED., .F., .F.,
 ( 4, 2, 2, 2, 2, 2, 2, 1, 2, 2, 1, 1, 1, 2, 2, 2, 2, 1, 1, 2, 2, 2, 2, 1, 2, 2, 2, 2, 2, 1, 2, 2, 4 ),
 ( 0.000000000000000000, 0.007812500000247135645, 0.01171875000047535587, 0.01562500000070357609, 0.02343750000116001653, 0.03125000000161645697, 0.04687500000205005457, 0.05468750000226685337, 0.05859375000237715403, 0.06250000000248745469, 0.09375000000158209557, 0.1093750000009845319, 0.1171875000006857570, 0.1210937500006842721, 0.1250000000006827872, 0.1875000000010061396, 0.2187500000011678158, 0.2343750000010602907, 0.2421875000010208778, 0.2460937500010011714, 0.2500000000009814372, 0.3750000000016789348, 0.4375000000019070301, 0.4687500000019094726, 0.4843750000018978152, 0.5000000000018861579, 0.6250000000012420065, 0.6875000000008204548, 0.7031250000008050227, 0.7187500000007895906, 0.7500000000007327472, 0.8750000000003663736, 1.000000000000000000 ),
 .UNSPECIFIED. ) ;
#106949 = CARTESIAN_POINT ( 'NONE',  ( -11.42598084535810088, 1481.698338076739901, 209.1408964386100138 ) ) ;
#106951 = CARTESIAN_POINT ( 'NONE',  ( -30.30078187369513643, 1526.189899547014875, 216.6986553323659166 ) ) ;
#106952 = CARTESIAN_POINT ( 'NONE',  ( 1.968522348845569869, 1498.935384250119796, 197.9561377214020013 ) ) ;
#106953 = CARTESIAN_POINT ( 'NONE',  ( 8.627556093114653990, 1521.551704408389696, 234.1780882150808623 ) ) ;
#106954 = CARTESIAN_POINT ( 'NONE',  ( 11.90642948233699983, 1452.497278707910027, 149.7233324945059678 ) ) ;
#106955 = CARTESIAN_POINT ( 'NONE',  ( 12.21937182940000000, 1420.343723557070007, 199.7692422141290081 ) ) ;
#106956 = CARTESIAN_POINT ( 'NONE',  ( -2.552257842228009999, 1476.146710473380153, 220.2966558116410170 ) ) ;
#106957 = CARTESIAN_POINT ( 'NONE',  ( -20.06562366400000030, 1485.934169092390221, 214.0282076738189971 ) ) ;
#106958 = CARTESIAN_POINT ( 'NONE',  ( -11.87502386937130083, 1433.007271227619867, 149.9804723889419904 ) ) ;
#106959 = CARTESIAN_POINT ( 'NONE',  ( 0.03684989003742775160, 1409.759860126017429, 233.0927588586005186 ) ) ;
#106961 = CARTESIAN_POINT ( 'NONE',  ( -105.9134890463210041, 1391.838458166060036, 304.2044508906599845 ) ) ;
#106960 = CARTESIAN_POINT ( 'NONE',  ( 30.00906687500045322, 1525.856064936156145, 197.1249949705187419 ) ) ;
#106962 = CARTESIAN_POINT ( 'NONE',  ( 12.38805570981969950, 1421.643760760719942, 207.4832281941469887 ) ) ;
#106963 = EDGE_CURVE ( 'NONE', #27637, #64407, #40421, .T. ) ;
#106964 = CIRCLE ( 'NONE', #58704, 7.842199003069996621 ) ;
#106965 = CARTESIAN_POINT ( 'NONE',  ( -24.03118224474849995, 1507.962100464060086, 222.3137046748230148 ) ) ;
#106966 = CARTESIAN_POINT ( 'NONE',  ( -7.809063951335000198, 1513.978875661330221, 201.9427188508670099 ) ) ;
#106967 = ORIENTED_EDGE ( 'NONE', *, *, #17506, .F. ) ;
#106968 = CARTESIAN_POINT ( 'NONE',  ( 11.09581607402950176, 1414.913057834409983, 221.9014645491780016 ) ) ;
#106969 = CARTESIAN_POINT ( 'NONE',  ( -16.70830179842720042, 1417.149226859160080, 207.3570905742490140 ) ) ;
#106970 = CARTESIAN_POINT ( 'NONE',  ( -103.2673858233620052, 1384.938584610499902, 311.1084624176889974 ) ) ;
#106971 = CARTESIAN_POINT ( 'NONE',  ( -8.372400094640001456, 1385.986562127730167, 199.8257561305989896 ) ) ;
#106972 = CARTESIAN_POINT ( 'NONE',  ( -14.93837044589999863, 1416.023439725270009, 212.9159407297890141 ) ) ;
#106974 = ORIENTED_EDGE ( 'NONE', *, *, #103466, .T. ) ;
#106973 = CARTESIAN_POINT ( 'NONE',  ( -17.59913612719639886, 1419.797432416249876, 206.6689813231369897 ) ) ;
#106975 = CARTESIAN_POINT ( 'NONE',  ( 16.81223226430000039, 1414.913060387329779, 210.6693098017280192 ) ) ;
#106976 = CARTESIAN_POINT ( 'NONE',  ( -0.8251472201360000591, 1438.194204504490017, 150.6035180695979818 ) ) ;
#106977 = ADVANCED_FACE ( 'NONE', ( #98918 ), #83065, .F. ) ;
#106978 = CARTESIAN_POINT ( 'NONE',  ( -7.454153900785907894, 1476.755908734740842, 216.3333321094707173 ) ) ;
#106979 = CARTESIAN_POINT ( 'NONE',  ( -19.38497611889999916, 1464.684217820690037, 212.9113686205490126 ) ) ;
#106980 = CARTESIAN_POINT ( 'NONE',  ( 14.58906255643499961, 1513.961173499609913, 225.5460952577670071 ) ) ;
#106981 = CARTESIAN_POINT ( 'NONE',  ( -17.15254157612201880, 1516.660421270687038, 223.0819975641380495 ) ) ;
#106982 = ADVANCED_FACE ( 'NONE', ( #15997 ), #75812, .T. ) ;
#106983 = CARTESIAN_POINT ( 'NONE',  ( -40.71506490407468704, 1443.618868061724470, 137.1015916554986802 ) ) ;
#106984 = CARTESIAN_POINT ( 'NONE',  ( -109.3697155611655489, 1387.313440419162134, 297.3840239876012674 ) ) ;
#106985 = CARTESIAN_POINT ( 'NONE',  ( 16.62404756210000301, 1422.111108379129973, 227.0758637081979998 ) ) ;
#106986 = CARTESIAN_POINT ( 'NONE',  ( 13.74310390781900004, 1517.151704408390060, 217.0905615615409943 ) ) ;
#106987 = CARTESIAN_POINT ( 'NONE',  ( 2.476450664134999702, 1516.843453247299749, 206.8221896160070230 ) ) ;
#106988 = CARTESIAN_POINT ( 'NONE',  ( 2.005628669607020242, 1474.789351304850015, 220.3635328066820023 ) ) ;
#106989 = CARTESIAN_POINT ( 'NONE',  ( -17.82265795360000027, 1409.535441317430241, 222.1575796720979952 ) ) ;
#106990 = CARTESIAN_POINT ( 'NONE',  ( 19.53759129830000063, 1435.323542146659975, 144.9538018687979957 ) ) ;
#106991 = CARTESIAN_POINT ( 'NONE',  ( -0.5630044002530000258, 1418.687151651130080, 227.8496307451979703 ) ) ;
#106992 = CARTESIAN_POINT ( 'NONE',  ( 5.381136289437809417, 1430.993983722579969, 154.5045433217829896 ) ) ;
#106993 = CARTESIAN_POINT ( 'NONE',  ( 12.78730314359999909, 1416.837309316629899, 222.9176234487979968 ) ) ;
#106994 = DIRECTION ( 'NONE',  ( 7.447054910797601740E-07, -0.9583089392864349021, -0.2857341017154824137 ) ) ;
#106995 = EDGE_CURVE ( 'NONE', #82569, #29284, #50727, .T. ) ;
#106996 = CARTESIAN_POINT ( 'NONE',  ( -36.54919900496939533, 1437.103027518239969, 136.4794237381429696 ) ) ;
#106997 = CARTESIAN_POINT ( 'NONE',  ( 0.2153128718845489786, 1454.373455522330005, 183.1944751942430116 ) ) ;
#106998 = CARTESIAN_POINT ( 'NONE',  ( -15.26494846990000021, 1409.446124134130059, 210.7631067400780012 ) ) ;
#106999 = CARTESIAN_POINT ( 'NONE',  ( -13.02322702410000055, 1416.825784011830137, 196.6108461443980104 ) ) ;
#107000 = CARTESIAN_POINT ( 'NONE',  ( -4.329448776040000446, 1515.064792882589927, 207.6699913460390121 ) ) ;
#107001 = ADVANCED_FACE ( 'NONE', ( #33915 ), #68109, .T. ) ;
#107002 = CARTESIAN_POINT ( 'NONE',  ( 0.9841710845998976609, 1484.601693631961325, 198.4550311835998855 ) ) ;
#107003 = CARTESIAN_POINT ( 'NONE',  ( 11.87957822189999924, 1433.311236608589979, 147.6243455281980061 ) ) ;
#107004 = CARTESIAN_POINT ( 'NONE',  ( -27.23873044170000313, 1435.448403991980058, 135.2737774014979948 ) ) ;
#107005 = CARTESIAN_POINT ( 'NONE',  ( 5.567438724339999645, 1439.949778329529863, 185.1713536890979981 ) ) ;
#107006 = VERTEX_POINT ( 'NONE', #6519 ) ;
#107007 = CARTESIAN_POINT ( 'NONE',  ( -1.322993174137927719, 1450.717402541238243, 181.8644873159974225 ) ) ;
#107008 = CARTESIAN_POINT ( 'NONE',  ( 4.570408800500000090, 1476.902228035989992, 198.8607389952989877 ) ) ;
#107009 = CARTESIAN_POINT ( 'NONE',  ( 27.84617737630000178, 1442.188138044969946, 137.3853255074979813 ) ) ;
#107010 = CARTESIAN_POINT ( 'NONE',  ( -11.42267527399999949, 1490.824039550989937, 209.4152927566280198 ) ) ;
#107012 = EDGE_CURVE ( 'NONE', #86132, #108494, #40672, .T. ) ;
#107011 = FACE_OUTER_BOUND ( 'NONE', #81656, .T. ) ;
#107013 = CARTESIAN_POINT ( 'NONE',  ( 14.87800470701120048, 1508.139627058890028, 232.3565943604129984 ) ) ;
#107014 = CARTESIAN_POINT ( 'NONE',  ( 31.99634982962822605, 1416.543175412537494, 269.3157931535475313 ) ) ;
#107015 = AXIS2_PLACEMENT_3D ( 'NONE', #51970, #51406, #78260 ) ;
#107016 = CARTESIAN_POINT ( 'NONE',  ( 8.214112888310001637, 1423.929736291430117, 211.6354380387589913 ) ) ;
#107017 = CARTESIAN_POINT ( 'NONE',  ( 18.66420869458052323, 1526.382868172864164, 232.7837831374276902 ) ) ;
#107018 = CARTESIAN_POINT ( 'NONE',  ( -93.24815347825941103, 1384.613258628189897, 309.6385292495870090 ) ) ;
#107019 = B_SPLINE_SURFACE_WITH_KNOTS ( 'NONE', 5, 5, ( 
 ( #13089, #4175, #55696, #5264, #89817, #107724, #79789, #81957, #47274 ),
 ( #22028, #89269, #106075, #37774, #29901, #56225, #29355, #37222, #12565 ),
 ( #3094, #71419, #81397, #31009, #105534, #64093, #20943, #65189, #4709 ),
 ( #73031, #21483, #63556, #38852, #63020, #13634, #47822, #107169, #80877 ),
 ( #46195, #97671, #97126, #71965, #28823, #38305, #30461, #64646, #98215 ),
 ( #98766, #20395, #54599, #11474, #72486, #88732, #12015, #106615, #73595 ),
 ( #39417, #90356, #55148, #19851, #54055, #80329, #45649, #3645, #88182 ),
 ( #75781, #14757, #101500, #109394, #32670, #41066, #24787, #66305, #39966 ),
 ( #100958, #57890, #15832, #83612, #50036, #90917, #84712, #65736, #6910 ) ),
 .UNSPECIFIED., .F., .F., .F.,
 ( 6, 3, 6 ),
 ( 6, 3, 6 ),
 ( 9.902195898180000455, 12.38020728900000123, 16.40090783169999966 ),
 ( 0.000000000000000000, 0.5000000000000000000, 1.000000000000000000 ),
 .UNSPECIFIED. ) ;
#107020 = CARTESIAN_POINT ( 'NONE',  ( -37.82349669198160313, 1384.984812771009729, 210.9237282750169982 ) ) ;
#107021 = CARTESIAN_POINT ( 'NONE',  ( -12.07909423994960108, 1491.047902796329936, 206.9755603749529769 ) ) ;
#107022 = CARTESIAN_POINT ( 'NONE',  ( -4.580619238605350141, 1508.551704408389924, 205.2658447893479945 ) ) ;
#107023 = CIRCLE ( 'NONE', #80267, 1.999996097696930430 ) ;
#107024 = CARTESIAN_POINT ( 'NONE',  ( 16.69366550187172038, 1526.382868172863937, 183.7020206129021176 ) ) ;
#107025 = EDGE_CURVE ( 'NONE', #96030, #86293, #35064, .T. ) ;
#107026 = FACE_OUTER_BOUND ( 'NONE', #69107, .T. ) ;
#107028 = ORIENTED_EDGE ( 'NONE', *, *, #107504, .T. ) ;
#107027 = CARTESIAN_POINT ( 'NONE',  ( 0.4995595210673769437, 1414.543198520750138, 184.8908676557550166 ) ) ;
#107029 = CARTESIAN_POINT ( 'NONE',  ( -109.3085299140000046, 1384.876463468619932, 311.2645433622590190 ) ) ;
#107030 = AXIS2_PLACEMENT_3D ( 'NONE', #50633, #84765, #8062 ) ;
#107031 = CARTESIAN_POINT ( 'NONE',  ( 40.27131413995757470, 1443.849994623672728, 137.1307286851228184 ) ) ;
#107032 = CARTESIAN_POINT ( 'NONE',  ( -11.25901873334290038, 1500.172003390719965, 210.8567363214919794 ) ) ;
#107033 = CARTESIAN_POINT ( 'NONE',  ( -0.1041750762200730068, 1420.399864921520020, 183.1908796769659773 ) ) ;
#107034 = CARTESIAN_POINT ( 'NONE',  ( -2.379192260459999986, 1422.184172195939937, 193.0946206466989850 ) ) ;
#107035 = CARTESIAN_POINT ( 'NONE',  ( 21.61088119619999759, 1409.667728988130193, 213.1529199375679866 ) ) ;
#107036 = CARTESIAN_POINT ( 'NONE',  ( 14.94707557629999961, 1464.258769156330118, 189.8680940798979861 ) ) ;
#107037 = CARTESIAN_POINT ( 'NONE',  ( -20.46642572180000030, 1467.931903674690147, 211.3545004319090026 ) ) ;
#107038 = CARTESIAN_POINT ( 'NONE',  ( -17.66402273019999924, 1423.191735939130240, 226.2866990750980278 ) ) ;
#107040 = CARTESIAN_POINT ( 'NONE',  ( -11.03395607409999890, 1380.324975612369826, 203.1430293853689761 ) ) ;
#107039 = CARTESIAN_POINT ( 'NONE',  ( -3.836805930384536545, 1511.512554418210811, 200.9783825810452527 ) ) ;
#107041 = CARTESIAN_POINT ( 'NONE',  ( -13.08811655757008374, 1380.207677608032782, 214.5718171420391229 ) ) ;
#107042 = CARTESIAN_POINT ( 'NONE',  ( -100.5161172128999993, 1371.894749952189613, 307.5116414118388093 ) ) ;
#107043 = CARTESIAN_POINT ( 'NONE',  ( -3.331783404088238143, 1522.051704408389924, 220.8088060444078451 ) ) ;
#107044 = EDGE_CURVE ( 'NONE', #24484, #95178, #46543, .T. ) ;
#107045 = CARTESIAN_POINT ( 'NONE',  ( -2.001405295990000166, 1417.433771689029982, 234.4571982132979997 ) ) ;
#107046 = CARTESIAN_POINT ( 'NONE',  ( 7.445922712500000706, 1367.935115748530052, 210.6218459616991936 ) ) ;
#107047 = CARTESIAN_POINT ( 'NONE',  ( -1.135185082175000026, 1516.778853242349896, 205.6747174714770097 ) ) ;
#107048 = CARTESIAN_POINT ( 'NONE',  ( -5.350563530668329904, 1484.262296847969992, 183.6824371965580269 ) ) ;
#107049 = VERTEX_POINT ( 'NONE', #96601 ) ;
#107050 = EDGE_CURVE ( 'NONE', #25418, #11098, #60242, .T. ) ;
#107051 = LINE ( 'NONE', #79670, #19028 ) ;
#107052 = CARTESIAN_POINT ( 'NONE',  ( -4.283506096700399723, 1440.960946171619980, 155.9766071721359992 ) ) ;
#107054 = VERTEX_POINT ( 'NONE', #79255 ) ;
#107053 = CARTESIAN_POINT ( 'NONE',  ( -67.57970925394799622, 1379.745139398459969, 278.8730669361860350 ) ) ;
#107055 = B_SPLINE_CURVE_WITH_KNOTS ( 'NONE', 5,
 ( #12174, #36832, #35726, #104027, #53663, #104586, #20556, #89441, #10526 ),
 .UNSPECIFIED., .F., .F.,
 ( 6, 3, 6 ),
 ( 0.000000000000000000, 0.4556035044110292587, 1.000000000000000000 ),
 .UNSPECIFIED. ) ;
#107056 = EDGE_LOOP ( 'NONE', ( #103501, #23560, #68, #95903 ) ) ;
#107057 = CARTESIAN_POINT ( 'NONE',  ( 28.25086440160000123, 1508.135696994329919, 209.3857010626460067 ) ) ;
#107058 = ORIENTED_EDGE ( 'NONE', *, *, #93291, .F. ) ;
#107059 = DIRECTION ( 'NONE',  ( -6.123233995736769734E-17, -1.000000000000000000, 0.000000000000000000 ) ) ;
#107060 = CARTESIAN_POINT ( 'NONE',  ( 11.23408297830000002, 1500.787540975290085, 206.3532497413090141 ) ) ;
#107062 = CARTESIAN_POINT ( 'NONE',  ( 1.623739401199999932, 1508.906036784929938, 180.0335669106979992 ) ) ;
#107061 = CARTESIAN_POINT ( 'NONE',  ( 15.85916472032949898, 1416.833704394080087, 191.3322456763750097 ) ) ;
#107063 = CARTESIAN_POINT ( 'NONE',  ( -7.326072182274999456, 1516.714320817460020, 209.8751461055349807 ) ) ;
#107064 = CARTESIAN_POINT ( 'NONE',  ( -24.07745899746860019, 1452.072289599009991, 136.6778791173090042 ) ) ;
#107065 = CARTESIAN_POINT ( 'NONE',  ( -11.73650491189999912, 1426.280347616930158, 144.1690576440980180 ) ) ;
#107066 = CARTESIAN_POINT ( 'NONE',  ( 14.54631876779999899, 1409.587692354329874, 227.1236616575980065 ) ) ;
#107067 = CARTESIAN_POINT ( 'NONE',  ( 7.161184789771309234, 1483.929743994920045, 217.3859321370360078 ) ) ;
#107068 = DIRECTION ( 'NONE',  ( 0.000000000000000000, 0.000000000000000000, 1.000000000000000000 ) ) ;
#107069 = CARTESIAN_POINT ( 'NONE',  ( 41.66155871505439734, 1443.633333538899933, 134.0999999981970063 ) ) ;
#107070 = FACE_OUTER_BOUND ( 'NONE', #64312, .T. ) ;
#107071 = VERTEX_POINT ( 'NONE', #94938 ) ;
#107072 = CARTESIAN_POINT ( 'NONE',  ( -19.34950235940319985, 1446.106554878399947, 200.0047909411070179 ) ) ;
#107073 = FACE_OUTER_BOUND ( 'NONE', #6403, .T. ) ;
#107074 = ORIENTED_EDGE ( 'NONE', *, *, #65359, .T. ) ;
#107075 = VERTEX_POINT ( 'NONE', #27732 ) ;
#107076 = CARTESIAN_POINT ( 'NONE',  ( 4.231647580394414021, 1410.439481984662734, 231.4381811129047435 ) ) ;
#107077 = CARTESIAN_POINT ( 'NONE',  ( 5.456719627610000067, 1455.595244131089885, 218.2350948550090095 ) ) ;
#107078 = CARTESIAN_POINT ( 'NONE',  ( -0.05678672266099999560, 1451.699960474029922, 183.0333059144979870 ) ) ;
#107079 = CARTESIAN_POINT ( 'NONE',  ( -3.397007901869999902, 1485.996548673229881, 182.1933214028979933 ) ) ;
#107080 = CARTESIAN_POINT ( 'NONE',  ( -14.53473250189999888, 1379.710786837239993, 208.2794111059409943 ) ) ;
#107081 = CARTESIAN_POINT ( 'NONE',  ( -65.61919861378314067, 1379.740928103604574, 273.5950405564674952 ) ) ;
#107082 = CARTESIAN_POINT ( 'NONE',  ( 10.96015508933500016, 1516.551704408390151, 225.0317485278669949 ) ) ;
#107083 = CARTESIAN_POINT ( 'NONE',  ( 27.93158904759999928, 1508.017348895330088, 207.9454904019079891 ) ) ;
#107084 = CARTESIAN_POINT ( 'NONE',  ( 9.435157646520000441, 1414.913060387329779, 196.1144213233980054 ) ) ;
#107085 = CARTESIAN_POINT ( 'NONE',  ( -54.32597545910780212, 1384.640566766860047, 232.6159698627500063 ) ) ;
#107086 = ORIENTED_EDGE ( 'NONE', *, *, #12582, .F. ) ;
#107087 = DIRECTION ( 'NONE',  ( 0.000000000000000000, 0.000000000000000000, -1.000000000000000000 ) ) ;
#107088 = CARTESIAN_POINT ( 'NONE',  ( -1.717139122245000094, 1516.949031626070109, 208.0040058453670042 ) ) ;
#107090 = ORIENTED_EDGE ( 'NONE', *, *, #69154, .F. ) ;
#107089 = B_SPLINE_CURVE_WITH_KNOTS ( 'NONE', 5,
 ( #4592, #3513, #62322, #20816, #37637, #72900, #30327, #64516, #71842, #13509, #55014, #21899 ),
 .UNSPECIFIED., .F., .F.,
 ( 6, 3, 3, 6 ),
 ( 14.91778236361800047, 20.16173081580000215, 25.40568016630000159, 28.75057693464048469 ),
 .UNSPECIFIED. ) ;
#107091 = CARTESIAN_POINT ( 'NONE',  ( 39.34366195029559776, 1440.913060387330006, 266.6071495697630098 ) ) ;
#107092 = CARTESIAN_POINT ( 'NONE',  ( -0.0003458708581578771369, 1452.035320502890499, 153.9482814617377073 ) ) ;
#107093 = ORIENTED_EDGE ( 'NONE', *, *, #70417, .F. ) ;
#107094 = CARTESIAN_POINT ( 'NONE',  ( -0.1083607850349780077, 1451.692459334710065, 183.0338343828840095 ) ) ;
#107095 = CARTESIAN_POINT ( 'NONE',  ( -16.05577010409999872, 1409.975501755830010, 191.6037359313979778 ) ) ;
#107096 = FACE_OUTER_BOUND ( 'NONE', #96891, .T. ) ;
#107097 = CARTESIAN_POINT ( 'NONE',  ( 20.96806063649999885, 1497.404333632189946, 212.2179028469190030 ) ) ;
#107098 = CARTESIAN_POINT ( 'NONE',  ( 22.44517203296219776, 1410.596246135090041, 206.2149503098679872 ) ) ;
#107099 = B_SPLINE_CURVE_WITH_KNOTS ( 'NONE', 3,
 ( #99345, #98812, #22074, #28866, #107216, #72527, #29947, #64140, #55743, #5869, #56269, #40011, #90960, #5307, #39466, #107768, #63058, #20433, #54640, #46241, #83662, #93699, #59041, #40562, #93163, #108320, #58482, #59584, #99900, #57937, #8603, #16433, #24838, #49537, #65782, #76375, #32162, #84759, #48988, #66349, #92610, #110524, #68002, #50086, #23197, #91523 ),
 .UNSPECIFIED., .F., .F.,
 ( 4, 3, 3, 3, 3, 3, 3, 3, 3, 3, 3, 3, 3, 3, 3, 4 ),
 ( 9.875699484660000138, 11.70136201872880122, 11.94830905290000089, 14.13772687250919979, 15.85048082565690031, 17.40076151789799752, 18.81555256143910171, 19.64990296329999708, 20.88619740925589952, 22.17317058353600245, 23.52607082560420082, 25.04768890600420050, 26.74277199947320227, 29.05331164702660018, 29.41780153859999913, 30.22064862599999913 ),
 .UNSPECIFIED. ) ;
#107100 = CARTESIAN_POINT ( 'NONE',  ( -5.523053292569629846, 1510.639750819970004, 201.5677449951700169 ) ) ;
#107101 = CARTESIAN_POINT ( 'NONE',  ( -3.535390471679999980, 1507.776749383930110, 180.9473287213979802 ) ) ;
#107102 = CARTESIAN_POINT ( 'NONE',  ( -12.91319902290000066, 1434.774343387339968, 147.8554079201980187 ) ) ;
#107103 = CARTESIAN_POINT ( 'NONE',  ( -21.92916355573733966, 1523.390106123591067, 183.0654104491212877 ) ) ;
#107105 = DIRECTION ( 'NONE',  ( 0.000000000000000000, 0.000000000000000000, -1.000000000000000000 ) ) ;
#107104 = CARTESIAN_POINT ( 'NONE',  ( 16.47764957789999940, 1459.038222156129905, 230.9212189925980283 ) ) ;
#107106 = CARTESIAN_POINT ( 'NONE',  ( -2.871580426725000024, 1517.129577905929864, 216.0720609035170128 ) ) ;
#107107 = CIRCLE ( 'NONE', #82076, 0.9999999999999765743 ) ;
#107108 = CARTESIAN_POINT ( 'NONE',  ( -18.19590854888121356, 1501.977400791986611, 238.2026672068777202 ) ) ;
#107109 = CARTESIAN_POINT ( 'NONE',  ( -10.96015512746500065, 1516.551704408390151, 193.2119433744669834 ) ) ;
#107110 = AXIS2_PLACEMENT_3D ( 'NONE', #41295, #109062, #100629 ) ;
#107111 = CARTESIAN_POINT ( 'NONE',  ( 19.33837180206075956, 1442.618379756513150, 212.9432736166801874 ) ) ;
#107112 = CARTESIAN_POINT ( 'NONE',  ( -3.447264387095000160, 1516.858765657450249, 212.5828932618570093 ) ) ;
#107113 = CARTESIAN_POINT ( 'NONE',  ( 2.329957330370219903, 1515.551704201149960, 212.9510108335710186 ) ) ;
#107114 = CARTESIAN_POINT ( 'NONE',  ( -4.726544020967549997, 1483.113842110900123, 199.5813482372220165 ) ) ;
#107116 = ORIENTED_EDGE ( 'NONE', *, *, #41222, .T. ) ;
#107115 = FACE_OUTER_BOUND ( 'NONE', #7230, .T. ) ;
#107117 = CARTESIAN_POINT ( 'NONE',  ( -1.191524307911313585, 1526.382868172864164, 179.0083900503168479 ) ) ;
#107118 = CARTESIAN_POINT ( 'NONE',  ( 23.91643402620000103, 1445.742613539229978, 213.3354513389379861 ) ) ;
#107119 = CARTESIAN_POINT ( 'NONE',  ( -11.27974580559999929, 1430.696192609630089, 151.3350657528979752 ) ) ;
#107120 = CARTESIAN_POINT ( 'NONE',  ( -15.04100366369999975, 1416.091181750810165, 205.5542740844690002 ) ) ;
#107121 = CARTESIAN_POINT ( 'NONE',  ( -7.497461585337410028, 1441.051475807649922, 203.6591753659959920 ) ) ;
#107122 = CARTESIAN_POINT ( 'NONE',  ( -31.32995031131208918, 1523.678648413191695, 196.3423562208917872 ) ) ;
#107123 = CARTESIAN_POINT ( 'NONE',  ( -18.05542497264810109, 1416.825784014559986, 209.4840452940109969 ) ) ;
#107124 = CARTESIAN_POINT ( 'NONE',  ( 11.87714051300000051, 1445.674110462049839, 187.3195967386980101 ) ) ;
#107126 = CARTESIAN_POINT ( 'NONE',  ( 5.361309434614839553, 1423.568641984250007, 149.4828989101069965 ) ) ;
#107125 = CARTESIAN_POINT ( 'NONE',  ( -18.56493692389999950, 1444.808688822819931, 226.5443963784980212 ) ) ;
#107127 = CARTESIAN_POINT ( 'NONE',  ( -0.3621993314549999954, 1416.825784017130218, 191.0664210094979865 ) ) ;
#107128 = AXIS2_PLACEMENT_3D ( 'NONE', #61130, #47058, #96348 ) ;
#107129 = VERTEX_POINT ( 'NONE', #102754 ) ;
#107130 = CARTESIAN_POINT ( 'NONE',  ( 1.121383591734999907, 1517.104192383289956, 204.4960559556369901 ) ) ;
#107131 = CARTESIAN_POINT ( 'NONE',  ( 1.331407961979999888, 1405.856278196329868, 267.2342693101979876 ) ) ;
#107132 = CARTESIAN_POINT ( 'NONE',  ( -0.7420515760000009342, 1515.368784161290250, 213.4096358822789909 ) ) ;
#107133 = CARTESIAN_POINT ( 'NONE',  ( 0.000000000000000000, 1512.187213306747481, 209.1218459616979999 ) ) ;
#107134 = CARTESIAN_POINT ( 'NONE',  ( 22.10779026040307826, 1430.188740980609509, 217.8605039218372212 ) ) ;
#107135 = CARTESIAN_POINT ( 'NONE',  ( -26.78836348560000147, 1451.977613598030075, 134.9156010057980097 ) ) ;
#107136 = CARTESIAN_POINT ( 'NONE',  ( -2.621457251404220035, 1517.151704408390060, 228.0616540033011574 ) ) ;
#107137 = CARTESIAN_POINT ( 'NONE',  ( 4.151444298953053114, 1516.720891557477444, 200.3679918764218826 ) ) ;
#107138 = CARTESIAN_POINT ( 'NONE',  ( -2.494611402081910345, 1449.235109927490157, 154.7923003029100073 ) ) ;
#107139 = CARTESIAN_POINT ( 'NONE',  ( -1.557563050309025421, 1451.010411511857455, 183.5840749928846094 ) ) ;
#107140 = ADVANCED_FACE ( 'NONE', ( #104439 ), #78823, .F. ) ;
#107141 = CARTESIAN_POINT ( 'NONE',  ( -19.59053950279439960, 1486.265866315750145, 189.8955481462990065 ) ) ;
#107142 = DIRECTION ( 'NONE',  ( 0.9455185755993178454, 0.000000000000000000, -0.3255681544571539243 ) ) ;
#107143 = CARTESIAN_POINT ( 'NONE',  ( -12.31949146158819985, 1378.253793448930082, 209.5105130821430066 ) ) ;
#107144 = CARTESIAN_POINT ( 'NONE',  ( -19.80583354730000067, 1436.359101690570242, 219.6133835737980178 ) ) ;
#107145 = CARTESIAN_POINT ( 'NONE',  ( 19.89552980014500250, 1507.835517169810373, 229.1917673227054024 ) ) ;
#107146 = CARTESIAN_POINT ( 'NONE',  ( 2.713894501950000038, 1440.141166743770100, 155.9953435499980117 ) ) ;
#107147 = CARTESIAN_POINT ( 'NONE',  ( -1.769923271310000157, 1475.735664967129878, 269.0444966765980439 ) ) ;
#107148 = CARTESIAN_POINT ( 'NONE',  ( -11.47040950403622617, 1425.342285957420017, 138.1876487757173493 ) ) ;
#107149 = CARTESIAN_POINT ( 'NONE',  ( 8.978224880359460869, 1452.688325515109909, 212.1105500328530127 ) ) ;
#107150 = DIRECTION ( 'NONE',  ( 0.4090087482554177756, 0.000000000000000000, -0.9125304618754029873 ) ) ;
#107151 = CARTESIAN_POINT ( 'NONE',  ( -28.43252842688429993, 1384.834145945409773, 226.5024172414440216 ) ) ;
#107152 = CARTESIAN_POINT ( 'NONE',  ( -5.005324004894529111, 1391.742413812679388, 214.7013071040425132 ) ) ;
#107153 = AXIS2_PLACEMENT_3D ( 'NONE', #31047, #65229, #96196 ) ;
#107154 = CARTESIAN_POINT ( 'NONE',  ( 12.26979804483799974, 1416.828039243390094, 223.5793509210460002 ) ) ;
#107155 = ADVANCED_FACE ( 'NONE', ( #4730 ), #75874, .F. ) ;
#107156 = B_SPLINE_SURFACE_WITH_KNOTS ( 'NONE', 5, 1, ( 
 ( #103990, #27288 ),
 ( #26731, #52507 ),
 ( #77154, #78802 ),
 ( #34580, #25610 ),
 ( #51949, #102868 ),
 ( #60919, #9931 ) ),
 .UNSPECIFIED., .F., .F., .F.,
 ( 6, 6 ),
 ( 2, 2 ),
 ( -7.538862163178030240E-05, 16.22318445422160238 ),
 ( 0.000000000000000000, 14.00007538862159961 ),
 .UNSPECIFIED. ) ;
#107157 = CARTESIAN_POINT ( 'NONE',  ( 12.12990662800260111, 1491.497813992390093, 207.1218616752200035 ) ) ;
#107158 = CARTESIAN_POINT ( 'NONE',  ( -19.30300490007812186, 1526.348417187222594, 185.0858834514397984 ) ) ;
#107159 = CARTESIAN_POINT ( 'NONE',  ( 7.321844823074391329, 1508.611350403034521, 203.6084103738731130 ) ) ;
#107160 = CARTESIAN_POINT ( 'NONE',  ( -10.89711927764389898, 1396.293596177750032, 211.0634950529329785 ) ) ;
#107161 = FACE_OUTER_BOUND ( 'NONE', #73724, .T. ) ;
#107162 = AXIS2_PLACEMENT_3D ( 'NONE', #87498, #56093, #56646 ) ;
#107163 = CARTESIAN_POINT ( 'NONE',  ( -44.90740486440000012, 1439.964170239070199, 269.6916829979979866 ) ) ;
#107164 = ORIENTED_EDGE ( 'NONE', *, *, #20564, .F. ) ;
#107165 = CARTESIAN_POINT ( 'NONE',  ( 2.500000000000000000, 1411.429641636930000, 146.1721969590979882 ) ) ;
#107166 = CARTESIAN_POINT ( 'NONE',  ( -13.59502692214180009, 1507.745895393389901, 209.3598175520070015 ) ) ;
#107167 = CARTESIAN_POINT ( 'NONE',  ( -11.81421902116150058, 1428.091850136479934, 150.2203612155920212 ) ) ;
#107169 = CARTESIAN_POINT ( 'NONE',  ( -12.04783380916500057, 1512.799725290120023, 192.4725698663669959 ) ) ;
#107168 = CARTESIAN_POINT ( 'NONE',  ( 11.12608870130000049, 1426.040907521229883, 108.0448315156979930 ) ) ;
#107170 = CARTESIAN_POINT ( 'NONE',  ( 1.997114501359404048, 1521.951704408389787, 188.3688149103338958 ) ) ;
#107171 = DIRECTION ( 'NONE',  ( -5.980589973904019347E-17, 1.000000000000000000, -1.736889445713099699E-16 ) ) ;
#107172 = B_SPLINE_CURVE_WITH_KNOTS ( 'NONE', 5,
 ( #82459, #14128, #39898, #5757, #4115, #98141 ),
 .UNSPECIFIED., .F., .F.,
 ( 6, 6 ),
 ( 0.000000000000000000, 1.000000000000000000 ),
 .UNSPECIFIED. ) ;
#107173 = CARTESIAN_POINT ( 'NONE',  ( 0.7391219670640019057, 1517.130100026000036, 202.1721425974470208 ) ) ;
#107174 = CARTESIAN_POINT ( 'NONE',  ( 11.85459481136119919, 1500.917689636769865, 208.6046480963290151 ) ) ;
#107175 = CARTESIAN_POINT ( 'NONE',  ( 18.46110511450000047, 1471.786120934990095, 195.2229451476989937 ) ) ;
#107176 = CARTESIAN_POINT ( 'NONE',  ( 2.411010536460000075, 1508.412767799730091, 180.8118562158980183 ) ) ;
#107177 = FACE_BOUND ( 'NONE', #23539, .T. ) ;
#107178 = CARTESIAN_POINT ( 'NONE',  ( -53.42892008310190022, 1379.491042053530009, 254.0488722920499640 ) ) ;
#107179 = ADVANCED_FACE ( 'NONE', ( #55720 ), #59745, .F. ) ;
#107180 = TOROIDAL_SURFACE ( 'NONE', #3558, 24.69926344187880929, 1.000000000000000000 ) ;
#107181 = CARTESIAN_POINT ( 'NONE',  ( 4.064762469398819356, 1367.001946128230202, 209.6218459617148824 ) ) ;
#107183 = ORIENTED_EDGE ( 'NONE', *, *, #46404, .T. ) ;
#107182 = CARTESIAN_POINT ( 'NONE',  ( 9.085013217329999335, 1453.300037844490134, 212.7885071865789826 ) ) ;
#107184 = EDGE_LOOP ( 'NONE', ( #27197, #106397, #61347, #71654, #22022, #110, #90387, #4850, #101744, #48990, #16043, #14703 ) ) ;
#107185 = CARTESIAN_POINT ( 'NONE',  ( -7.928786415319999392, 1396.369758677929894, 199.8437903500179686 ) ) ;
#107186 = VECTOR ( 'NONE', #108969, 1000.000000000000000 ) ;
#107187 = CARTESIAN_POINT ( 'NONE',  ( -21.82696587910000119, 1410.169385423830136, 214.9179092355680041 ) ) ;
#107188 = CARTESIAN_POINT ( 'NONE',  ( -7.717505791104999346, 1516.857914730730045, 201.4043401791270185 ) ) ;
#107189 = CARTESIAN_POINT ( 'NONE',  ( -12.68794671246196515, 1445.019395964141040, 169.4610012160564736 ) ) ;
#107190 = CARTESIAN_POINT ( 'NONE',  ( 11.89850863680000082, 1497.713060387329961, 228.0402318450979919 ) ) ;
#107191 = FACE_OUTER_BOUND ( 'NONE', #9817, .T. ) ;
#107194 = EDGE_CURVE ( 'NONE', #29531, #66077, #82241, .T. ) ;
#107193 = CARTESIAN_POINT ( 'NONE',  ( 17.68800140140000110, 1413.542839617829941, 225.2903305969980181 ) ) ;
#107192 = CARTESIAN_POINT ( 'NONE',  ( -104.2118261680000018, 1389.977870280240040, 305.3688602097590206 ) ) ;
#107195 = CARTESIAN_POINT ( 'NONE',  ( -31.33756686635658184, 1523.580204110583963, 196.3415365203911449 ) ) ;
#107196 = CARTESIAN_POINT ( 'NONE',  ( -3.983812761516020373, 1463.710686891660089, 200.0140896495050242 ) ) ;
#107197 = CARTESIAN_POINT ( 'NONE',  ( -37.53081473069939733, 1450.871859837360034, 135.1685289577449964 ) ) ;
#107198 = B_SPLINE_CURVE_WITH_KNOTS ( 'NONE', 5,
 ( #40422, #66214, #64558, #6813, #49391, #5171 ),
 .UNSPECIFIED., .F., .F.,
 ( 6, 6 ),
 ( 0.000000000000000000, 1.000000000000000000 ),
 .UNSPECIFIED. ) ;
#107199 = CARTESIAN_POINT ( 'NONE',  ( 10.87134764885750116, 1396.292696212680084, 207.0252786116620030 ) ) ;
#107200 = CARTESIAN_POINT ( 'NONE',  ( 31.12456774391174719, 1525.960063244516959, 201.1524202391562710 ) ) ;
#107201 = CARTESIAN_POINT ( 'NONE',  ( 11.45344409740000202, 1425.467136357829986, 145.4513200822979968 ) ) ;
#107202 = CARTESIAN_POINT ( 'NONE',  ( 41.14441233990000057, 1444.077580987459896, 136.9184759350980016 ) ) ;
#107203 = ORIENTED_EDGE ( 'NONE', *, *, #43441, .T. ) ;
#107204 = CARTESIAN_POINT ( 'NONE',  ( 16.93884299705920071, 1507.634939766059915, 188.0954313100240256 ) ) ;
#107205 = CARTESIAN_POINT ( 'NONE',  ( 22.08622291482331335, 1523.382868172864164, 184.4183880513174927 ) ) ;
#107206 = EDGE_LOOP ( 'NONE', ( #57069, #62147, #18309, #97636, #85960 ) ) ;
#107207 = EDGE_LOOP ( 'NONE', ( #37940, #25265, #2227, #22061, #37826, #34497, #46190, #94465, #29681, #65226, #102731, #82330, #4905, #54194, #6961, #9794, #39161, #31479, #104450, #45791 ) ) ;
#107208 = CARTESIAN_POINT ( 'NONE',  ( -17.57407502070000049, 1419.698630043679941, 206.3903661100590057 ) ) ;
#107209 = FACE_OUTER_BOUND ( 'NONE', #26208, .T. ) ;
#107210 = CARTESIAN_POINT ( 'NONE',  ( -108.9869942201588913, 1387.752788737366473, 310.8052485749022367 ) ) ;
#107211 = CARTESIAN_POINT ( 'NONE',  ( 13.01583361309999809, 1416.817366564930126, 196.3351323531979915 ) ) ;
#107212 = CARTESIAN_POINT ( 'NONE',  ( -3.452917061035000401, 1517.089216728169959, 216.0711116162470091 ) ) ;
#107213 = CARTESIAN_POINT ( 'NONE',  ( -12.60028346443769998, 1379.611581493590165, 209.5698690232689785 ) ) ;
#107214 = VERTEX_POINT ( 'NONE', #36557 ) ;
#107215 = CARTESIAN_POINT ( 'NONE',  ( -18.53384158972099982, 1508.522892864089954, 210.7233192446600185 ) ) ;
#107216 = CARTESIAN_POINT ( 'NONE',  ( 2.500000000000000000, 1448.768630321689898, 157.0420996650450149 ) ) ;
#107217 = CARTESIAN_POINT ( 'NONE',  ( -43.21650806019999891, 1376.046645985830082, 226.3493147691589797 ) ) ;
#107218 = CARTESIAN_POINT ( 'NONE',  ( 2.845602704200000055, 1416.216739748429973, 226.8837702527980298 ) ) ;
#107219 = CARTESIAN_POINT ( 'NONE',  ( -4.621897862544999569, 1516.858533673840157, 204.5099662467769974 ) ) ;
#107220 = ORIENTED_EDGE ( 'NONE', *, *, #19041, .T. ) ;
#107221 = AXIS2_PLACEMENT_3D ( 'NONE', #24261, #66855, #84720 ) ;
#107222 = CARTESIAN_POINT ( 'NONE',  ( -8.946235101802798795, 1451.321446327319791, 206.7355029101660193 ) ) ;
#107223 = CARTESIAN_POINT ( 'NONE',  ( -35.04866985580577676, 1424.104380813952048, 269.5321808552227481 ) ) ;
#107224 = CARTESIAN_POINT ( 'NONE',  ( 6.044020038074999768, 1511.752511073100095, 217.4188488492769977 ) ) ;
#107226 = ORIENTED_EDGE ( 'NONE', *, *, #23551, .T. ) ;
#107225 = CARTESIAN_POINT ( 'NONE',  ( -8.486299124169999430, 1519.913060387329779, 187.6206292133980185 ) ) ;
#107227 = CARTESIAN_POINT ( 'NONE',  ( -0.0009079351378022920520, 1450.913092093069963, 181.3802231108539900 ) ) ;
#107228 = CARTESIAN_POINT ( 'NONE',  ( -27.56560605785089990, 1440.913060397009986, 229.3484830648729940 ) ) ;
#107229 = CARTESIAN_POINT ( 'NONE',  ( -54.13602515839999541, 1384.720040384200047, 270.3656545589590223 ) ) ;
#107230 = CARTESIAN_POINT ( 'NONE',  ( -0.2143714289189239952, 1465.016896992510055, 237.3853670223340089 ) ) ;
#107231 = CARTESIAN_POINT ( 'NONE',  ( 34.76658121969929738, 1422.301991258000271, 269.9820564234090057 ) ) ;
#107232 = CARTESIAN_POINT ( 'NONE',  ( 5.010422963235000360, 1516.929569650079884, 213.1529883219070030 ) ) ;
#107233 = CARTESIAN_POINT ( 'NONE',  ( -56.64534719470000113, 1379.747652096109960, 254.3393773118589536 ) ) ;
#107234 = CARTESIAN_POINT ( 'NONE',  ( 23.70457460020000084, 1410.841732588929972, 207.9725391979379765 ) ) ;
#107235 = CARTESIAN_POINT ( 'NONE',  ( 29.86461515634913866, 1525.960063244516959, 197.2746849027935809 ) ) ;
#107236 = CARTESIAN_POINT ( 'NONE',  ( 15.82512562826290292, 1427.733577895149892, 200.2964982622260095 ) ) ;
#107237 = CARTESIAN_POINT ( 'NONE',  ( -7.709610715716689988, 1516.556413965810179, 210.7279121869730147 ) ) ;
#107238 = CARTESIAN_POINT ( 'NONE',  ( 0.01265818781360149997, 1516.959716008189844, 210.8316124642570060 ) ) ;
#107239 = CARTESIAN_POINT ( 'NONE',  ( 4.333461763824229429, 1420.406249667820020, 185.6739041016720080 ) ) ;
#107240 = CARTESIAN_POINT ( 'NONE',  ( -4.419614911900000109, 1417.909206216429993, 232.4142678098980070 ) ) ;
#107241 = CARTESIAN_POINT ( 'NONE',  ( 9.046206015765411834, 1421.595877805006012, 137.0999999980981841 ) ) ;
#107242 = EDGE_LOOP ( 'NONE', ( #73636, #73492, #44374, #46207 ) ) ;
#107243 = CARTESIAN_POINT ( 'NONE',  ( -31.71748227402730080, 1385.225470378949922, 229.9276196292890120 ) ) ;
#107244 = AXIS2_PLACEMENT_3D ( 'NONE', #84565, #75639, #8399 ) ;
#107245 = DIRECTION ( 'NONE',  ( 9.267597007367818816E-06, 0.03085854715862546352, -0.9995237615891732208 ) ) ;
#107246 = CARTESIAN_POINT ( 'NONE',  ( 0.4962749089960000193, 1415.445620500730001, 233.3779880030980109 ) ) ;
#107247 = CARTESIAN_POINT ( 'NONE',  ( -20.99189748682200118, 1509.583339404279968, 229.4943028042000321 ) ) ;
#107248 = VECTOR ( 'NONE', #86540, 1000.000000000000000 ) ;
#107249 = CARTESIAN_POINT ( 'NONE',  ( -106.5186165409613466, 1391.553752504539716, 307.6918442614858122 ) ) ;
#107250 = CARTESIAN_POINT ( 'NONE',  ( 10.76697211809999999, 1423.735811814160115, 203.5994285750890072 ) ) ;
#107251 = DIRECTION ( 'NONE',  ( -1.755985294532469921E-16, 1.000000000000000000, -1.338183447452831989E-16 ) ) ;
#107253 = CARTESIAN_POINT ( 'NONE',  ( 18.05542497264820057, 1416.825784014559986, 208.7596466293869923 ) ) ;
#107252 = CARTESIAN_POINT ( 'NONE',  ( -2.871580426725000024, 1517.129577905929864, 216.0720609035170128 ) ) ;
#107254 = CARTESIAN_POINT ( 'NONE',  ( 8.631780704876279131, 1438.018275767699834, 210.0183142686710198 ) ) ;
#107255 = EDGE_LOOP ( 'NONE', ( #84318, #50631, #102123, #86833 ) ) ;
#107256 = CARTESIAN_POINT ( 'NONE',  ( -7.717505791104999346, 1516.857914730730045, 201.4043401791270185 ) ) ;
#107257 = CARTESIAN_POINT ( 'NONE',  ( 10.52024531799330020, 1481.173637506630030, 208.1780703194219768 ) ) ;
#107258 = ORIENTED_EDGE ( 'NONE', *, *, #40920, .F. ) ;
#107259 = CIRCLE ( 'NONE', #10726, 1.999999999999997780 ) ;
#107260 = CARTESIAN_POINT ( 'NONE',  ( 16.68463225901000158, 1442.773887286389936, 162.0935120915889911 ) ) ;
#107261 = CARTESIAN_POINT ( 'NONE',  ( 21.94066466509999813, 1452.058359354930190, 220.5450223258980031 ) ) ;
#107262 =( BOUNDED_SURFACE ( )  B_SPLINE_SURFACE ( 3, 2, ( 
 ( #107235, #49007, #6437 ),
 ( #65802, #99923, #29969 ),
 ( #82024, #30526, #98279 ),
 ( #31075, #5886, #49556 ),
 ( #65258, #21555, #13151 ),
 ( #38914, #73096, #64718 ) ),
 .UNSPECIFIED., .F., .F., .F. ) 
 B_SPLINE_SURFACE_WITH_KNOTS ( ( 4, 2, 4 ),
 ( 3, 3 ),
 ( -2.493664996716660198E-17, 0.001312027981647308043, 0.002624055963294641240 ),
 ( 0.000000000000000000, 1.000000000000000000 ),
 .UNSPECIFIED. ) 
 GEOMETRIC_REPRESENTATION_ITEM ( )  RATIONAL_B_SPLINE_SURFACE ( (
 ( 1.000000000000000000, 0.9376006582765884501, 1.000000000000000000),
 ( 1.000000000000000000, 0.9569320108029427674, 1.000000000000000000),
 ( 1.000000000000000000, 0.9725743441609863149, 1.000000000000000000),
 ( 1.000000000000000000, 0.9942095667144646987, 1.000000000000000000),
 ( 1.000000000000000000, 1.000043666450031843, 1.000000000000000000),
 ( 1.000000000000000000, 1.000000000000000000, 1.000000000000000000) ) ) 
 REPRESENTATION_ITEM ( '' )  SURFACE ( )  );
#107263 = CARTESIAN_POINT ( 'NONE',  ( 8.113228662610344699, 1437.975597658936522, 153.6229958193256380 ) ) ;
#107264 = CARTESIAN_POINT ( 'NONE',  ( 0.03226293719758020068, 1410.297897419189894, 233.2219341505459909 ) ) ;
#107265 = CARTESIAN_POINT ( 'NONE',  ( 2.159699301869999477, 1441.959095157789989, 218.4271172946090189 ) ) ;
#107266 = CARTESIAN_POINT ( 'NONE',  ( 16.47590419726208921, 1421.672314134083535, 227.1462306721412290 ) ) ;
#107267 = CARTESIAN_POINT ( 'NONE',  ( 17.10950584751149961, 1472.077583655310036, 198.3318500205459998 ) ) ;
#107268 = CARTESIAN_POINT ( 'NONE',  ( -19.34922152300000064, 1425.422359720030045, 223.6439256038979693 ) ) ;
#107269 = CARTESIAN_POINT ( 'NONE',  ( -20.55757218060000113, 1485.073878606189965, 207.1049163177690104 ) ) ;
#107270 = CARTESIAN_POINT ( 'NONE',  ( -105.7579672239999979, 1388.939243398469898, 299.5452684353589916 ) ) ;
#107271 = CARTESIAN_POINT ( 'NONE',  ( 19.36651210059999784, 1488.299738432130198, 189.6546506392980120 ) ) ;
#107273 = CARTESIAN_POINT ( 'NONE',  ( -17.40400757659919506, 1433.874116228432058, 216.4982986272186167 ) ) ;
#107272 = CARTESIAN_POINT ( 'NONE',  ( -106.5656785119999910, 1391.248054752850067, 300.3923073593589947 ) ) ;
#107274 = DIRECTION ( 'NONE',  ( 0.000000000000000000, 1.000000000000000000, 0.000000000000000000 ) ) ;
#107275 = ORIENTED_EDGE ( 'NONE', *, *, #36574, .T. ) ;
#107276 = CARTESIAN_POINT ( 'NONE',  ( -105.3812639519999976, 1378.843495839950037, 304.0411346596590079 ) ) ;
#107277 = DIRECTION ( 'NONE',  ( 0.4999997527789440399, 0.7071067730516870098, -0.5000002587253580266 ) ) ;
#107278 = CARTESIAN_POINT ( 'NONE',  ( -113.4000000000000057, 1379.886883438980021, 304.2218459572590064 ) ) ;
#107279 = CYLINDRICAL_SURFACE ( 'NONE', #68226, 0.2999999999999669598 ) ;
#107280 = DIRECTION ( 'NONE',  ( -0.8090169943751894799, 3.009330011589934659E-31, -0.5877852522921398482 ) ) ;
#107281 = VECTOR ( 'NONE', #34954, 1000.000000000000000 ) ;
#107282 = CARTESIAN_POINT ( 'NONE',  ( 1.469666176117540246, 1486.774276370960024, 182.0003414483169877 ) ) ;
#107283 = CARTESIAN_POINT ( 'NONE',  ( -2.700443415721282658, 1524.678872986499073, 241.8612037782705784 ) ) ;
#107284 = CARTESIAN_POINT ( 'NONE',  ( -13.23821889442530697, 1443.160654751977518, 186.8362721621839455 ) ) ;
#107285 = B_SPLINE_SURFACE_WITH_KNOTS ( 'NONE', 5, 5, ( 
 ( #96692, #80984, #78781, #62572, #55251, #89383 ),
 ( #46310, #54157, #2095, #19962, #70409, #12675 ),
 ( #11027, #104528, #4290, #97226, #38417, #71528 ),
 ( #2648, #106184, #72593, #3754, #3205, #106721 ),
 ( #36776, #37332, #20497, #11577, #30012, #44639 ),
 ( #45196, #64202, #27825, #87179, #37886, #45754 ),
 ( #62005, #96125, #19399, #53603, #79337, #105084 ),
 ( #79891, #100530, #56893, #15410, #23809, #32232 ),
 ( #108944, #7028, #64765, #91024, #107833, #55808 ) ),
 .UNSPECIFIED., .F., .F., .F.,
 ( 6, 3, 6 ),
 ( 6, 6 ),
 ( 9.104900351529998659, 12.35991293620000064, 15.61492552089999997 ),
 ( 0.000000000000000000, 2.000000000000000000 ),
 .UNSPECIFIED. ) ;
#107286 = CARTESIAN_POINT ( 'NONE',  ( -7.500000019064997581, 1516.976251993718961, 208.9751496355367806 ) ) ;
#107287 = CARTESIAN_POINT ( 'NONE',  ( -0.1681681984989999989, 1420.016189442530049, 171.1670476502980023 ) ) ;
#107288 = DIRECTION ( 'NONE',  ( -1.000000000000000000, 0.000000000000000000, 0.000000000000000000 ) ) ;
#107290 = ADVANCED_FACE ( 'NONE', ( #78567 ), #102629, .T. ) ;
#107289 = CARTESIAN_POINT ( 'NONE',  ( -102.6163738449689902, 1383.762319109039936, 310.8816873798210167 ) ) ;
#107291 = CARTESIAN_POINT ( 'NONE',  ( 24.69316157360000119, 1435.858930896569973, 137.7793382546979899 ) ) ;
#107292 = CARTESIAN_POINT ( 'NONE',  ( 5.598416906409999783, 1429.565212975089935, 216.3190638356489899 ) ) ;
#107294 = VERTEX_POINT ( 'NONE', #11635 ) ;
#107293 = CARTESIAN_POINT ( 'NONE',  ( 20.45347777980000004, 1495.695647834889996, 214.2365953844490036 ) ) ;
#107295 = VECTOR ( 'NONE', #53792, 1000.000000000000000 ) ;
#107296 = DIRECTION ( 'NONE',  ( 0.000000000000000000, 1.000000000000000000, 0.000000000000000000 ) ) ;
#107297 = CARTESIAN_POINT ( 'NONE',  ( 12.18971934853500194, 1512.123542805230272, 223.8476153537669973 ) ) ;
#107298 = EDGE_CURVE ( 'NONE', #77569, #17947, #71592, .T. ) ;
#107299 = ORIENTED_EDGE ( 'NONE', *, *, #34365, .F. ) ;
#107300 = ORIENTED_EDGE ( 'NONE', *, *, #22203, .F. ) ;
#107301 = CARTESIAN_POINT ( 'NONE',  ( 16.78845670593169714, 1414.971513442450032, 209.5374550761620185 ) ) ;
#107302 = CARTESIAN_POINT ( 'NONE',  ( 13.29979961619999962, 1509.142656770830172, 233.9102947482979857 ) ) ;
#107303 = DIRECTION ( 'NONE',  ( -1.836970198721029688E-16, -1.000000000000000000, 0.000000000000000000 ) ) ;
#107305 = CARTESIAN_POINT ( 'NONE',  ( -28.33103133910000082, 1450.578314054559769, 240.1819618728980004 ) ) ;
#107304 = CARTESIAN_POINT ( 'NONE',  ( 29.77132726792740414, 1419.409540564665576, 269.4683900306495730 ) ) ;
#107306 = CARTESIAN_POINT ( 'NONE',  ( 8.614620945600030666, 1437.484188997010051, 209.9974677346399972 ) ) ;
#107307 = CARTESIAN_POINT ( 'NONE',  ( -11.89338303359999927, 1433.289361183159826, 150.1518857174980042 ) ) ;
#107308 = CARTESIAN_POINT ( 'NONE',  ( -12.28946836655069852, 1378.262473314609906, 210.0681950494530099 ) ) ;
#107309 = CARTESIAN_POINT ( 'NONE',  ( -19.12425472950000227, 1486.130686572730156, 189.5132436031979921 ) ) ;
#107310 = CARTESIAN_POINT ( 'NONE',  ( 24.40137257056360198, 1418.525752740940106, 209.6082346408329897 ) ) ;
#107311 = CARTESIAN_POINT ( 'NONE',  ( -27.26752128509999906, 1441.515264747369883, 137.3262972417980166 ) ) ;
#107312 = CARTESIAN_POINT ( 'NONE',  ( -0.8481724230074738635, 1515.120541028469916, 213.4498349211539789 ) ) ;
#107313 = CARTESIAN_POINT ( 'NONE',  ( 7.134032011620000446, 1442.025630637640006, 154.4960302486979913 ) ) ;
#107314 = CARTESIAN_POINT ( 'NONE',  ( -8.346688520235490572, 1478.631378035029911, 217.2409271317110040 ) ) ;
#107315 = CARTESIAN_POINT ( 'NONE',  ( 0.05521217508070846297, 1361.591753888529865, 210.6218459617142003 ) ) ;
#107316 = CARTESIAN_POINT ( 'NONE',  ( 33.52308185467321522, 1525.402221411319715, 200.6636391946808828 ) ) ;
#107318 = ORIENTED_EDGE ( 'NONE', *, *, #55132, .F. ) ;
#107317 = CARTESIAN_POINT ( 'NONE',  ( 4.449893896030659734E-11, 1411.549994435260032, 254.7521586903190212 ) ) ;
#107319 = ORIENTED_EDGE ( 'NONE', *, *, #66866, .T. ) ;
#107320 = CARTESIAN_POINT ( 'NONE',  ( -11.86575960015439968, 1432.312193440490091, 149.9823566586960055 ) ) ;
#107321 = CARTESIAN_POINT ( 'NONE',  ( -0.3862418810146379666, 1500.063169577209919, 233.1571753207470010 ) ) ;
#107322 = CARTESIAN_POINT ( 'NONE',  ( -15.04635340419999956, 1470.707757194930082, 270.3649393566980166 ) ) ;
#107323 = CARTESIAN_POINT ( 'NONE',  ( 13.31241404839999909, 1509.377940129630133, 234.8971984757980067 ) ) ;
#107324 = CARTESIAN_POINT ( 'NONE',  ( -123.7110048619999958, 1378.528619065190696, 314.5328508192591244 ) ) ;
#107325 = DIRECTION ( 'NONE',  ( 0.9125304618753908859, 0.000000000000000000, -0.4090087482554448095 ) ) ;
#107326 = AXIS2_PLACEMENT_3D ( 'NONE', #31653, #65833, #13179 ) ;
#107327 = B_SPLINE_CURVE_WITH_KNOTS ( 'NONE', 3,
 ( #103095, #31076, #75313, #5329, #9053, #676 ),
 .UNSPECIFIED., .F., .F.,
 ( 4, 2, 4 ),
 ( 0.000000000000000000, 0.002988018091905742402, 0.005976036183811482203 ),
 .UNSPECIFIED. ) ;
#107328 = CARTESIAN_POINT ( 'NONE',  ( 0.3320937139126450277, 1450.964402829440132, 181.7697017419690155 ) ) ;
#107329 = CARTESIAN_POINT ( 'NONE',  ( -13.23585369709999959, 1420.111225874029969, 228.0945412171980138 ) ) ;
#107330 = CARTESIAN_POINT ( 'NONE',  ( -3.179033936840000241, 1457.997354091689886, 219.3203917952990025 ) ) ;
#107331 = CARTESIAN_POINT ( 'NONE',  ( 9.971295257839999593, 1364.502667329740007, 207.6218459616989946 ) ) ;
#107332 = CARTESIAN_POINT ( 'NONE',  ( -28.65682362046179676, 1414.257978759259913, 269.3829595885329695 ) ) ;
#107333 = AXIS2_PLACEMENT_3D ( 'NONE', #57501, #12717, #107325 ) ;
#107334 = EDGE_LOOP ( 'NONE', ( #79975, #40009, #97020, #90242 ) ) ;
#107335 = CARTESIAN_POINT ( 'NONE',  ( -3.034926079678203159, 1369.200812461396481, 210.6218459616991936 ) ) ;
#107336 = ORIENTED_EDGE ( 'NONE', *, *, #53536, .F. ) ;
#107337 = ORIENTED_EDGE ( 'NONE', *, *, #18113, .T. ) ;
#107338 = CARTESIAN_POINT ( 'NONE',  ( -6.546001388695000145, 1516.557392317769882, 210.8318505190270002 ) ) ;
#107339 = DIRECTION ( 'NONE',  ( 0.3363363969979660806, -0.9417419115949053898, 0.000000000000000000 ) ) ;
#107341 = CARTESIAN_POINT ( 'NONE',  ( -17.64585193930734519, 1419.365468075514855, 207.2015379587035682 ) ) ;
#107340 = CARTESIAN_POINT ( 'NONE',  ( 1.135460316954999938, 1516.790374942449944, 212.3751473514870156 ) ) ;
#107342 = CARTESIAN_POINT ( 'NONE',  ( -16.80535727200000196, 1440.439471750479925, 190.3762289849980220 ) ) ;
#107343 = AXIS2_PLACEMENT_3D ( 'NONE', #52418, #96053, #20428 ) ;
#107344 = CARTESIAN_POINT ( 'NONE',  ( -17.33645362950000290, 1414.996442546130083, 207.8511177337479978 ) ) ;
#107345 = ORIENTED_EDGE ( 'NONE', *, *, #57592, .F. ) ;
#107346 = CARTESIAN_POINT ( 'NONE',  ( -26.64877008739999908, 1436.583672242290049, 136.7640741069980095 ) ) ;
#107347 = CARTESIAN_POINT ( 'NONE',  ( -2.291676311554999845, 1516.534976163889951, 201.8006522243570089 ) ) ;
#107348 = B_SPLINE_CURVE_WITH_KNOTS ( 'NONE', 5,
 ( #93208, #32213, #76416, #100513, #16478, #7004 ),
 .UNSPECIFIED., .F., .F.,
 ( 6, 6 ),
 ( -107.3223151640000026, -30.86246213379999404 ),
 .UNSPECIFIED. ) ;
#107349 = DIRECTION ( 'NONE',  ( -0.6038592750913978069, -0.7071067811868650965, 0.3679048462383208151 ) ) ;
#107350 = CARTESIAN_POINT ( 'NONE',  ( -25.73887467969239751, 1384.546265937980024, 203.5795097568579877 ) ) ;
#107351 = CARTESIAN_POINT ( 'NONE',  ( -35.01820525347180535, 1420.005377583910104, 270.2098316748109710 ) ) ;
#107352 = CARTESIAN_POINT ( 'NONE',  ( -9.161428420492889302, 1488.487993194839873, 190.2768237055279883 ) ) ;
#107353 = CARTESIAN_POINT ( 'NONE',  ( -3.730240969670000073, 1396.578899543130092, 197.1274014984979885 ) ) ;
#107355 = EDGE_LOOP ( 'NONE', ( #74176, #17186, #2453, #82289, #10239, #42765, #46776, #55941, #39301 ) ) ;
#107354 = CARTESIAN_POINT ( 'NONE',  ( -8.775285687485823161, 1364.676427693243795, 210.6218459617142003 ) ) ;
#107356 = ORIENTED_EDGE ( 'NONE', *, *, #96805, .F. ) ;
#107357 = CARTESIAN_POINT ( 'NONE',  ( -121.3986813195241723, 1384.899971913130003, 304.3468000529767323 ) ) ;
#107358 = CARTESIAN_POINT ( 'NONE',  ( -14.05078142410000019, 1379.708754511839743, 206.9026084073089748 ) ) ;
#107359 = CARTESIAN_POINT ( 'NONE',  ( -14.58502509368319977, 1436.245402443870034, 149.8759987050300140 ) ) ;
#107360 = VECTOR ( 'NONE', #58956, 1000.000000000000000 ) ;
#107361 = CARTESIAN_POINT ( 'NONE',  ( 3.968827103902559550, 1517.151704408390060, 188.7040005461919918 ) ) ;
#107362 = CARTESIAN_POINT ( 'NONE',  ( 6.563915523884999992, 1517.184063036290127, 210.2461356256870033 ) ) ;
#107363 = CARTESIAN_POINT ( 'NONE',  ( 6.888583400142420210, 1460.429153260329031, 202.3504153456137260 ) ) ;
#107364 = CARTESIAN_POINT ( 'NONE',  ( 6.121126660120000729, 1455.402339941889750, 217.8370560331890147 ) ) ;
#107365 = CARTESIAN_POINT ( 'NONE',  ( 7.611664470185079523, 1439.490851628699829, 213.6370682771540146 ) ) ;
#107366 = CARTESIAN_POINT ( 'NONE',  ( 12.54563646380000108, 1416.254459047329874, 223.2775148006980146 ) ) ;
#107367 = FACE_OUTER_BOUND ( 'NONE', #99609, .T. ) ;
#107368 = CARTESIAN_POINT ( 'NONE',  ( -5.014195139944999546, 1517.120861839400050, 207.4163795216369977 ) ) ;
#107369 = ORIENTED_EDGE ( 'NONE', *, *, #32296, .T. ) ;
#107370 = DIRECTION ( 'NONE',  ( -1.224646799147350002E-16, 1.836970198721029688E-16, 1.000000000000000000 ) ) ;
#107371 = DIRECTION ( 'NONE',  ( 0.000000000000000000, 0.000000000000000000, 1.000000000000000000 ) ) ;
#107372 = ORIENTED_EDGE ( 'NONE', *, *, #107785, .T. ) ;
#107374 = CIRCLE ( 'NONE', #93062, 1.560060070890045836 ) ;
#107373 = CARTESIAN_POINT ( 'NONE',  ( -5.032977197542991554, 1391.805267110368050, 214.4361776410948721 ) ) ;
#107375 = CARTESIAN_POINT ( 'NONE',  ( 25.32192960925430114, 1450.806448946380215, 137.4488745918710322 ) ) ;
#107376 = CARTESIAN_POINT ( 'NONE',  ( -4.118002615245018205, 1440.027047901042351, 185.4484253817595629 ) ) ;
#107377 = CARTESIAN_POINT ( 'NONE',  ( -5.013264327984152224, 1375.413060387289988, 203.5257471471711312 ) ) ;
#107378 = CARTESIAN_POINT ( 'NONE',  ( 20.28125875170000114, 1409.621297549229894, 202.2274701143080051 ) ) ;
#107379 = CARTESIAN_POINT ( 'NONE',  ( -24.89775069963104315, 1442.835541681095037, 210.5176539881000508 ) ) ;
#107380 = DIRECTION ( 'NONE',  ( -5.980589973904019347E-17, 1.000000000000000000, -1.736889445713099699E-16 ) ) ;
#107381 = CARTESIAN_POINT ( 'NONE',  ( 4.247914338581740168, 1441.369206175110094, 161.4618793966889996 ) ) ;
#107382 = CYLINDRICAL_SURFACE ( 'NONE', #17553, 2.000000000000003553 ) ;
#107383 = CARTESIAN_POINT ( 'NONE',  ( -7.325541825264999751, 1516.710692850270107, 214.1269169785269924 ) ) ;
#107384 = ORIENTED_EDGE ( 'NONE', *, *, #709, .T. ) ;
#107385 = CARTESIAN_POINT ( 'NONE',  ( 7.712015721893069831, 1516.648258902369889, 208.0703445135380036 ) ) ;
#107386 = CARTESIAN_POINT ( 'NONE',  ( 3.902542035141590038, 1426.015650130040058, 185.2953857556300079 ) ) ;
#107387 = LINE ( 'NONE', #30683, #10640 ) ;
#107388 = CARTESIAN_POINT ( 'NONE',  ( -11.73564150307709930, 1425.610157878649943, 144.1659385557379949 ) ) ;
#107389 = CARTESIAN_POINT ( 'NONE',  ( 0.6889265495279990326, 1475.123389914190057, 220.5466911795989802 ) ) ;
#107390 = CARTESIAN_POINT ( 'NONE',  ( 11.60004869885203860, 1425.871340881105198, 138.5940851285356530 ) ) ;
#107391 = CARTESIAN_POINT ( 'NONE',  ( -0.8350686643532192477, 1526.382868172863937, 177.3106345060153046 ) ) ;
#107392 = CIRCLE ( 'NONE', #87762, 3.000000000000002665 ) ;
#107393 = CARTESIAN_POINT ( 'NONE',  ( 17.99132714227145158, 1424.137213421525985, 225.5015134895514564 ) ) ;
#107394 = CARTESIAN_POINT ( 'NONE',  ( -109.1553531783490030, 1385.186054570089937, 297.1423525096689673 ) ) ;
#107395 = CARTESIAN_POINT ( 'NONE',  ( -3.520303095042100390E-07, 1407.050513786409965, 222.1263857351630122 ) ) ;
#107396 = B_SPLINE_SURFACE_WITH_KNOTS ( 'NONE', 5, 5, ( 
 ( #82220, #105796, #63796, #90618, #29077, #73845, #96842, #54844, #3897 ),
 ( #38026, #54302, #88430, #72205, #55391, #12813, #106864, #107419, #38559 ),
 ( #46993, #81116, #72738, #98468, #13342, #47534, #39105, #73282, #76445 ),
 ( #101620, #17049, #43411, #59662, #57051, #102188, #15962, #78100, #93770 ),
 ( #60782, #110050, #1402, #25468, #51246, #92686, #42854, #84826, #51812 ),
 ( #33882, #65453, #85379, #50165, #84293, #26585, #110599, #7584, #99561 ) ),
 .UNSPECIFIED., .F., .F., .F.,
 ( 6, 6 ),
 ( 6, 3, 6 ),
 ( 0.4666582264910000277, 2.797885342316130064 ),
 ( -1.082960613491289913E-05, 1.000000000000000000, 2.000000000000000000 ),
 .UNSPECIFIED. ) ;
#107397 = CARTESIAN_POINT ( 'NONE',  ( 32.17164650389580061, 1440.913060383229777, 244.5574107866939926 ) ) ;
#107398 = CARTESIAN_POINT ( 'NONE',  ( -10.50217937927759948, 1470.323102136789885, 212.1317377489009743 ) ) ;
#107399 = DIRECTION ( 'NONE',  ( -1.836970198721029688E-16, -1.000000000000000000, 0.000000000000000000 ) ) ;
#107400 = EDGE_LOOP ( 'NONE', ( #83510, #11087, #68101, #80127 ) ) ;
#107401 = ORIENTED_EDGE ( 'NONE', *, *, #80874, .F. ) ;
#107402 = CARTESIAN_POINT ( 'NONE',  ( 11.78140839543589991, 1479.499659610600020, 209.2033645326229703 ) ) ;
#107403 = CARTESIAN_POINT ( 'NONE',  ( -19.07563200129111536, 1485.497391648796565, 189.6206291117065348 ) ) ;
#107404 = CARTESIAN_POINT ( 'NONE',  ( 12.98226713004290112, 1414.913060387349788, 198.3280232619060257 ) ) ;
#107405 = DIRECTION ( 'NONE',  ( -0.3090169943749446757, 0.000000000000000000, 0.9510565162951544194 ) ) ;
#107406 = AXIS2_PLACEMENT_3D ( 'NONE', #106409, #31344, #29693 ) ;
#107407 = FACE_OUTER_BOUND ( 'NONE', #109273, .T. ) ;
#107408 = CARTESIAN_POINT ( 'NONE',  ( -2.092371031960829963, 1508.551704408389924, 220.0661208745100055 ) ) ;
#107409 = CARTESIAN_POINT ( 'NONE',  ( -52.62061106118209608, 1383.807654112509908, 266.7032437734779933 ) ) ;
#107410 = CARTESIAN_POINT ( 'NONE',  ( -3.279658057385000269, 1511.011611623890076, 201.5574319706369977 ) ) ;
#107411 = CARTESIAN_POINT ( 'NONE',  ( -13.74793944760000031, 1453.152003546729929, 193.7924838359980129 ) ) ;
#107412 = CARTESIAN_POINT ( 'NONE',  ( -9.094257307180781069, 1384.874748761890260, 199.9429999480310016 ) ) ;
#107413 = CARTESIAN_POINT ( 'NONE',  ( 2.750555178629999986, 1464.695220873430117, 236.8701282433979998 ) ) ;
#107415 = ORIENTED_EDGE ( 'NONE', *, *, #96727, .T. ) ;
#107414 = CARTESIAN_POINT ( 'NONE',  ( 32.31946296792703066, 1524.082582765195411, 216.0996188568618948 ) ) ;
#107416 = CARTESIAN_POINT ( 'NONE',  ( -0.4632198342000000135, 1452.646946044229935, 183.2964164767980151 ) ) ;
#107417 = CARTESIAN_POINT ( 'NONE',  ( -35.14840751239999861, 1380.299282000710036, 212.7497223807189926 ) ) ;
#107418 = CARTESIAN_POINT ( 'NONE',  ( -3.251166460929999946, 1475.808624674589737, 199.1811513380790188 ) ) ;
#107420 = ORIENTED_EDGE ( 'NONE', *, *, #91174, .F. ) ;
#107419 = CARTESIAN_POINT ( 'NONE',  ( -18.23773974694429967, 1416.535698381769862, 208.9530515259610013 ) ) ;
#107421 = CARTESIAN_POINT ( 'NONE',  ( -13.05159921682169966, 1467.538567272380078, 191.8992743155650089 ) ) ;
#107422 = ORIENTED_EDGE ( 'NONE', *, *, #64561, .T. ) ;
#107423 = VECTOR ( 'NONE', #28356, 1000.000000000000000 ) ;
#107424 = CARTESIAN_POINT ( 'NONE',  ( -11.34773204379960099, 1388.518463159120074, 216.6153406976970075 ) ) ;
#107425 = CARTESIAN_POINT ( 'NONE',  ( -2.329898844065350083, 1515.219291385429869, 204.7964424083469908 ) ) ;
#107426 = CARTESIAN_POINT ( 'NONE',  ( 3.487586588097512319, 1508.731359868794925, 213.6768079589742513 ) ) ;
#107427 = CARTESIAN_POINT ( 'NONE',  ( -5.487686449739999972, 1463.833492974589944, 200.5004408324890335 ) ) ;
#107428 = CARTESIAN_POINT ( 'NONE',  ( -15.20114627789167550, 1420.043106467314828, 212.3145834610196800 ) ) ;
#107429 = CIRCLE ( 'NONE', #96750, 1.000000000000000000 ) ;
#107430 = CARTESIAN_POINT ( 'NONE',  ( 21.04904418909999819, 1494.916427559390058, 209.1218459616989946 ) ) ;
#107431 = CARTESIAN_POINT ( 'NONE',  ( 3.610699138176100220, 1409.039148779609832, 194.5764597407000167 ) ) ;
#107432 = CARTESIAN_POINT ( 'NONE',  ( 0.4274148046680000257, 1409.096031529930087, 185.6227931958979980 ) ) ;
#107433 = CARTESIAN_POINT ( 'NONE',  ( 17.80745809460000117, 1457.129128898490080, 217.9030147174489969 ) ) ;
#107434 = DIRECTION ( 'NONE',  ( 9.500914144214121536E-47, -1.000000000000000000, 1.836970198721029688E-16 ) ) ;
#107435 = CARTESIAN_POINT ( 'NONE',  ( 25.50064889474995411, 1507.958245409381789, 199.2056517364818262 ) ) ;
#107436 = CARTESIAN_POINT ( 'NONE',  ( -2.304688949170010215, 1449.852729981760149, 182.9576120315739729 ) ) ;
#107437 = ORIENTED_EDGE ( 'NONE', *, *, #98607, .T. ) ;
#107438 = CIRCLE ( 'NONE', #78855, 1.999999950040888708 ) ;
#107439 = ORIENTED_EDGE ( 'NONE', *, *, #61737, .F. ) ;
#107440 = LINE ( 'NONE', #90638, #58294 ) ;
#107441 = CARTESIAN_POINT ( 'NONE',  ( 19.24176482687100176, 1456.016048631040121, 226.4226196092550083 ) ) ;
#107442 = CARTESIAN_POINT ( 'NONE',  ( -11.80724586129999842, 1434.031939626420126, 151.0333753425979921 ) ) ;
#107443 = AXIS2_PLACEMENT_3D ( 'NONE', #16885, #66261, #100378 ) ;
#107444 = CARTESIAN_POINT ( 'NONE',  ( -4.333209346896190216E-10, 1466.864290985080061, 244.5380620273480190 ) ) ;
#107445 = CARTESIAN_POINT ( 'NONE',  ( -33.93019615848938031, 1522.382868172863937, 220.5829544587965927 ) ) ;
#107446 = CARTESIAN_POINT ( 'NONE',  ( -15.06439020900000081, 1420.324155258209885, 212.5657008686889924 ) ) ;
#107447 = CARTESIAN_POINT ( 'NONE',  ( -108.9463587139999845, 1386.276479558989877, 311.0446671882590408 ) ) ;
#107448 = CARTESIAN_POINT ( 'NONE',  ( -7.937147302369870872, 1511.433279536600139, 214.9445374233650057 ) ) ;
#107449 = CARTESIAN_POINT ( 'NONE',  ( -10.96668869512642708, 1365.480022806811803, 207.6218459616987673 ) ) ;
#107450 = CARTESIAN_POINT ( 'NONE',  ( -45.66951489795039265, 1440.472176206239965, 266.1885706457709944 ) ) ;
#107451 = CARTESIAN_POINT ( 'NONE',  ( 13.94437673319849935, 1452.624323591719985, 223.0644266127340245 ) ) ;
#107452 = EDGE_CURVE ( 'NONE', #44905, #104774, #79398, .T. ) ;
#107453 = CARTESIAN_POINT ( 'NONE',  ( -0.01012492377659850000, 1516.989863902050047, 207.9939175986969815 ) ) ;
#107454 = CARTESIAN_POINT ( 'NONE',  ( -8.557097019430230489, 1448.618184358840153, 212.3365240749560030 ) ) ;
#107455 = CARTESIAN_POINT ( 'NONE',  ( 2.589250188618630322, 1407.329176837810110, 221.9615471100440232 ) ) ;
#107456 = CARTESIAN_POINT ( 'NONE',  ( -14.09108604789070185, 1436.127728589789967, 150.1512849377759835 ) ) ;
#107457 = CARTESIAN_POINT ( 'NONE',  ( -7.767268757120000089, 1385.037450386940009, 218.9155715650490208 ) ) ;
#107458 = DIRECTION ( 'NONE',  ( 1.755985294532464991E-16, -1.000000000000000000, 1.338183447452830017E-16 ) ) ;
#107459 = CARTESIAN_POINT ( 'NONE',  ( 7.164851019203979376, 1424.936393926430128, 212.9153315477099966 ) ) ;
#107460 = EDGE_LOOP ( 'NONE', ( #40219, #31317, #73917, #61804 ) ) ;
#107461 = CARTESIAN_POINT ( 'NONE',  ( 31.18244400170000219, 1434.782053685459914, 244.2061907803979750 ) ) ;
#107462 = CARTESIAN_POINT ( 'NONE',  ( -3.234068298869999580, 1415.020930770710038, 205.6238868179589758 ) ) ;
#107464 = CARTESIAN_POINT ( 'NONE',  ( -15.08187219341120056, 1512.240709848920005, 221.7951975401620075 ) ) ;
#107463 = CARTESIAN_POINT ( 'NONE',  ( 1.502583036259999894, 1464.119958549930061, 182.9892790823980135 ) ) ;
#107465 = CARTESIAN_POINT ( 'NONE',  ( -44.93136215053984728, 1435.581077993269218, 269.6838109711935090 ) ) ;
#107466 = CARTESIAN_POINT ( 'NONE',  ( -9.325404488320000240, 1417.437271135130004, 238.2842604422980060 ) ) ;
#107467 = CARTESIAN_POINT ( 'NONE',  ( -17.17241001986462123, 1523.382868172864164, 237.6251415217917895 ) ) ;
#107468 = CARTESIAN_POINT ( 'NONE',  ( -15.48003957830860067, 1452.372485493469867, 147.5117064112409935 ) ) ;
#107469 = CARTESIAN_POINT ( 'NONE',  ( -18.64646854149999911, 1416.843576337130116, 208.5596655672609927 ) ) ;
#107470 = ORIENTED_EDGE ( 'NONE', *, *, #59780, .F. ) ;
#107471 = DIRECTION ( 'NONE',  ( 0.2857341030884418265, -0.9583089388770653638, 7.461198772136227059E-07 ) ) ;
#107472 = CARTESIAN_POINT ( 'NONE',  ( 17.30126322264623084, 1523.462669333488975, 237.3930845918952741 ) ) ;
#107473 = CARTESIAN_POINT ( 'NONE',  ( 14.24651345449999873, 1509.423843874130171, 235.0733074521980086 ) ) ;
#107474 = ORIENTED_EDGE ( 'NONE', *, *, #53718, .F. ) ;
#107475 = ORIENTED_EDGE ( 'NONE', *, *, #91070, .T. ) ;
#107476 = CARTESIAN_POINT ( 'NONE',  ( -23.00263897809999847, 1384.817261601950122, 202.3843131321090141 ) ) ;
#107477 = CARTESIAN_POINT ( 'NONE',  ( -24.11493509802720325, 1410.987047801660083, 208.7879060775239850 ) ) ;
#107478 = ORIENTED_EDGE ( 'NONE', *, *, #69028, .T. ) ;
#107479 = CARTESIAN_POINT ( 'NONE',  ( -0.04536310503330000243, 1416.820969729929857, 227.2853261166980303 ) ) ;
#107480 = DIRECTION ( 'NONE',  ( 1.755985294532469921E-16, -1.000000000000000000, 1.338183447452831989E-16 ) ) ;
#107481 =( GEOMETRIC_REPRESENTATION_CONTEXT ( 3 ) GLOBAL_UNCERTAINTY_ASSIGNED_CONTEXT ( ( #67071 ) ) GLOBAL_UNIT_ASSIGNED_CONTEXT ( ( #33917, #102225, #60247 ) ) REPRESENTATION_CONTEXT ( 'NONE', 'WORKASPACE' ) );
#107482 = CARTESIAN_POINT ( 'NONE',  ( -2.903514209118760014, 1462.727859335829862, 184.2752576602030103 ) ) ;
#107483 = CARTESIAN_POINT ( 'NONE',  ( 0.7786186376918419194, 1443.353423969640062, 200.2227269049809877 ) ) ;
#107485 = ORIENTED_EDGE ( 'NONE', *, *, #61646, .T. ) ;
#107484 = EDGE_CURVE ( 'NONE', #18655, #80453, #42927, .T. ) ;
#107486 = EDGE_CURVE ( 'NONE', #345, #54152, #104479, .T. ) ;
#107487 = CARTESIAN_POINT ( 'NONE',  ( 45.51178678918370224, 1443.683907448070158, 268.9784073772149782 ) ) ;
#107488 = EDGE_CURVE ( 'NONE', #36910, #109511, #60852, .T. ) ;
#107489 = CARTESIAN_POINT ( 'NONE',  ( -12.37273845018560081, 1415.932840154009909, 221.9815680357259851 ) ) ;
#107490 = CARTESIAN_POINT ( 'NONE',  ( 0.1792131508849999777, 1419.175541713529810, 184.6431858978980074 ) ) ;
#107491 = CARTESIAN_POINT ( 'NONE',  ( 2.868433798504999910, 1517.020727862619879, 204.1095288638669842 ) ) ;
#107492 = VECTOR ( 'NONE', #13828, 1000.000000000000114 ) ;
#107493 = EDGE_LOOP ( 'NONE', ( #39607, #44447, #54320, #31064 ) ) ;
#107495 = ADVANCED_FACE ( 'NONE', ( #87240 ), #48297, .T. ) ;
#107494 = DIRECTION ( 'NONE',  ( 0.000000000000000000, 0.000000000000000000, 1.000000000000000000 ) ) ;
#107496 = B_SPLINE_CURVE_WITH_KNOTS ( 'NONE', 3,
 ( #78345, #85616, #8359, #42527, #35790, #27381, #17291, #2217, #70526, #34126, #102423, #68314, #25704, #77252, #59357, #93465, #8916, #43091, #3318, #45863, #37995, #72709, #98438, #87866, #30126, #72178, #54810, #11155, #90031, #53728, #19522, #46419, #88938, #62684, #13308, #47503, #45316, #71078, #79454, #2765, #79996, #37445, #4403, #106832, #12229, #71643, #105763, #29048, #64317, #21708, #36885, #55913, #106297, #80551, #105203, #81627, #28492, #54272, #29580, #96807, #62121, #63765, #81086, #63234, #97879, #20077, #88397, #38531, #11688, #97340, #21155, #12786, #20610, #3867, #55360, #89492, #46965, #4929, #39073 ),
 .UNSPECIFIED., .F., .F.,
 ( 4, 3, 3, 3, 3, 3, 3, 3, 3, 3, 3, 3, 3, 3, 3, 3, 3, 3, 3, 3, 3, 3, 3, 3, 3, 3, 4 ),
 ( 0.000000000000000000, 0.4544021449487510300, 0.9179962495654619969, 1.396393621504530058, 1.883881772313160008, 2.384423073347710087, 2.507852632510000124, 3.024297152344930684, 3.546339487294009718, 4.069687867730900521, 4.589703316606949635, 5.097876012234750398, 5.597257678202040232, 6.082185787997209658, 6.405353355340000832, 7.038449128034610425, 7.690329614618261367, 8.360401334715410471, 9.048938637463850299, 9.739081358835889546, 10.41820253846390010, 10.57568948873339920, 11.41685275061539961, 12.28892242647819977, 13.18071908141179982, 14.10021730575109977, 14.18573955799999986 ),
 .UNSPECIFIED. ) ;
#107497 = CARTESIAN_POINT ( 'NONE',  ( 6.195891505149140777, 1479.055035075845808, 200.6311094197622822 ) ) ;
#107498 = ORIENTED_EDGE ( 'NONE', *, *, #68263, .T. ) ;
#107499 = ORIENTED_EDGE ( 'NONE', *, *, #24066, .F. ) ;
#107500 = CARTESIAN_POINT ( 'NONE',  ( -10.53750713949369988, 1480.572745636769923, 208.8422318348939939 ) ) ;
#107501 = EDGE_CURVE ( 'NONE', #74953, #48466, #60471, .T. ) ;
#107502 = CARTESIAN_POINT ( 'NONE',  ( 4.832616789874995433, 1508.551704408610021, 205.6342609684716933 ) ) ;
#107503 = CARTESIAN_POINT ( 'NONE',  ( 4.672708027043240619, 1498.588723887579818, 198.5412103530289869 ) ) ;
#107504 = EDGE_CURVE ( 'NONE', #52145, #99066, #32212, .T. ) ;
#107505 = CARTESIAN_POINT ( 'NONE',  ( -13.52455581696280085, 1512.715996828740117, 193.8118672836219787 ) ) ;
#107506 = CARTESIAN_POINT ( 'NONE',  ( 11.58059658486819998, 1502.144060851190034, 214.4076140139739834 ) ) ;
#107507 = CARTESIAN_POINT ( 'NONE',  ( -1.657064955213390106E-05, 1410.034462405030126, 269.8654312530960055 ) ) ;
#107508 = CARTESIAN_POINT ( 'NONE',  ( -0.8218185942339699679, 1475.571559382040050, 220.5270802406460007 ) ) ;
#107509 = B_SPLINE_CURVE_WITH_KNOTS ( 'NONE', 3,
 ( #73000, #74654, #98731, #73559, #99265, #6330, #30976, #74105, #49452, #23114, #6870, #83575, #41027, #4681, #107692, #65152, #108235, #99822, #47239, #55660, #23673, #22543, #75205, #5795, #32083, #100388, #29872, #21993, #56185, #81926, #48912, #56745, #90881, #89782, #65702, #13052, #31523, #83039, #38820, #47789, #14168, #57318, #91445, #40481, #48353, #82493, #81367, #108791, #107134, #66271, #57856, #30426, #5229, #39936, #91985, #64613, #15260, #39382, #90322, #13602, #64060, #98179, #21449, #42695, #50551, #75749, #109894, #84675, #18020 ),
 .UNSPECIFIED., .F., .F.,
 ( 4, 2, 2, 1, 1, 2, 2, 2, 2, 1, 1, 1, 2, 2, 2, 2, 1, 1, 1, 2, 2, 2, 1, 1, 1, 1, 2, 2, 2, 1, 1, 1, 2, 2, 2, 1, 1, 2, 2, 2, 2, 2, 4 ),
 ( 0.000000000000000000, 0.06249999999907170090, 0.09374999999862482225, 0.1093749999984014037, 0.1171874999982728954, 0.1210937499981919879, 0.1249999999981110665, 0.1874999999972762066, 0.2187499999968588182, 0.2343749999966500963, 0.2421874999965457909, 0.2460937499965085429, 0.2480468749964898911, 0.2499999999964712116, 0.3124999999961673991, 0.3437499999960300090, 0.3593749999959603425, 0.3671874999959142127, 0.3710937499958910646, 0.3730468749958914532, 0.3749999999958918417, 0.4374999999964430120, 0.4687499999967315589, 0.4843749999968646747, 0.4921874999969201858, 0.4960937499969577114, 0.4980468749969765851, 0.4999999999969954034, 0.5624999999973115949, 0.5937499999974805709, 0.6093749999975639486, 0.6171874999976156850, 0.6210937499976517673, 0.6249999999976877385, 0.6874999999981096233, 0.7187499999983193444, 0.7343749999984254817, 0.7421874999984677812, 0.7499999999985099697, 0.8124999999988933297, 0.8437499999990838440, 0.8749999999992744693, 1.000000000000000000 ),
 .UNSPECIFIED. ) ;
#107510 = CARTESIAN_POINT ( 'NONE',  ( -20.40003431008743462, 1509.667963569866515, 230.7573408031066720 ) ) ;
#107511 = CARTESIAN_POINT ( 'NONE',  ( 0.01224639691883819444, 1408.939459843195209, 232.0643345525089103 ) ) ;
#107513 = CARTESIAN_POINT ( 'NONE',  ( -106.0556850682889944, 1391.049837136749829, 307.0681549835799728 ) ) ;
#107512 = CARTESIAN_POINT ( 'NONE',  ( -16.77483171992739841, 1414.364824855560073, 191.6397021085149959 ) ) ;
#107514 = CARTESIAN_POINT ( 'NONE',  ( 11.02997679787949892, 1425.732792483290041, 206.4966215837540062 ) ) ;
#107515 = CIRCLE ( 'NONE', #41346, 1.000000000000001332 ) ;
#107516 = CARTESIAN_POINT ( 'NONE',  ( -9.670994933606040789, 1440.251970265710042, 206.4953985460990111 ) ) ;
#107517 = CARTESIAN_POINT ( 'NONE',  ( 7.298550013359999866, 1430.724169039930075, 149.5003602673979799 ) ) ;
#107518 = ORIENTED_EDGE ( 'NONE', *, *, #24331, .F. ) ;
#107519 = CARTESIAN_POINT ( 'NONE',  ( -4.772433264290000032, 1461.586210710390105, 228.1254610687989839 ) ) ;
#107520 = CARTESIAN_POINT ( 'NONE',  ( -95.07483883942900604, 1384.957810138419973, 310.0626363712590319 ) ) ;
#107521 = CARTESIAN_POINT ( 'NONE',  ( -9.930017291230001319, 1389.522641720639967, 201.7040244565289981 ) ) ;
#107522 = CARTESIAN_POINT ( 'NONE',  ( 20.05523460210000053, 1476.340215940290136, 212.0965055883189905 ) ) ;
#107523 = ADVANCED_FACE ( 'NONE', ( #31732 ), #109117, .T. ) ;
#107525 = ORIENTED_EDGE ( 'NONE', *, *, #77112, .T. ) ;
#107524 = CARTESIAN_POINT ( 'NONE',  ( -15.68545621147730174, 1420.312772934420082, 210.6112538882230183 ) ) ;
#107526 = CARTESIAN_POINT ( 'NONE',  ( 3.249023004060000552, 1430.716676741390074, 218.0587861596190180 ) ) ;
#107527 = CONICAL_SURFACE ( 'NONE', #68241, 0.9999999999999930056, 0.7853981633970000820 ) ;
#107528 = FACE_OUTER_BOUND ( 'NONE', #11366, .T. ) ;
#107529 = CARTESIAN_POINT ( 'NONE',  ( -14.00913000090000082, 1416.839648763730111, 221.8523350387980031 ) ) ;
#107530 = CARTESIAN_POINT ( 'NONE',  ( 11.55605632620000200, 1433.836531958829937, 151.2482139994980059 ) ) ;
#107531 = CARTESIAN_POINT ( 'NONE',  ( 10.83195828224429214, 1414.913060387329779, 221.4508951956685792 ) ) ;
#107532 = CARTESIAN_POINT ( 'NONE',  ( 12.40160425683189871, 1414.913057846380070, 197.9605655507020003 ) ) ;
#107533 = EDGE_CURVE ( 'NONE', #48130, #63715, #8277, .T. ) ;
#107534 = CIRCLE ( 'NONE', #96846, 1.999999999999999556 ) ;
#107535 = CARTESIAN_POINT ( 'NONE',  ( 9.862951377358559313, 1519.551704408389924, 189.8497022443989977 ) ) ;
#107536 = CARTESIAN_POINT ( 'NONE',  ( -108.4312383940858382, 1388.726877007316716, 298.0798814299226365 ) ) ;
#107537 = EDGE_CURVE ( 'NONE', #59101, #54399, #4351, .T. ) ;
#107538 = CARTESIAN_POINT ( 'NONE',  ( 5.972257072449999704, 1422.095562574530049, 231.6255282193980065 ) ) ;
#107539 = DIRECTION ( 'NONE',  ( -0.9455185755993178454, 0.000000000000000000, 0.3255681544571539243 ) ) ;
#107540 = LINE ( 'NONE', #73403, #71766 ) ;
#107541 = CARTESIAN_POINT ( 'NONE',  ( -17.26894667200000200, 1409.516105293429973, 223.1920633181979952 ) ) ;
#107542 = DIRECTION ( 'NONE',  ( 0.000000000000000000, 1.000000000000000000, 0.000000000000000000 ) ) ;
#107543 = EDGE_CURVE ( 'NONE', #88970, #94093, #109840, .T. ) ;
#107544 = CARTESIAN_POINT ( 'NONE',  ( 20.19608870919999788, 1508.016571200030057, 189.3847908446980171 ) ) ;
#107545 = DIRECTION ( 'NONE',  ( -1.000000000000000000, 0.000000000000000000, 0.000000000000000000 ) ) ;
#107546 = CARTESIAN_POINT ( 'NONE',  ( -17.28494824625980186, 1410.440304317500022, 192.2716381327950046 ) ) ;
#107547 = CARTESIAN_POINT ( 'NONE',  ( -0.7147294630179988895, 1515.255091259190067, 204.7973799830389794 ) ) ;
#107548 = CARTESIAN_POINT ( 'NONE',  ( 12.47690690837549887, 1427.073077267369854, 206.5591765600709948 ) ) ;
#107549 = CARTESIAN_POINT ( 'NONE',  ( -2.515613211938379834, 1448.349718483709921, 188.5842421559209754 ) ) ;
#107550 = CARTESIAN_POINT ( 'NONE',  ( -10.26243781420000012, 1415.425644477229980, 223.2927970104979920 ) ) ;
#107551 = CARTESIAN_POINT ( 'NONE',  ( -19.64992912988063267, 1521.951704408389787, 210.5515370059081022 ) ) ;
#107552 = CARTESIAN_POINT ( 'NONE',  ( -10.96539760289999954, 1409.236356875930142, 199.6509366764479694 ) ) ;
#107553 = CARTESIAN_POINT ( 'NONE',  ( -16.73038498189999856, 1415.425582719929707, 203.0852499532379909 ) ) ;
#107554 = B_SPLINE_CURVE_WITH_KNOTS ( 'NONE', 3,
 ( #22788, #41278, #23360, #58093, #65950, #24451 ),
 .UNSPECIFIED., .F., .F.,
 ( 4, 2, 4 ),
 ( -1.285435071114701246E-05, 0.001079388306740486445, 0.002171630964192120157 ),
 .UNSPECIFIED. ) ;
#107555 = CARTESIAN_POINT ( 'NONE',  ( -28.90421869647610009, 1509.875083456920038, 211.4900521685889885 ) ) ;
#107556 = CARTESIAN_POINT ( 'NONE',  ( 13.19887955559999959, 1434.900409039649958, 147.6247122247980030 ) ) ;
#107557 = CARTESIAN_POINT ( 'NONE',  ( -34.92262157014030066, 1435.778361307009845, 134.0999999978019730 ) ) ;
#107558 = CARTESIAN_POINT ( 'NONE',  ( 4.053537042790000378, 1441.572390738320109, 183.3424090224980034 ) ) ;
#107559 = ORIENTED_EDGE ( 'NONE', *, *, #101568, .F. ) ;
#107560 = CARTESIAN_POINT ( 'NONE',  ( -16.54281257266368144, 1524.843416604514232, 180.8453930184409160 ) ) ;
#107561 = CARTESIAN_POINT ( 'NONE',  ( 2.880867337579580134, 1368.384084939549894, 207.8228488383560091 ) ) ;
#107562 = CARTESIAN_POINT ( 'NONE',  ( -104.4567500548372578, 1380.520305296903643, 307.5064808547090820 ) ) ;
#107563 = CARTESIAN_POINT ( 'NONE',  ( -12.02051124189999953, 1491.153688314190049, 206.6632161944989718 ) ) ;
#107564 = CARTESIAN_POINT ( 'NONE',  ( -0.1750448602389990116, 1463.552070523890052, 202.0965116382990061 ) ) ;
#107565 = CARTESIAN_POINT ( 'NONE',  ( 14.38486959344260008, 1507.535180641189982, 232.5758893386449984 ) ) ;
#107566 = CARTESIAN_POINT ( 'NONE',  ( 27.40305221345824549, 1413.568219286974681, 269.4051270913062694 ) ) ;
#107567 = CARTESIAN_POINT ( 'NONE',  ( 20.39519499389999879, 1453.159462793129933, 209.8471671030170000 ) ) ;
#107568 = CARTESIAN_POINT ( 'NONE',  ( -14.29022294670000015, 1380.323766294540064, 210.1136064056900068 ) ) ;
#107569 = CARTESIAN_POINT ( 'NONE',  ( 2.661139925880000145, 1428.713487558729867, 184.2796365262979918 ) ) ;
#107570 = CARTESIAN_POINT ( 'NONE',  ( -58.47517137479839988, 1385.054044359190129, 240.7570610490290051 ) ) ;
#107571 = AXIS2_PLACEMENT_3D ( 'NONE', #29808, #89714, #23041 ) ;
#107572 = CARTESIAN_POINT ( 'NONE',  ( -12.25240435165759934, 1490.361895997039937, 209.2004140072839959 ) ) ;
#107573 = CARTESIAN_POINT ( 'NONE',  ( -4.036901419354849807, 1508.551704408389924, 204.6714407391750115 ) ) ;
#107574 = CARTESIAN_POINT ( 'NONE',  ( -29.27865644980259674, 1509.812245390119870, 208.6395913010300092 ) ) ;
#107575 = CARTESIAN_POINT ( 'NONE',  ( -6.754078978114156584, 1512.913060387330006, 184.4732361498326156 ) ) ;
#107576 = CARTESIAN_POINT ( 'NONE',  ( -15.83290313645639991, 1409.465936823030006, 225.2763103180130031 ) ) ;
#107578 = ORIENTED_EDGE ( 'NONE', *, *, #43355, .T. ) ;
#107577 = LINE ( 'NONE', #91329, #21572 ) ;
#107579 = CARTESIAN_POINT ( 'NONE',  ( -109.9857366969999930, 1384.899971912069987, 311.4562997972589642 ) ) ;
#107580 = CARTESIAN_POINT ( 'NONE',  ( 9.901850170015880082, 1470.206455802750042, 211.0690064422630030 ) ) ;
#107581 = CARTESIAN_POINT ( 'NONE',  ( 23.10442899973940101, 1411.095127650270115, 207.3185325528490068 ) ) ;
#107582 = CARTESIAN_POINT ( 'NONE',  ( -109.2989494770000078, 1384.622952429599763, 311.2534360572589662 ) ) ;
#107583 = CARTESIAN_POINT ( 'NONE',  ( -0.3973340087122340103, 1418.672806152889962, 184.7148007238050127 ) ) ;
#107584 = CARTESIAN_POINT ( 'NONE',  ( -2.030806273019999773E-05, 1465.118916741829935, 238.1343320395980072 ) ) ;
#107585 = CARTESIAN_POINT ( 'NONE',  ( 22.94835125820000243, 1411.074625106729854, 213.6345867971880068 ) ) ;
#107586 = CARTESIAN_POINT ( 'NONE',  ( -2.668712174941869630, 1414.945758603789955, 186.3719431407839693 ) ) ;
#107587 = CARTESIAN_POINT ( 'NONE',  ( -16.58048539533550070, 1464.422290153699805, 220.5762272166699915 ) ) ;
#107588 = CARTESIAN_POINT ( 'NONE',  ( 5.805282093358999695, 1389.008761609309886, 209.1218459616989946 ) ) ;
#107590 = DIRECTION ( 'NONE',  ( -5.980589973904019347E-17, 1.000000000000000000, -1.736889445713099699E-16 ) ) ;
#107589 = CARTESIAN_POINT ( 'NONE',  ( -3.747637931291374347, 1511.538143005324173, 201.0064871382184890 ) ) ;
#107591 = CARTESIAN_POINT ( 'NONE',  ( 24.08291147301929769, 1411.090674609899906, 209.6339324557180248 ) ) ;
#107592 = CARTESIAN_POINT ( 'NONE',  ( -96.14154407968895555, 1340.114449826968894, 308.6286533442801101 ) ) ;
#107593 = CARTESIAN_POINT ( 'NONE',  ( 17.84054676580441168, 1523.580203803270933, 237.8810931560534243 ) ) ;
#107594 = CARTESIAN_POINT ( 'NONE',  ( -21.10523119420000171, 1505.940419546890098, 209.1830678612959957 ) ) ;
#107595 = CARTESIAN_POINT ( 'NONE',  ( 8.476942927309998765, 1362.523913559719858, 210.6218459616991936 ) ) ;
#107596 = EDGE_CURVE ( 'NONE', #44597, #59669, #13622, .T. ) ;
#107597 = AXIS2_PLACEMENT_3D ( 'NONE', #8963, #59397, #93508 ) ;
#107598 = CARTESIAN_POINT ( 'NONE',  ( -5.011367984924999242, 1516.974592746400049, 205.6720686163770324 ) ) ;
#107599 = CARTESIAN_POINT ( 'NONE',  ( -3.320716570817880076, 1484.261045064220070, 183.3706358249989989 ) ) ;
#107600 = ORIENTED_EDGE ( 'NONE', *, *, #72798, .F. ) ;
#107601 = DIRECTION ( 'NONE',  ( 0.000000000000000000, 1.000000000000000000, 0.000000000000000000 ) ) ;
#107602 = CARTESIAN_POINT ( 'NONE',  ( -4.227936195309520251, 1441.550847847370051, 165.4924148592990036 ) ) ;
#107604 = ORIENTED_EDGE ( 'NONE', *, *, #98663, .T. ) ;
#107603 = CARTESIAN_POINT ( 'NONE',  ( -67.63909761182219427, 1379.745505766160022, 278.9989825627670257 ) ) ;
#107605 = ORIENTED_EDGE ( 'NONE', *, *, #101526, .F. ) ;
#107606 = CARTESIAN_POINT ( 'NONE',  ( 28.01396353250000004, 1509.154209357430091, 211.9611640590480022 ) ) ;
#107607 = VERTEX_POINT ( 'NONE', #83245 ) ;
#107608 = CARTESIAN_POINT ( 'NONE',  ( -0.03631497420734799975, 1485.874503519110021, 221.0111561022920057 ) ) ;
#107609 = CARTESIAN_POINT ( 'NONE',  ( -19.53984293939999972, 1410.902666576429965, 197.4202668715979883 ) ) ;
#107611 = CARTESIAN_POINT ( 'NONE',  ( 0.5133626083067620582, 1410.311097044259895, 185.0719925509139898 ) ) ;
#107610 = CARTESIAN_POINT ( 'NONE',  ( -11.73792004973664227, 1426.279486323856190, 144.2703440561577395 ) ) ;
#107612 = CARTESIAN_POINT ( 'NONE',  ( -2.476170635034999901, 1516.819260244609950, 210.8389306816469855 ) ) ;
#107613 =( BOUNDED_CURVE ( )  B_SPLINE_CURVE ( 3, ( #44966, #61768, #105403, #20822 ),
 .UNSPECIFIED., .F., .T. ) 
 B_SPLINE_CURVE_WITH_KNOTS ( ( 4, 4 ),
 ( 2.550106748235465126, 2.860742008493075250 ),
 .UNSPECIFIED. ) 
 CURVE ( )  GEOMETRIC_REPRESENTATION_ITEM ( )  RATIONAL_B_SPLINE_CURVE ( ( 1.000000000000000000, 0.9919749634430294893, 0.9919749634430294893, 1.000000000000000000 ) ) 
 REPRESENTATION_ITEM ( '' )  );
#107614 = CIRCLE ( 'NONE', #41519, 2.000000000000003553 ) ;
#107615 = ADVANCED_FACE ( 'NONE', ( #29530 ), #42760, .T. ) ;
#107616 = CARTESIAN_POINT ( 'NONE',  ( -25.50355197240790162, 1451.146063814939907, 136.9902061369730291 ) ) ;
#107617 = CARTESIAN_POINT ( 'NONE',  ( -11.73652925620000076, 1426.280330920429833, 144.1708004945979837 ) ) ;
#107618 = CARTESIAN_POINT ( 'NONE',  ( -14.42577973733840047, 1379.717605820849940, 208.2725693216679872 ) ) ;
#107619 = CARTESIAN_POINT ( 'NONE',  ( 10.53166116164130095, 1481.128123199839820, 211.0446672586460011 ) ) ;
#107620 = APPLICATION_PROTOCOL_DEFINITION ( 'draft international standard', 'automotive_design', 1998, #104952 ) ;
#107621 = CARTESIAN_POINT ( 'NONE',  ( 4.869069343142859552, 1508.551704408389924, 212.3687905588049887 ) ) ;
#107622 = B_SPLINE_CURVE_WITH_KNOTS ( 'NONE', 3,
 ( #108940, #92673, #50151, #7574, #75888, #25454, #23259 ),
 .UNSPECIFIED., .F., .F.,
 ( 4, 3, 4 ),
 ( -167.5289128750000032, -131.9184636301120008, -78.04659651044040913 ),
 .UNSPECIFIED. ) ;
#107623 = CARTESIAN_POINT ( 'NONE',  ( -39.96762391852740137, 1441.625738433479910, 136.8927567948610147 ) ) ;
#107624 = ORIENTED_EDGE ( 'NONE', *, *, #76153, .F. ) ;
#107625 = CARTESIAN_POINT ( 'NONE',  ( -5.221955787189999754, 1489.269541098190075, 185.8916489435990229 ) ) ;
#107626 = CARTESIAN_POINT ( 'NONE',  ( -17.12015143466543066, 1526.107880201381477, 235.9348175143726394 ) ) ;
#107627 = ORIENTED_EDGE ( 'NONE', *, *, #55579, .T. ) ;
#107628 = ORIENTED_EDGE ( 'NONE', *, *, #103447, .F. ) ;
#107629 = CARTESIAN_POINT ( 'NONE',  ( 13.81770597796416666, 1410.768353600875116, 228.1343084947812088 ) ) ;
#107630 = CARTESIAN_POINT ( 'NONE',  ( 16.77415063058788292, 1513.652806712936126, 195.7035532396738517 ) ) ;
#107631 = CARTESIAN_POINT ( 'NONE',  ( 12.26246110829129954, 1499.794402872200180, 205.9643549718410043 ) ) ;
#107632 = CARTESIAN_POINT ( 'NONE',  ( -3.127789639369999986, 1485.522978138030112, 182.9202317313979904 ) ) ;
#107633 = CARTESIAN_POINT ( 'NONE',  ( -2.500000000000000000, 1439.522697816390064, 164.2180430355600151 ) ) ;
#107634 = CIRCLE ( 'NONE', #28911, 1.000000000039231285 ) ;
#107635 = FACE_OUTER_BOUND ( 'NONE', #97365, .T. ) ;
#107636 = CARTESIAN_POINT ( 'NONE',  ( -63.57354255950622957, 1379.735521214616938, 269.2845494244093629 ) ) ;
#107637 = CARTESIAN_POINT ( 'NONE',  ( -0.1906498135749990219, 1465.356101280390021, 198.0942218014990033 ) ) ;
#107638 = EDGE_CURVE ( 'NONE', #28487, #35481, #21558, .T. ) ;
#107639 = CARTESIAN_POINT ( 'NONE',  ( 30.29107669316897855, 1523.847248782568613, 222.4926083572483151 ) ) ;
#107640 = CARTESIAN_POINT ( 'NONE',  ( 12.37274144529999909, 1415.932840167130053, 196.2621264754979791 ) ) ;
#107641 = CARTESIAN_POINT ( 'NONE',  ( -71.90316716507038564, 1384.749119938380090, 269.7490035479099788 ) ) ;
#107642 = ORIENTED_EDGE ( 'NONE', *, *, #63868, .F. ) ;
#107643 = AXIS2_PLACEMENT_3D ( 'NONE', #74298, #30619, #55847 ) ;
#107644 = CARTESIAN_POINT ( 'NONE',  ( 9.146299198640271300, 1461.861878385089767, 205.8341600298289791 ) ) ;
#107645 = CARTESIAN_POINT ( 'NONE',  ( -4.626591905484999323, 1517.096587378560116, 207.4170511287669854 ) ) ;
#107646 = ORIENTED_EDGE ( 'NONE', *, *, #10056, .T. ) ;
#107647 = CARTESIAN_POINT ( 'NONE',  ( 35.79086060848550233, 1440.913060387330006, 261.9942551139580473 ) ) ;
#107648 = CARTESIAN_POINT ( 'NONE',  ( -0.0001992799835346449090, 1452.696936729286335, 153.3245174021012076 ) ) ;
#107649 = ORIENTED_EDGE ( 'NONE', *, *, #13601, .T. ) ;
#107650 = CARTESIAN_POINT ( 'NONE',  ( -0.2439063137306309859, 1452.338815250500147, 183.2775397759450016 ) ) ;
#107651 = DIRECTION ( 'NONE',  ( -0.02616798426500965835, 0.9993150019883683122, 0.02616798426500955774 ) ) ;
#107652 = CARTESIAN_POINT ( 'NONE',  ( -17.96672434486609760, 1508.456899395794380, 211.9397210758587562 ) ) ;
#107653 = CARTESIAN_POINT ( 'NONE',  ( -2.919621720534709919, 1419.522956690290130, 186.2043860719099939 ) ) ;
#107654 = CARTESIAN_POINT ( 'NONE',  ( -13.04207679966010147, 1409.368499744919745, 225.9431846064669855 ) ) ;
#107655 = CARTESIAN_POINT ( 'NONE',  ( -22.08622291482314282, 1512.187213306747481, 233.8253038720786776 ) ) ;
#107656 = CARTESIAN_POINT ( 'NONE',  ( -2.162510980229999991, 1508.218318618129842, 180.6352365529979807 ) ) ;
#107657 = CARTESIAN_POINT ( 'NONE',  ( -6.191282293671606318, 1510.848430435494720, 201.6637636903093949 ) ) ;
#107658 = CARTESIAN_POINT ( 'NONE',  ( 26.11817593136069604, 1491.282851520119948, 206.2269962030060242 ) ) ;
#107659 = ADVANCED_FACE ( 'NONE', ( #16553 ), #42343, .T. ) ;
#107661 = CARTESIAN_POINT ( 'NONE',  ( -11.60004869883471557, 1424.776443364156648, 137.5692383712261062 ) ) ;
#107660 = CARTESIAN_POINT ( 'NONE',  ( 17.13490080239999713, 1458.470257116130142, 230.0791330072979974 ) ) ;
#107662 = CARTESIAN_POINT ( 'NONE',  ( -4.846113964861681112, 1422.339154117763201, 184.7758569840760572 ) ) ;
#107663 = CARTESIAN_POINT ( 'NONE',  ( -2.872208748294999836, 1517.145312756229941, 216.4596396827270155 ) ) ;
#107664 = ADVANCED_FACE ( 'NONE', ( #373 ), #50743, .F. ) ;
#107665 = FACE_OUTER_BOUND ( 'NONE', #2712, .T. ) ;
#107666 = CARTESIAN_POINT ( 'NONE',  ( -0.1360155611962030053, 1507.785361668840096, 180.7547526672690026 ) ) ;
#107667 = CARTESIAN_POINT ( 'NONE',  ( 18.49405840734494078, 1446.012071220772441, 215.4331772447790740 ) ) ;
#107669 = B_SPLINE_CURVE_WITH_KNOTS ( 'NONE', 3,
 ( #89732, #55608, #38770, #56691, #72944, #90827 ),
 .UNSPECIFIED., .F., .F.,
 ( 4, 2, 4 ),
 ( 0.003574833876271631995, 0.004151067118842836218, 0.004727300361414039573 ),
 .UNSPECIFIED. ) ;
#107668 = CARTESIAN_POINT ( 'NONE',  ( -4.029572678834999699, 1516.858649670339901, 213.1633184439769764 ) ) ;
#107670 = CARTESIAN_POINT ( 'NONE',  ( 18.55728982200000132, 1509.324399912330136, 187.7614924380980028 ) ) ;
#107671 = CARTESIAN_POINT ( 'NONE',  ( -11.60004869885203682, 1426.116538955981241, 139.0982239796293527 ) ) ;
#107673 = ORIENTED_EDGE ( 'NONE', *, *, #2359, .T. ) ;
#107672 = CARTESIAN_POINT ( 'NONE',  ( -11.50563503569702029, 1508.158922853092690, 207.5673892822083531 ) ) ;
#107674 = CARTESIAN_POINT ( 'NONE',  ( -2.596261494520234248, 1525.907212628473644, 177.4701144822248011 ) ) ;
#107675 = CARTESIAN_POINT ( 'NONE',  ( 2.317514236480000100, 1508.438296843690068, 220.2276651528989930 ) ) ;
#107676 = CARTESIAN_POINT ( 'NONE',  ( -11.55594655870000054, 1430.767682321529946, 151.0182484257979922 ) ) ;
#107677 = DIRECTION ( 'NONE',  ( 0.000000000000000000, -1.000000000000000000, 0.000000000000000000 ) ) ;
#107678 = CARTESIAN_POINT ( 'NONE',  ( -7.825739482554860516, 1440.186617985560133, 204.8166144522810157 ) ) ;
#107679 = CARTESIAN_POINT ( 'NONE',  ( -20.22359736010910325, 1485.406499196400091, 187.9853393324099784 ) ) ;
#107680 = DIRECTION ( 'NONE',  ( -1.755985294532469921E-16, 1.000000000000000000, -1.338183447452831989E-16 ) ) ;
#107681 = EDGE_CURVE ( 'NONE', #23279, #54088, #19736, .T. ) ;
#107682 = CARTESIAN_POINT ( 'NONE',  ( -8.588755447433969792, 1437.818850531529961, 207.9413692731380081 ) ) ;
#107684 = CARTESIAN_POINT ( 'NONE',  ( -3.187593557069610117, 1421.874555467776645, 137.0999999977043728 ) ) ;
#107683 = CARTESIAN_POINT ( 'NONE',  ( -19.94616634080000139, 1444.802756643080102, 224.2822642680980039 ) ) ;
#107685 = CARTESIAN_POINT ( 'NONE',  ( -1.808741800610000006, 1485.212281157229882, 182.6012063751979895 ) ) ;
#107686 = ORIENTED_EDGE ( 'NONE', *, *, #51811, .F. ) ;
#107687 = CARTESIAN_POINT ( 'NONE',  ( -6.947377821305000367, 1517.009964551830080, 204.5062011277169916 ) ) ;
#107688 = CARTESIAN_POINT ( 'NONE',  ( 4.970023385829999363, 1406.187660922729947, 266.9514890597980070 ) ) ;
#107689 = EDGE_CURVE ( 'NONE', #36047, #75555, #53749, .T. ) ;
#107690 = DIRECTION ( 'NONE',  ( 0.000000000000000000, 0.000000000000000000, 1.000000000000000000 ) ) ;
#107691 = CARTESIAN_POINT ( 'NONE',  ( 18.46986075919999948, 1410.877533305329962, 194.2880693953979971 ) ) ;
#107692 = CARTESIAN_POINT ( 'NONE',  ( 24.29957117401547961, 1437.103412567565329, 213.1125009194426809 ) ) ;
#107693 = CARTESIAN_POINT ( 'NONE',  ( 2.137144914719688593, 1464.211915265456355, 199.5352916986041976 ) ) ;
#107694 = CARTESIAN_POINT ( 'NONE',  ( 11.60004869885204037, 1423.119116085875930, 136.9990592530850506 ) ) ;
#107695 = AXIS2_PLACEMENT_3D ( 'NONE', #53174, #10611, #71098 ) ;
#107696 = CARTESIAN_POINT ( 'NONE',  ( -6.648038047673147766, 1439.929303981514749, 203.4146418879364830 ) ) ;
#107697 = CARTESIAN_POINT ( 'NONE',  ( -0.8729612245483540089, 1450.882575899840049, 154.5162482229659986 ) ) ;
#107698 = CARTESIAN_POINT ( 'NONE',  ( -12.29575077220000168, 1445.147283749560074, 186.2458169469979907 ) ) ;
#107699 = CARTESIAN_POINT ( 'NONE',  ( -19.81676069552977282, 1485.772319128206391, 190.4006065858834518 ) ) ;
#107700 = CARTESIAN_POINT ( 'NONE',  ( -1.754420609230000094, 1507.305123787589991, 221.4484239625990085 ) ) ;
#107701 = CYLINDRICAL_SURFACE ( 'NONE', #110455, 1.455175085940062507 ) ;
#107702 = CARTESIAN_POINT ( 'NONE',  ( -15.71554773450000297, 1429.441490235930132, 224.8635562088979896 ) ) ;
#107703 = CARTESIAN_POINT ( 'NONE',  ( 22.69876404240098111, 1501.977400791986611, 236.8953202675778016 ) ) ;
#107704 = CARTESIAN_POINT ( 'NONE',  ( 2.500000002460000204, 1440.023046414310102, 162.2537046324979997 ) ) ;
#107705 = CARTESIAN_POINT ( 'NONE',  ( -2.772197528860000038, 1475.921741880330046, 267.2318177738980012 ) ) ;
#107706 = CARTESIAN_POINT ( 'NONE',  ( -11.03641823134053723, 1425.191710119871232, 138.6345187158980252 ) ) ;
#107707 = CARTESIAN_POINT ( 'NONE',  ( -17.63857530519999983, 1411.941882070129850, 193.4046992581980078 ) ) ;
#107708 = CARTESIAN_POINT ( 'NONE',  ( -20.71343476517491311, 1512.187213306747481, 238.3377464195766890 ) ) ;
#107709 = CARTESIAN_POINT ( 'NONE',  ( -24.59239876478699927, 1384.847462785510061, 223.4254781314130014 ) ) ;
#107710 = CARTESIAN_POINT ( 'NONE',  ( 1.455000209906389896, 1507.073729425429974, 236.7651043255590082 ) ) ;
#107711 = VECTOR ( 'NONE', #25560, 1000.000000000000000 ) ;
#107712 = CARTESIAN_POINT ( 'NONE',  ( 12.24150297172569957, 1416.512142028610015, 223.5518725947510177 ) ) ;
#107713 = CARTESIAN_POINT ( 'NONE',  ( -105.3194880639999980, 1379.015581655369942, 303.4536826814589858 ) ) ;
#107714 = FACE_OUTER_BOUND ( 'NONE', #60414, .T. ) ;
#107715 = CARTESIAN_POINT ( 'NONE',  ( -14.38276615813130022, 1509.537722091349906, 182.7943691049900110 ) ) ;
#107716 = CARTESIAN_POINT ( 'NONE',  ( -19.69424761119999800, 1410.523354731429890, 197.7052557853979806 ) ) ;
#107717 = B_SPLINE_CURVE_WITH_KNOTS ( 'NONE', 3,
 ( #74873, #32837, #109024, #33383, #77077, #40702, #101137, #24431, #59722, #15477 ),
 .UNSPECIFIED., .F., .F.,
 ( 4, 2, 2, 2, 4 ),
 ( -0.1358553352198900166, -0.1155267796648780099, -0.07212482838321790379, -0.03632190733730258914, -3.752851029936721261E-09 ),
 .UNSPECIFIED. ) ;
#107718 = CARTESIAN_POINT ( 'NONE',  ( 12.80045406827199983, 1421.352217623579918, 205.8583691802969895 ) ) ;
#107719 = CARTESIAN_POINT ( 'NONE',  ( 31.81407709660768646, 1522.862737210649811, 196.2902540610627682 ) ) ;
#107720 = ORIENTED_EDGE ( 'NONE', *, *, #6539, .F. ) ;
#107721 = CARTESIAN_POINT ( 'NONE',  ( -19.83329619529999732, 1467.071755593990019, 210.0771979357010082 ) ) ;
#107722 = CARTESIAN_POINT ( 'NONE',  ( 3.217370068945899941, 1424.184623523179880, 188.9579833762999783 ) ) ;
#107724 = CARTESIAN_POINT ( 'NONE',  ( -11.12931925036500047, 1512.151624459629829, 193.3374815694669735 ) ) ;
#107723 = CARTESIAN_POINT ( 'NONE',  ( 11.11916130470000041, 1425.182366623929965, 141.8404308875980178 ) ) ;
#107725 = CARTESIAN_POINT ( 'NONE',  ( 17.34064885126017685, 1525.506916460683669, 236.9219916297327018 ) ) ;
#107726 = CARTESIAN_POINT ( 'NONE',  ( -6.923625731939999639, 1452.810235840890073, 202.5026240206190096 ) ) ;
#107727 = EDGE_CURVE ( 'NONE', #1510, #2790, #39403, .T. ) ;
#107728 = CARTESIAN_POINT ( 'NONE',  ( -5.005071046424999892, 1516.710692850270107, 201.7963041449669959 ) ) ;
#107729 = CARTESIAN_POINT ( 'NONE',  ( 8.061555088029999538, 1427.901936262589970, 212.7968812046490257 ) ) ;
#107730 = CARTESIAN_POINT ( 'NONE',  ( -21.46486174369999844, 1504.440211354589792, 215.6677629392290214 ) ) ;
#107731 = CARTESIAN_POINT ( 'NONE',  ( 15.48184689783500012, 1513.486273623730085, 194.4742589842670100 ) ) ;
#107732 = FACE_BOUND ( 'NONE', #68359, .T. ) ;
#107733 = CARTESIAN_POINT ( 'NONE',  ( -11.16990621730810140, 1377.949346146600192, 211.9847173479319906 ) ) ;
#107734 = CARTESIAN_POINT ( 'NONE',  ( 7.474134278654832819, 1365.552169080253861, 209.6218459617148824 ) ) ;
#107736 = ORIENTED_EDGE ( 'NONE', *, *, #49063, .F. ) ;
#107735 = CARTESIAN_POINT ( 'NONE',  ( -19.29089395862319734, 1379.713382923030167, 212.5251929917019993 ) ) ;
#107737 = ORIENTED_EDGE ( 'NONE', *, *, #58534, .F. ) ;
#107738 = CARTESIAN_POINT ( 'NONE',  ( -14.29155582609999975, 1442.454908126789860, 188.8169266407979876 ) ) ;
#107739 = CARTESIAN_POINT ( 'NONE',  ( -20.92480426329999688, 1409.643770653630099, 213.2359878676279834 ) ) ;
#107740 = LINE ( 'NONE', #47289, #84240 ) ;
#107741 = CARTESIAN_POINT ( 'NONE',  ( -13.29164969346664193, 1444.599138759567268, 169.3795078411781105 ) ) ;
#107742 = CARTESIAN_POINT ( 'NONE',  ( -25.31823295080000236, 1509.573488454329890, 197.1833682395979679 ) ) ;
#107743 = CARTESIAN_POINT ( 'NONE',  ( -15.54057306903361102, 1416.153203235703131, 210.7896593000916994 ) ) ;
#107745 = CARTESIAN_POINT ( 'NONE',  ( -1.359675940647320003, 1412.718853561030073, 185.5028861769010007 ) ) ;
#107744 = CARTESIAN_POINT ( 'NONE',  ( 2.978012241769999680, 1445.410371645589976, 200.4888750985090269 ) ) ;
#107746 = EDGE_CURVE ( 'NONE', #58393, #36440, #98455, .T. ) ;
#107747 = CARTESIAN_POINT ( 'NONE',  ( 2.642385910419999817, 1429.770789213729813, 184.7597551400980080 ) ) ;
#107748 = CARTESIAN_POINT ( 'NONE',  ( -7.681064681269999639, 1415.931669658029932, 192.6807567567980186 ) ) ;
#107749 = CARTESIAN_POINT ( 'NONE',  ( -40.94874006156769752, 1446.742020086070170, 136.1409490009270087 ) ) ;
#107750 = PRESENTATION_STYLE_ASSIGNMENT (( #99880 ) ) ;
#107751 = CARTESIAN_POINT ( 'NONE',  ( 10.06792015711779875, 1396.264639913020119, 204.5271174533559986 ) ) ;
#107752 = CARTESIAN_POINT ( 'NONE',  ( 0.7440358369610000633, 1416.274718422629803, 190.3966560648979964 ) ) ;
#107753 = CARTESIAN_POINT ( 'NONE',  ( 11.75171807110000088, 1426.266890984929887, 145.3097295381980132 ) ) ;
#107754 = CARTESIAN_POINT ( 'NONE',  ( 40.71506682779999409, 1443.618738319280055, 137.1015903996979830 ) ) ;
#107755 = ORIENTED_EDGE ( 'NONE', *, *, #26767, .T. ) ;
#107756 = CARTESIAN_POINT ( 'NONE',  ( -16.73628186595857059, 1526.382868172864164, 184.0591879540917546 ) ) ;
#107757 = CARTESIAN_POINT ( 'NONE',  ( 21.92050665148286370, 1524.523992613103701, 233.6743653272424979 ) ) ;
#107758 = VERTEX_POINT ( 'NONE', #90333 ) ;
#107759 = ORIENTED_EDGE ( 'NONE', *, *, #103754, .T. ) ;
#107760 = CARTESIAN_POINT ( 'NONE',  ( -38.60872993109999385, 1443.613625523540122, 137.1750381502980076 ) ) ;
#107761 = CARTESIAN_POINT ( 'NONE',  ( 7.445922712490000706, 1367.935115748530052, 207.6218459616989946 ) ) ;
#107762 = CARTESIAN_POINT ( 'NONE',  ( -12.78657892559999887, 1416.813004075630033, 195.9657752819979919 ) ) ;
#107763 = CARTESIAN_POINT ( 'NONE',  ( -29.36670733769854991, 1526.000688113720798, 197.3383209345158491 ) ) ;
#107764 = CARTESIAN_POINT ( 'NONE',  ( 3.261635932824999973, 1516.613881697390070, 216.0569793506570022 ) ) ;
#107765 = CARTESIAN_POINT ( 'NONE',  ( -12.33083890915290048, 1378.999358067989988, 209.7207202901829817 ) ) ;
#107766 = ORIENTED_EDGE ( 'NONE', *, *, #63840, .T. ) ;
#107767 = CARTESIAN_POINT ( 'NONE',  ( -12.33148714679999891, 1502.584565209489938, 208.9079283441639916 ) ) ;
#107768 = CARTESIAN_POINT ( 'NONE',  ( 2.500000000000000000, 1448.458776228290162, 161.2301877404750030 ) ) ;
#107769 = CARTESIAN_POINT ( 'NONE',  ( -29.97486656939999961, 1379.299027991060029, 213.1946222551189862 ) ) ;
#107770 = CARTESIAN_POINT ( 'NONE',  ( 18.89907699009999931, 1416.828040557830036, 210.6687202295679811 ) ) ;
#107771 = CARTESIAN_POINT ( 'NONE',  ( 2.284199363404999961, 1516.940296199220029, 205.8526610237369994 ) ) ;
#107772 = ORIENTED_EDGE ( 'NONE', *, *, #32373, .T. ) ;
#107773 = CARTESIAN_POINT ( 'NONE',  ( 5.011551368014999674, 1517.080322339569875, 209.8587501411369942 ) ) ;
#107774 = CARTESIAN_POINT ( 'NONE',  ( -9.003774537682598833, 1451.190698364410082, 206.9733706270170046 ) ) ;
#107775 = EDGE_CURVE ( 'NONE', #41473, #35962, #76983, .T. ) ;
#107776 = CARTESIAN_POINT ( 'NONE',  ( -16.20545877105858423, 1412.767257293050761, 269.3699492879471222 ) ) ;
#107777 = CARTESIAN_POINT ( 'NONE',  ( -1.271723871399999872, 1409.895803293729841, 232.9734008183979768 ) ) ;
#107778 = EDGE_CURVE ( 'NONE', #91418, #103319, #31104, .T. ) ;
#107780 = EDGE_LOOP ( 'NONE', ( #102865, #3183, #91155, #5841 ) ) ;
#107779 = CARTESIAN_POINT ( 'NONE',  ( -3.871411596960000256, 1475.513060387329915, 188.6584480527980077 ) ) ;
#107781 = CARTESIAN_POINT ( 'NONE',  ( 2.500000000000000000, 1421.615752562629950, 151.7766360386979727 ) ) ;
#107782 = CARTESIAN_POINT ( 'NONE',  ( -27.10898335609390131, 1440.913060414239908, 227.3295655018380046 ) ) ;
#107783 = CARTESIAN_POINT ( 'NONE',  ( -96.27487712110000473, 1383.766385264410019, 310.4021576922589816 ) ) ;
#107784 = CARTESIAN_POINT ( 'NONE',  ( -0.2823795768692209940, 1467.126800852679935, 235.6211964996780068 ) ) ;
#107785 = EDGE_CURVE ( 'NONE', #31171, #6800, #47801, .T. ) ;
#107786 = CARTESIAN_POINT ( 'NONE',  ( 8.103047004457721414, 1409.756119192850065, 270.3694257726410228 ) ) ;
#107787 = CARTESIAN_POINT ( 'NONE',  ( -4.028307778284999863, 1516.797038924770050, 212.3881954442970255 ) ) ;
#107788 = CARTESIAN_POINT ( 'NONE',  ( -47.76848070539999469, 1379.673518999439921, 235.2760716095589828 ) ) ;
#107789 = EDGE_CURVE ( 'NONE', #29868, #8432, #86655, .T. ) ;
#107790 = CARTESIAN_POINT ( 'NONE',  ( 24.09245823930000086, 1410.845047763129969, 209.4791609914190076 ) ) ;
#107791 = CARTESIAN_POINT ( 'NONE',  ( -20.01067139950000140, 1507.877425041529932, 188.9709217985979706 ) ) ;
#107792 = CARTESIAN_POINT ( 'NONE',  ( 12.13997568453070031, 1492.634789084120030, 211.4080700421230006 ) ) ;
#107793 = CARTESIAN_POINT ( 'NONE',  ( -7.711161960695579687, 1516.615653621549882, 210.3347488552499840 ) ) ;
#107794 = CARTESIAN_POINT ( 'NONE',  ( 5.014195101815000832, 1517.120861839400050, 210.8273123806970091 ) ) ;
#107795 = CARTESIAN_POINT ( 'NONE',  ( 0.3019365487449059970, 1424.316146906500080, 227.5104060230709990 ) ) ;
#107796 = CARTESIAN_POINT ( 'NONE',  ( 15.08448175589999884, 1409.953164874830009, 191.7150831455979869 ) ) ;
#107797 = CARTESIAN_POINT ( 'NONE',  ( -96.24310955420000369, 1384.607824056739901, 310.5744048422590140 ) ) ;
#107799 = ORIENTED_EDGE ( 'NONE', *, *, #55094, .T. ) ;
#107798 = CARTESIAN_POINT ( 'NONE',  ( -32.10879564089999860, 1385.224147136040074, 229.9470470709589733 ) ) ;
#107800 = CARTESIAN_POINT ( 'NONE',  ( -47.10980919147239376, 1385.139645660309952, 255.7820939229709722 ) ) ;
#107801 = CARTESIAN_POINT ( 'NONE',  ( 0.7024623020930000905, 1417.310603422230088, 234.7649661555979890 ) ) ;
#107802 = DIRECTION ( 'NONE',  ( -1.000000000000000000, 0.000000000000000000, 0.000000000000000000 ) ) ;
#107803 = CARTESIAN_POINT ( 'NONE',  ( 10.38136293079987027, 1472.225397094090113, 214.0145097960788689 ) ) ;
#107804 = CARTESIAN_POINT ( 'NONE',  ( 12.92606856909999991, 1421.113610090889779, 204.2842550098989989 ) ) ;
#107805 = CARTESIAN_POINT ( 'NONE',  ( -2.753739293390117471, 1497.642705930136572, 198.1704566312156999 ) ) ;
#107807 = DIRECTION ( 'NONE',  ( -0.03489949451910427658, -0.1170788569999639955, 0.9925092274260693959 ) ) ;
#107806 = CARTESIAN_POINT ( 'NONE',  ( -5.778999811904999895, 1516.955859323880077, 216.4549161051170074 ) ) ;
#107808 = CARTESIAN_POINT ( 'NONE',  ( -1.027716997790000031, 1461.008287043790233, 228.8024499230989761 ) ) ;
#107809 = CARTESIAN_POINT ( 'NONE',  ( 1.250333271336267371, 1515.565566433146614, 205.1761050331341494 ) ) ;
#107810 = ORIENTED_EDGE ( 'NONE', *, *, #103447, .T. ) ;
#107811 = CARTESIAN_POINT ( 'NONE',  ( 3.259729297834999873, 1517.119374999550018, 201.7846921639870175 ) ) ;
#107812 = EDGE_CURVE ( 'NONE', #98568, #79053, #71207, .T. ) ;
#107813 = CARTESIAN_POINT ( 'NONE',  ( -15.78436440076499991, 1512.151624459629829, 220.2511651824670196 ) ) ;
#107814 = ORIENTED_EDGE ( 'NONE', *, *, #105925, .F. ) ;
#107815 = CARTESIAN_POINT ( 'NONE',  ( 3.246772394788723481, 1512.187213306747481, 241.0944358625217774 ) ) ;
#107816 = CARTESIAN_POINT ( 'NONE',  ( 20.63350300269999948, 1453.978644282629830, 223.8963513020979974 ) ) ;
#107817 = CARTESIAN_POINT ( 'NONE',  ( 10.94382554143900066, 1461.342062594439994, 209.7546787681809803 ) ) ;
#107818 = EDGE_CURVE ( 'NONE', #76431, #19773, #93021, .T. ) ;
#107819 = CARTESIAN_POINT ( 'NONE',  ( 7.663889412338700247, 1510.954290761809943, 203.6521466954270068 ) ) ;
#107820 = CARTESIAN_POINT ( 'NONE',  ( 2.657280408040000097, 1442.422209172990051, 217.7150463564190090 ) ) ;
#107821 = CARTESIAN_POINT ( 'NONE',  ( 16.02248003201332693, 1421.322728439146886, 227.4075243507649020 ) ) ;
#107822 = CARTESIAN_POINT ( 'NONE',  ( -3.657345064219999831, 1446.327858494690190, 165.9157432180979868 ) ) ;
#107823 = CARTESIAN_POINT ( 'NONE',  ( -19.44038716410000234, 1426.366113336930084, 223.7849254028979828 ) ) ;
#107824 = CARTESIAN_POINT ( 'NONE',  ( -24.10732407660000121, 1435.765176705550175, 139.1454052177980145 ) ) ;
#107825 = CARTESIAN_POINT ( 'NONE',  ( -108.0060064069999868, 1388.416414365789933, 298.3043112637590184 ) ) ;
#107826 = CARTESIAN_POINT ( 'NONE',  ( 19.29275756170000022, 1507.866073478030103, 188.6099784302979856 ) ) ;
#107827 = CARTESIAN_POINT ( 'NONE',  ( -2.694739704345536335, 1522.051704408389924, 212.0779207114006510 ) ) ;
#107828 = CARTESIAN_POINT ( 'NONE',  ( -29.71179856916630158, 1462.459958223590093, 269.4677673287446282 ) ) ;
#107829 = ORIENTED_EDGE ( 'NONE', *, *, #61921, .T. ) ;
#107830 = LINE ( 'NONE', #89379, #5199 ) ;
#107831 = CARTESIAN_POINT ( 'NONE',  ( 3.347801439296144377, 1523.456872492435195, 242.0893193391992497 ) ) ;
#107832 = CARTESIAN_POINT ( 'NONE',  ( 31.93052144186282604, 1525.394057003702756, 201.2251853851623196 ) ) ;
#107833 = CARTESIAN_POINT ( 'NONE',  ( -5.787667333660000857, 1484.577386382489976, 199.2118433045889958 ) ) ;
#107834 = CARTESIAN_POINT ( 'NONE',  ( -0.2151303249849999821, 1415.407078916530054, 233.4369296871979884 ) ) ;
#107835 = CARTESIAN_POINT ( 'NONE',  ( -13.49108505849066830, 1443.663885487968173, 187.1285806743424587 ) ) ;
#107836 = CARTESIAN_POINT ( 'NONE',  ( -8.616829302300699212, 1437.329206855350094, 209.9044458843100074 ) ) ;
#107837 = CARTESIAN_POINT ( 'NONE',  ( -3.665627820750973598, 1507.166784779998579, 236.6858190950203493 ) ) ;
#107838 = PLANE ( 'NONE',  #3838 ) ;
#107839 = CARTESIAN_POINT ( 'NONE',  ( -14.23978842837620107, 1415.677402202509938, 204.6746519906900232 ) ) ;
#107840 = CARTESIAN_POINT ( 'NONE',  ( 17.04824238339829634, 1423.676546790900147, 228.9394188427949928 ) ) ;
#107841 = CARTESIAN_POINT ( 'NONE',  ( -12.83622357435112527, 1442.860320894220195, 169.4450327812936052 ) ) ;
#107843 = ORIENTED_EDGE ( 'NONE', *, *, #57628, .F. ) ;
#107842 = CARTESIAN_POINT ( 'NONE',  ( 18.00387273070569805, 1424.690294994519945, 226.0499844219949921 ) ) ;
#107844 = CARTESIAN_POINT ( 'NONE',  ( -103.7379217180000097, 1384.886069803950022, 296.9203887490589864 ) ) ;
#107845 = CARTESIAN_POINT ( 'NONE',  ( 14.97085957818899971, 1514.147575501549909, 223.8949061397489970 ) ) ;
#107846 = EDGE_LOOP ( 'NONE', ( #12766, #5567, #29856, #66563 ) ) ;
#107847 = ORIENTED_EDGE ( 'NONE', *, *, #78321, .F. ) ;
#107848 = CARTESIAN_POINT ( 'NONE',  ( 18.06717587838990013, 1416.826860677879949, 208.8995450462120118 ) ) ;
#107849 = CARTESIAN_POINT ( 'NONE',  ( 12.95381060480000102, 1508.673484890930013, 233.5419616260979865 ) ) ;
#107851 = CARTESIAN_POINT ( 'NONE',  ( -19.57999079410000220, 1459.737765216430034, 238.2202614069979916 ) ) ;
#107850 = CARTESIAN_POINT ( 'NONE',  ( 4.001542931430000394, 1454.513261907689866, 217.6365205154789919 ) ) ;
#107852 = CARTESIAN_POINT ( 'NONE',  ( -19.39408456770000200, 1487.979652943030032, 189.5452868223979976 ) ) ;
#107853 = CARTESIAN_POINT ( 'NONE',  ( -11.88208569280000049, 1433.207756250380044, 150.1653117102979991 ) ) ;
#107854 = DIRECTION ( 'NONE',  ( 0.3255681544571546460, 0.000000000000000000, 0.9455185755993176233 ) ) ;
#107855 = CARTESIAN_POINT ( 'NONE',  ( 9.067032342309868653, 1422.697473864469885, 213.1748852504530021 ) ) ;
#107856 = CARTESIAN_POINT ( 'NONE',  ( 9.355425336389100011, 1464.485869949779953, 212.1516644132140073 ) ) ;
#107857 = CARTESIAN_POINT ( 'NONE',  ( -26.44687317989999897, 1439.558179940190030, 137.2464839519979876 ) ) ;
#107858 = CARTESIAN_POINT ( 'NONE',  ( 0.8972167984987801104, 1515.116734647830071, 213.4499345946999824 ) ) ;
#107859 = CARTESIAN_POINT ( 'NONE',  ( 5.820774579480000099, 1441.874794564960212, 154.7773490369980038 ) ) ;
#107860 = CARTESIAN_POINT ( 'NONE',  ( -4.063907090412950396, 1476.726422537800090, 219.8840548534849972 ) ) ;
#107861 = CARTESIAN_POINT ( 'NONE',  ( -2.179640835936603960, 1362.370409203572308, 208.3718459617061285 ) ) ;
#107862 = CARTESIAN_POINT ( 'NONE',  ( -2.612018202825398649, 1509.136298029517775, 239.0293567375654789 ) ) ;
#107864 = ORIENTED_EDGE ( 'NONE', *, *, #73570, .T. ) ;
#107863 = CARTESIAN_POINT ( 'NONE',  ( 1.500377517123119864E-08, 1408.384000088409948, 262.1948535354470096 ) ) ;
#107865 = ORIENTED_EDGE ( 'NONE', *, *, #45307, .F. ) ;
#107866 = CARTESIAN_POINT ( 'NONE',  ( -11.86404314291600137, 1432.192232348270181, 149.9804585586999792 ) ) ;
#107867 = B_SPLINE_CURVE_WITH_KNOTS ( 'NONE', 3,
 ( #35018, #52402, #43436, #50194, #110627, #85976, #17637, #86525, #59689, #33352, #8704, #75924, #42321, #1427, #77587, #27181, #67547, #26045, #17078, #61364, #69197, #42882, #51273, #60808, #78123, #101649, #93801, #77039, #16532 ),
 .UNSPECIFIED., .F., .F.,
 ( 4, 2, 2, 1, 1, 2, 2, 2, 2, 2, 2, 2, 1, 2, 2, 4 ),
 ( 0.000000000000000000, 0.1250000000036102510, 0.1875000000054153904, 0.2187500000062866101, 0.2343750000067222339, 0.2421875000068499373, 0.2500000000069776407, 0.3750000000063050121, 0.4375000000059334204, 0.5000000000055617733, 0.6250000000043715032, 0.6875000000035829117, 0.7187500000030055958, 0.7343750000027402525, 0.7500000000024747981, 1.000000000000000000 ),
 .UNSPECIFIED. ) ;
#107868 = CARTESIAN_POINT ( 'NONE',  ( -13.63402676890000009, 1504.645044512890081, 227.7399864453990119 ) ) ;
#107869 = CARTESIAN_POINT ( 'NONE',  ( -3.165485081419999958, 1473.508234980229872, 270.3910588708980640 ) ) ;
#107870 = CARTESIAN_POINT ( 'NONE',  ( 12.72577279029999886, 1508.073447237130040, 233.4251884259979875 ) ) ;
#107871 = CARTESIAN_POINT ( 'NONE',  ( -125.2268008667000458, 1376.302340817389677, 316.0486468239593592 ) ) ;
#107872 = CARTESIAN_POINT ( 'NONE',  ( 7.932410439648875489, 1391.426148861440197, 209.1218459572589836 ) ) ;
#107873 = CARTESIAN_POINT ( 'NONE',  ( 4.327045307009350417, 1515.156577661779920, 209.3136710241140008 ) ) ;
#107874 = CARTESIAN_POINT ( 'NONE',  ( -8.379472588110001396, 1384.543820896499938, 199.7942522451990044 ) ) ;
#107875 = CARTESIAN_POINT ( 'NONE',  ( 18.07842109055869884, 1431.201698177569824, 206.4737439103550116 ) ) ;
#107876 = CARTESIAN_POINT ( 'NONE',  ( -3.840975779399999901, 1458.116743529589939, 218.6763403738689817 ) ) ;
#107877 = CARTESIAN_POINT ( 'NONE',  ( 11.84442987637726930, 1365.578918197742496, 208.3718459617010978 ) ) ;
#107878 = CARTESIAN_POINT ( 'NONE',  ( -37.64115395575449696, 1420.091924967339992, 267.8855929252160308 ) ) ;
#107879 = ORIENTED_EDGE ( 'NONE', *, *, #82871, .F. ) ;
#107880 = CYLINDRICAL_SURFACE ( 'NONE', #82391, 30.10786454236638576 ) ;
#107881 = ORIENTED_EDGE ( 'NONE', *, *, #70506, .F. ) ;
#107882 = ORIENTED_EDGE ( 'NONE', *, *, #24836, .F. ) ;
#107883 = CARTESIAN_POINT ( 'NONE',  ( -1.700706814495000163, 1516.923170579120097, 211.4225755968969906 ) ) ;
#107884 = CARTESIAN_POINT ( 'NONE',  ( 34.00753574056176376, 1444.324653571831277, 154.9193549732159454 ) ) ;
#107885 = DIRECTION ( 'NONE',  ( 0.03489949670251145386, -0.9993908270190954291, 0.000000000000000000 ) ) ;
#107887 = CARTESIAN_POINT ( 'NONE',  ( -4.221362096953909848, 1441.596168439879875, 170.5366494805969921 ) ) ;
#107886 = CARTESIAN_POINT ( 'NONE',  ( 1.715361092244999996, 1516.743010792419909, 212.5670474586069929 ) ) ;
#107888 = CARTESIAN_POINT ( 'NONE',  ( -17.05703394869999912, 1440.440300860529987, 190.5363989150980046 ) ) ;
#107889 = B_SPLINE_CURVE_WITH_KNOTS ( 'NONE', 3,
 ( #279, #34950, #19231, #18140, #85337, #8634, #69134, #33843, #52336, #86459, #103820, #76970, #95422, #27119, #61304, #18685, #53440, #68034, #102143, #25424, #79739, #11967, #38259, #3047, #80281 ),
 .UNSPECIFIED., .F., .F.,
 ( 4, 3, 3, 3, 3, 3, 3, 3, 4 ),
 ( 80.62324409590000585, 83.04996275482889700, 85.46931539243300335, 87.87555010193320015, 89.44943093207820084, 91.83314302553000630, 94.22747645563690355, 96.63741502969980957, 98.11410426366440163 ),
 .UNSPECIFIED. ) ;
#107890 = CARTESIAN_POINT ( 'NONE',  ( -2.349669919091817327, 1449.655171934847658, 182.9923140666560641 ) ) ;
#107891 = VERTEX_POINT ( 'NONE', #65713 ) ;
#107892 = CARTESIAN_POINT ( 'NONE',  ( -26.35025291359999855, 1436.552346511289898, 136.8052071317979994 ) ) ;
#107893 = CARTESIAN_POINT ( 'NONE',  ( 0.7386049046750020608, 1517.122674412569950, 202.5597518628069906 ) ) ;
#107894 = EDGE_CURVE ( 'NONE', #81601, #52122, #35895, .T. ) ;
#107895 = CARTESIAN_POINT ( 'NONE',  ( -40.23884947949994029, 1448.346529241730877, 135.0415268541977412 ) ) ;
#107896 = CARTESIAN_POINT ( 'NONE',  ( -14.95647597185759992, 1384.522095472869751, 200.6334766323439851 ) ) ;
#107897 = CARTESIAN_POINT ( 'NONE',  ( 0.06979919672880000037, 1408.910622945630166, 194.1218459596979926 ) ) ;
#107898 = CARTESIAN_POINT ( 'NONE',  ( -16.66701395081548398, 1523.530870145312292, 180.4846106723514083 ) ) ;
#107899 = CARTESIAN_POINT ( 'NONE',  ( -1.113853250640000070, 1395.951956999929962, 198.1149994302979849 ) ) ;
#107901 = EDGE_LOOP ( 'NONE', ( #15916, #13901 ) ) ;
#107900 = CARTESIAN_POINT ( 'NONE',  ( -9.978586514379999883, 1364.539968386210148, 207.6218459616989946 ) ) ;
#107902 = ORIENTED_EDGE ( 'NONE', *, *, #90545, .F. ) ;
#107903 = CARTESIAN_POINT ( 'NONE',  ( 0.3125186096800000035, 1450.902146997000045, 181.9094756310980188 ) ) ;
#107904 = AXIS2_PLACEMENT_3D ( 'NONE', #58550, #69162, #24899 ) ;
#107905 = CARTESIAN_POINT ( 'NONE',  ( 29.84438983998366623, 1466.863671349131209, 269.3606549350047885 ) ) ;
#107906 = FACE_OUTER_BOUND ( 'NONE', #45326, .T. ) ;
#107907 = DIRECTION ( 'NONE',  ( -0.000000000000000000, -1.000000000000000000, -0.000000000000000000 ) ) ;
#107908 = FACE_OUTER_BOUND ( 'NONE', #100545, .T. ) ;
#107909 = CARTESIAN_POINT ( 'NONE',  ( -6.548200625775000283, 1516.632821972880038, 210.2524534341069966 ) ) ;
#107910 = CARTESIAN_POINT ( 'NONE',  ( -18.26023438560000045, 1443.256148476890075, 213.5656046648789754 ) ) ;
#107911 = CARTESIAN_POINT ( 'NONE',  ( 3.750000000000000000, 1524.051704408389924, 209.1218459616989946 ) ) ;
#107912 = ADVANCED_FACE ( 'NONE', ( #5806 ), #98191, .T. ) ;
#107913 = CARTESIAN_POINT ( 'NONE',  ( 4.093827366729640538, 1442.069873536569730, 216.9756443559270167 ) ) ;
#107914 = CARTESIAN_POINT ( 'NONE',  ( 8.170896223665000235, 1511.354819475749991, 204.2943405042869927 ) ) ;
#107915 =( BOUNDED_SURFACE ( )  B_SPLINE_SURFACE ( 3, 2, ( 
 ( #87751, #18847, #53043 ),
 ( #35668, #69855, #110721 ),
 ( #51931, #77138, #53608 ),
 ( #35115, #77677, #27828 ),
 ( #17172, #11033, #45200 ),
 ( #68205, #19404, #93905 ) ),
 .UNSPECIFIED., .F., .F., .F. ) 
 B_SPLINE_SURFACE_WITH_KNOTS ( ( 4, 2, 4 ),
 ( 3, 3 ),
 ( 3.469446951953614189E-18, 0.001312027981647208297, 0.002624055963294413124 ),
 ( 0.000000000000000000, 1.000000000000000000 ),
 .UNSPECIFIED. ) 
 GEOMETRIC_REPRESENTATION_ITEM ( )  RATIONAL_B_SPLINE_SURFACE ( (
 ( 1.000000000000000000, 0.9376006582765969988, 1.000000000000000000),
 ( 1.000000000000000000, 0.9569320108030995309, 1.000000000000000000),
 ( 1.000000000000000000, 0.9725743441607752615, 1.000000000000000000),
 ( 1.000000000000000000, 0.9942095667146912952, 1.000000000000000000),
 ( 1.000000000000000000, 1.000043666449861757, 1.000000000000000000),
 ( 1.000000000000000000, 1.000000000000000000, 1.000000000000000000) ) ) 
 REPRESENTATION_ITEM ( '' )  SURFACE ( )  );
#107916 = CARTESIAN_POINT ( 'NONE',  ( -3.269184946495000244, 1516.940296199220029, 206.8376465686969823 ) ) ;
#107917 = ORIENTED_EDGE ( 'NONE', *, *, #80504, .T. ) ;
#107918 = CARTESIAN_POINT ( 'NONE',  ( -7.973546373915826990, 1425.245985973295547, 205.1887633420602413 ) ) ;
#107919 = B_SPLINE_CURVE_WITH_KNOTS ( 'NONE', 5,
 ( #100890, #77243, #1094, #58374, #35780, #69407 ),
 .UNSPECIFIED., .F., .F.,
 ( 6, 6 ),
 ( -88.78633455690000176, -19.55448171529999968 ),
 .UNSPECIFIED. ) ;
#107920 = CARTESIAN_POINT ( 'NONE',  ( -10.03141724199999985, 1472.765117119090064, 207.2972502656089944 ) ) ;
#107921 = CARTESIAN_POINT ( 'NONE',  ( -23.22468639008607383, 1449.418569010514830, 216.9711829936322829 ) ) ;
#107922 = ORIENTED_EDGE ( 'NONE', *, *, #80171, .F. ) ;
#107924 = B_SPLINE_CURVE_WITH_KNOTS ( 'NONE', 3,
 ( #56469, #21721, #107403, #81639, #30699, #98992, #90601, #5503, #97894, #107956, #54285, #45875, #80564, #29593, #80010, #37457, #71659, #54828, #106309, #88951, #63777, #7700, #101190, #74387, #58126, #84414, #83309, #65990, #7159, #101747, #24487, #100112, #108512, #33436, #48630, #91709, #41316, #74933, #50816, #6053, #23394, #110715, #49726 ),
 .UNSPECIFIED., .F., .F.,
 ( 4, 2, 2, 2, 2, 2, 2, 2, 2, 1, 1, 2, 2, 2, 2, 2, 2, 1, 1, 1, 2, 2, 2, 4 ),
 ( 0.000000000000000000, 0.007812500000093510269, 0.01562500000018702054, 0.02343750000028053254, 0.03125000000037404108, 0.06250000000091890384, 0.1250000000021675994, 0.1875000000034163228, 0.2187500000040124293, 0.2343750000042608417, 0.2421875000043403892, 0.2460937500043932358, 0.2500000000044461101, 0.3125000000050295879, 0.3750000000056131211, 0.4375000000061965988, 0.4687500000065056849, 0.4843750000068736128, 0.4921875000067835737, 0.4960937500067363892, 0.4980468750067104100, 0.5000000000066844308, 0.7500000000033421044, 1.000000000000000000 ),
 .UNSPECIFIED. ) ;
#107923 = CYLINDRICAL_SURFACE ( 'NONE', #92790, 1.999999999999997335 ) ;
#107926 = ADVANCED_FACE ( 'NONE', ( #64072 ), #90245, .F. ) ;
#107925 = LINE ( 'NONE', #41281, #44863 ) ;
#107927 = CARTESIAN_POINT ( 'NONE',  ( 13.79047275900000002, 1415.263254653229978, 197.3591164767980217 ) ) ;
#107928 = CARTESIAN_POINT ( 'NONE',  ( -9.123736379228210680, 1384.508619151900120, 199.9712811155520171 ) ) ;
#107929 = CARTESIAN_POINT ( 'NONE',  ( 20.27230674349999973, 1410.542376202429978, 198.0398506171979989 ) ) ;
#107930 = CARTESIAN_POINT ( 'NONE',  ( 7.649034400464999273, 1514.243099272629934, 214.7715657207469917 ) ) ;
#107931 = DIRECTION ( 'NONE',  ( -1.755985294532469921E-16, 1.000000000000000000, -1.338183447452831989E-16 ) ) ;
#107932 = B_SPLINE_CURVE_WITH_KNOTS ( 'NONE', 3,
 ( #75146, #14662, #24689, #92461, #33114, #15732, #41533, #101961, #109293, #25247, #84071, #31463, #67849, #93018, #83512, #100327, #66754, #32578, #23612, #57799, #7911, #108728, #75691, #32018, #67301, #59450, #42082, #16834 ),
 .UNSPECIFIED., .F., .F.,
 ( 4, 3, 3, 3, 3, 3, 3, 3, 3, 4 ),
 ( -7.332849270026669863, -7.070672308253410421, -6.683016686340660151, -6.206605020891959867, -5.597668811241430120, -5.172869050969330473, -4.989338611940850043, -4.363064878034809801, -3.699273191951379935, -3.012888606410000669 ),
 .UNSPECIFIED. ) ;
#107933 = CARTESIAN_POINT ( 'NONE',  ( -0.3821804589910179906, 1506.433683733660018, 187.1424611576989889 ) ) ;
#107934 = CARTESIAN_POINT ( 'NONE',  ( 24.33873747859275483, 1445.475447480255298, 214.1757831162466630 ) ) ;
#107935 = LINE ( 'NONE', #88931, #22657 ) ;
#107936 = LINE ( 'NONE', #65410, #12065 ) ;
#107937 = CARTESIAN_POINT ( 'NONE',  ( 0.7533001353030019942, 1516.714320817460020, 216.4479181143769893 ) ) ;
#107938 = VERTEX_POINT ( 'NONE', #33733 ) ;
#107939 = CARTESIAN_POINT ( 'NONE',  ( -17.43675232709999889, 1417.688629781069949, 206.2161169699189713 ) ) ;
#107940 = CARTESIAN_POINT ( 'NONE',  ( -3.565775599929999817, 1474.072336424830155, 270.1349117941979898 ) ) ;
#107941 = CARTESIAN_POINT ( 'NONE',  ( -2.500000000000000000, 1448.577607907360061, 183.6861132275980140 ) ) ;
#107942 = CARTESIAN_POINT ( 'NONE',  ( -11.00428676220000135, 1425.778354413130046, 91.15517427569778874 ) ) ;
#107943 = CARTESIAN_POINT ( 'NONE',  ( -1.062931043700000133, 1475.464638824089889, 220.1331094441989933 ) ) ;
#107944 = EDGE_CURVE ( 'NONE', #110657, #109170, #102035, .T. ) ;
#107945 = CARTESIAN_POINT ( 'NONE',  ( 11.60004869885203682, 1426.459365826449584, 139.0214960885385551 ) ) ;
#107946 = CARTESIAN_POINT ( 'NONE',  ( -38.64637139473789773, 1443.913060387190171, 137.1864063576500143 ) ) ;
#107947 = CARTESIAN_POINT ( 'NONE',  ( -2.136599176237389930, 1477.791721619980081, 183.3770592319010007 ) ) ;
#107948 = CARTESIAN_POINT ( 'NONE',  ( -2.283851398302360280, 1454.773268660870144, 198.8765668124689796 ) ) ;
#107949 = DIRECTION ( 'NONE',  ( 0.9455185755993178454, 0.000000000000000000, -0.3255681544571539243 ) ) ;
#107950 = CARTESIAN_POINT ( 'NONE',  ( 32.66611766053999588, 1440.913060383240008, 245.7919428914240143 ) ) ;
#107951 = CARTESIAN_POINT ( 'NONE',  ( -10.12171546665249977, 1470.644541919200037, 212.0628956816030097 ) ) ;
#107952 = CARTESIAN_POINT ( 'NONE',  ( -121.3980906523484009, 1384.913060387289988, 304.3966198592502792 ) ) ;
#107953 = ORIENTED_EDGE ( 'NONE', *, *, #46375, .T. ) ;
#107954 = ORIENTED_EDGE ( 'NONE', *, *, #9321, .F. ) ;
#107955 = CARTESIAN_POINT ( 'NONE',  ( 12.45478753333600430, 1442.762691980110276, 150.7713593675359505 ) ) ;
#107956 = CARTESIAN_POINT ( 'NONE',  ( -19.13255955744318726, 1485.540540826345932, 189.6605840472149964 ) ) ;
#107957 = CARTESIAN_POINT ( 'NONE',  ( -27.85007288970000161, 1509.193792693030218, 210.7874566006480279 ) ) ;
#107958 = CARTESIAN_POINT ( 'NONE',  ( 7.472831402659999789, 1423.077331640449984, 195.6326729942990141 ) ) ;
#107959 = DIRECTION ( 'NONE',  ( 0.1867471702549220458, -2.391457216852619248E-16, -0.9824080081115885710 ) ) ;
#107960 = CARTESIAN_POINT ( 'NONE',  ( -17.45336505325400012, 1413.337826481620141, 225.8632813675029922 ) ) ;
#107961 = CARTESIAN_POINT ( 'NONE',  ( -0.9649234502016059700, 1508.551704408389924, 220.0742041972960124 ) ) ;
#107962 = CARTESIAN_POINT ( 'NONE',  ( -38.38927993948440331, 1383.830596176209838, 239.0580260840490041 ) ) ;
#107963 = CARTESIAN_POINT ( 'NONE',  ( -5.106974084935000491, 1511.397837225850026, 200.5635451951269772 ) ) ;
#107964 = DIRECTION ( 'NONE',  ( -0.000000000000000000, -0.000000000000000000, 1.000000000000000000 ) ) ;
#107965 = FACE_OUTER_BOUND ( 'NONE', #14498, .T. ) ;
#107966 = CARTESIAN_POINT ( 'NONE',  ( 2.441369149599999844, 1464.626822193330099, 236.1885516863980001 ) ) ;
#107968 = VERTEX_POINT ( 'NONE', #8533 ) ;
#107967 = CARTESIAN_POINT ( 'NONE',  ( -32.38845791999490586, 1523.382868172864164, 216.1254071228449902 ) ) ;
#107969 = CARTESIAN_POINT ( 'NONE',  ( -1.031182265530000253, 1450.900347381030087, 182.2739190327980054 ) ) ;
#107970 = CARTESIAN_POINT ( 'NONE',  ( -8.870422689270000660, 1380.884123086199907, 216.4346137712589950 ) ) ;
#107971 = CARTESIAN_POINT ( 'NONE',  ( 3.780333224634049749, 1508.551704408389924, 204.4954358679670179 ) ) ;
#107973 = ORIENTED_EDGE ( 'NONE', *, *, #72032, .T. ) ;
#107972 = DIRECTION ( 'NONE',  ( -0.8672669759446666182, 0.000000000000000000, -0.4978433412588672557 ) ) ;
#107974 = CARTESIAN_POINT ( 'NONE',  ( -19.86622909784430036, 1443.388413634180097, 213.1207225405120198 ) ) ;
#107975 = ORIENTED_EDGE ( 'NONE', *, *, #100730, .T. ) ;
#107976 = CARTESIAN_POINT ( 'NONE',  ( -7.873989245522249547, 1386.913809585709942, 218.7666999748780086 ) ) ;
#107977 = CARTESIAN_POINT ( 'NONE',  ( 33.91369278643569629, 1437.010534640189690, 136.5611839302279691 ) ) ;
#107978 = AXIS2_PLACEMENT_3D ( 'NONE', #38209, #12461, #29810 ) ;
#107979 = CARTESIAN_POINT ( 'NONE',  ( 1.925297169133120212, 1517.051704408389924, 230.6853930764029883 ) ) ;
#107980 = CARTESIAN_POINT ( 'NONE',  ( -106.1530010540000006, 1379.143473661730013, 300.9588320359590057 ) ) ;
#107981 = DIRECTION ( 'NONE',  ( -1.000000000000000000, 0.000000000000000000, 0.000000000000000000 ) ) ;
#107982 = CARTESIAN_POINT ( 'NONE',  ( -10.16450165796499938, 1472.456210521550020, 207.1947926051400088 ) ) ;
#107983 = CARTESIAN_POINT ( 'NONE',  ( 10.82176781693950041, 1409.290964846770066, 198.8079905577820057 ) ) ;
#107984 = CARTESIAN_POINT ( 'NONE',  ( 18.52259990968499892, 1425.592936175037948, 225.5468824535050203 ) ) ;
#107985 = DIRECTION ( 'NONE',  ( -0.6736849260863841948, 0.000000000000000000, 0.7390186874254148774 ) ) ;
#107986 = CARTESIAN_POINT ( 'NONE',  ( -18.93959894380000009, 1463.213399808430040, 190.7720972619979705 ) ) ;
#107987 = CARTESIAN_POINT ( 'NONE',  ( -67.87070494639999652, 1379.748617063760094, 278.3152404517590526 ) ) ;
#107988 = CIRCLE ( 'NONE', #70468, 24.69926344187880929 ) ;
#107989 = CARTESIAN_POINT ( 'NONE',  ( -2.321573235545089986, 1449.941122205050078, 183.5337604117939918 ) ) ;
#107990 = ORIENTED_EDGE ( 'NONE', *, *, #88303, .T. ) ;
#107991 = CARTESIAN_POINT ( 'NONE',  ( -7.320051284198429542, 1508.610505975320166, 215.2032464672789729 ) ) ;
#107992 = CARTESIAN_POINT ( 'NONE',  ( 18.98967647182920260, 1456.684695305999867, 227.0095329493280190 ) ) ;
#107993 = FACE_OUTER_BOUND ( 'NONE', #1171, .T. ) ;
#107994 = CARTESIAN_POINT ( 'NONE',  ( 6.763640255447179445E-10, 1465.118916387369836, 238.1343321182859825 ) ) ;
#107995 = CARTESIAN_POINT ( 'NONE',  ( -20.42135399285539776, 1502.078354143829984, 190.5572915927370161 ) ) ;
#107996 = CARTESIAN_POINT ( 'NONE',  ( -32.02808312589930040, 1511.187213306747708, 198.2787714533499752 ) ) ;
#107997 = CARTESIAN_POINT ( 'NONE',  ( -108.5006393170000081, 1386.602053732790182, 310.8681882702589974 ) ) ;
#107998 = CARTESIAN_POINT ( 'NONE',  ( -8.631375286013071246, 1511.600151312669823, 215.0326715986050203 ) ) ;
#107999 = CARTESIAN_POINT ( 'NONE',  ( -9.178315062057500029, 1363.109187794154195, 210.6218459616991936 ) ) ;
#108000 = CARTESIAN_POINT ( 'NONE',  ( -46.16084778820400203, 1440.247791815949995, 266.9716791494209929 ) ) ;
#108001 = CARTESIAN_POINT ( 'NONE',  ( -19.40520978109999817, 1426.254488764730240, 225.7391413128980275 ) ) ;
#108002 = CARTESIAN_POINT ( 'NONE',  ( 3.059311260596259352, 1525.343710797494396, 176.8478414008731932 ) ) ;
#108003 = CARTESIAN_POINT ( 'NONE',  ( 4.028611221114998919, 1516.744381837270112, 207.9874879615069858 ) ) ;
#108004 = CARTESIAN_POINT ( 'NONE',  ( -9.072363224181140495, 1449.404768024669920, 210.5087561342340052 ) ) ;
#108005 = CARTESIAN_POINT ( 'NONE',  ( 1.289002268286620012, 1407.277490461829984, 222.1229423106349827 ) ) ;
#108006 = CARTESIAN_POINT ( 'NONE',  ( 29.71163624023410321, 1526.333389947941441, 201.1407003069334678 ) ) ;
#108007 = CIRCLE ( 'NONE', #68721, 0.9999999999999880096 ) ;
#108008 = DIRECTION ( 'NONE',  ( 0.9455185755993178454, 0.000000000000000000, -0.3255681544571537578 ) ) ;
#108009 = CARTESIAN_POINT ( 'NONE',  ( 7.041307337603809557, 1424.896087700059979, 213.1365174684090107 ) ) ;
#108010 = ORIENTED_EDGE ( 'NONE', *, *, #95558, .F. ) ;
#108011 = CARTESIAN_POINT ( 'NONE',  ( 34.48978217459999485, 1438.727114832149937, 250.0021841848979989 ) ) ;
#108012 = CARTESIAN_POINT ( 'NONE',  ( -26.42702185619999966, 1508.126183420129792, 201.6901284736979960 ) ) ;
#108014 = CARTESIAN_POINT ( 'NONE',  ( -21.84020450222076448, 1523.382868172864164, 183.2638850454220858 ) ) ;
#108013 = CARTESIAN_POINT ( 'NONE',  ( -0.4938787171589999470, 1469.871322339429980, 182.4160331598980065 ) ) ;
#108015 = CARTESIAN_POINT ( 'NONE',  ( -114.5985638465105154, 1347.163060387289988, 306.4158023619849018 ) ) ;
#108016 = CARTESIAN_POINT ( 'NONE',  ( -14.01630619230000008, 1418.416544456529891, 240.3753821333979772 ) ) ;
#108017 = CARTESIAN_POINT ( 'NONE',  ( -4.636716969933436516, 1378.031735257917717, 214.3255111405700575 ) ) ;
#108018 = CARTESIAN_POINT ( 'NONE',  ( -12.12288233474179933, 1452.489720007740061, 149.6117171413690130 ) ) ;
#108019 = CARTESIAN_POINT ( 'NONE',  ( 27.02655771539999918, 1451.969198393830084, 135.3521981671979972 ) ) ;
#108020 = ORIENTED_EDGE ( 'NONE', *, *, #67878, .F. ) ;
#108021 = CARTESIAN_POINT ( 'NONE',  ( -107.6858065237089903, 1378.913060387379801, 300.3274025718760072 ) ) ;
#108022 = CARTESIAN_POINT ( 'NONE',  ( 3.152372269302069840E-05, 1408.236641047440116, 270.3925689135490416 ) ) ;
#108023 = CARTESIAN_POINT ( 'NONE',  ( 16.14572133049080094, 1423.056865153649824, 229.1739396973900114 ) ) ;
#108024 = CARTESIAN_POINT ( 'NONE',  ( 9.760879523209998965, 1463.475536510490201, 209.9230695397520208 ) ) ;
#108025 = ORIENTED_EDGE ( 'NONE', *, *, #92498, .F. ) ;
#108026 = VERTEX_POINT ( 'NONE', #25321 ) ;
#108027 = CARTESIAN_POINT ( 'NONE',  ( -2.185878866602459838E-15, 1384.627966395730027, 199.6314228471690058 ) ) ;
#108028 = CARTESIAN_POINT ( 'NONE',  ( -24.10619303449700013, 1410.858805650359955, 208.8787671924330027 ) ) ;
#108029 = ORIENTED_EDGE ( 'NONE', *, *, #18277, .F. ) ;
#108030 = CARTESIAN_POINT ( 'NONE',  ( 3.487586701839819892, 1508.731366863229823, 204.5668911354170234 ) ) ;
#108031 = DIRECTION ( 'NONE',  ( 0.000000000000000000, 0.000000000000000000, 1.000000000000000000 ) ) ;
#108032 = CARTESIAN_POINT ( 'NONE',  ( -7.500890280090000140, 1498.345403818429986, 235.0614749778980013 ) ) ;
#108033 = CARTESIAN_POINT ( 'NONE',  ( 16.75454338845089453, 1526.382868172571079, 234.5462402641960864 ) ) ;
#108034 = ORIENTED_EDGE ( 'NONE', *, *, #27629, .F. ) ;
#108035 = EDGE_CURVE ( 'NONE', #39872, #3178, #36463, .T. ) ;
#108036 = CARTESIAN_POINT ( 'NONE',  ( 43.01404880660360419, 1452.566160834499897, 269.0485511200449764 ) ) ;
#108037 = CARTESIAN_POINT ( 'NONE',  ( -11.87146819872990022, 1414.971390223319986, 220.8694174431610122 ) ) ;
#108038 = CARTESIAN_POINT ( 'NONE',  ( 0.03302424225530000562, 1420.442649414729885, 183.2904121144979683 ) ) ;
#108039 = CARTESIAN_POINT ( 'NONE',  ( 0.7365611785030020675, 1517.066898074209803, 204.4979538714769944 ) ) ;
#108040 = ORIENTED_EDGE ( 'NONE', *, *, #44047, .F. ) ;
#108041 = CARTESIAN_POINT ( 'NONE',  ( 5.952292128818620576, 1483.732806304819860, 219.3495610126499855 ) ) ;
#108042 = CARTESIAN_POINT ( 'NONE',  ( 14.79494652412309819, 1512.129944624190102, 196.8603049394490085 ) ) ;
#108043 = CARTESIAN_POINT ( 'NONE',  ( 13.45635499389495848, 1443.545252278519229, 187.9751403306488555 ) ) ;
#108044 = EDGE_LOOP ( 'NONE', ( #85386, #72669, #78946, #84500, #100716, #57476 ) ) ;
#108045 = EDGE_LOOP ( 'NONE', ( #90011, #105061, #95359 ) ) ;
#108046 = CARTESIAN_POINT ( 'NONE',  ( -11.00988902727860008, 1481.333122227119929, 209.3333858298779830 ) ) ;
#108048 = ADVANCED_FACE ( 'NONE', ( #93630 ), #85652, .T. ) ;
#108047 = CARTESIAN_POINT ( 'NONE',  ( -2.654144332375780291, 1508.551704412109984, 220.2468185985560183 ) ) ;
#108049 = CARTESIAN_POINT ( 'NONE',  ( -12.92498210531170066, 1512.351864386150055, 193.9290602599010072 ) ) ;
#108050 = CARTESIAN_POINT ( 'NONE',  ( 6.700690081702690648, 1452.679067133560011, 151.6942415867249849 ) ) ;
#108051 = CARTESIAN_POINT ( 'NONE',  ( 12.65754557789999879, 1420.238440408800216, 200.3470417333290072 ) ) ;
#108052 = CARTESIAN_POINT ( 'NONE',  ( 18.79226589730000185, 1456.307606824690083, 213.7887498653890077 ) ) ;
#108053 = CARTESIAN_POINT ( 'NONE',  ( -108.8100569807280351, 1381.628441269055884, 297.7725132315368910 ) ) ;
#108054 = CARTESIAN_POINT ( 'NONE',  ( 10.45814682399799977, 1479.299028883320034, 205.9955659561700259 ) ) ;
#108055 = AXIS2_PLACEMENT_3D ( 'NONE', #16438, #76380, #93705 ) ;
#108056 = FACE_OUTER_BOUND ( 'NONE', #38029, .T. ) ;
#108058 = CARTESIAN_POINT ( 'NONE',  ( -106.9652640938700046, 1391.913060387289988, 306.6581628094390339 ) ) ;
#108057 = CARTESIAN_POINT ( 'NONE',  ( 29.86283313086964597, 1525.137881624885267, 196.1139775505488956 ) ) ;
#108059 = CARTESIAN_POINT ( 'NONE',  ( 10.66765284868029973, 1424.188739277350123, 206.6454873575900137 ) ) ;
#108060 = CARTESIAN_POINT ( 'NONE',  ( -9.827361973644409332, 1439.976119166509989, 207.2092696800089868 ) ) ;
#108061 = CARTESIAN_POINT ( 'NONE',  ( 9.660544699540000835, 1432.353341358199941, 148.7316627034979888 ) ) ;
#108062 = ORIENTED_EDGE ( 'NONE', *, *, #35497, .T. ) ;
#108063 = CARTESIAN_POINT ( 'NONE',  ( 11.69744348346759999, 1415.090956648730071, 222.2791104206980037 ) ) ;
#108064 = AXIS2_PLACEMENT_3D ( 'NONE', #31561, #24790, #99857 ) ;
#108065 = CARTESIAN_POINT ( 'NONE',  ( 0.000000000000000000, 1395.913060387330006, 201.1218459616980283 ) ) ;
#108066 = CARTESIAN_POINT ( 'NONE',  ( -94.96697414727451303, 1384.958059057069704, 310.0402463594970186 ) ) ;
#108067 = B_SPLINE_SURFACE_WITH_KNOTS ( 'NONE', 5, 5, ( 
 ( #80326, #89266, #12562, #97123, #12012, #37769 ),
 ( #62452, #64090, #46192, #19848, #10917, #45092 ),
 ( #88179, #28259, #71962, #98212, #55145, #106072 ),
 ( #70859, #20392, #70304, #87629, #54595, #79232 ),
 ( #54053, #80873, #29897, #11471, #29352, #13085 ),
 ( #46742, #89814, #96013, #63552, #4172, #38302 ) ),
 .UNSPECIFIED., .F., .F., .F.,
 ( 6, 6 ),
 ( 6, 6 ),
 ( 8.898447406460000764, 11.87289910710000029 ),
 ( 0.000000000000000000, 1.449276807229999964 ),
 .UNSPECIFIED. ) ;
#108068 = CARTESIAN_POINT ( 'NONE',  ( -8.151272894939999958, 1385.300637405240195, 199.6428762611590173 ) ) ;
#108069 = CARTESIAN_POINT ( 'NONE',  ( 10.62807384989510062, 1422.391294950000201, 210.1053146505880136 ) ) ;
#108071 = ORIENTED_EDGE ( 'NONE', *, *, #93387, .F. ) ;
#108070 = CARTESIAN_POINT ( 'NONE',  ( 10.98461821322850085, 1423.291179694809898, 203.2749711373830337 ) ) ;
#108072 = CARTESIAN_POINT ( 'NONE',  ( 3.975098305720000447, 1430.458171852989835, 217.7504258046890016 ) ) ;
#108073 = FACE_OUTER_BOUND ( 'NONE', #84026, .T. ) ;
#108074 = CARTESIAN_POINT ( 'NONE',  ( -14.20177183849999913, 1416.825532263429977, 221.7377879684979973 ) ) ;
#108075 = CARTESIAN_POINT ( 'NONE',  ( 11.78366509199999967, 1433.667675045369833, 150.8308889936979824 ) ) ;
#108076 = CARTESIAN_POINT ( 'NONE',  ( 8.881784197000000993E-16, 1472.413060387330006, 271.1218459616979999 ) ) ;
#108077 = B_SPLINE_SURFACE_WITH_KNOTS ( 'NONE', 5, 5, ( 
 ( #33969, #42371, #34524, #6147, #68165, #59743 ),
 ( #93864, #42939, #68705, #60866, #102809, #60294 ),
 ( #94412, #103937, #17689, #77638, #35076, #52454 ),
 ( #27235, #86583, #82857, #1492, #61415, #95538 ),
 ( #18811, #88251, #53006, #11544, #29978, #28897 ),
 ( #10430, #20463, #105050, #64170, #28339, #72035 ),
 ( #63091, #96087, #45163, #27783, #46277, #79303 ),
 ( #104490, #80404, #45719, #19363, #3717, #106150 ),
 ( #89346, #88800, #12082, #87140, #97189, #62534 ) ),
 .UNSPECIFIED., .F., .F., .F.,
 ( 6, 3, 6 ),
 ( 6, 6 ),
 ( 19.61749528909999896, 20.80534586139999931, 22.34240631349999973 ),
 ( 0.000000000000000000, 2.000000000000000000 ),
 .UNSPECIFIED. ) ;
#108078 = CARTESIAN_POINT ( 'NONE',  ( 4.500000000000000000, 1508.551704408389924, 209.1218459616989946 ) ) ;
#108079 = CARTESIAN_POINT ( 'NONE',  ( 3.429115760092809939, 1458.481892967550039, 200.0825522186730154 ) ) ;
#108080 = DIRECTION ( 'NONE',  ( 0.000000000000000000, 0.000000000000000000, -1.000000000000000000 ) ) ;
#108081 = CARTESIAN_POINT ( 'NONE',  ( 11.02428137105887807, 1512.359593911811089, 224.9978793913905974 ) ) ;
#108082 = CARTESIAN_POINT ( 'NONE',  ( -22.41686883764721827, 1524.667648926078527, 236.2663900491539266 ) ) ;
#108083 = DIRECTION ( 'NONE',  ( -0.6736849260863841948, 0.000000000000000000, 0.7390186874254148774 ) ) ;
#108084 = CARTESIAN_POINT ( 'NONE',  ( -18.18090960190000160, 1410.471885800429845, 224.4285890788979998 ) ) ;
#108085 = CARTESIAN_POINT ( 'NONE',  ( 28.62143996450550176, 1526.335487865669620, 220.1875038795444937 ) ) ;
#108086 = CARTESIAN_POINT ( 'NONE',  ( -0.9052398807790000834, 1424.182955095330044, 228.3523643996979899 ) ) ;
#108087 = B_SPLINE_CURVE_WITH_KNOTS ( 'NONE', 5,
 ( #63096, #29433, #9880, #10996, #45168, #104497 ),
 .UNSPECIFIED., .F., .F.,
 ( 6, 6 ),
 ( 4.250950522270000143, 7.082025451739999866 ),
 .UNSPECIFIED. ) ;
#108088 = CARTESIAN_POINT ( 'NONE',  ( -9.868474398105202994, 1442.396259418528871, 184.8303838034649118 ) ) ;
#108089 = CARTESIAN_POINT ( 'NONE',  ( -0.6370436997427022519, 1517.051704408389924, 217.8527312947061603 ) ) ;
#108090 = CARTESIAN_POINT ( 'NONE',  ( 0.008286608639350531713, 1515.284302758789863, 204.7981455896689909 ) ) ;
#108091 = CARTESIAN_POINT ( 'NONE',  ( -0.4151546846821905778, 1522.382868172863937, 173.3106345060153046 ) ) ;
#108092 = DIRECTION ( 'NONE',  ( 0.03618059822125301722, -0.9992709451211057026, -0.01218780329364530825 ) ) ;
#108093 = CARTESIAN_POINT ( 'NONE',  ( -12.13987719790000064, 1415.426210663629945, 221.7061748208979850 ) ) ;
#108094 = AXIS2_PLACEMENT_3D ( 'NONE', #8903, #50929, #85602 ) ;
#108095 = CARTESIAN_POINT ( 'NONE',  ( 0.2130788428118109978, 1455.621404727349955, 183.1409395639289812 ) ) ;
#108096 = CARTESIAN_POINT ( 'NONE',  ( -14.95126388759999969, 1409.435170027230015, 210.7295747781880095 ) ) ;
#108097 = CARTESIAN_POINT ( 'NONE',  ( -14.46594802229999921, 1415.931784856029935, 198.6496374484979981 ) ) ;
#108098 = CARTESIAN_POINT ( 'NONE',  ( -113.4000000000000057, 1384.913060387289988, 304.2218459572590064 ) ) ;
#108099 = CARTESIAN_POINT ( 'NONE',  ( 11.87555827259999930, 1433.006750501450142, 147.9453531988980046 ) ) ;
#108100 = CARTESIAN_POINT ( 'NONE',  ( -36.12226356709360431, 1436.069430019170113, 134.0999999971620014 ) ) ;
#108101 = CARTESIAN_POINT ( 'NONE',  ( 5.510472668829999421, 1441.112718070130086, 184.8635310645979928 ) ) ;
#108102 = VERTEX_POINT ( 'NONE', #44376 ) ;
#108103 = CARTESIAN_POINT ( 'NONE',  ( -16.64711227028525897, 1523.843271061947462, 180.4998300114153267 ) ) ;
#108104 = CARTESIAN_POINT ( 'NONE',  ( 1.916663553690000077, 1477.644687611890049, 198.8912423807989853 ) ) ;
#108105 = CARTESIAN_POINT ( 'NONE',  ( -103.6083266501182436, 1379.909801553448006, 304.7209094884234446 ) ) ;
#108106 = CARTESIAN_POINT ( 'NONE',  ( -11.79358356080000014, 1490.862585118089783, 208.2019470143079900 ) ) ;
#108107 = CARTESIAN_POINT ( 'NONE',  ( -0.7975830076839999228, 1452.841034471829971, 183.3931114573979926 ) ) ;
#108108 = CARTESIAN_POINT ( 'NONE',  ( 14.14834384894100161, 1509.157209502659953, 233.5082961851909999 ) ) ;
#108109 = CARTESIAN_POINT ( 'NONE',  ( -109.1309839890330124, 1384.924126711810004, 311.2646841801559958 ) ) ;
#108110 = CARTESIAN_POINT ( 'NONE',  ( -19.46057851763744395, 1490.124445399882006, 189.4835821391595516 ) ) ;
#108111 = CARTESIAN_POINT ( 'NONE',  ( -12.29824070849999806, 1378.903937160740043, 210.1974271105389960 ) ) ;
#108112 = CARTESIAN_POINT ( 'NONE',  ( 3.920881188560000119, 1439.701871974669984, 184.6839050870979975 ) ) ;
#108113 = CARTESIAN_POINT ( 'NONE',  ( -51.31128716130019995, 1385.023817170500024, 227.3449767567900039 ) ) ;
#108114 = CARTESIAN_POINT ( 'NONE',  ( -12.22815867699069869, 1490.645326540880205, 208.2429163971229968 ) ) ;
#108115 = CARTESIAN_POINT ( 'NONE',  ( -4.987078426973329925, 1508.551704408389924, 206.6339106789369851 ) ) ;
#108116 = ORIENTED_EDGE ( 'NONE', *, *, #36330, .F. ) ;
#108117 = CARTESIAN_POINT ( 'NONE',  ( -27.01382282590000017, 1451.969727051930022, 134.9184453750980026 ) ) ;
#108118 = CARTESIAN_POINT ( 'NONE',  ( -16.10184242527700249, 1409.577400629780186, 225.8122160371329983 ) ) ;
#108120 = EDGE_LOOP ( 'NONE', ( #72086, #25938, #27163, #5578 ) ) ;
#108119 = CARTESIAN_POINT ( 'NONE',  ( 0.4905038111388070332, 1417.380665725640029, 184.7693946335109842 ) ) ;
#108121 = CARTESIAN_POINT ( 'NONE',  ( -109.8262407909999894, 1384.894770813300056, 311.3808759242589872 ) ) ;
#108122 = CARTESIAN_POINT ( 'NONE',  ( 10.89060804628219969, 1471.196313911609877, 210.4292383253470007 ) ) ;
#108123 = ADVANCED_FACE ( 'NONE', ( #95861 ), #103710, .F. ) ;
#108124 = CARTESIAN_POINT ( 'NONE',  ( 17.96908779310200188, 1430.390183715600187, 212.2284757796069812 ) ) ;
#108125 = FILL_AREA_STYLE ('',( #56089 ) ) ;
#108126 = CARTESIAN_POINT ( 'NONE',  ( -0.1826741778924199922, 1419.424196826690149, 184.4619947973449996 ) ) ;
#108127 = CARTESIAN_POINT ( 'NONE',  ( 1.037447696609999914, 1466.935166012330001, 235.3575387440980080 ) ) ;
#108128 = EDGE_CURVE ( 'NONE', #71147, #84553, #18624, .T. ) ;
#108129 = CARTESIAN_POINT ( 'NONE',  ( 20.51925379220000067, 1409.629608526529864, 217.0260594629280035 ) ) ;
#108130 = FACE_OUTER_BOUND ( 'NONE', #108151, .T. ) ;
#108131 = ADVANCED_FACE ( 'NONE', ( #95315 ), #87696, .T. ) ;
#108132 = CARTESIAN_POINT ( 'NONE',  ( 1.012183099500000072, 1463.352738468689950, 230.5387435546990105 ) ) ;
#108133 = CARTESIAN_POINT ( 'NONE',  ( -17.34583796720000137, 1423.871196963929833, 227.2247444212979985 ) ) ;
#108135 = CARTESIAN_POINT ( 'NONE',  ( -4.155669664704369382, 1439.704322410719897, 185.4969487652249995 ) ) ;
#108134 = CARTESIAN_POINT ( 'NONE',  ( -4.598104748810852627, 1511.399590460244326, 200.7322199627068642 ) ) ;
#108136 = CARTESIAN_POINT ( 'NONE',  ( 27.12645382674940109, 1488.751129074109940, 207.9500232232510086 ) ) ;
#108137 = CARTESIAN_POINT ( 'NONE',  ( -123.5941673823403306, 1331.448250124728247, 287.0365551081088142 ) ) ;
#108138 = FACE_OUTER_BOUND ( 'NONE', #48192, .T. ) ;
#108139 = CARTESIAN_POINT ( 'NONE',  ( -21.53565904410000087, 1506.077647802389947, 209.2113159668039941 ) ) ;
#108140 = AXIS2_PLACEMENT_3D ( 'NONE', #50794, #32874, #15509 ) ;
#108141 = CARTESIAN_POINT ( 'NONE',  ( -5.065976868932539290, 1375.180419861180098, 203.5022389763250033 ) ) ;
#108142 = CARTESIAN_POINT ( 'NONE',  ( -4.622842882315000068, 1516.901952101700090, 205.0913314195169903 ) ) ;
#108143 = CARTESIAN_POINT ( 'NONE',  ( -6.512854995241789346, 1485.815955151150092, 183.1454636990030167 ) ) ;
#108144 = ORIENTED_EDGE ( 'NONE', *, *, #61343, .T. ) ;
#108145 = AXIS2_PLACEMENT_3D ( 'NONE', #65523, #12493, #91251 ) ;
#108146 = CARTESIAN_POINT ( 'NONE',  ( -17.83486663330464950, 1523.678648413191695, 237.8759530894961074 ) ) ;
#108147 = CARTESIAN_POINT ( 'NONE',  ( -4.250056676659310639, 1441.348028558830038, 161.1060492004820048 ) ) ;
#108148 = VECTOR ( 'NONE', #35966, 1000.000000000000114 ) ;
#108150 = ORIENTED_EDGE ( 'NONE', *, *, #34092, .T. ) ;
#108149 = CARTESIAN_POINT ( 'NONE',  ( -68.61976775002999318, 1379.747679567690057, 280.2166557527820032 ) ) ;
#108151 = EDGE_LOOP ( 'NONE', ( #4185, #87645, #109529, #105816 ) ) ;
#108152 = CARTESIAN_POINT ( 'NONE',  ( 22.74803453391442787, 1523.678648413191695, 183.6833808205261676 ) ) ;
#108153 = ORIENTED_EDGE ( 'NONE', *, *, #108912, .F. ) ;
#108154 = DIRECTION ( 'NONE',  ( 1.755985294532464991E-16, -1.000000000000000000, 1.338183447452830017E-16 ) ) ;
#108155 = CARTESIAN_POINT ( 'NONE',  ( 11.40388019490000104, 1502.140095079889988, 207.7801577285290193 ) ) ;
#108157 = CARTESIAN_POINT ( 'NONE',  ( 15.79075242492770315, 1409.464554496639948, 192.8587461545550070 ) ) ;
#108156 = CARTESIAN_POINT ( 'NONE',  ( -11.61544799517619886, 1425.877524782230012, 142.6765297559990131 ) ) ;
#108158 = CARTESIAN_POINT ( 'NONE',  ( -0.7374509209069979310, 1516.978425811520083, 210.2554991112269818 ) ) ;
#108159 = EDGE_CURVE ( 'NONE', #88484, #42556, #80503, .T. ) ;
#108160 = CARTESIAN_POINT ( 'NONE',  ( -107.1247494950929990, 1378.913060387289988, 307.3562546172859697 ) ) ;
#108161 = DIRECTION ( 'NONE',  ( -0.000000000000000000, -1.000000000000000000, -0.000000000000000000 ) ) ;
#108162 = CARTESIAN_POINT ( 'NONE',  ( 12.47249016976989999, 1501.230039276080106, 211.6023161739269938 ) ) ;
#108163 = PRODUCT_DEFINITION_SHAPE ( 'NONE', 'NONE',  #102745 ) ;
#108164 = EDGE_CURVE ( 'NONE', #77584, #26024, #55136, .T. ) ;
#108165 = DIRECTION ( 'NONE',  ( 0.9942586961433749204, -3.929125341476398997E-15, -0.1070030146457386366 ) ) ;
#108166 = CARTESIAN_POINT ( 'NONE',  ( -40.27281773781609786, 1443.421733393530303, 137.0938879172039719 ) ) ;
#108167 = CARTESIAN_POINT ( 'NONE',  ( -20.43379574667769916, 1466.940197274710044, 211.2182803883939926 ) ) ;
#108168 = DIRECTION ( 'NONE',  ( 1.755985294532464991E-16, -1.000000000000000000, 1.338183447452830017E-16 ) ) ;
#108169 = ORIENTED_EDGE ( 'NONE', *, *, #29514, .F. ) ;
#108170 = ORIENTED_EDGE ( 'NONE', *, *, #107638, .F. ) ;
#108171 = CARTESIAN_POINT ( 'NONE',  ( 10.04954308034672650, 1410.638657478467394, 229.7980651590800960 ) ) ;
#108172 = CARTESIAN_POINT ( 'NONE',  ( 0.009922064841440000546, 1452.352461717429833, 183.2658050908980272 ) ) ;
#108173 = CARTESIAN_POINT ( 'NONE',  ( -18.41923349776079633, 1508.551704408389924, 210.4158544684339915 ) ) ;
#108174 = CARTESIAN_POINT ( 'NONE',  ( -2.500000000000000000, 1439.615672362369878, 170.5246407198980023 ) ) ;
#108175 = CARTESIAN_POINT ( 'NONE',  ( -13.18452986259999982, 1379.569437749970120, 208.3223905408900123 ) ) ;
#108176 = CARTESIAN_POINT ( 'NONE',  ( 38.81202641429280220, 1436.797832205790201, 135.3769915889319861 ) ) ;
#108177 = CARTESIAN_POINT ( 'NONE',  ( 1.946844730679999858, 1465.062448901589960, 199.3137936548990012 ) ) ;
#108178 = CIRCLE ( 'NONE', #102799, 0.9999999999999976685 ) ;
#108179 = CARTESIAN_POINT ( 'NONE',  ( 25.87197768239999718, 1438.599946763920116, 137.3989826761979884 ) ) ;
#108180 = CARTESIAN_POINT ( 'NONE',  ( 2.121003584631406813, 1512.187213306747481, 239.6750300321239138 ) ) ;
#108181 = CARTESIAN_POINT ( 'NONE',  ( -82.48335923482800069, 1384.806338349549833, 286.1427824359119541 ) ) ;
#108182 = VERTEX_POINT ( 'NONE', #104266 ) ;
#108183 = CARTESIAN_POINT ( 'NONE',  ( 1.708747624254999931, 1517.213554313520035, 202.1696795498070003 ) ) ;
#108184 = CARTESIAN_POINT ( 'NONE',  ( -5.788691363644999477, 1517.157901477309906, 207.9987443536870160 ) ) ;
#108185 = ORIENTED_EDGE ( 'NONE', *, *, #32610, .T. ) ;
#108186 = CARTESIAN_POINT ( 'NONE',  ( 38.69786524538719874, 1440.913060387330006, 265.8278627617990537 ) ) ;
#108187 = B_SPLINE_CURVE_WITH_KNOTS ( 'NONE', 3,
 ( #90093, #48682, #13376, #107451, #4992, #31852, #29644, #5559 ),
 .UNSPECIFIED., .F., .F.,
 ( 4, 2, 2, 4 ),
 ( -0.07898079781686900835, -0.04381124047686119766, -0.01845156514537110715, 0.000000000000000000 ),
 .UNSPECIFIED. ) ;
#108188 = CARTESIAN_POINT ( 'NONE',  ( -0.0002161185356587633102, 1452.672516883277240, 153.3651468782901759 ) ) ;
#108189 = EDGE_LOOP ( 'NONE', ( #3972, #64088, #103934, #84299 ) ) ;
#108190 = CARTESIAN_POINT ( 'NONE',  ( -0.04116744988597149935, 1450.911622788300065, 181.8848909658740070 ) ) ;
#108191 = ADVANCED_FACE ( 'NONE', ( #61738 ), #57920, .F. ) ;
#108192 = CARTESIAN_POINT ( 'NONE',  ( -15.42891520709999931, 1409.953600697129787, 191.2302129608980010 ) ) ;
#108193 = CARTESIAN_POINT ( 'NONE',  ( 0.000000000000000000, 1414.913060387329779, 209.1218459616979999 ) ) ;
#108194 = CIRCLE ( 'NONE', #58172, 11.73843354579999954 ) ;
#108195 = CARTESIAN_POINT ( 'NONE',  ( -10.17685046697009987, 1462.839848933360145, 206.1631249775429922 ) ) ;
#108196 = FACE_OUTER_BOUND ( 'NONE', #38043, .T. ) ;
#108197 = CARTESIAN_POINT ( 'NONE',  ( -5.863482209052399696, 1511.603576927810082, 200.6690587505990209 ) ) ;
#108198 = CARTESIAN_POINT ( 'NONE',  ( -1.517310980229999995, 1507.186118473530087, 180.8246499581979947 ) ) ;
#108199 = CARTESIAN_POINT ( 'NONE',  ( -11.94157476580000043, 1433.614967702190143, 147.1502177932979976 ) ) ;
#108200 = DIRECTION ( 'NONE',  ( -0.7384854939285241393, 0.000000000000000000, 0.6742693640208961003 ) ) ;
#108202 = CARTESIAN_POINT ( 'NONE',  ( -23.98820069242849939, 1430.810317484149891, 210.9021713681929953 ) ) ;
#108201 = CARTESIAN_POINT ( 'NONE',  ( 12.32422840039999912, 1461.784851115730135, 233.7517049971980043 ) ) ;
#108203 = CARTESIAN_POINT ( 'NONE',  ( 5.316196956075327051, 1522.051704408389924, 187.2259631713411636 ) ) ;
#108204 = B_SPLINE_SURFACE_WITH_KNOTS ( 'NONE', 5, 5, ( 
 ( #52804, #88065, #43295, #44965, #69063, #43840 ),
 ( #744, #95343, #25904, #9129, #104295, #11351 ),
 ( #18604, #203, #34875, #103164, #26465, #60660 ),
 ( #35432, #34326, #69619, #45522, #86935, #36537 ),
 ( #94785, #18062, #52256, #9668, #19153, #10226 ),
 ( #60102, #35995, #94218, #70185, #28134, #44404 ),
 ( #17493, #10795, #77986, #61767, #1292, #27582 ),
 ( #95893, #53360, #62325, #51691, #79113, #70734 ),
 ( #104847, #96450, #85832, #28695, #89144, #97009 ) ),
 .UNSPECIFIED., .F., .F., .F.,
 ( 6, 3, 6 ),
 ( 6, 6 ),
 ( 3.139241426659999945, 5.400505795499999984, 7.661770164330000021 ),
 ( 0.000000000000000000, 2.000000000000000000 ),
 .UNSPECIFIED. ) ;
#108205 = CARTESIAN_POINT ( 'NONE',  ( 0.7526715501680020237, 1516.710624944440042, 216.8354948044169817 ) ) ;
#108206 = ORIENTED_EDGE ( 'NONE', *, *, #24196, .T. ) ;
#108207 = CARTESIAN_POINT ( 'NONE',  ( -5.334733590569999073, 1453.182326120890139, 200.0999779489789887 ) ) ;
#108208 = PRODUCT_RELATED_PRODUCT_CATEGORY ( 'part', '', ( #54500 ) ) ;
#108209 = CARTESIAN_POINT ( 'NONE',  ( -0.07873616178531450682, 1508.524200534259990, 180.2296851813550234 ) ) ;
#108210 = CARTESIAN_POINT ( 'NONE',  ( 31.26701299883995944, 1523.919943579690425, 221.8945623323605503 ) ) ;
#108211 = CARTESIAN_POINT ( 'NONE',  ( -2.284526496774999860, 1516.956048353049937, 212.5847947667770086 ) ) ;
#108212 = CARTESIAN_POINT ( 'NONE',  ( 18.65451744259999955, 1507.632629720729938, 188.5326157633979847 ) ) ;
#108213 = CARTESIAN_POINT ( 'NONE',  ( -11.60004869885203682, 1426.445093601214467, 138.8745978379924679 ) ) ;
#108215 = ORIENTED_EDGE ( 'NONE', *, *, #75832, .T. ) ;
#108214 = CARTESIAN_POINT ( 'NONE',  ( -11.82500768155940030, 1501.487207883790006, 211.3803078134539817 ) ) ;
#108216 = CARTESIAN_POINT ( 'NONE',  ( -20.15452302159999931, 1507.845791376729949, 228.9024215066979764 ) ) ;
#108217 = FACE_OUTER_BOUND ( 'NONE', #110236, .T. ) ;
#108218 = CARTESIAN_POINT ( 'NONE',  ( -10.96178248360000040, 1431.789698015990098, 151.7500217919979661 ) ) ;
#108219 = CARTESIAN_POINT ( 'NONE',  ( -4.329790274010359319, 1515.051704408389696, 205.2060425482763151 ) ) ;
#108220 = CARTESIAN_POINT ( 'NONE',  ( -109.9019402774279968, 1384.041146777030008, 311.3911408799560263 ) ) ;
#108221 = CARTESIAN_POINT ( 'NONE',  ( -18.80392059315889952, 1444.590799732510050, 207.5778593429040200 ) ) ;
#108222 = CARTESIAN_POINT ( 'NONE',  ( 12.65728676410210163, 1420.119835224449844, 200.3472210950669989 ) ) ;
#108223 = CARTESIAN_POINT ( 'NONE',  ( -5.560649665117820106, 1476.805467003079912, 214.4102409124259907 ) ) ;
#108224 = EDGE_CURVE ( 'NONE', #56949, #46666, #108450, .T. ) ;
#108226 = CARTESIAN_POINT ( 'NONE',  ( -12.78943302956389871, 1502.708798875820094, 209.0180534851929792 ) ) ;
#108225 = CARTESIAN_POINT ( 'NONE',  ( -19.65613647119999641, 1457.446755667530169, 225.8342101607980226 ) ) ;
#108227 = CARTESIAN_POINT ( 'NONE',  ( -12.91238589569339901, 1379.507750453399922, 211.2365448389620042 ) ) ;
#108228 = ORIENTED_EDGE ( 'NONE', *, *, #80254, .F. ) ;
#108229 = CARTESIAN_POINT ( 'NONE',  ( -6.561686461364999445, 1517.069378699710114, 205.6695567495270041 ) ) ;
#108230 = CARTESIAN_POINT ( 'NONE',  ( 6.204532493290000339, 1406.059425862230000, 267.5209521470980008 ) ) ;
#108231 = ADVANCED_FACE ( 'NONE', ( #85007, #26203 ), #18350, .T. ) ;
#108232 = CARTESIAN_POINT ( 'NONE',  ( -0.3258850517759999676, 1410.291732226329941, 185.0570438166979841 ) ) ;
#108233 = B_SPLINE_CURVE_WITH_KNOTS ( 'NONE', 3,
 ( #26804, #79430, #45289, #70502, #71055, #105178, #88374, #87842, #10563, #69391, #27354, #103502, #54248, #1078, #78887, #28469, #62098, #95117, #44175, #18381, #11130, #2193 ),
 .UNSPECIFIED., .F., .F.,
 ( 4, 2, 2, 1, 1, 1, 1, 2, 2, 2, 2, 2, 4 ),
 ( 0.000000000000000000, 0.2499999999997699618, 0.3749999999996527222, 0.4374999999995941025, 0.4687499999995649591, 0.4843749999995503597, 0.4921874999995429767, 0.4960937499995419775, 0.4999999999995410338, 0.7499999999997783995, 0.8124999999998353539, 0.8749999999998923084, 1.000000000000000000 ),
 .UNSPECIFIED. ) ;
#108234 = CARTESIAN_POINT ( 'NONE',  ( 10.86989410202379958, 1489.795966696680125, 207.8815529146370125 ) ) ;
#108235 = CARTESIAN_POINT ( 'NONE',  ( 24.22202933080170340, 1436.664598046718766, 213.2981740296385453 ) ) ;
#108236 = AXIS2_PLACEMENT_3D ( 'NONE', #32518, #109234, #67239 ) ;
#108237 = CARTESIAN_POINT ( 'NONE',  ( -24.43498997089999847, 1452.059775937329960, 135.9951607580979953 ) ) ;
#108238 = CARTESIAN_POINT ( 'NONE',  ( 27.44018068100522356, 1508.035990152466638, 213.3629281564213898 ) ) ;
#108239 = CARTESIAN_POINT ( 'NONE',  ( -10.22015420455159962, 1447.362584368680018, 210.7051702221340008 ) ) ;
#108240 = CARTESIAN_POINT ( 'NONE',  ( -1.962873838212560118, 1450.341737221240010, 154.5188792923449910 ) ) ;
#108241 = CARTESIAN_POINT ( 'NONE',  ( -12.36661650740000162, 1446.466068106850116, 187.6273874412979978 ) ) ;
#108242 = CARTESIAN_POINT ( 'NONE',  ( -19.62491598524822578, 1486.234197820471536, 189.9488111625408351 ) ) ;
#108243 = B_SPLINE_SURFACE_WITH_KNOTS ( 'NONE', 5, 5, ( 
 ( #52671, #44832, #26334, #95761, #52121, #96316 ),
 ( #85695, #19026, #10097, #34197, #70050, #35301 ),
 ( #103609, #44272, #36401, #43709, #70593, #78415 ),
 ( #2289, #104161, #94653, #616, #1170, #86249 ),
 ( #68936, #53229, #78986, #65, #87370, #9540 ),
 ( #104708, #85143, #8992, #77318, #1727, #43163 ),
 ( #26908, #77861, #61097, #34748, #28002, #95213 ),
 ( #27447, #8431, #42602, #35865, #76757, #68380 ),
 ( #25778, #59976, #94092, #17364, #19594, #62758 ) ),
 .UNSPECIFIED., .F., .F., .F.,
 ( 6, 3, 6 ),
 ( 6, 6 ),
 ( 4.218056259389999951, 8.316051950089999423, 13.74231060039999974 ),
 ( 0.000000000000000000, 2.000000000000000000 ),
 .UNSPECIFIED. ) ;
#108244 = CARTESIAN_POINT ( 'NONE',  ( -14.31665923842830068, 1416.051481378920016, 221.2469180764289831 ) ) ;
#108245 = CARTESIAN_POINT ( 'NONE',  ( -10.29050077590000001, 1499.663130460889988, 214.7767004497089829 ) ) ;
#108246 = CARTESIAN_POINT ( 'NONE',  ( -5.453001891610000484, 1437.869668061290213, 208.3330863909599771 ) ) ;
#108247 = CARTESIAN_POINT ( 'NONE',  ( -27.38276294334009719, 1507.983226544079798, 210.8770510937970073 ) ) ;
#108248 = CARTESIAN_POINT ( 'NONE',  ( 2.499999942879999715, 1440.188278801189881, 170.5317984358979970 ) ) ;
#108249 = CARTESIAN_POINT ( 'NONE',  ( -3.401812130889999786, 1475.226509619029912, 269.4945985741979939 ) ) ;
#108250 = CARTESIAN_POINT ( 'NONE',  ( -4.223240706370930297, 1446.235532200490070, 167.1955850464350135 ) ) ;
#108251 = CARTESIAN_POINT ( 'NONE',  ( -17.70270299129999714, 1414.019030144130056, 193.3444296426980316 ) ) ;
#108252 = EDGE_CURVE ( 'NONE', #86845, #46740, #48373, .T. ) ;
#108253 = DIRECTION ( 'NONE',  ( 1.755985294532464991E-16, -1.000000000000000000, 1.338183447452830017E-16 ) ) ;
#108254 = CARTESIAN_POINT ( 'NONE',  ( -50.54537835619269970, 1384.737437541280087, 262.8619960603269874 ) ) ;
#108255 = CARTESIAN_POINT ( 'NONE',  ( -107.2521063185319861, 1391.913060387289988, 301.2044319119630131 ) ) ;
#108256 = CARTESIAN_POINT ( 'NONE',  ( 4.240945049459830862, 1509.032014876047242, 212.8661584255399646 ) ) ;
#108257 = DIRECTION ( 'NONE',  ( 0.000000000000000000, 0.000000000000000000, 1.000000000000000000 ) ) ;
#108258 = CARTESIAN_POINT ( 'NONE',  ( 32.48455292688698393, 1524.659148609483054, 217.0704923713155949 ) ) ;
#108259 = CARTESIAN_POINT ( 'NONE',  ( -18.89905695062199698, 1416.828039266840278, 207.5749027128360069 ) ) ;
#108261 = EDGE_CURVE ( 'NONE', #56930, #55445, #75227, .T. ) ;
#108260 = AXIS2_PLACEMENT_3D ( 'NONE', #108193, #13564, #12490 ) ;
#108262 = CARTESIAN_POINT ( 'NONE',  ( -7.075873090581220301E-12, 1395.913060387330006, 220.1216245177919859 ) ) ;
#108263 =( BOUNDED_CURVE ( )  B_SPLINE_CURVE ( 3, ( #7017, #68598, #26566, #51791 ),
 .UNSPECIFIED., .F., .T. ) 
 B_SPLINE_CURVE_WITH_KNOTS ( ( 4, 4 ),
 ( 1.036083218751772561, 2.105411800329895833 ),
 .UNSPECIFIED. ) 
 CURVE ( )  GEOMETRIC_REPRESENTATION_ITEM ( )  RATIONAL_B_SPLINE_CURVE ( ( 1.000000000000000000, 0.9069598260854428995, 0.9069598260854428995, 1.000000000000000000 ) ) 
 REPRESENTATION_ITEM ( '' )  );
#108264 = EDGE_CURVE ( 'NONE', #49508, #27633, #60958, .T. ) ;
#108265 = CARTESIAN_POINT ( 'NONE',  ( 12.87612663444389938, 1421.246860338839952, 205.1732608065919976 ) ) ;
#108266 = CARTESIAN_POINT ( 'NONE',  ( -35.13956213160000175, 1419.958835960429951, 269.8639799881980252 ) ) ;
#108267 = ORIENTED_EDGE ( 'NONE', *, *, #72159, .T. ) ;
#108268 = CARTESIAN_POINT ( 'NONE',  ( -2.276495432953816511, 1410.370859958793062, 232.7304497416644438 ) ) ;
#108269 = DIRECTION ( 'NONE',  ( 0.8200914087127335605, -0.4884709562386523873, -0.2980708074717494660 ) ) ;
#108270 = AXIS2_PLACEMENT_3D ( 'NONE', #31469, #72405, #47737 ) ;
#108271 = CARTESIAN_POINT ( 'NONE',  ( -14.38097912129089906, 1422.143799352299993, 196.2925665020329973 ) ) ;
#108273 = DIRECTION ( 'NONE',  ( 1.000000000000000000, 2.249639673992789970E-32, 1.224646799147350002E-16 ) ) ;
#108272 = CARTESIAN_POINT ( 'NONE',  ( -16.49435349732149803, 1417.029099322570119, 208.6185211527730132 ) ) ;
#108274 = DIRECTION ( 'NONE',  ( -1.000000000000000000, 0.000000000000000000, 0.000000000000000000 ) ) ;
#108275 = CARTESIAN_POINT ( 'NONE',  ( -8.532458278280000030, 1445.788163739789979, 215.0754535007789912 ) ) ;
#108276 = CARTESIAN_POINT ( 'NONE',  ( -4.863842518140000237, 1453.445020719190097, 199.8398594391789800 ) ) ;
#108277 = EDGE_CURVE ( 'NONE', #77300, #20038, #103830, .T. ) ;
#108278 = CARTESIAN_POINT ( 'NONE',  ( 7.715625202974999652, 1516.786099423779888, 202.5670817708370066 ) ) ;
#108279 = CARTESIAN_POINT ( 'NONE',  ( 7.477834654460000507, 1427.293509551050192, 212.7723093538689909 ) ) ;
#108280 = CARTESIAN_POINT ( 'NONE',  ( -9.584198994920001269, 1428.531551829730233, 147.0197059986979866 ) ) ;
#108281 = CARTESIAN_POINT ( 'NONE',  ( 16.64927606573499830, 1512.799725290110018, 197.0740121610670030 ) ) ;
#108282 = CARTESIAN_POINT ( 'NONE',  ( -15.71863267061869962, 1420.991171932389989, 203.3936535414759703 ) ) ;
#108283 = CARTESIAN_POINT ( 'NONE',  ( -11.23768197768379906, 1379.896853569739960, 211.2083033905840352 ) ) ;
#108284 = CARTESIAN_POINT ( 'NONE',  ( 20.51030872011919826, 1508.877646971749982, 228.8223684417449988 ) ) ;
#108285 = ADVANCED_FACE ( 'NONE', ( #67693 ), #101801, .F. ) ;
#108287 = ORIENTED_EDGE ( 'NONE', *, *, #20636, .F. ) ;
#108286 = CARTESIAN_POINT ( 'NONE',  ( 10.13545555999999870, 1453.511788975089985, 212.2748783715589980 ) ) ;
#108288 = ORIENTED_EDGE ( 'NONE', *, *, #94158, .T. ) ;
#108289 = CARTESIAN_POINT ( 'NONE',  ( -11.56322555989999934, 1396.494206780630066, 212.6176595098179973 ) ) ;
#108290 = CARTESIAN_POINT ( 'NONE',  ( -19.37964200209999888, 1409.589812403130054, 219.8414950337979974 ) ) ;
#108291 = ORIENTED_EDGE ( 'NONE', *, *, #66749, .F. ) ;
#108292 = CARTESIAN_POINT ( 'NONE',  ( -12.97512972099614892, 1444.891494972908504, 169.4251994755254884 ) ) ;
#108293 = CARTESIAN_POINT ( 'NONE',  ( -0.04548916784355099691, 1416.835419214280137, 227.2860346676060033 ) ) ;
#108294 = LINE ( 'NONE', #83096, #51644 ) ;
#108296 = CARTESIAN_POINT ( 'NONE',  ( 17.35196363740000081, 1421.690952144829907, 226.5939839563979774 ) ) ;
#108295 = CARTESIAN_POINT ( 'NONE',  ( 2.189499658180000363, 1445.800293503789817, 199.2521182821290040 ) ) ;
#108297 = EDGE_CURVE ( 'NONE', #53518, #48271, #98099, .T. ) ;
#108298 = CARTESIAN_POINT ( 'NONE',  ( 1.616461792820000021, 1449.240018237009963, 183.6572643142980326 ) ) ;
#108299 = CARTESIAN_POINT ( 'NONE',  ( -4.534957494478200068, 1464.558362628190025, 199.0720338271949856 ) ) ;
#108300 = CARTESIAN_POINT ( 'NONE',  ( 1.225455118299999979, 1418.194176457360072, 204.0816376824290046 ) ) ;
#108302 = EDGE_CURVE ( 'NONE', #642, #53387, #107055, .T. ) ;
#108301 = CARTESIAN_POINT ( 'NONE',  ( 11.07060849806599911, 1396.299654554839890, 208.8974423235020197 ) ) ;
#108303 = CARTESIAN_POINT ( 'NONE',  ( 1.556584322539999787, 1415.163755998629995, 191.2532905271980042 ) ) ;
#108304 = CARTESIAN_POINT ( 'NONE',  ( 10.83255468690000001, 1424.906521154930033, 145.5564295056979915 ) ) ;
#108305 = CARTESIAN_POINT ( 'NONE',  ( 17.11714618750000128, 1443.086052842849995, 162.7561046190980107 ) ) ;
#108306 = VERTEX_POINT ( 'NONE', #79943 ) ;
#108307 = CARTESIAN_POINT ( 'NONE',  ( 12.93434948142389906, 1435.679596294389967, 150.6798643324129898 ) ) ;
#108308 = CARTESIAN_POINT ( 'NONE',  ( 2.062938842272421525, 1450.143278206232480, 181.9957652172806775 ) ) ;
#108309 = VERTEX_POINT ( 'NONE', #45259 ) ;
#108310 = EDGE_CURVE ( 'NONE', #63480, #92455, #44700, .T. ) ;
#108311 = ORIENTED_EDGE ( 'NONE', *, *, #110159, .F. ) ;
#108312 = CARTESIAN_POINT ( 'NONE',  ( -5.010230551890000328, 1425.855359004169941, 208.5321073727319856 ) ) ;
#108313 = CARTESIAN_POINT ( 'NONE',  ( -15.74154650769999897, 1459.394320623929843, 230.7248345380980084 ) ) ;
#108314 = CARTESIAN_POINT ( 'NONE',  ( -109.4770690486002422, 1386.916355746966929, 311.1337243306537061 ) ) ;
#108315 = CARTESIAN_POINT ( 'NONE',  ( 7.330554133425000174, 1516.857992118400034, 216.4511490482170188 ) ) ;
#108316 = CARTESIAN_POINT ( 'NONE',  ( -12.31936382470650138, 1378.277364386369982, 209.5341328486059922 ) ) ;
#108317 = EDGE_CURVE ( 'NONE', #74608, #94671, #3634, .T. ) ;
#108318 = ORIENTED_EDGE ( 'NONE', *, *, #33237, .T. ) ;
#108319 = CARTESIAN_POINT ( 'NONE',  ( -11.42889282249999994, 1501.636458983090051, 208.2613504466779943 ) ) ;
#108320 = CARTESIAN_POINT ( 'NONE',  ( 2.500000000000000000, 1448.308226215490095, 164.1023061046490170 ) ) ;
#108321 = CARTESIAN_POINT ( 'NONE',  ( -29.97486656949999784, 1376.157435337470133, 213.1946222555589827 ) ) ;
#108322 = AXIS2_PLACEMENT_3D ( 'NONE', #99601, #82814, #90104 ) ;
#108323 = VERTEX_POINT ( 'NONE', #11092 ) ;
#108324 = CARTESIAN_POINT ( 'NONE',  ( -0.7572979743539989261, 1516.829948096479939, 205.6721984920870057 ) ) ;
#108325 = ORIENTED_EDGE ( 'NONE', *, *, #15978, .F. ) ;
#108326 = CARTESIAN_POINT ( 'NONE',  ( -6.562094107424999656, 1517.122674412569950, 208.3832410274270046 ) ) ;
#108327 = CARTESIAN_POINT ( 'NONE',  ( -21.39772452180000073, 1509.704964747930035, 229.7894198983979948 ) ) ;
#108328 = B_SPLINE_SURFACE_WITH_KNOTS ( 'NONE', 5, 5, ( 
 ( #45392, #104714, #46492, #80625, #62763, #88477 ),
 ( #28007, #38605, #96880, #27453, #38067, #72244 ),
 ( #106371, #29658, #61637, #63844, #20149, #45931 ),
 ( #23458, #100708, #40264, #30200, #65492, #90661 ),
 ( #7224, #14501, #64391, #98512, #47575, #57652 ),
 ( #23989, #83920, #83362, #21780, #13944, #32425 ),
 ( #6108, #39721, #73885, #91220, #66604, #91764 ),
 ( #100173, #5570, #22885, #66050, #6662, #99602 ),
 ( #73328, #15040, #108013, #58185, #57095, #72785 ),
 ( #107463, #48691, #49239, #31309, #74447, #48134 ),
 ( #106912, #82815, #82272, #92313, #5007, #55982 ),
 ( #90105, #108573, #31862, #40815, #74994, #15584 ) ),
 .UNSPECIFIED., .F., .F., .F.,
 ( 6, 3, 3, 6 ),
 ( 6, 6 ),
 ( 31.69285121669999938, 50.14584306709999595, 68.35602240260000428, 108.8243570000000062 ),
 ( -9.967974889959999953E-09, 15.21005427680000111 ),
 .UNSPECIFIED. ) ;
#108329 = CARTESIAN_POINT ( 'NONE',  ( -39.55833958944460704, 1430.592406935262488, 269.6025355008150655 ) ) ;
#108330 = CARTESIAN_POINT ( 'NONE',  ( -2.069513320929999622, 1408.985329384930083, 231.7586132267979906 ) ) ;
#108332 = ORIENTED_EDGE ( 'NONE', *, *, #94245, .F. ) ;
#108331 = CARTESIAN_POINT ( 'NONE',  ( 0.2465388108663439937, 1414.971349104640012, 225.7948585416679634 ) ) ;
#108333 = CARTESIAN_POINT ( 'NONE',  ( 24.57684123230000139, 1440.965828712510074, 212.8359049822580289 ) ) ;
#108334 = CARTESIAN_POINT ( 'NONE',  ( -29.65916216564760077, 1440.913060386779989, 237.2382442218989809 ) ) ;
#108335 = CARTESIAN_POINT ( 'NONE',  ( -47.38717424370000231, 1384.438055640320044, 256.2720914158589949 ) ) ;
#108336 = CARTESIAN_POINT ( 'NONE',  ( -0.1267477471548290047, 1466.039099894230048, 235.8527109107560022 ) ) ;
#108337 = B_SPLINE_CURVE_WITH_KNOTS ( 'NONE', 5,
 ( #34966, #10889, #8650, #19818, #26563, #69715, #36089, #104941, #42827 ),
 .UNSPECIFIED., .F., .F.,
 ( 6, 3, 6 ),
 ( 234.6130002419999983, 237.3878297990000021, 239.4206172199999969 ),
 .UNSPECIFIED. ) ;
#108338 = CARTESIAN_POINT ( 'NONE',  ( 13.03173489774369997, 1411.479542611389888, 269.8789902196239723 ) ) ;
#108339 = CARTESIAN_POINT ( 'NONE',  ( -2.866857931135000204, 1516.951766529250108, 213.1652121904069759 ) ) ;
#108340 = CARTESIAN_POINT ( 'NONE',  ( 22.81565299040000028, 1409.709731146529975, 209.0774165718939912 ) ) ;
#108341 = EDGE_CURVE ( 'NONE', #86690, #76843, #94958, .T. ) ;
#108342 = FACE_OUTER_BOUND ( 'NONE', #4450, .T. ) ;
#108343 = CARTESIAN_POINT ( 'NONE',  ( 12.03563314606459933, 1492.750536582230097, 211.9176864492389996 ) ) ;
#108345 = CARTESIAN_POINT ( 'NONE',  ( -7.715586062468250184, 1516.784603496080081, 209.6398392507250321 ) ) ;
#108344 = CIRCLE ( 'NONE', #17103, 0.5000000000000000000 ) ;
#108346 = CARTESIAN_POINT ( 'NONE',  ( 3.269025135755000200, 1517.026534522949987, 210.2412850599169758 ) ) ;
#108348 = ADVANCED_FACE ( 'NONE', ( #2707 ), #45810, .F. ) ;
#108347 = CARTESIAN_POINT ( 'NONE',  ( -2.864433789270523167, 1447.807611701459109, 154.7916386383528504 ) ) ;
#108349 = CARTESIAN_POINT ( 'NONE',  ( -31.92108011125336375, 1511.187213306747708, 220.9591791661900686 ) ) ;
#108350 = CARTESIAN_POINT ( 'NONE',  ( 10.97212503029999908, 1432.504868931790043, 151.7700489660979883 ) ) ;
#108352 = ORIENTED_EDGE ( 'NONE', *, *, #13931, .T. ) ;
#108351 = CARTESIAN_POINT ( 'NONE',  ( -28.59007200240000302, 1388.502510938900059, 224.5857233694589752 ) ) ;
#108353 = CARTESIAN_POINT ( 'NONE',  ( -50.29540186739819774, 1385.120236129709838, 262.3351411316949680 ) ) ;
#108354 = CARTESIAN_POINT ( 'NONE',  ( 18.89942250099999654, 1416.835808384130132, 210.6687153374880097 ) ) ;
#108355 = CARTESIAN_POINT ( 'NONE',  ( -17.17007368362429531, 1414.941152333210539, 207.7552173661434551 ) ) ;
#108356 = CIRCLE ( 'NONE', #108094, 1.999999999999995559 ) ;
#108357 = FACE_OUTER_BOUND ( 'NONE', #5543, .T. ) ;
#108358 = CARTESIAN_POINT ( 'NONE',  ( -5.411774941350000034, 1435.306181909920042, 154.6725816278979835 ) ) ;
#108359 = CARTESIAN_POINT ( 'NONE',  ( 11.51329883360000039, 1422.113191770029971, 206.0591625496990105 ) ) ;
#108360 = CARTESIAN_POINT ( 'NONE',  ( 1.155535764753627292, 1498.748878490413290, 197.8505271270100252 ) ) ;
#108361 = ADVANCED_FACE ( 'NONE', ( #87236 ), #3259, .F. ) ;
#108363 = CARTESIAN_POINT ( 'NONE',  ( -8.861845913810000752, 1384.884034691229999, 218.6850541249889943 ) ) ;
#108362 = CARTESIAN_POINT ( 'NONE',  ( -7.329303116114999739, 1516.857992118400034, 216.4524001036569985 ) ) ;
#108364 = CARTESIAN_POINT ( 'NONE',  ( 2.981764508932377655, 1456.749145576906358, 198.8578630351947538 ) ) ;
#108365 = CARTESIAN_POINT ( 'NONE',  ( 31.03088476499823045, 1523.982201850120191, 221.8691499995717606 ) ) ;
#108366 = ORIENTED_EDGE ( 'NONE', *, *, #86, .T. ) ;
#108367 = CARTESIAN_POINT ( 'NONE',  ( -2.873329398885000163, 1516.572193931679976, 201.7997408644770019 ) ) ;
#108368 = CARTESIAN_POINT ( 'NONE',  ( -15.46640442256500059, 1511.810036768419877, 221.1669702143669838 ) ) ;
#108369 = ORIENTED_EDGE ( 'NONE', *, *, #105916, .T. ) ;
#108370 = CARTESIAN_POINT ( 'NONE',  ( -27.02655812420177028, 1451.969196582628911, 135.3522152283978528 ) ) ;
#108371 = CARTESIAN_POINT ( 'NONE',  ( 2.326513265190000013, 1476.258183643389884, 197.8633931559990060 ) ) ;
#108372 = CARTESIAN_POINT ( 'NONE',  ( 7.151890254928414237, 1438.987468099824355, 154.0970018937933332 ) ) ;
#108373 = CARTESIAN_POINT ( 'NONE',  ( 8.913965239475833968, 1424.958290419335526, 195.7060191906770399 ) ) ;
#108374 = CARTESIAN_POINT ( 'NONE',  ( -1.349081561059999990, 1443.127676870989944, 219.0403161255090083 ) ) ;
#108375 = CARTESIAN_POINT ( 'NONE',  ( 6.975311473106522442, 1416.765600848013037, 231.0738521692657059 ) ) ;
#108376 = EDGE_CURVE ( 'NONE', #76626, #38078, #17954, .T. ) ;
#108377 = FACE_OUTER_BOUND ( 'NONE', #72269, .T. ) ;
#108378 = CARTESIAN_POINT ( 'NONE',  ( -18.92517849950000297, 1425.859884652129949, 225.1369558184979951 ) ) ;
#108379 = CARTESIAN_POINT ( 'NONE',  ( 8.338382627507524347, 1487.567140753732701, 202.1928651156333956 ) ) ;
#108380 = CARTESIAN_POINT ( 'NONE',  ( -106.9747615859999996, 1387.585777271070128, 298.0968282848589865 ) ) ;
#108381 = CARTESIAN_POINT ( 'NONE',  ( 20.15502270700000054, 1507.862952647929887, 189.3407284623980047 ) ) ;
#108382 = B_SPLINE_CURVE_WITH_KNOTS ( 'NONE', 3,
 ( #98151, #46139, #28757, #104356, #37162, #62961, #45586, #88676, #45034, #21425 ),
 .UNSPECIFIED., .F., .F.,
 ( 4, 2, 2, 2, 4 ),
 ( 1.301042606982605321E-18, 0.0007406479101618187273, 0.001481295820323636154, 0.002221943730485453471, 0.002962591640647271006 ),
 .UNSPECIFIED. ) ;
#108383 = CARTESIAN_POINT ( 'NONE',  ( -106.1541768740000009, 1391.913060387289988, 303.5024934578589750 ) ) ;
#108384 = CARTESIAN_POINT ( 'NONE',  ( -31.28589133189229443, 1461.258894143585167, 269.4849877309756607 ) ) ;
#108385 = VERTEX_POINT ( 'NONE', #3816 ) ;
#108387 = EDGE_CURVE ( 'NONE', #7904, #21837, #73382, .T. ) ;
#108386 = CARTESIAN_POINT ( 'NONE',  ( -9.526130908711980538, 1440.436523450050117, 205.9995045934610118 ) ) ;
#108388 = CARTESIAN_POINT ( 'NONE',  ( -33.30421208489385521, 1417.542625019127172, 269.2880441342906011 ) ) ;
#108389 = CARTESIAN_POINT ( 'NONE',  ( -17.61566626013477332, 1524.599984580802357, 237.5963446818502973 ) ) ;
#108390 = CARTESIAN_POINT ( 'NONE',  ( -0.9766393796380001824, 1453.313060387329870, 229.7750655478980093 ) ) ;
#108391 = CARTESIAN_POINT ( 'NONE',  ( -32.38601544705593938, 1523.530935881284904, 202.1199691060090515 ) ) ;
#108392 = CARTESIAN_POINT ( 'NONE',  ( -12.55703987801026500, 1442.777179238205917, 186.0009298388953880 ) ) ;
#108393 = CARTESIAN_POINT ( 'NONE',  ( 2.470168521978398868, 1501.977400791986611, 175.3649660270905315 ) ) ;
#108394 = CARTESIAN_POINT ( 'NONE',  ( -2.849562163009459859, 1515.551843419029865, 213.1048050409179950 ) ) ;
#108395 = CARTESIAN_POINT ( 'NONE',  ( -2.694739704345535891, 1517.051704408389924, 212.0779207114006510 ) ) ;
#108396 = CARTESIAN_POINT ( 'NONE',  ( 24.45953054869999832, 1435.631735371460081, 137.6709130696980026 ) ) ;
#108397 = CARTESIAN_POINT ( 'NONE',  ( -12.72569297477883588, 1442.818307999958733, 169.4573488157998611 ) ) ;
#108399 = ORIENTED_EDGE ( 'NONE', *, *, #56286, .T. ) ;
#108398 = CARTESIAN_POINT ( 'NONE',  ( -15.06903107870000191, 1410.389868148830146, 226.7125060204980116 ) ) ;
#108400 = DIRECTION ( 'NONE',  ( -1.000000000000000000, 0.000000000000000000, 0.000000000000000000 ) ) ;
#108401 = EDGE_CURVE ( 'NONE', #38113, #1907, #46979, .T. ) ;
#108402 = CARTESIAN_POINT ( 'NONE',  ( -3.805207261640000116, 1409.045941153030071, 230.7650822874980179 ) ) ;
#108403 = ORIENTED_EDGE ( 'NONE', *, *, #13079, .F. ) ;
#108404 = VERTEX_POINT ( 'NONE', #40131 ) ;
#108405 = CARTESIAN_POINT ( 'NONE',  ( 16.06427069504690053, 1414.913060387399810, 208.9262394168359833 ) ) ;
#108406 = CARTESIAN_POINT ( 'NONE',  ( -9.196349486490200675, 1517.051704408389924, 203.7768694350468195 ) ) ;
#108408 = CARTESIAN_POINT ( 'NONE',  ( -25.51518049010000055, 1444.285382571919854, 220.8700590728979876 ) ) ;
#108407 = FACE_OUTER_BOUND ( 'NONE', #456, .T. ) ;
#108409 = CARTESIAN_POINT ( 'NONE',  ( -1.795663807680000001, 1444.786284551390054, 217.9357666183690014 ) ) ;
#108410 = CARTESIAN_POINT ( 'NONE',  ( -11.46969010090000118, 1433.199005582570180, 151.2954870453980050 ) ) ;
#108411 = ADVANCED_FACE ( 'NONE', ( #99470 ), #33012, .F. ) ;
#108412 = FACE_OUTER_BOUND ( 'NONE', #45125, .T. ) ;
#108413 = CARTESIAN_POINT ( 'NONE',  ( 13.72878283421173506, 1517.051704408389924, 191.9723449582409955 ) ) ;
#108414 = CARTESIAN_POINT ( 'NONE',  ( -26.67861085519999875, 1438.479473329630082, 136.9888825721979799 ) ) ;
#108415 = CARTESIAN_POINT ( 'NONE',  ( -24.46932507910000254, 1440.032561122739935, 210.9836422549680037 ) ) ;
#108416 = FACE_BOUND ( 'NONE', #63257, .T. ) ;
#108417 = CARTESIAN_POINT ( 'NONE',  ( 1.521080599399999844, 1450.730010003210054, 182.2924144091979883 ) ) ;
#108418 = CARTESIAN_POINT ( 'NONE',  ( 7.930007129861151860, 1364.752738923533116, 209.6218459617148824 ) ) ;
#108419 = ADVANCED_FACE ( 'NONE', ( #106779 ), #56398, .F. ) ;
#108420 = CARTESIAN_POINT ( 'NONE',  ( -11.05120362203290618, 1509.424098794511337, 237.0121822441638813 ) ) ;
#108422 = ORIENTED_EDGE ( 'NONE', *, *, #63923, .T. ) ;
#108421 = CARTESIAN_POINT ( 'NONE',  ( -2.060856689691449839E-09, 1413.853476841760084, 248.1683309011359881 ) ) ;
#108423 = EDGE_LOOP ( 'NONE', ( #97598, #35323 ) ) ;
#108424 = CIRCLE ( 'NONE', #60164, 2.000000000000000000 ) ;
#108425 = CARTESIAN_POINT ( 'NONE',  ( -11.86598650706779878, 1432.328056081479872, 149.9824201572170352 ) ) ;
#108426 = CARTESIAN_POINT ( 'NONE',  ( -18.81286786266959865, 1505.121906714500028, 222.5033949973810081 ) ) ;
#108427 = CARTESIAN_POINT ( 'NONE',  ( -7.595213676849999374, 1473.705021973730027, 270.1248737330980134 ) ) ;
#108428 = CARTESIAN_POINT ( 'NONE',  ( -14.87168881317970026, 1430.147188212150240, 221.8136313441650032 ) ) ;
#108429 = CYLINDRICAL_SURFACE ( 'NONE', #11103, 10.00000000000000000 ) ;
#108430 = CARTESIAN_POINT ( 'NONE',  ( 34.46379809770260039, 1450.419497442319880, 136.2296061301330212 ) ) ;
#108431 = CARTESIAN_POINT ( 'NONE',  ( 4.327012391429460259, 1515.157834657049989, 209.2496350220929742 ) ) ;
#108432 = CARTESIAN_POINT ( 'NONE',  ( -8.154251837229999467, 1384.787012670900140, 199.6488997829790151 ) ) ;
#108433 = CARTESIAN_POINT ( 'NONE',  ( -0.6370436997426996983, 1517.151704408390060, 217.8527312947061603 ) ) ;
#108434 = CARTESIAN_POINT ( 'NONE',  ( -4.329448776275169664, 1515.064792882719985, 206.7917118343879963 ) ) ;
#108435 = B_SPLINE_CURVE_WITH_KNOTS ( 'NONE', 3,
 ( #34691, #16753, #101876, #102436, #94588, #7290, #76149, #50417, #43108, #52066, #32499, #92942, #68881, #49857, #41454, #26281, #76696, #102983, #59922, #8375, #60470, #17868 ),
 .UNSPECIFIED., .F., .F.,
 ( 4, 2, 2, 1, 1, 1, 1, 2, 2, 2, 2, 2, 4 ),
 ( 0.000000000000000000, 0.2499999999991435740, 0.3749999999987154720, 0.4374999999985075827, 0.4687499999983973931, 0.4843749999983563703, 0.4921874999983420484, 0.4960937499983150145, 0.4999999999982880361, 0.6249999999986949328, 0.6874999999989206412, 0.7499999999991464605, 1.000000000000000000 ),
 .UNSPECIFIED. ) ;
#108436 = CARTESIAN_POINT ( 'NONE',  ( 10.76932834697634611, 1366.129144616212216, 207.6218459616987673 ) ) ;
#108437 = CARTESIAN_POINT ( 'NONE',  ( -33.64184985774720360, 1416.594321794520056, 267.0652993242159710 ) ) ;
#108438 = ORIENTED_EDGE ( 'NONE', *, *, #78685, .T. ) ;
#108439 = CARTESIAN_POINT ( 'NONE',  ( -4.328570061217769549, 1515.098349647940040, 210.2573761392540064 ) ) ;
#108440 = EDGE_CURVE ( 'NONE', #107891, #88507, #50939, .T. ) ;
#108441 = EDGE_LOOP ( 'NONE', ( #36551, #52103, #26608, #23390 ) ) ;
#108442 = ORIENTED_EDGE ( 'NONE', *, *, #32346, .T. ) ;
#108443 = CARTESIAN_POINT ( 'NONE',  ( -4.995726007844999650, 1516.651306816259876, 211.4173314712770093 ) ) ;
#108444 = CARTESIAN_POINT ( 'NONE',  ( 4.608371281445468703, 1423.726610470979267, 183.8391095067188985 ) ) ;
#108445 = CARTESIAN_POINT ( 'NONE',  ( -2.500000000000000000, 1436.878463555260169, 183.6520988947980015 ) ) ;
#108446 = EDGE_CURVE ( 'NONE', #19741, #74400, #5508, .T. ) ;
#108448 = CARTESIAN_POINT ( 'NONE',  ( -17.64822974267435640, 1419.534037284996202, 207.1517795833794935 ) ) ;
#108447 = CARTESIAN_POINT ( 'NONE',  ( -7.710610441124999603, 1516.594591938570147, 212.5759658869370128 ) ) ;
#108449 = CARTESIAN_POINT ( 'NONE',  ( -17.25278045389999804, 1455.455490790330032, 189.9113160770979789 ) ) ;
#108450 = B_SPLINE_CURVE_WITH_KNOTS ( 'NONE', 5,
 ( #59296, #43034, #92861, #44141, #1046, #41922, #68257, #86127, #58726, #34618, #50877, #16138, #68803, #76078, #102905 ),
 .UNSPECIFIED., .F., .F.,
 ( 6, 3, 3, 3, 6 ),
 ( 0.000000000000000000, 0.1365561072326384739, 0.2978444876294450983, 0.5106123751859845683, 1.000000000000000000 ),
 .UNSPECIFIED. ) ;
#108451 = CARTESIAN_POINT ( 'NONE',  ( -2.359913115097718617, 1449.630106320913455, 182.9978952858132004 ) ) ;
#108452 = ORIENTED_EDGE ( 'NONE', *, *, #91858, .F. ) ;
#108453 = CARTESIAN_POINT ( 'NONE',  ( -26.07187536489999857, 1435.414138736239920, 135.5217793413980019 ) ) ;
#108454 = CARTESIAN_POINT ( 'NONE',  ( 5.002593359325000044, 1516.960844870249957, 202.5626772953570196 ) ) ;
#108455 = CARTESIAN_POINT ( 'NONE',  ( -41.63813745289505164, 1444.512220545661876, 135.5979520083818954 ) ) ;
#108456 = DIRECTION ( 'NONE',  ( -0.3255681544571569219, -1.836970198721028948E-16, -0.9455185755993167351 ) ) ;
#108457 = CARTESIAN_POINT ( 'NONE',  ( -40.61004888632240295, 1425.241059834939961, 269.7704499877880266 ) ) ;
#108458 = CARTESIAN_POINT ( 'NONE',  ( -16.66231036550741607, 1523.604703353109699, 180.4882076302515372 ) ) ;
#108459 = CARTESIAN_POINT ( 'NONE',  ( -1.244837129730000047, 1397.637433091830189, 196.1147955250980033 ) ) ;
#108461 = ORIENTED_EDGE ( 'NONE', *, *, #96150, .T. ) ;
#108460 = CARTESIAN_POINT ( 'NONE',  ( -8.910739657505105882, 1364.460249266779101, 207.6218459616988241 ) ) ;
#108462 = VERTEX_POINT ( 'NONE', #51859 ) ;
#108463 = DIRECTION ( 'NONE',  ( -0.000000000000000000, -1.000000000000000000, -0.000000000000000000 ) ) ;
#108464 = CARTESIAN_POINT ( 'NONE',  ( 1.704192342800000001E-13, 1475.048391919030109, 269.6500679772980220 ) ) ;
#108465 = CARTESIAN_POINT ( 'NONE',  ( 10.87353205008450097, 1460.686552688219990, 207.9238305753009683 ) ) ;
#108466 = CARTESIAN_POINT ( 'NONE',  ( -14.58761689442209963, 1436.245193537610021, 149.8743049802889971 ) ) ;
#108467 = CARTESIAN_POINT ( 'NONE',  ( -2.105916269280000197, 1485.584842596029830, 182.5101088919979873 ) ) ;
#108468 = CARTESIAN_POINT ( 'NONE',  ( 6.563254890855000134, 1517.139039350860003, 211.6051684241269868 ) ) ;
#108469 = CARTESIAN_POINT ( 'NONE',  ( -68.77345375519999493, 1379.748012843780089, 280.2452975165590487 ) ) ;
#108470 = FACE_OUTER_BOUND ( 'NONE', #62210, .T. ) ;
#108471 = CARTESIAN_POINT ( 'NONE',  ( -14.42407037529999947, 1430.147381752329920, 222.2644859324980189 ) ) ;
#108472 = CARTESIAN_POINT ( 'NONE',  ( 3.885349673800238879, 1440.907261985867081, 156.3247486698534487 ) ) ;
#108473 = CARTESIAN_POINT ( 'NONE',  ( 7.548380872364999661, 1510.399296111369949, 204.3167683741870064 ) ) ;
#108474 = ORIENTED_EDGE ( 'NONE', *, *, #48835, .T. ) ;
#108475 = CARTESIAN_POINT ( 'NONE',  ( 2.476170596904999854, 1516.819260244609950, 207.4047612206870213 ) ) ;
#108476 = ORIENTED_EDGE ( 'NONE', *, *, #18017, .F. ) ;
#108477 = CARTESIAN_POINT ( 'NONE',  ( -36.37832868406120213, 1451.642701156830071, 135.3761648280290046 ) ) ;
#108478 = CARTESIAN_POINT ( 'NONE',  ( -10.57604552250000118, 1471.371694624089741, 208.7882177754879933 ) ) ;
#108480 = B_SPLINE_CURVE_WITH_KNOTS ( 'NONE', 3,
 ( #8816, #461, #100135, #23420 ),
 .UNSPECIFIED., .F., .F.,
 ( 4, 4 ),
 ( 0.000000000000000000, 0.0002960034161023844057 ),
 .UNSPECIFIED. ) ;
#108479 = CARTESIAN_POINT ( 'NONE',  ( -20.69466133717958911, 1455.350803762641135, 223.8685399355039465 ) ) ;
#108481 = ORIENTED_EDGE ( 'NONE', *, *, #41059, .F. ) ;
#108482 = CARTESIAN_POINT ( 'NONE',  ( 20.21728935790000037, 1475.862786327189951, 209.1218459616989946 ) ) ;
#108483 = CARTESIAN_POINT ( 'NONE',  ( 12.92073010750949891, 1435.120627881940209, 150.2915359750790003 ) ) ;
#108484 = CARTESIAN_POINT ( 'NONE',  ( 13.97021087459999933, 1416.254459046630018, 196.4665394535979885 ) ) ;
#108485 = CARTESIAN_POINT ( 'NONE',  ( -11.95964865010000011, 1416.297031888519996, 205.9046802826989904 ) ) ;
#108486 = DIRECTION ( 'NONE',  ( 0.9483721503360844629, -0.1343667288060120535, 0.2872905265700261279 ) ) ;
#108487 = CARTESIAN_POINT ( 'NONE',  ( 3.503183429743535804, 1450.836852080426297, 184.0621120680351339 ) ) ;
#108488 = CARTESIAN_POINT ( 'NONE',  ( 7.407046107680000269, 1488.581653516390134, 199.5623810922690211 ) ) ;
#108489 = CARTESIAN_POINT ( 'NONE',  ( 31.34137657907887231, 1523.481610118014260, 221.9025654077128991 ) ) ;
#108490 = CARTESIAN_POINT ( 'NONE',  ( 23.79381763197114097, 1448.079399027135651, 216.0042285759331833 ) ) ;
#108491 = CARTESIAN_POINT ( 'NONE',  ( -12.00000000000000000, 1443.913060387330006, 150.5878346084980137 ) ) ;
#108492 = DIRECTION ( 'NONE',  ( 0.000000000000000000, 0.000000000000000000, 1.000000000000000000 ) ) ;
#108493 = CARTESIAN_POINT ( 'NONE',  ( -2.484577695354999616, 1517.170512887980067, 216.4602579296269766 ) ) ;
#108494 = VERTEX_POINT ( 'NONE', #102770 ) ;
#108495 = CARTESIAN_POINT ( 'NONE',  ( -17.58082291759999904, 1417.836406065290021, 206.7640894888989749 ) ) ;
#108496 = CARTESIAN_POINT ( 'NONE',  ( 0.000000000000000000, 1512.187213306747481, 209.1218459616979999 ) ) ;
#108497 = CARTESIAN_POINT ( 'NONE',  ( -17.45313156558830059, 1508.551704408389924, 211.9416870107529860 ) ) ;
#108498 = CARTESIAN_POINT ( 'NONE',  ( 1.366628593997903707, 1414.941152333447462, 191.9517722785298588 ) ) ;
#108499 = CARTESIAN_POINT ( 'NONE',  ( -3.721063415729999695E-09, 1475.837061091930082, 266.9611530633980010 ) ) ;
#108500 = CARTESIAN_POINT ( 'NONE',  ( 11.44982798326090290, 1425.806312135371854, 139.0983210244855854 ) ) ;
#108501 = CARTESIAN_POINT ( 'NONE',  ( -7.145324146093005702, 1508.387575007782061, 219.7168039286800081 ) ) ;
#108502 = CARTESIAN_POINT ( 'NONE',  ( 17.98447767965197741, 1424.110086477602408, 225.5366282599816543 ) ) ;
#108503 = CARTESIAN_POINT ( 'NONE',  ( -1.791500013333100050, 1454.995498928959933, 198.7702412911150134 ) ) ;
#108504 = CARTESIAN_POINT ( 'NONE',  ( 2.359533070475779804E-16, 1517.051704408389924, 209.1218459616989946 ) ) ;
#108505 = CARTESIAN_POINT ( 'NONE',  ( 31.79362791131370258, 1440.913060383409857, 243.5716590067270033 ) ) ;
#108507 = FACE_OUTER_BOUND ( 'NONE', #76945, .T. ) ;
#108506 = CARTESIAN_POINT ( 'NONE',  ( -10.26287757781059895, 1470.737246754300031, 211.5706239509080149 ) ) ;
#108508 = CARTESIAN_POINT ( 'NONE',  ( 13.11885828660000008, 1419.893985557330097, 221.7273098061980079 ) ) ;
#108509 = ORIENTED_EDGE ( 'NONE', *, *, #29151, .T. ) ;
#108510 = VERTEX_POINT ( 'NONE', #68668 ) ;
#108511 = CYLINDRICAL_SURFACE ( 'NONE', #55111, 2.000000000000003109 ) ;
#108512 = CARTESIAN_POINT ( 'NONE',  ( -19.67602081376940859, 1485.246767906123978, 190.3296067428275649 ) ) ;
#108513 = FACE_OUTER_BOUND ( 'NONE', #41142, .T. ) ;
#108514 = CARTESIAN_POINT ( 'NONE',  ( 11.53450314954949896, 1502.145229493909937, 211.3292107343589805 ) ) ;
#108515 = FACE_OUTER_BOUND ( 'NONE', #44720, .T. ) ;
#108516 = CARTESIAN_POINT ( 'NONE',  ( -11.73701141503820011, 1426.696005490819971, 144.1689084034089774 ) ) ;
#108517 = CARTESIAN_POINT ( 'NONE',  ( -16.75454338844117430, 1526.382868173645875, 234.5462402642023108 ) ) ;
#108518 = CARTESIAN_POINT ( 'NONE',  ( 1.473600209469299926, 1508.551704408389924, 219.7879707489230157 ) ) ;
#108519 = CARTESIAN_POINT ( 'NONE',  ( -50.70725589956350632, 1383.810751608489909, 262.7987874578989818 ) ) ;
#108520 = CARTESIAN_POINT ( 'NONE',  ( -3.481979457305000025, 1511.353635254350138, 201.3868063830669826 ) ) ;
#108521 = CARTESIAN_POINT ( 'NONE',  ( -0.2612772979118159755, 1416.851343897360039, 227.4677505453099968 ) ) ;
#108522 = CARTESIAN_POINT ( 'NONE',  ( -12.01522815608920070, 1502.252156548509902, 208.9183199409420126 ) ) ;
#108523 = CARTESIAN_POINT ( 'NONE',  ( 12.08872186521969994, 1492.701414612239887, 211.6956945743199867 ) ) ;
#108525 = EDGE_LOOP ( 'NONE', ( #13494, #35302, #3862, #35447, #28704, #69092, #22847, #91914, #104607, #89592 ) ) ;
#108524 = CARTESIAN_POINT ( 'NONE',  ( -2.525609700800000024, 1456.035086478289941, 218.2565648270789609 ) ) ;
#108526 = CARTESIAN_POINT ( 'NONE',  ( 32.59719044532317866, 1523.982201850120191, 217.0485567930457762 ) ) ;
#108527 = EDGE_CURVE ( 'NONE', #47285, #2864, #42902, .T. ) ;
#108528 = CARTESIAN_POINT ( 'NONE',  ( -45.95279786519999732, 1383.059815259339985, 219.1337940620589961 ) ) ;
#108529 = ADVANCED_FACE ( 'NONE', ( #60829 ), #76492, .T. ) ;
#108530 = CARTESIAN_POINT ( 'NONE',  ( 3.246944597107860098, 1508.551704408389924, 204.2527766185579878 ) ) ;
#108531 = ORIENTED_EDGE ( 'NONE', *, *, #104202, .T. ) ;
#108532 = ORIENTED_EDGE ( 'NONE', *, *, #4133, .T. ) ;
#108533 = CARTESIAN_POINT ( 'NONE',  ( -7.984562924460901101, 1386.832004956829905, 218.6792132728400020 ) ) ;
#108534 = CARTESIAN_POINT ( 'NONE',  ( -4.325403553846939531, 1515.219291385629958, 206.7919471186340274 ) ) ;
#108536 = CARTESIAN_POINT ( 'NONE',  ( -9.519812938348620079, 1460.017558366200092, 210.6311618255110147 ) ) ;
#108535 = FACE_OUTER_BOUND ( 'NONE', #63507, .T. ) ;
#108537 = CARTESIAN_POINT ( 'NONE',  ( -5.452217511760000690, 1462.447772966889943, 201.0260644561890047 ) ) ;
#108538 = CARTESIAN_POINT ( 'NONE',  ( -105.2984536779999871, 1379.565129866090047, 301.9749307548589741 ) ) ;
#108539 = CARTESIAN_POINT ( 'NONE',  ( -113.4000000000000057, 1377.913060387289988, 304.2218459572590064 ) ) ;
#108540 = APPLICATION_CONTEXT ( 'automotive_design' ) ;
#108541 = CARTESIAN_POINT ( 'NONE',  ( -13.81128163186000002, 1508.551704408389924, 215.9575079269010018 ) ) ;
#108542 = CARTESIAN_POINT ( 'NONE',  ( 10.58919714376239973, 1409.282843299900151, 198.5624303964659987 ) ) ;
#108543 = CARTESIAN_POINT ( 'NONE',  ( 18.80368963479999778, 1425.915429421829913, 225.1658117488979940 ) ) ;
#108544 = CYLINDRICAL_SURFACE ( 'NONE', #80454, 2.000000000000000000 ) ;
#108545 = CARTESIAN_POINT ( 'NONE',  ( 8.562350050396240420, 1433.778962878430093, 204.3790883806010186 ) ) ;
#108546 = CARTESIAN_POINT ( 'NONE',  ( -4.223640783000890409, 1441.596330317800039, 170.5493994362460057 ) ) ;
#108547 = CIRCLE ( 'NONE', #28062, 2.000000000000068390 ) ;
#108548 = ADVANCED_FACE ( 'NONE', ( #912, #59707 ), #69215, .F. ) ;
#108549 = DIRECTION ( 'NONE',  ( 0.9702683578407125253, 0.000000000000000000, -0.2420316379589395328 ) ) ;
#108550 = EDGE_LOOP ( 'NONE', ( #21739, #43527, #793, #31719 ) ) ;
#108551 = CARTESIAN_POINT ( 'NONE',  ( -1.623075365390000080, 1428.602351821930142, 149.4837496357980058 ) ) ;
#108552 = CARTESIAN_POINT ( 'NONE',  ( 18.61188344111999982, 1458.579614889230015, 227.5056110255299870 ) ) ;
#108553 = CARTESIAN_POINT ( 'NONE',  ( -11.39739833580000017, 1434.677645552710146, 151.4902371962980112 ) ) ;
#108554 = DIRECTION ( 'NONE',  ( -0.000000000000000000, -1.000000000000000000, -0.000000000000000000 ) ) ;
#108555 = CARTESIAN_POINT ( 'NONE',  ( -4.219438644781110526, 1441.595895916910195, 183.5288106640859951 ) ) ;
#108556 = CARTESIAN_POINT ( 'NONE',  ( -24.92720798968933238, 1436.178265573613999, 137.8894290697291751 ) ) ;
#108557 = CARTESIAN_POINT ( 'NONE',  ( -108.9096775629999883, 1387.161515960729957, 310.8237188872590195 ) ) ;
#108558 = CARTESIAN_POINT ( 'NONE',  ( -0.5561591756040000778, 1484.827948844329967, 181.8894219878979754 ) ) ;
#108559 = CARTESIAN_POINT ( 'NONE',  ( -10.74627850421423680, 1362.045253526237047, 208.3718459617010978 ) ) ;
#108560 = CARTESIAN_POINT ( 'NONE',  ( -45.85227038866229776, 1440.469603780929901, 268.7564394150250564 ) ) ;
#108561 = CARTESIAN_POINT ( 'NONE',  ( -19.04437315719999901, 1425.784752839030034, 226.3805134473980161 ) ) ;
#108562 = CARTESIAN_POINT ( 'NONE',  ( -19.99778532869999736, 1488.358619900530130, 191.8244647984979849 ) ) ;
#108563 = CARTESIAN_POINT ( 'NONE',  ( -5.006259886824999228, 1516.939723362869927, 209.1347437590049765 ) ) ;
#108564 = CARTESIAN_POINT ( 'NONE',  ( -25.07511837043467295, 1507.939514509590708, 198.1595777679482921 ) ) ;
#108565 = AXIS2_PLACEMENT_3D ( 'NONE', #30407, #98716, #5776 ) ;
#108566 = CARTESIAN_POINT ( 'NONE',  ( -32.28466283162165240, 1501.977400791986611, 199.0684425896249081 ) ) ;
#108567 = EDGE_CURVE ( 'NONE', #43145, #11042, #33666, .T. ) ;
#108568 = CARTESIAN_POINT ( 'NONE',  ( 8.690383195619999057, 1424.104242789630007, 112.3001073638979932 ) ) ;
#108569 = CARTESIAN_POINT ( 'NONE',  ( 6.965382933308789326, 1424.882428658780100, 213.2657788462730082 ) ) ;
#108570 = EDGE_LOOP ( 'NONE', ( #44178, #71977, #32451, #36916 ) ) ;
#108571 = CARTESIAN_POINT ( 'NONE',  ( 14.01630619149999823, 1418.416544456529891, 240.3753821261979908 ) ) ;
#108572 = CARTESIAN_POINT ( 'NONE',  ( -27.30475511710000092, 1508.128822472029924, 204.4091660346579999 ) ) ;
#108574 = LINE ( 'NONE', #101246, #32024 ) ;
#108573 = CARTESIAN_POINT ( 'NONE',  ( 0.5480496121420000977, 1452.697021778130193, 183.2754429902979894 ) ) ;
#108575 =( BOUNDED_CURVE ( )  B_SPLINE_CURVE ( 3, ( #56455, #22256, #46967, #97342 ),
 .UNSPECIFIED., .F., .F. ) 
 B_SPLINE_CURVE_WITH_KNOTS ( ( 4, 4 ),
 ( 3.141592653589793116, 4.712388980384689674 ),
 .UNSPECIFIED. ) 
 CURVE ( )  GEOMETRIC_REPRESENTATION_ITEM ( )  RATIONAL_B_SPLINE_CURVE ( ( 1.000000000000000000, 0.8047378541243649375, 0.8047378541243649375, 1.000000000000000000 ) ) 
 REPRESENTATION_ITEM ( '' )  );
#108576 = EDGE_CURVE ( 'NONE', #33227, #101013, #48375, .T. ) ;
#108577 = CARTESIAN_POINT ( 'NONE',  ( -2.713387635329040037, 1419.520833911499949, 186.1633376940620224 ) ) ;
#108578 = CARTESIAN_POINT ( 'NONE',  ( -19.57999073310000071, 1422.088355595230269, 238.2202611127979708 ) ) ;
#108579 = CARTESIAN_POINT ( 'NONE',  ( -5.080289282479999002, 1480.093209919690253, 228.8812397303989883 ) ) ;
#108580 = CARTESIAN_POINT ( 'NONE',  ( -22.49711446700899842, 1452.127443838799991, 139.6705065661170124 ) ) ;
#108581 = B_SPLINE_CURVE_WITH_KNOTS ( 'NONE', 3,
 ( #11930, #95936, #36578, #89730, #53398, #88103, #4630, #62938 ),
 .UNSPECIFIED., .F., .F.,
 ( 4, 2, 2, 4 ),
 ( -0.08162639889109629676, -0.08079092939402009177, -0.04068425817429450336, 0.000000000000000000 ),
 .UNSPECIFIED. ) ;
#108582 = CARTESIAN_POINT ( 'NONE',  ( -18.89942250099999654, 1416.835808384130132, 207.5749765859080185 ) ) ;
#108583 = VERTEX_POINT ( 'NONE', #106111 ) ;
#108584 = CARTESIAN_POINT ( 'NONE',  ( -2.500000000000000000, 1419.382782049920024, 144.1108465772580018 ) ) ;
#108585 = CARTESIAN_POINT ( 'NONE',  ( 2.603400736049609843E-05, 1407.928373405780121, 270.2926942668629522 ) ) ;
#108586 = CARTESIAN_POINT ( 'NONE',  ( 15.52525468725849933, 1421.896024094239920, 227.9304414622129968 ) ) ;
#108587 = CARTESIAN_POINT ( 'NONE',  ( 10.10980088610000038, 1462.073314986889955, 210.1684032625090026 ) ) ;
#108588 = ORIENTED_EDGE ( 'NONE', *, *, #48069, .T. ) ;
#108589 = EDGE_LOOP ( 'NONE', ( #82700, #68273, #31686, #39186 ) ) ;
#108590 = CARTESIAN_POINT ( 'NONE',  ( -58.29236204880000116, 1384.661700128139955, 240.0739325125589971 ) ) ;
#108591 = CARTESIAN_POINT ( 'NONE',  ( -23.03704750979090221, 1409.747334528499778, 208.9847852389330001 ) ) ;
#108592 = VERTEX_POINT ( 'NONE', #88766 ) ;
#108593 = CARTESIAN_POINT ( 'NONE',  ( 4.802243920988390258, 1508.551704408389924, 204.6921040114409891 ) ) ;
#108594 = VECTOR ( 'NONE', #84401, 1000.000000000000114 ) ;
#108595 = DIRECTION ( 'NONE',  ( 1.755985294532464991E-16, -1.000000000000000000, 1.338183447452830017E-16 ) ) ;
#108596 = CARTESIAN_POINT ( 'NONE',  ( -2.896892187767880156, 1484.263391075600111, 183.3160938869699805 ) ) ;
#108597 = CARTESIAN_POINT ( 'NONE',  ( -21.87294976469999952, 1415.845546353629970, 216.4166232744080105 ) ) ;
#108598 = VERTEX_POINT ( 'NONE', #94953 ) ;
#108599 = CARTESIAN_POINT ( 'NONE',  ( 46.01111071544060138, 1442.797791010789979, 266.6782117715599725 ) ) ;
#108600 = CARTESIAN_POINT ( 'NONE',  ( -4.333361549047180183, 1508.551704406479985, 204.4537186006569982 ) ) ;
#108601 = CARTESIAN_POINT ( 'NONE',  ( -6.992186432439999599, 1426.424829897749987, 202.7541583518589903 ) ) ;
#108602 = CARTESIAN_POINT ( 'NONE',  ( -3.266349512195000138, 1516.797038924770050, 205.0935381919470046 ) ) ;
#108603 = EDGE_LOOP ( 'NONE', ( #62589, #98464, #40770, #82487, #43049 ) ) ;
#108604 = CARTESIAN_POINT ( 'NONE',  ( -8.861482052969998691, 1384.950957082100103, 218.6848127019790127 ) ) ;
#108605 = CYLINDRICAL_SURFACE ( 'NONE', #61662, 2.500000000000001776 ) ;
#108606 = CARTESIAN_POINT ( 'NONE',  ( 13.47882082157883232, 1444.213219860304434, 187.9195826302412229 ) ) ;
#108607 = ORIENTED_EDGE ( 'NONE', *, *, #61935, .T. ) ;
#108608 = CARTESIAN_POINT ( 'NONE',  ( 4.832611339330939337, 1508.551704408389924, 206.6339237841029899 ) ) ;
#108609 = CARTESIAN_POINT ( 'NONE',  ( 26.83363330979009831, 1450.700274826909890, 136.4563300885299668 ) ) ;
#108610 = CARTESIAN_POINT ( 'NONE',  ( -13.64573741497510184, 1512.804203059160045, 193.8098271449230197 ) ) ;
#108611 = CARTESIAN_POINT ( 'NONE',  ( 6.454219559888790592, 1504.605177847159894, 220.1239436410009773 ) ) ;
#108612 = CARTESIAN_POINT ( 'NONE',  ( -1.681286490166120328E-05, 1409.206633381659913, 270.3713656704379673 ) ) ;
#108613 = CARTESIAN_POINT ( 'NONE',  ( 0.4691691604916909952, 1431.662181100700082, 218.6011377030980043 ) ) ;
#108614 = CARTESIAN_POINT ( 'NONE',  ( -8.829505046341829200, 1493.480017849250089, 200.5570910297369949 ) ) ;
#108615 = CARTESIAN_POINT ( 'NONE',  ( -4.677432903610000636, 1495.589319749489960, 198.5260162735989695 ) ) ;
#108616 = CARTESIAN_POINT ( 'NONE',  ( 4.124127541549999165, 1440.791920158089852, 218.1322488136489994 ) ) ;
#108618 = CARTESIAN_POINT ( 'NONE',  ( 29.35073940689247962, 1526.211523310372058, 220.5206201286387113 ) ) ;
#108617 = CARTESIAN_POINT ( 'NONE',  ( -13.13384863970290084, 1434.838379660660166, 149.0654039179239874 ) ) ;
#108619 = CIRCLE ( 'NONE', #37176, 7.868384924639995504 ) ;
#108620 = CARTESIAN_POINT ( 'NONE',  ( 10.82955669553860112, 1425.268927654319896, 206.5179382998420010 ) ) ;
#108621 = CARTESIAN_POINT ( 'NONE',  ( -13.08811969939999997, 1380.207675299450102, 214.5718119823889936 ) ) ;
#108622 = CARTESIAN_POINT ( 'NONE',  ( -7.645478605405000572, 1514.134513140259969, 203.0666490157069859 ) ) ;
#108623 = ORIENTED_EDGE ( 'NONE', *, *, #51793, .T. ) ;
#108624 = CARTESIAN_POINT ( 'NONE',  ( 17.83186622659999898, 1434.542072767689888, 214.3676144197979738 ) ) ;
#108625 = CARTESIAN_POINT ( 'NONE',  ( 0.000000000000000000, 0.000000000000000000, 137.0999999980979851 ) ) ;
#108626 = CIRCLE ( 'NONE', #38839, 2.000079913604663417 ) ;
#108627 = CARTESIAN_POINT ( 'NONE',  ( -103.9199421708199935, 1384.937015199220014, 311.1477413758909734 ) ) ;
#108628 = CARTESIAN_POINT ( 'NONE',  ( -7.954531997339999272, 1385.329339385649973, 199.4936033243889710 ) ) ;
#108629 = CARTESIAN_POINT ( 'NONE',  ( 7.114141310732409629, 1427.484008838899626, 137.0999999980979567 ) ) ;
#108631 = EDGE_LOOP ( 'NONE', ( #2871, #108144, #88406, #107882 ) ) ;
#108630 = CARTESIAN_POINT ( 'NONE',  ( 10.97092914054660007, 1423.389121826950031, 203.2629501824719966 ) ) ;
#108632 = CARTESIAN_POINT ( 'NONE',  ( 1.188910551360000012, 1429.998391900489878, 217.3728214398389866 ) ) ;
#108633 = CARTESIAN_POINT ( 'NONE',  ( -3.034707026709789979, 1440.440247136690004, 157.2489849372729793 ) ) ;
#108634 = CARTESIAN_POINT ( 'NONE',  ( -16.70830602919999919, 1417.149230822529944, 207.3570811876390110 ) ) ;
#108635 = CARTESIAN_POINT ( 'NONE',  ( 11.92075754520000075, 1433.502514733529779, 150.2427968400980092 ) ) ;
#108636 = CARTESIAN_POINT ( 'NONE',  ( 6.832964021560000489, 1472.413060387330006, 271.1218459616979999 ) ) ;
#108637 = DIRECTION ( 'NONE',  ( -1.755985294532469921E-16, 1.000000000000000000, -1.338183447452831989E-16 ) ) ;
#108638 = B_SPLINE_CURVE_WITH_KNOTS ( 'NONE', 5,
 ( #25273, #16860, #40992, #33138, #101424, #110404, #59474, #6832, #75171, #60026, #124, #109321 ),
 .UNSPECIFIED., .F., .F.,
 ( 6, 3, 3, 6 ),
 ( 0.000000000000000000, 0.2395393521504640966, 0.6197696760997779553, 1.000000000000000000 ),
 .UNSPECIFIED. ) ;
#108639 = CARTESIAN_POINT ( 'NONE',  ( -29.35747451427760168, 1526.382868173645875, 201.0438982057195290 ) ) ;
#108640 = CARTESIAN_POINT ( 'NONE',  ( 17.83486663330488042, 1523.678648413191695, 180.3677388338999776 ) ) ;
#108641 = DIRECTION ( 'NONE',  ( -1.755985294532469921E-16, 1.000000000000000000, -1.338183447452831989E-16 ) ) ;
#108642 = CARTESIAN_POINT ( 'NONE',  ( 16.93584435349999850, 1422.112459457830028, 226.8792436412979896 ) ) ;
#108643 = DIRECTION ( 'NONE',  ( -0.9455185755993177343, 0.000000000000000000, 0.3255681544571540909 ) ) ;
#108644 = CARTESIAN_POINT ( 'NONE',  ( 8.432239102140002274, 1391.913060387289988, 209.1218459572589836 ) ) ;
#108645 = CARTESIAN_POINT ( 'NONE',  ( -17.85795099530000130, 1410.033484215229919, 224.6176101541979904 ) ) ;
#108646 = AXIS2_PLACEMENT_3D ( 'NONE', #84681, #68467, #16356 ) ;
#108647 = CARTESIAN_POINT ( 'NONE',  ( 20.39632456690000240, 1508.015821253330159, 189.6607555625980126 ) ) ;
#108648 = CARTESIAN_POINT ( 'NONE',  ( -4.125529553939999872, 1479.921875556590066, 229.1190508355989834 ) ) ;
#108649 = DIRECTION ( 'NONE',  ( -0.000000000000000000, -1.000000000000000000, -0.000000000000000000 ) ) ;
#108650 = CARTESIAN_POINT ( 'NONE',  ( 1.081422847559999845, 1515.099766759590011, 204.7933130088590019 ) ) ;
#108651 = CARTESIAN_POINT ( 'NONE',  ( -2.372478608332517336, 1522.382868172863937, 174.8996806668726549 ) ) ;
#108652 = CARTESIAN_POINT ( 'NONE',  ( 4.677562527581470064, 1434.889072014880185, 228.7640133665269957 ) ) ;
#108653 = CARTESIAN_POINT ( 'NONE',  ( -11.61528297169999924, 1414.971352895729979, 221.0857775958980085 ) ) ;
#108654 = CARTESIAN_POINT ( 'NONE',  ( 0.1719439918013369872, 1479.188729932770229, 182.1292389662029905 ) ) ;
#108656 = ORIENTED_EDGE ( 'NONE', *, *, #45365, .T. ) ;
#108655 = CARTESIAN_POINT ( 'NONE',  ( 9.862951377130659836, 1521.951704408389787, 189.8497022437369708 ) ) ;
#108657 = CARTESIAN_POINT ( 'NONE',  ( -17.11714625305222981, 1444.740067931810927, 162.7561045841209193 ) ) ;
#108658 = CARTESIAN_POINT ( 'NONE',  ( -1.637258856660000150, 1483.893433971690001, 198.5669146070989939 ) ) ;
#108659 = CARTESIAN_POINT ( 'NONE',  ( 12.40405681299999863, 1434.420100264380153, 149.4777463942980091 ) ) ;
#108660 = CARTESIAN_POINT ( 'NONE',  ( -41.18215094384600405, 1440.963619929689912, 134.0999999980659823 ) ) ;
#108661 = CARTESIAN_POINT ( 'NONE',  ( 5.605776958220000772, 1441.571049125840091, 184.4074510981980097 ) ) ;
#108662 = ORIENTED_EDGE ( 'NONE', *, *, #32981, .F. ) ;
#108663 = CARTESIAN_POINT ( 'NONE',  ( -5.432410439472700858, 1391.426148861440197, 203.3415300314919989 ) ) ;
#108664 = CARTESIAN_POINT ( 'NONE',  ( 13.02322703161950024, 1416.825784015089994, 221.6328457863429833 ) ) ;
#108665 = CARTESIAN_POINT ( 'NONE',  ( -105.2424085362494139, 1381.071453570725225, 308.6724721103511229 ) ) ;
#108666 = CYLINDRICAL_SURFACE ( 'NONE', #78552, 2.000000000000003109 ) ;
#108667 = FACE_OUTER_BOUND ( 'NONE', #14794, .T. ) ;
#108668 = VECTOR ( 'NONE', #7304, 1000.000000000000114 ) ;
#108669 = CARTESIAN_POINT ( 'NONE',  ( -109.1311308840000009, 1384.934002237980167, 311.2646438852589768 ) ) ;
#108670 = CARTESIAN_POINT ( 'NONE',  ( -22.52609270479999992, 1509.699688878229836, 208.9176257130850161 ) ) ;
#108671 = CARTESIAN_POINT ( 'NONE',  ( -12.30621109530000012, 1378.371660281350159, 209.8675522742090038 ) ) ;
#108672 = CARTESIAN_POINT ( 'NONE',  ( 2.988808142889999520, 1436.945273251980097, 184.3538548285980028 ) ) ;
#108673 = CARTESIAN_POINT ( 'NONE',  ( -66.81779111251940151, 1385.096065578679827, 259.0793199826619571 ) ) ;
#108674 = CARTESIAN_POINT ( 'NONE',  ( -19.39983987835377732, 1522.382868172864164, 239.2921289694226061 ) ) ;
#108675 = CARTESIAN_POINT ( 'NONE',  ( -4.363624498282149489, 1508.551704408389924, 204.9809794401540159 ) ) ;
#108676 = ORIENTED_EDGE ( 'NONE', *, *, #48711, .F. ) ;
#108677 = CARTESIAN_POINT ( 'NONE',  ( -29.03159036203449972, 1509.651961618060113, 208.6837609952029879 ) ) ;
#108678 = CARTESIAN_POINT ( 'NONE',  ( -16.03542055943749745, 1410.434532276399977, 226.6320020206029824 ) ) ;
#108679 = EDGE_CURVE ( 'NONE', #59011, #86431, #14368, .T. ) ;
#108681 = ORIENTED_EDGE ( 'NONE', *, *, #39442, .T. ) ;
#108680 = CARTESIAN_POINT ( 'NONE',  ( -21.83863730835998140, 1523.580203803270933, 234.9763103460708180 ) ) ;
#108682 = CARTESIAN_POINT ( 'NONE',  ( 2.720194589200000124, 1473.666501463190116, 219.1326999374989839 ) ) ;
#108683 = CARTESIAN_POINT ( 'NONE',  ( 9.936615814174009742, 1469.595287704849852, 210.7004918180149957 ) ) ;
#108684 = CARTESIAN_POINT ( 'NONE',  ( -7.717505791104999346, 1516.857914730730045, 216.8393517232070167 ) ) ;
#108685 = CARTESIAN_POINT ( 'NONE',  ( -109.4663766940000045, 1384.534820742290094, 311.2654509672589711 ) ) ;
#108686 = CARTESIAN_POINT ( 'NONE',  ( 1.963370033230000145, 1464.924280339329925, 237.5709149063980021 ) ) ;
#108687 = ADVANCED_FACE ( 'NONE', ( #18223 ), #44777, .T. ) ;
#108688 = CARTESIAN_POINT ( 'NONE',  ( 22.39508854780000036, 1411.055311095129809, 215.1301064521879880 ) ) ;
#108689 = CARTESIAN_POINT ( 'NONE',  ( -2.419942311379319921, 1417.229693625109803, 186.1923575038539980 ) ) ;
#108690 = CARTESIAN_POINT ( 'NONE',  ( -17.74698610909999985, 1424.418662807230021, 227.3573823931980087 ) ) ;
#108691 = CARTESIAN_POINT ( 'NONE',  ( -3.858625071233336978, 1511.506728505285992, 200.9714742573962951 ) ) ;
#108692 = DIRECTION ( 'NONE',  ( 0.000000000000000000, -1.000000000000000000, -0.000000000000000000 ) ) ;
#108693 = CARTESIAN_POINT ( 'NONE',  ( -104.0812585028400008, 1311.832804576489934, 304.2218459572590064 ) ) ;
#108694 = CARTESIAN_POINT ( 'NONE',  ( -3.005276066430000448, 1369.205039411269809, 207.6218459616989946 ) ) ;
#108695 = B_SPLINE_CURVE_WITH_KNOTS ( 'NONE', 3,
 ( #42025, #34166, #16778, #76722, #76173, #68352, #102458 ),
 .UNSPECIFIED., .F., .F.,
 ( 4, 3, 4 ),
 ( -157.7301682610000171, -100.4763595781870009, -30.40177460629999473 ),
 .UNSPECIFIED. ) ;
#108696 = CIRCLE ( 'NONE', #26437, 1.000000000000000888 ) ;
#108697 = CARTESIAN_POINT ( 'NONE',  ( 5.604365146380000162, 1361.139420828400034, 210.6218459616991936 ) ) ;
#108698 = CARTESIAN_POINT ( 'NONE',  ( 6.935133380425000382, 1516.613881697390070, 205.8602099992770036 ) ) ;
#108699 = CARTESIAN_POINT ( 'NONE',  ( -4.461987601309290064, 1485.816428176619866, 182.7387781610549951 ) ) ;
#108700 = VERTEX_POINT ( 'NONE', #54635 ) ;
#108701 = CARTESIAN_POINT ( 'NONE',  ( 3.127269064749419236, 1466.004634090720629, 199.2798694621438926 ) ) ;
#108702 = FACE_OUTER_BOUND ( 'NONE', #42468, .T. ) ;
#108704 = ORIENTED_EDGE ( 'NONE', *, *, #3633, .F. ) ;
#108703 = CARTESIAN_POINT ( 'NONE',  ( -68.46221940491409441, 1379.747295280180197, 280.0472515979760146 ) ) ;
#108705 = ORIENTED_EDGE ( 'NONE', *, *, #76033, .F. ) ;
#108706 = CARTESIAN_POINT ( 'NONE',  ( -9.029782795278201490, 1380.828793225110530, 217.6116281277577684 ) ) ;
#108707 = ORIENTED_EDGE ( 'NONE', *, *, #88133, .F. ) ;
#108708 = MECHANICAL_DESIGN_GEOMETRIC_PRESENTATION_REPRESENTATION (  '', ( #28228 ), #12158 ) ;
#108709 = CARTESIAN_POINT ( 'NONE',  ( -1.427070966906029970, 1486.249699017309922, 220.9490979875029950 ) ) ;
#108710 = CARTESIAN_POINT ( 'NONE',  ( 11.57530258789999955, 1501.342160219190191, 208.5271145533289996 ) ) ;
#108712 = CARTESIAN_POINT ( 'NONE',  ( 15.82718059914979847, 1409.568640700319975, 192.3709770614890147 ) ) ;
#108711 = CARTESIAN_POINT ( 'NONE',  ( -11.15639751152448511, 1425.159686727654162, 144.2660521923811530 ) ) ;
#108713 = CARTESIAN_POINT ( 'NONE',  ( -5.775625115495000017, 1516.745833913490060, 209.8771724060850090 ) ) ;
#108714 = CARTESIAN_POINT ( 'NONE',  ( 41.62259533861070082, 1442.636044721269855, 135.5651380244540007 ) ) ;
#108715 = CARTESIAN_POINT ( 'NONE',  ( -108.0661742336610018, 1378.913060387289988, 308.5496305239910271 ) ) ;
#108716 = CARTESIAN_POINT ( 'NONE',  ( -3.310397198750480108, 1509.102546110879985, 179.4781337253649838 ) ) ;
#108717 = CARTESIAN_POINT ( 'NONE',  ( 12.63405317313929821, 1500.911264070530024, 210.5278134812520250 ) ) ;
#108718 = APPLICATION_PROTOCOL_DEFINITION ( 'draft international standard', 'automotive_design', 1998, #22664 ) ;
#108719 = CARTESIAN_POINT ( 'NONE',  ( 37.29624469549910515, 1450.849357696539982, 134.0999999986649698 ) ) ;
#108720 =( BOUNDED_CURVE ( )  B_SPLINE_CURVE ( 3, ( #84357, #101687, #24978, #17675 ),
 .UNSPECIFIED., .F., .T. ) 
 B_SPLINE_CURVE_WITH_KNOTS ( ( 4, 4 ),
 ( 1.021750339367931915, 2.119842335967295099 ),
 .UNSPECIFIED. ) 
 CURVE ( )  GEOMETRIC_REPRESENTATION_ITEM ( )  RATIONAL_B_SPLINE_CURVE ( ( 1.000000000000000000, 0.9020151856930300749, 0.9020151856930300749, 1.000000000000000000 ) ) 
 REPRESENTATION_ITEM ( '' )  );
#108721 = DIRECTION ( 'NONE',  ( -0.9993902469235412811, 0.03489947644508400310, 0.001077449749359510062 ) ) ;
#108722 = ORIENTED_EDGE ( 'NONE', *, *, #90209, .F. ) ;
#108723 = CARTESIAN_POINT ( 'NONE',  ( -21.46486174369999844, 1504.440211354589792, 215.6677629392290214 ) ) ;
#108724 = CARTESIAN_POINT ( 'NONE',  ( -18.48828930349999666, 1458.367965555730052, 227.6410138353980130 ) ) ;
#108725 = ORIENTED_EDGE ( 'NONE', *, *, #95558, .T. ) ;
#108726 = VERTEX_POINT ( 'NONE', #53524 ) ;
#108727 = CARTESIAN_POINT ( 'NONE',  ( -0.1267786306729990209, 1432.696254167089819, 203.3330887969689798 ) ) ;
#108728 = CARTESIAN_POINT ( 'NONE',  ( 10.34090598038000053, 1453.264473920479759, 211.4883971156640143 ) ) ;
#108729 = CARTESIAN_POINT ( 'NONE',  ( 12.58710147329349915, 1500.144068373949949, 207.5432606781910181 ) ) ;
#108730 = CIRCLE ( 'NONE', #15734, 2.000000000000000000 ) ;
#108731 = CARTESIAN_POINT ( 'NONE',  ( -2.330134125103331844, 1515.320037165259464, 213.3925622817942553 ) ) ;
#108732 = CARTESIAN_POINT ( 'NONE',  ( -2.500000000000039968, 1439.311176619419939, 160.3626367463150189 ) ) ;
#108733 = CARTESIAN_POINT ( 'NONE',  ( -5.013435694540000043, 1375.426148861440197, 203.5256706139790310 ) ) ;
#108734 = CARTESIAN_POINT ( 'NONE',  ( -13.86144133729999872, 1379.734592797399955, 208.2043628488259799 ) ) ;
#108735 = CARTESIAN_POINT ( 'NONE',  ( 38.81202644819820335, 1436.797832379770171, 134.4205481884810069 ) ) ;
#108736 = CARTESIAN_POINT ( 'NONE',  ( 2.070960726044260181, 1421.152689218060004, 183.1770975898769791 ) ) ;
#108737 = CARTESIAN_POINT ( 'NONE',  ( 29.85692059557557343, 1525.159177407156221, 222.1259724534683073 ) ) ;
#108738 = FACE_OUTER_BOUND ( 'NONE', #92170, .T. ) ;
#108739 = CARTESIAN_POINT ( 'NONE',  ( -83.31223204895070467, 1384.810193783940122, 287.0493513657310132 ) ) ;
#108740 = EDGE_LOOP ( 'NONE', ( #20174, #88347, #52652, #93798 ) ) ;
#108741 = CARTESIAN_POINT ( 'NONE',  ( 6.941727252324999320, 1516.882217593000178, 201.7906628411569727 ) ) ;
#108742 = CARTESIAN_POINT ( 'NONE',  ( -1.715109485185000171, 1516.963431999339946, 208.3866188148990091 ) ) ;
#108743 = ORIENTED_EDGE ( 'NONE', *, *, #95662, .F. ) ;
#108744 = CARTESIAN_POINT ( 'NONE',  ( 37.64188185173559731, 1440.913060387330006, 264.5003480932859929 ) ) ;
#108745 = CARTESIAN_POINT ( 'NONE',  ( -0.0001997011801151793269, 1452.268962891940419, 153.8032004743181176 ) ) ;
#108746 = VERTEX_POINT ( 'NONE', #18771 ) ;
#108747 = CARTESIAN_POINT ( 'NONE',  ( -2.664535259099999805E-15, 1424.786834349990158, 209.1218459616989946 ) ) ;
#108748 = CARTESIAN_POINT ( 'NONE',  ( -15.26118644339999975, 1409.612623021030004, 191.5370205933980117 ) ) ;
#108749 = CARTESIAN_POINT ( 'NONE',  ( 21.10560967990464576, 1525.661276915132476, 233.3100090447210562 ) ) ;
#108750 = CARTESIAN_POINT ( 'NONE',  ( -9.841064997534830994, 1462.508760387780057, 206.4810345683729906 ) ) ;
#108751 = CARTESIAN_POINT ( 'NONE',  ( 21.79577993357450083, 1409.838234761750073, 206.3155456279520195 ) ) ;
#108752 = CARTESIAN_POINT ( 'NONE',  ( -6.013128445097610353, 1510.874996213040049, 201.6036617501539752 ) ) ;
#108753 = CARTESIAN_POINT ( 'NONE',  ( -2.561957929796738309, 1389.413060387289988, 210.6827340313378443 ) ) ;
#108754 = CARTESIAN_POINT ( 'NONE',  ( -12.91347167789999872, 1434.774310044260119, 146.4344527888979997 ) ) ;
#108755 = CARTESIAN_POINT ( 'NONE',  ( 26.67729797004249903, 1503.852178143910123, 206.2304859205609944 ) ) ;
#108757 = PLANE ( 'NONE',  #54522 ) ;
#108756 = CARTESIAN_POINT ( 'NONE',  ( 15.04941445769999930, 1461.565441850729940, 229.9667256941980042 ) ) ;
#108758 = CARTESIAN_POINT ( 'NONE',  ( -4.424915418274963486, 1421.993387322426543, 184.5440085787073770 ) ) ;
#108759 = AXIS2_PLACEMENT_3D ( 'NONE', #78819, #2133, #96165 ) ;
#108760 = CARTESIAN_POINT ( 'NONE',  ( 6.942344691835000248, 1516.810037859429940, 216.8380980232070101 ) ) ;
#108761 = VERTEX_POINT ( 'NONE', #12049 ) ;
#108762 = CARTESIAN_POINT ( 'NONE',  ( -1.004950505856348597, 1486.301326980616750, 181.7814475905654206 ) ) ;
#108763 = CARTESIAN_POINT ( 'NONE',  ( -0.04975610472413720398, 1508.745098571959943, 179.9291894445549929 ) ) ;
#108764 = CARTESIAN_POINT ( 'NONE',  ( -21.95754362317823549, 1524.412928176730020, 233.6990317443709273 ) ) ;
#108765 = CARTESIAN_POINT ( 'NONE',  ( -1.703779643355000095, 1517.057265928030120, 213.1670284501570052 ) ) ;
#108766 = CARTESIAN_POINT ( 'NONE',  ( 18.54307487750000050, 1508.238692192329836, 188.5097067394980002 ) ) ;
#108767 = CARTESIAN_POINT ( 'NONE',  ( -0.3530891408735000181, 1467.116854267079816, 235.6078141451939985 ) ) ;
#108769 = ORIENTED_EDGE ( 'NONE', *, *, #105576, .T. ) ;
#108768 = CARTESIAN_POINT ( 'NONE',  ( 3.861651023821930373, 1508.610718263850003, 213.8016401658969983 ) ) ;
#108770 = CARTESIAN_POINT ( 'NONE',  ( -1.590879946460538319, 1526.333389948038530, 178.3980910637346255 ) ) ;
#108771 = CARTESIAN_POINT ( 'NONE',  ( 2.876567151200000172, 1508.185761598690078, 220.3556610966990092 ) ) ;
#108772 = CARTESIAN_POINT ( 'NONE',  ( -11.76832574670000042, 1432.246854381219919, 150.8115016154980026 ) ) ;
#108773 = CARTESIAN_POINT ( 'NONE',  ( -2.026117440780000223, 1436.275455653890049, 227.5319773123989933 ) ) ;
#108774 = CARTESIAN_POINT ( 'NONE',  ( -109.9698195215979979, 1384.452562162210143, 311.4357956501490321 ) ) ;
#108775 = CARTESIAN_POINT ( 'NONE',  ( 6.446325746348199104, 1432.345391573609959, 154.6647259147359819 ) ) ;
#108776 = CARTESIAN_POINT ( 'NONE',  ( 20.02479433700000300, 1424.420966076929972, 224.6196048453980154 ) ) ;
#108777 = VECTOR ( 'NONE', #34001, 1000.000000000000227 ) ;
#108778 = CARTESIAN_POINT ( 'NONE',  ( -4.285402615378519187, 1475.851751799939848, 215.4336415230879993 ) ) ;
#108779 = B_SPLINE_CURVE_WITH_KNOTS ( 'NONE', 3,
 ( #73943, #65552, #55498, #82876, #89625, #106978, #40323, #31921, #30266, #21841, #23517, #66114, #12913, #91826, #49295, #47093, #56038, #555, #92929, #51490, #7819 ),
 .UNSPECIFIED., .F., .F.,
 ( 4, 2, 2, 2, 1, 1, 1, 1, 1, 2, 2, 2, 4 ),
 ( 0.000000000000000000, 0.2499999999978126386, 0.3749999999967190689, 0.4374999999961580177, 0.4687499999958776309, 0.4843749999957374097, 0.4921874999956772911, 0.4960937499956372121, 0.4980468749956170060, 0.4990234374956199481, 0.4999999999956228902, 0.7499999999978114174, 1.000000000000000000 ),
 .UNSPECIFIED. ) ;
#108781 = CARTESIAN_POINT ( 'NONE',  ( -4.332041340678299157, 1420.009902215498869, 137.0999999980978430 ) ) ;
#108780 = CARTESIAN_POINT ( 'NONE',  ( -19.78242928659999933, 1495.375247112429861, 228.5198483940980054 ) ) ;
#108782 = CARTESIAN_POINT ( 'NONE',  ( -2.105918939980000015, 1485.584836081030062, 182.5101142617980088 ) ) ;
#108783 = ORIENTED_EDGE ( 'NONE', *, *, #79618, .F. ) ;
#108785 = VECTOR ( 'NONE', #106485, 999.9999999999998863 ) ;
#108784 = CARTESIAN_POINT ( 'NONE',  ( -5.786837717054999608, 1517.040132827679827, 205.8646253294070050 ) ) ;
#108786 = CARTESIAN_POINT ( 'NONE',  ( 14.63616075459999877, 1407.516636404930068, 267.4468191936979906 ) ) ;
#108787 = CARTESIAN_POINT ( 'NONE',  ( 0.3096082303459999907, 1409.092176632029805, 185.5936471484980075 ) ) ;
#108788 = AXIS2_PLACEMENT_3D ( 'NONE', #108098, #91852, #48777 ) ;
#108789 = CYLINDRICAL_SURFACE ( 'NONE', #40710, 0.5000000000000031086 ) ;
#108790 = AXIS2_PLACEMENT_3D ( 'NONE', #79179, #104915, #36064 ) ;
#108791 = CARTESIAN_POINT ( 'NONE',  ( 22.17856219145011210, 1430.336759468506671, 217.7288953034882013 ) ) ;
#108792 = CARTESIAN_POINT ( 'NONE',  ( -8.723519235820038631, 1388.537837264801283, 217.9447364732859853 ) ) ;
#108793 = CARTESIAN_POINT ( 'NONE',  ( -12.78776258889159934, 1416.851343895820037, 195.9645815067300134 ) ) ;
#108794 = AXIS2_PLACEMENT_3D ( 'NONE', #1047, #69355, #60959 ) ;
#108795 = CARTESIAN_POINT ( 'NONE',  ( 0.000000000000000000, 1395.913060387330006, 215.6218459616979999 ) ) ;
#108796 = CARTESIAN_POINT ( 'NONE',  ( -3.179033943583710276, 1457.997354099609993, 219.3203918230290128 ) ) ;
#108797 = CARTESIAN_POINT ( 'NONE',  ( -1.640778594498735421, 1450.655424612788693, 183.1975428507971628 ) ) ;
#108798 = CARTESIAN_POINT ( 'NONE',  ( 0.5697989931917299966, 1450.893162568030220, 155.3351411520599754 ) ) ;
#108799 = CARTESIAN_POINT ( 'NONE',  ( -14.30888197749849944, 1416.029511585999899, 221.2389454739920041 ) ) ;
#108800 = CARTESIAN_POINT ( 'NONE',  ( -4.287908595200000228, 1515.369371658090131, 209.8551202939650011 ) ) ;
#108801 = CARTESIAN_POINT ( 'NONE',  ( -5.481756276210000500, 1437.661022548789788, 208.5938030632829907 ) ) ;
#108802 = CARTESIAN_POINT ( 'NONE',  ( -27.28973479252249845, 1507.987442490729791, 210.9867140273689756 ) ) ;
#108803 = CARTESIAN_POINT ( 'NONE',  ( 2.705683380580000019, 1440.723906225590099, 165.1197260195979766 ) ) ;
#108804 = CARTESIAN_POINT ( 'NONE',  ( -4.983379166339999777, 1475.784981106930218, 267.2248697199979688 ) ) ;
#108806 = AXIS2_PLACEMENT_3D ( 'NONE', #25489, #104427, #45102 ) ;
#108805 = CARTESIAN_POINT ( 'NONE',  ( -11.64998282343909253, 1425.712254131211921, 138.1866827809310792 ) ) ;
#108807 = CARTESIAN_POINT ( 'NONE',  ( -15.00581081485931279, 1514.742480524781740, 193.0300471132391351 ) ) ;
#108808 = LINE ( 'NONE', #83056, #103923 ) ;
#108809 = CARTESIAN_POINT ( 'NONE',  ( -51.28913027418060011, 1384.733897297830026, 264.3868833375080385 ) ) ;
#108810 = CARTESIAN_POINT ( 'NONE',  ( -107.3690818753550076, 1391.913060387289988, 300.9869897165519887 ) ) ;
#108811 = CARTESIAN_POINT ( 'NONE',  ( 12.25713978260370141, 1416.640375556570007, 223.5670658059360107 ) ) ;
#108812 = DIRECTION ( 'NONE',  ( -0.4794255386042076128, 0.000000000000000000, 0.8775825618903700942 ) ) ;
#108813 = CARTESIAN_POINT ( 'NONE',  ( 31.92312126443668419, 1524.775785348138015, 216.6640869107574758 ) ) ;
#108814 = CARTESIAN_POINT ( 'NONE',  ( 24.27343987535987679, 1509.087591976627664, 195.8036345857676963 ) ) ;
#108815 = CARTESIAN_POINT ( 'NONE',  ( 3.687149994097108433E-15, 1511.187213306747708, 239.2297105040643714 ) ) ;
#108816 = CARTESIAN_POINT ( 'NONE',  ( -15.64852212096800166, 1421.346706121272064, 227.1284945715040067 ) ) ;
#108817 = CARTESIAN_POINT ( 'NONE',  ( 10.84130981773069990, 1478.843033899609964, 205.9626931864170274 ) ) ;
#108818 = ORIENTED_EDGE ( 'NONE', *, *, #59893, .F. ) ;
#108819 = ADVANCED_FACE ( 'NONE', ( #69782 ), #61594, .T. ) ;
#108820 = CARTESIAN_POINT ( 'NONE',  ( -6.373555541172550853, 1410.509728914295238, 231.3423281520361172 ) ) ;
#108821 = CARTESIAN_POINT ( 'NONE',  ( -13.59157698562750127, 1508.214338131689829, 209.5916190095410059 ) ) ;
#108822 = CARTESIAN_POINT ( 'NONE',  ( 18.38166056955379801, 1428.164368491259893, 201.4944003554669791 ) ) ;
#108824 = CARTESIAN_POINT ( 'NONE',  ( -12.45150583203999872, 1379.026621145309946, 211.0139914652599771 ) ) ;
#108823 = CARTESIAN_POINT ( 'NONE',  ( -16.03814159374950066, 1416.346020389309842, 209.5174529804690167 ) ) ;
#108825 = CARTESIAN_POINT ( 'NONE',  ( 17.10337015680181239, 1524.478200376951690, 237.2711292833226366 ) ) ;
#108826 = DIRECTION ( 'NONE',  ( -1.224646799147353947E-16, 1.836970198721029688E-16, 1.000000000000000000 ) ) ;
#108827 = CARTESIAN_POINT ( 'NONE',  ( -29.66215386746315374, 1526.345556099435726, 201.2527107338347321 ) ) ;
#108828 = CARTESIAN_POINT ( 'NONE',  ( -7.330554171554999776, 1516.857992118400034, 201.7925428541169879 ) ) ;
#108829 = CARTESIAN_POINT ( 'NONE',  ( -4.848919996459999382, 1489.192135936889827, 188.8958457811990002 ) ) ;
#108830 = CARTESIAN_POINT ( 'NONE',  ( -11.57397602220189725, 1398.256226300480648, 203.1998198725468114 ) ) ;
#108831 = CARTESIAN_POINT ( 'NONE',  ( 15.24995204913500046, 1513.868118914750085, 194.1593619713669909 ) ) ;
#108832 = FACE_BOUND ( 'NONE', #81603, .T. ) ;
#108833 = CARTESIAN_POINT ( 'NONE',  ( -11.40323313910470127, 1380.342188320790001, 209.3118107140630002 ) ) ;
#108834 = CARTESIAN_POINT ( 'NONE',  ( 20.59269091049739941, 1507.766057095049973, 227.7908381428599967 ) ) ;
#108836 = ORIENTED_EDGE ( 'NONE', *, *, #15071, .F. ) ;
#108835 = CARTESIAN_POINT ( 'NONE',  ( -54.27049659481630073, 1379.703136558600136, 254.1616898847049981 ) ) ;
#108837 = ORIENTED_EDGE ( 'NONE', *, *, #28233, .T. ) ;
#108838 = CARTESIAN_POINT ( 'NONE',  ( 11.67990115640299997, 1434.088071600169769, 151.1483243173979929 ) ) ;
#108839 = CARTESIAN_POINT ( 'NONE',  ( -9.361745962389999676, 1396.239979760129927, 215.6895990424980027 ) ) ;
#108840 = CARTESIAN_POINT ( 'NONE',  ( -22.51990863569999846, 1410.619212186330060, 212.0399858907879889 ) ) ;
#108841 = ORIENTED_EDGE ( 'NONE', *, *, #96638, .F. ) ;
#108842 = CARTESIAN_POINT ( 'NONE',  ( -13.16099798814397204, 1444.747053629154379, 169.3968106364190191 ) ) ;
#108843 = CARTESIAN_POINT ( 'NONE',  ( 20.59987592950000135, 1509.677367935830262, 230.5839143914980127 ) ) ;
#108844 = CARTESIAN_POINT ( 'NONE',  ( -10.10004869884733125, 1422.222932908416851, 137.0999999980979851 ) ) ;
#108846 = CARTESIAN_POINT ( 'NONE',  ( 17.85789328519999941, 1419.045775438330111, 225.4480613795979878 ) ) ;
#108845 = CARTESIAN_POINT ( 'NONE',  ( 0.7786077578810010058, 1443.353418816490148, 200.2227257021989715 ) ) ;
#108847 = CARTESIAN_POINT ( 'NONE',  ( 11.47832759589999974, 1468.696517459929964, 186.4345343207980079 ) ) ;
#108848 = CARTESIAN_POINT ( 'NONE',  ( -7.561650701720000534, 1415.425582719929707, 193.0231593168980169 ) ) ;
#108849 = DIRECTION ( 'NONE',  ( 0.000000000000000000, 0.000000000000000000, 1.000000000000000000 ) ) ;
#108850 =( NAMED_UNIT ( * ) SI_UNIT ( $, .STERADIAN. ) SOLID_ANGLE_UNIT ( ) );
#108851 = B_SPLINE_SURFACE_WITH_KNOTS ( 'NONE', 5, 5, ( 
 ( #84451, #7737, #17203, #60367, #41898, #84982 ),
 ( #67672, #17760, #25070, #43561, #51964, #86105 ),
 ( #32398, #76600, #59273, #8278, #42442, #54739 ),
 ( #78818, #11613, #2132, #63158, #95611, #28413 ),
 ( #53639, #26744, #27858, #19999, #96726, #60933 ),
 ( #18877, #45789, #69331, #105687, #79372, #88868 ),
 ( #79924, #36256, #3238, #103438, #20535, #70444 ),
 ( #104564, #86651, #52520, #35699, #95062, #18329 ),
 ( #9947, #44119, #28968, #35147, #78254, #54191 ) ),
 .UNSPECIFIED., .F., .F., .F.,
 ( 6, 3, 6 ),
 ( 6, 6 ),
 ( 17.98520084990000001, 40.17980702489999345, 62.49762447089999995 ),
 ( 0.000000000000000000, 1.595529479780000148 ),
 .UNSPECIFIED. ) ;
#108852 = CARTESIAN_POINT ( 'NONE',  ( 8.782767202921888838, 1396.219761434090060, 202.4073701858239929 ) ) ;
#108853 = CARTESIAN_POINT ( 'NONE',  ( 1.441539353570000070, 1414.983773854429955, 191.7394860450980048 ) ) ;
#108854 = CARTESIAN_POINT ( 'NONE',  ( 11.72512635530000047, 1429.059158185030128, 149.9312760468980059 ) ) ;
#108855 = CARTESIAN_POINT ( 'NONE',  ( 8.640072888135000184, 1511.773927532309926, 202.9615657546970056 ) ) ;
#108856 = VERTEX_POINT ( 'NONE', #37809 ) ;
#108857 = CARTESIAN_POINT ( 'NONE',  ( 13.12713025425550128, 1434.844877208209937, 149.2796170260219810 ) ) ;
#108858 = ORIENTED_EDGE ( 'NONE', *, *, #53463, .F. ) ;
#108859 = VERTEX_POINT ( 'NONE', #71997 ) ;
#108860 = EDGE_CURVE ( 'NONE', #13119, #13894, #55570, .T. ) ;
#108861 = CARTESIAN_POINT ( 'NONE',  ( -4.924195455119999565, 1424.762629879490078, 209.7208662265510100 ) ) ;
#108862 = CARTESIAN_POINT ( 'NONE',  ( -9.200915198040000575, 1463.128421874929927, 234.0379130468980122 ) ) ;
#108863 = CIRCLE ( 'NONE', #98147, 1.999999999999999556 ) ;
#108864 = CARTESIAN_POINT ( 'NONE',  ( -109.4829888131453259, 1386.904664127187289, 311.1374333086192223 ) ) ;
#108865 = CARTESIAN_POINT ( 'NONE',  ( -4.033653302454999867, 1517.028034847769959, 215.6825881955670070 ) ) ;
#108866 = CARTESIAN_POINT ( 'NONE',  ( -13.12422835985349856, 1380.070863199510086, 209.3681815004020166 ) ) ;
#108867 = AXIS2_PLACEMENT_3D ( 'NONE', #10675, #2299, #28010 ) ;
#108868 = B_SPLINE_CURVE_WITH_KNOTS ( 'NONE', 3,
 ( #22838, #100122, #91169, #47527, #31262, #57596, #40767, #55933, #14447, #64894, #13891, #66002, #40216, #108522, #83319, #74945, #81648, #13335, #91718, #5515, #38552, #14992, #29602, #99001, #39670, #97903, #89514, #4426, #4953, #39096, #73273, #30708, #22278, #73838 ),
 .UNSPECIFIED., .F., .F.,
 ( 4, 3, 3, 3, 3, 3, 3, 3, 3, 3, 3, 4 ),
 ( -2.000000000000000000, -1.856589768169299992, -1.673906318599919896, -1.488963774399080009, -1.302849350329150058, -1.115290844420000038, -0.9273284311027238935, -0.7394249586046770517, -0.5520371894422699821, -0.3663516837637139645, -0.1822529853692169688, 0.000000000000000000 ),
 .UNSPECIFIED. ) ;
#108869 = ORIENTED_EDGE ( 'NONE', *, *, #60710, .T. ) ;
#108870 = CARTESIAN_POINT ( 'NONE',  ( -12.86990655680000017, 1502.949917638090028, 208.7255105242149682 ) ) ;
#108871 = DIRECTION ( 'NONE',  ( 1.755985294532469921E-16, -1.000000000000000000, 1.338183447452831989E-16 ) ) ;
#108872 = CARTESIAN_POINT ( 'NONE',  ( -29.19545364349999872, 1380.228231664269970, 214.3784411298690031 ) ) ;
#108873 = VECTOR ( 'NONE', #70523, 1000.000000000000000 ) ;
#108874 = ORIENTED_EDGE ( 'NONE', *, *, #36650, .F. ) ;
#108875 = CARTESIAN_POINT ( 'NONE',  ( 1.119439089684999944, 1517.026534522949987, 205.8528207963470038 ) ) ;
#108876 = ORIENTED_EDGE ( 'NONE', *, *, #75568, .F. ) ;
#108877 = CARTESIAN_POINT ( 'NONE',  ( 1.709766494024999917, 1516.959716008189844, 209.1091877442879934 ) ) ;
#108878 = CARTESIAN_POINT ( 'NONE',  ( -20.52130963250000306, 1509.391296577229923, 229.7160214944979941 ) ) ;
#108879 = CARTESIAN_POINT ( 'NONE',  ( -38.93016163265561147, 1429.415421242818866, 269.5917615160539640 ) ) ;
#108880 = CARTESIAN_POINT ( 'NONE',  ( -1.169015704899999841, 1409.121795253429809, 232.4446791288980023 ) ) ;
#108882 = VERTEX_POINT ( 'NONE', #54090 ) ;
#108881 = CARTESIAN_POINT ( 'NONE',  ( -1.377258800830409857, 1414.913060387399810, 225.7566283813699783 ) ) ;
#108883 = CARTESIAN_POINT ( 'NONE',  ( 5.513435558014999849, 1509.038615934239942, 216.6345961781970288 ) ) ;
#108884 = CARTESIAN_POINT ( 'NONE',  ( -30.79536835113719917, 1440.913060387759970, 240.7855773362489913 ) ) ;
#108885 = CARTESIAN_POINT ( 'NONE',  ( -36.11164246829999769, 1384.804902789069956, 235.4725595070590032 ) ) ;
#108886 = CARTESIAN_POINT ( 'NONE',  ( -0.6774407473332200169, 1465.095561399730059, 238.0673353718009935 ) ) ;
#108887 = CIRCLE ( 'NONE', #12320, 1.000000000000000000 ) ;
#108888 = CARTESIAN_POINT ( 'NONE',  ( 10.80862676779999987, 1409.502744133030092, 270.4164080866979702 ) ) ;
#108889 = CARTESIAN_POINT ( 'NONE',  ( 2.490245914424999985, 1516.691389976299888, 213.7302634767470124 ) ) ;
#108890 = CARTESIAN_POINT ( 'NONE',  ( 24.13936747690000217, 1411.115472691630202, 209.3334965061050070 ) ) ;
#108891 = CARTESIAN_POINT ( 'NONE',  ( -21.24031773869999995, 1509.721128092229947, 188.1621763370980034 ) ) ;
#108892 = CARTESIAN_POINT ( 'NONE',  ( 12.22337018873460046, 1492.513505122720062, 210.8907448166860092 ) ) ;
#108894 = EDGE_CURVE ( 'NONE', #47496, #80799, #45684, .T. ) ;
#108893 = CARTESIAN_POINT ( 'NONE',  ( 7.444963622127359848, 1508.731180391300086, 214.6350537489069836 ) ) ;
#108895 = CARTESIAN_POINT ( 'NONE',  ( 3.269984781304999810, 1516.999105586269934, 210.8242519552970009 ) ) ;
#108896 = EDGE_CURVE ( 'NONE', #33631, #6602, #50217, .T. ) ;
#108897 = CARTESIAN_POINT ( 'NONE',  ( -3.812352470338788546, 1447.062376414930668, 154.8462586213417751 ) ) ;
#108898 = CARTESIAN_POINT ( 'NONE',  ( 0.2538825943349999892, 1420.503732742429975, 182.7635796100980201 ) ) ;
#108899 = CARTESIAN_POINT ( 'NONE',  ( -14.78542619307623873, 1486.064264431397760, 186.1959007592220701 ) ) ;
#108900 = EDGE_CURVE ( 'NONE', #105726, #59860, #76315, .T. ) ;
#108902 = ORIENTED_EDGE ( 'NONE', *, *, #46642, .F. ) ;
#108901 = CARTESIAN_POINT ( 'NONE',  ( -50.81938515019999869, 1390.824046508720130, 243.7260639249589929 ) ) ;
#108903 = CARTESIAN_POINT ( 'NONE',  ( -49.76867394811179679, 1385.123425707419756, 261.2502804024239822 ) ) ;
#108904 = CARTESIAN_POINT ( 'NONE',  ( 30.10642679900000118, 1468.180645040329864, 266.8105454816980000 ) ) ;
#108905 = ADVANCED_FACE ( 'NONE', ( #99337 ), #89508, .T. ) ;
#108906 = DIRECTION ( 'NONE',  ( 0.000000000000000000, 1.000000000000000000, 0.000000000000000000 ) ) ;
#108907 = EDGE_CURVE ( 'NONE', #31410, #104032, #68411, .T. ) ;
#108908 = DIRECTION ( 'NONE',  ( 0.4794255386042041156, -5.511896626706601104E-17, -0.8775825618903722036 ) ) ;
#108909 = CARTESIAN_POINT ( 'NONE',  ( 9.986106302859869999, 1472.420748959189950, 214.7747459013789921 ) ) ;
#108910 = CARTESIAN_POINT ( 'NONE',  ( 12.65362936969999907, 1421.491550492859915, 206.7389950482590280 ) ) ;
#108911 = DIRECTION ( 'NONE',  ( -0.9455185755993178454, 0.000000000000000000, 0.3255681544571537578 ) ) ;
#108912 = EDGE_CURVE ( 'NONE', #11504, #55526, #74727, .T. ) ;
#108914 = CARTESIAN_POINT ( 'NONE',  ( -8.297441882400001134, 1384.888147545379979, 218.7035559121489996 ) ) ;
#108913 = CARTESIAN_POINT ( 'NONE',  ( 6.554764161265000055, 1516.786099423779888, 216.8374711732070068 ) ) ;
#108915 = CARTESIAN_POINT ( 'NONE',  ( -31.61373809194337170, 1450.520981466214153, 136.3130663088220160 ) ) ;
#108916 = CARTESIAN_POINT ( 'NONE',  ( 29.99620953741496621, 1526.382868172863937, 219.7462484079458704 ) ) ;
#108917 = ORIENTED_EDGE ( 'NONE', *, *, #34328, .T. ) ;
#108918 = CARTESIAN_POINT ( 'NONE',  ( -6.943602691585000208, 1516.858069504249897, 202.1807456543569685 ) ) ;
#108919 = CARTESIAN_POINT ( 'NONE',  ( 11.94601693890058591, 1433.509856785846750, 149.8908047706937623 ) ) ;
#108920 = CARTESIAN_POINT ( 'NONE',  ( 0.3722769094550000268, 1457.826255240429873, 228.9731060097980162 ) ) ;
#108921 = AXIS2_PLACEMENT_3D ( 'NONE', #99143, #5668, #39815 ) ;
#108922 = DIRECTION ( 'NONE',  ( -0.2054769195713184726, 3.564456361518036305E-16, 0.9786619618251657382 ) ) ;
#108923 = CARTESIAN_POINT ( 'NONE',  ( 10.82757510571090087, 1461.786499189259985, 210.8991486123640016 ) ) ;
#108924 = CARTESIAN_POINT ( 'NONE',  ( -4.653281936863520762, 1425.827070423550140, 186.2156739099499987 ) ) ;
#108925 = EDGE_CURVE ( 'NONE', #21199, #81391, #73630, .T. ) ;
#108926 =( BOUNDED_CURVE ( )  B_SPLINE_CURVE ( 3, ( #24153, #109843, #92468, #6274 ),
 .UNSPECIFIED., .F., .T. ) 
 B_SPLINE_CURVE_WITH_KNOTS ( ( 4, 4 ),
 ( 1.569654396653685113, 1.584183882043254998 ),
 .UNSPECIFIED. ) 
 CURVE ( )  GEOMETRIC_REPRESENTATION_ITEM ( )  RATIONAL_B_SPLINE_CURVE ( ( 1.000000000000000000, 0.9999824079152302980, 0.9999824079152302980, 1.000000000000000000 ) ) 
 REPRESENTATION_ITEM ( '' )  );
#108927 = CARTESIAN_POINT ( 'NONE',  ( 4.780307568339999591, 1467.625956517089890, 217.8721402715589761 ) ) ;
#108928 = PLANE ( 'NONE',  #19218 ) ;
#108929 = AXIS2_PLACEMENT_3D ( 'NONE', #86339, #43793, #109357 ) ;
#108930 = CARTESIAN_POINT ( 'NONE',  ( 39.92950177491940167, 1445.941520873710033, 136.8098320836529922 ) ) ;
#108931 = CARTESIAN_POINT ( 'NONE',  ( -20.08890542589999839, 1427.297090845429921, 222.6039534643979891 ) ) ;
#108932 = CIRCLE ( 'NONE', #85647, 2.000000000000000444 ) ;
#108933 = CARTESIAN_POINT ( 'NONE',  ( -20.61188484020000189, 1484.905759244990122, 208.1134661061090014 ) ) ;
#108934 = CARTESIAN_POINT ( 'NONE',  ( -104.8482432769999946, 1389.575902442549932, 300.8837059871590327 ) ) ;
#108935 = DIRECTION ( 'NONE',  ( 0.9455185755993178454, 0.000000000000000000, -0.3255681544571537578 ) ) ;
#108936 = CARTESIAN_POINT ( 'NONE',  ( 20.28160989817542870, 1526.000688113705564, 184.8337570730933237 ) ) ;
#108937 = ADVANCED_FACE ( 'NONE', ( #56814 ), #60689, .T. ) ;
#108938 = CARTESIAN_POINT ( 'NONE',  ( -32.70045657439047204, 1460.057872603863643, 269.5016316249235047 ) ) ;
#108939 = EDGE_LOOP ( 'NONE', ( #106032, #78630, #109351, #9009 ) ) ;
#108940 = CARTESIAN_POINT ( 'NONE',  ( -27.43355922089999765, 1507.980920696029898, 210.8261541407979962 ) ) ;
#108941 = CARTESIAN_POINT ( 'NONE',  ( -42.04831442898936444, 1427.619777667461676, 269.0744805272954068 ) ) ;
#108942 = ADVANCED_FACE ( 'NONE', ( #81991 ), #43674, .F. ) ;
#108943 = CARTESIAN_POINT ( 'NONE',  ( -4.668127369574689212, 1508.551704406479985, 213.4552074811490172 ) ) ;
#108944 = CARTESIAN_POINT ( 'NONE',  ( -5.102344180470000268, 1483.010475857490064, 199.7820757393690201 ) ) ;
#108945 = CARTESIAN_POINT ( 'NONE',  ( -32.38845791999504797, 1523.456872492435195, 202.1182848005516632 ) ) ;
#108946 = CARTESIAN_POINT ( 'NONE',  ( -13.50801430494305144, 1444.065531194597725, 187.0996317180838560 ) ) ;
#108947 = CARTESIAN_POINT ( 'NONE',  ( -8.651457448287009910, 1437.323783882450016, 208.9337525471009656 ) ) ;
#108948 = CARTESIAN_POINT ( 'NONE',  ( -3.272146740928380204, 1515.551704204679936, 212.7661985179009889 ) ) ;
#108949 = AXIS2_PLACEMENT_3D ( 'NONE', #71636, #88933, #61556 ) ;
#108950 = EDGE_CURVE ( 'NONE', #106739, #29094, #84207, .T. ) ;
#108951 = CARTESIAN_POINT ( 'NONE',  ( 0.000000000000000000, 1442.773887286369927, 126.8032249175980155 ) ) ;
#108952 = CARTESIAN_POINT ( 'NONE',  ( -15.28181346384849881, 1415.677402202079975, 208.7265255348459903 ) ) ;
#108953 = CIRCLE ( 'NONE', #32056, 1.999999999999997780 ) ;
#108954 = LINE ( 'NONE', #31679, #33897 ) ;
#108955 = CARTESIAN_POINT ( 'NONE',  ( -3.643503312559999596, 1432.730203132190127, 213.6018711577490024 ) ) ;
#108957 = ORIENTED_EDGE ( 'NONE', *, *, #31790, .T. ) ;
#108956 = CARTESIAN_POINT ( 'NONE',  ( -14.06840730360000080, 1410.335884372329929, 226.9421448683980032 ) ) ;
#108958 = B_SPLINE_CURVE_WITH_KNOTS ( 'NONE', 3,
 ( #43012, #77169, #92292, #49763 ),
 .UNSPECIFIED., .F., .F.,
 ( 4, 4 ),
 ( 0.000000000000000000, 0.0002960034161023848936 ),
 .UNSPECIFIED. ) ;
#108959 = CARTESIAN_POINT ( 'NONE',  ( 0.3166099824879999858, 1416.237488680629895, 190.8312741502979861 ) ) ;
#108960 = CARTESIAN_POINT ( 'NONE',  ( 21.95218051589786157, 1509.537469184427891, 226.8469781385923909 ) ) ;
#108961 = ORIENTED_EDGE ( 'NONE', *, *, #90559, .T. ) ;
#108962 = VERTEX_POINT ( 'NONE', #75283 ) ;
#108963 = CARTESIAN_POINT ( 'NONE',  ( 17.90185111903100079, 1415.935475482089942, 209.1139596251610158 ) ) ;
#108964 = DIRECTION ( 'NONE',  ( -0.1070030146457317810, 0.000000000000000000, 0.9942586961433755866 ) ) ;
#108966 = CARTESIAN_POINT ( 'NONE',  ( 2.828023937740000225E-08, 1459.479586679530030, 211.7966661906679917 ) ) ;
#108965 = CARTESIAN_POINT ( 'NONE',  ( 3.733372969449999967, 1456.065302378790193, 219.0848356464390179 ) ) ;
#108967 = CARTESIAN_POINT ( 'NONE',  ( -20.41479141479999981, 1507.904137136529926, 189.4586056721979901 ) ) ;
#108968 = CARTESIAN_POINT ( 'NONE',  ( -11.81534876189999927, 1433.145554964519988, 150.5637033868979699 ) ) ;
#108969 = DIRECTION ( 'NONE',  ( 5.980589973904019347E-17, -1.000000000000000000, 1.736889445713099699E-16 ) ) ;
#108970 = AXIS2_PLACEMENT_3D ( 'NONE', #8905, #27371, #10020 ) ;
#108971 = CARTESIAN_POINT ( 'NONE',  ( 15.74021840827733598, 1519.551704408389924, 196.3375305112799936 ) ) ;
#108972 = CARTESIAN_POINT ( 'NONE',  ( 12.39098288733500119, 1517.051704408389924, 218.3803088333170024 ) ) ;
#108973 = CARTESIAN_POINT ( 'NONE',  ( -24.42533849189999984, 1437.817893690260235, 210.7709910404479956 ) ) ;
#108974 = FACE_BOUND ( 'NONE', #90636, .T. ) ;
#108975 = CARTESIAN_POINT ( 'NONE',  ( 1.885834960689999784, 1450.497026778770078, 182.4567463587980001 ) ) ;
#108976 = CARTESIAN_POINT ( 'NONE',  ( 7.602738516744689257, 1364.209988717608212, 208.3718459617061285 ) ) ;
#108977 = CARTESIAN_POINT ( 'NONE',  ( -16.02051642983965252, 1509.593599257673759, 183.6930697544212023 ) ) ;
#108978 = EDGE_CURVE ( 'NONE', #7065, #46444, #26938, .T. ) ;
#108980 = EDGE_LOOP ( 'NONE', ( #104748, #9869, #37768, #3711, #72657 ) ) ;
#108979 = CARTESIAN_POINT ( 'NONE',  ( 6.225972109890000716, 1494.795958560490135, 219.7811165620990153 ) ) ;
#108981 = ORIENTED_EDGE ( 'NONE', *, *, #25761, .F. ) ;
#108982 = CARTESIAN_POINT ( 'NONE',  ( -11.75396294214339932, 1426.798760010640081, 145.3508344385039948 ) ) ;
#108983 = ADVANCED_FACE ( 'NONE', ( #2457 ), #36033, .T. ) ;
#108984 = CARTESIAN_POINT ( 'NONE',  ( 19.43854577420000140, 1499.207340252790118, 221.7758532508989902 ) ) ;
#108985 = CARTESIAN_POINT ( 'NONE',  ( -5.349258416210000533, 1473.354001796429884, 270.3881948814980092 ) ) ;
#108986 = CARTESIAN_POINT ( 'NONE',  ( -18.86688640473622414, 1511.187213306747708, 180.7825021045441076 ) ) ;
#108987 = CARTESIAN_POINT ( 'NONE',  ( -113.4000000000000057, 1368.558218059089995, 316.1375217595589788 ) ) ;
#108988 = CARTESIAN_POINT ( 'NONE',  ( -14.65245215464970130, 1420.119839417710182, 213.8659310620899987 ) ) ;
#108989 = AXIS2_PLACEMENT_3D ( 'NONE', #53635, #28408, #45229 ) ;
#108990 = CARTESIAN_POINT ( 'NONE',  ( 2.165176160181189857, 1526.186458717540972, 240.2894009330130132 ) ) ;
#108991 = CARTESIAN_POINT ( 'NONE',  ( -8.845811798939999804, 1384.799939604860128, 199.9263747969989709 ) ) ;
#108992 = CARTESIAN_POINT ( 'NONE',  ( 5.513435558014999849, 1509.038615934239942, 216.6345961781970288 ) ) ;
#108993 = CARTESIAN_POINT ( 'NONE',  ( -4.329341215434440393, 1515.068899831251429, 206.1636082373503598 ) ) ;
#108994 = CARTESIAN_POINT ( 'NONE',  ( 11.76506628332722748, 1365.966147004922504, 208.3718459617010978 ) ) ;
#108995 = CARTESIAN_POINT ( 'NONE',  ( -41.65756761579879708, 1426.556841175060072, 269.0856960666789632 ) ) ;
#108996 = ORIENTED_EDGE ( 'NONE', *, *, #77689, .F. ) ;
#108997 = LINE ( 'NONE', #32283, #62766 ) ;
#108998 = B_SPLINE_SURFACE_WITH_KNOTS ( 'NONE', 5, 5, ( 
 ( #25537, #61401, #18793, #51307, #42925, #8742 ),
 ( #77082, #34510, #78164, #9860, #44027, #68687 ),
 ( #35608, #41807, #102793, #26090, #1476, #69803 ),
 ( #60279, #17677, #51880, #86016, #9316, #43479 ),
 ( #77624, #935, #21545, #80385, #3701, #72541 ),
 ( #78727, #27766, #2042, #89328, #10973, #54655 ) ),
 .UNSPECIFIED., .F., .F., .F.,
 ( 6, 6 ),
 ( 6, 6 ),
 ( 95.54053164052498914, 167.5214209060000030 ),
 ( -0.0006553164636343219865, 2.000655316463329836 ),
 .UNSPECIFIED. ) ;
#108999 = EDGE_LOOP ( 'NONE', ( #47090, #47181 ) ) ;
#109000 = ORIENTED_EDGE ( 'NONE', *, *, #13707, .F. ) ;
#109001 = CARTESIAN_POINT ( 'NONE',  ( 5.787476994515000861, 1517.070197312179971, 211.9915394291670054 ) ) ;
#109002 = ADVANCED_FACE ( 'NONE', ( #11923 ), #95540, .F. ) ;
#109003 = CARTESIAN_POINT ( 'NONE',  ( 17.22592475669603473, 1443.913060387329097, 162.9227486557985003 ) ) ;
#109004 = CARTESIAN_POINT ( 'NONE',  ( 5.838247866735959413, 1424.382028414360093, 193.5240377819480102 ) ) ;
#109006 = CARTESIAN_POINT ( 'NONE',  ( -2.370970874524634286, 1427.002265528474027, 134.0999999980980135 ) ) ;
#109005 = CARTESIAN_POINT ( 'NONE',  ( -1.702754409475000008, 1517.014196759610059, 212.5856132281170119 ) ) ;
#109007 = CARTESIAN_POINT ( 'NONE',  ( -10.00325457980000010, 1455.444522322430203, 186.2569471202980083 ) ) ;
#109008 = AXIS2_PLACEMENT_3D ( 'NONE', #31488, #91413, #106557 ) ;
#109009 = CARTESIAN_POINT ( 'NONE',  ( -17.64503295873700139, 1507.624289566409971, 229.7594340571970122 ) ) ;
#109010 = B_SPLINE_SURFACE_WITH_KNOTS ( 'NONE', 5, 5, ( 
 ( #88854, #4308, #12138, #80460, #79911, #79358 ),
 ( #21619, #12692, #13219, #105105, #2672, #45776 ),
 ( #70989, #3224, #3773, #28396, #36797, #73157 ),
 ( #37906, #106202, #62596, #63680, #87768, #98346 ),
 ( #11049, #81531, #38980, #72611, #63143, #37351 ),
 ( #28954, #55274, #55824, #97244, #96713, #97791 ) ),
 .UNSPECIFIED., .F., .F., .F.,
 ( 6, 6 ),
 ( 6, 6 ),
 ( 0.9031050603770000018, 1.041569279630000011 ),
 ( 0.000000000000000000, 2.000000000000000000 ),
 .UNSPECIFIED. ) ;
#109011 = ORIENTED_EDGE ( 'NONE', *, *, #104098, .T. ) ;
#109012 = CARTESIAN_POINT ( 'NONE',  ( -26.81252206619999967, 1435.744110061079937, 136.2294616770979871 ) ) ;
#109013 = CARTESIAN_POINT ( 'NONE',  ( -4.037378294184999383, 1516.688761843659904, 202.5730239910470232 ) ) ;
#109014 = VECTOR ( 'NONE', #65853, 1000.000000000000000 ) ;
#109015 = EDGE_CURVE ( 'NONE', #25299, #21185, #88415, .T. ) ;
#109016 = B_SPLINE_SURFACE_WITH_KNOTS ( 'NONE', 5, 5, ( 
 ( #78389, #52645, #45363, #54317, #68912, #18446 ),
 ( #52095, #103579, #26309, #94623, #88446, #10071 ),
 ( #17898, #9517, #44246, #44805, #77836, #71124 ),
 ( #105245, #62165, #35277, #43685, #69462, #26881 ),
 ( #61070, #1697, #35838, #96291, #70021, #104135 ),
 ( #27421, #77295, #61604, #19001, #28536, #53201 ),
 ( #87342, #78958, #87910, #2265, #62737, #36379 ),
 ( #70568, #19570, #11199, #79502, #2809, #97386 ),
 ( #64914, #12826, #3910, #98483, #37488, #38574 ),
 ( #55953, #88983, #38040, #20657, #39119, #72219 ),
 ( #54859, #106880, #13914, #22860, #12271, #99025 ),
 ( #89537, #47006, #107986, #105811, #55405, #48099 ),
 ( #31283, #30171, #65467, #71692, #29627, #90075 ),
 ( #81130, #13358, #29090, #82239, #106341, #56504 ),
 ( #22301, #63275, #5540, #57066, #47549, #39691 ) ),
 .UNSPECIFIED., .F., .F., .F.,
 ( 6, 3, 3, 3, 6 ),
 ( 6, 6 ),
 ( 29.73194161469999841, 37.05188947199999916, 56.18585872479999921, 82.63977583489999290, 135.5476100549999785 ),
 ( -3.023210959359999692E-09, 2.000000000000000000 ),
 .UNSPECIFIED. ) ;
#109017 = CARTESIAN_POINT ( 'NONE',  ( -7.487063421429379417, 1517.051703294439903, 208.6815157772669806 ) ) ;
#109018 = CARTESIAN_POINT ( 'NONE',  ( -41.60088707320420554, 1384.587835658240010, 214.5004774267979997 ) ) ;
#109019 = CARTESIAN_POINT ( 'NONE',  ( -44.93140602508920267, 1440.913053221170003, 269.6837651506019711 ) ) ;
#109020 = CARTESIAN_POINT ( 'NONE',  ( -4.802552260849999755, 1482.676166849490073, 203.0569153438389947 ) ) ;
#109021 = DIRECTION ( 'NONE',  ( 4.440892098500004934E-16, 1.000000000000000000, -1.817990202819999994E-15 ) ) ;
#109022 = CIRCLE ( 'NONE', #89349, 20.98341875040010507 ) ;
#109023 = EDGE_CURVE ( 'NONE', #63480, #66318, #97731, .T. ) ;
#109025 = EDGE_LOOP ( 'NONE', ( #16509, #65471 ) ) ;
#109024 = CARTESIAN_POINT ( 'NONE',  ( -38.57017548137279306, 1443.484401788910191, 137.1611502647359941 ) ) ;
#109026 = EDGE_LOOP ( 'NONE', ( #27411, #14414, #66730, #44975, #8133 ) ) ;
#109027 = CARTESIAN_POINT ( 'NONE',  ( 0.2421645026379999899, 1451.163597850030101, 182.5480897152980049 ) ) ;
#109028 = CARTESIAN_POINT ( 'NONE',  ( -28.82451532742324929, 1526.348417187219184, 220.0525736641747017 ) ) ;
#109029 = CARTESIAN_POINT ( 'NONE',  ( -1.925896724263820081, 1425.116320396220090, 191.2239611826650219 ) ) ;
#109030 = CARTESIAN_POINT ( 'NONE',  ( -23.77614021810000011, 1435.333969175160064, 137.3595125206979901 ) ) ;
#109031 = CARTESIAN_POINT ( 'NONE',  ( -24.90875591689999879, 1442.283708403439960, 210.4817964918080122 ) ) ;
#109033 = CARTESIAN_POINT ( 'NONE',  ( -2.863787893864999656, 1516.788317650260069, 210.8382387120070121 ) ) ;
#109032 = AXIS2_PLACEMENT_3D ( 'NONE', #13458, #8791, #24486 ) ;
#109034 = CARTESIAN_POINT ( 'NONE',  ( -68.77631069450001178, 1379.747998137240074, 280.2624785784589676 ) ) ;
#109035 = DIRECTION ( 'NONE',  ( 0.000000000000000000, 0.000000000000000000, 1.000000000000000000 ) ) ;
#109036 = CARTESIAN_POINT ( 'NONE',  ( -14.32036905050000009, 1426.820448865629942, 222.1614598904980085 ) ) ;
#109037 = CARTESIAN_POINT ( 'NONE',  ( 3.646194203732994854, 1440.832530381142760, 156.5727254137537159 ) ) ;
#109038 = ADVANCED_FACE ( 'NONE', ( #8455 ), #26668, .T. ) ;
#109039 = CARTESIAN_POINT ( 'NONE',  ( -2.299983615734999987, 1516.861367446839949, 206.8392230197369770 ) ) ;
#109040 = ORIENTED_EDGE ( 'NONE', *, *, #79994, .T. ) ;
#109041 = CARTESIAN_POINT ( 'NONE',  ( 7.709151570915000029, 1516.538881389200014, 206.5697199716970260 ) ) ;
#109042 = CARTESIAN_POINT ( 'NONE',  ( -8.630767090659189122, 1438.254930141910108, 208.1080191835690130 ) ) ;
#109043 = CARTESIAN_POINT ( 'NONE',  ( -19.66086063814984186, 1456.978398402603716, 225.7864354487686285 ) ) ;
#109044 = ORIENTED_EDGE ( 'NONE', *, *, #23088, .T. ) ;
#109045 = CARTESIAN_POINT ( 'NONE',  ( 7.366459948930000223, 1481.681596261390041, 209.4342970301970013 ) ) ;
#109046 = ADVANCED_FACE ( 'NONE', ( #49932 ), #64446, .F. ) ;
#109047 = DIRECTION ( 'NONE',  ( 0.8248189069719331634, 0.4629720251890361293, -0.3245468758037705626 ) ) ;
#109048 = CARTESIAN_POINT ( 'NONE',  ( -4.113893833246661025, 1440.069258426123497, 185.4380465277182282 ) ) ;
#109049 = CARTESIAN_POINT ( 'NONE',  ( 15.05358515032119904, 1410.831827804430077, 191.5175411757069810 ) ) ;
#109050 = CARTESIAN_POINT ( 'NONE',  ( 2.500000000000000000, 1443.913060387330006, 150.6726614421979775 ) ) ;
#109051 = CARTESIAN_POINT ( 'NONE',  ( -10.22326110114815201, 1374.913060387290216, 213.8507217284212345 ) ) ;
#109052 = CARTESIAN_POINT ( 'NONE',  ( 5.634333898429999543, 1486.294848711289887, 199.9182129588890007 ) ) ;
#109053 = CARTESIAN_POINT ( 'NONE',  ( 2.409586283469999923, 1426.663880916129983, 144.1938086916980239 ) ) ;
#109054 = CARTESIAN_POINT ( 'NONE',  ( 22.06126275483152810, 1452.693645232389372, 220.1374946003218440 ) ) ;
#109055 = EDGE_CURVE ( 'NONE', #83948, #31992, #21552, .T. ) ;
#109056 = TOROIDAL_SURFACE ( 'NONE', #23191, 2.000000000000000000, 1.000000000000000000 ) ;
#109057 = CARTESIAN_POINT ( 'NONE',  ( -17.76922258761841888, 1445.720595802438993, 202.6296028318632523 ) ) ;
#109058 = DIRECTION ( 'NONE',  ( 0.8730704095473449389, 0.4873619484741930075, 0.01504630028510589926 ) ) ;
#109059 = CARTESIAN_POINT ( 'NONE',  ( 3.454748808194999743, 1516.609912606490070, 216.4448802441970088 ) ) ;
#109060 = ORIENTED_EDGE ( 'NONE', *, *, #49397, .F. ) ;
#109061 = CARTESIAN_POINT ( 'NONE',  ( -11.69744348347709995, 1415.090956648730071, 195.9645815027980120 ) ) ;
#109062 = DIRECTION ( 'NONE',  ( 1.755985294532464991E-16, -1.000000000000000000, 1.338183447452830017E-16 ) ) ;
#109063 = CARTESIAN_POINT ( 'NONE',  ( 0.2538967969029999883, 1420.503737814829947, 182.7635776114979933 ) ) ;
#109064 = ADVANCED_FACE ( 'NONE', ( #57798 ), #91920, .T. ) ;
#109065 = EDGE_CURVE ( 'NONE', #68085, #41682, #83511, .T. ) ;
#109066 = CARTESIAN_POINT ( 'NONE',  ( -1.176577584829999967, 1474.814957531289792, 219.4969863823990011 ) ) ;
#109067 = CARTESIAN_POINT ( 'NONE',  ( -9816.840209716168829, 50.13405481564039690, 1424.308828391800034 ) ) ;
#109068 = CARTESIAN_POINT ( 'NONE',  ( -11.21541762013639953, 1471.302741629689990, 206.9949349079969920 ) ) ;
#109069 = CARTESIAN_POINT ( 'NONE',  ( -5.719822330129272103, 1508.285359404909286, 220.2077194730133556 ) ) ;
#109070 = CIRCLE ( 'NONE', #26809, 8.989690721650012151 ) ;
#109071 = CARTESIAN_POINT ( 'NONE',  ( 17.20725958045629866, 1422.406334852679720, 226.7076084557567981 ) ) ;
#109072 = CARTESIAN_POINT ( 'NONE',  ( -2.568069795494909879, 1454.639726342709992, 198.9496893171560146 ) ) ;
#109073 = CARTESIAN_POINT ( 'NONE',  ( -21.83550407203940580, 1523.678648413191695, 183.2743720722710350 ) ) ;
#109074 = CARTESIAN_POINT ( 'NONE',  ( 25.98102620618460179, 1446.564900598649956, 138.2990622187049894 ) ) ;
#109076 = CARTESIAN_POINT ( 'NONE',  ( 4.326992699989999913, 1515.158586642790169, 209.1218459614979963 ) ) ;
#109075 = CARTESIAN_POINT ( 'NONE',  ( -10.14096832535920001, 1471.320523670169905, 210.8482381047599858 ) ) ;
#109077 = DIRECTION ( 'NONE',  ( -0.02617070069600989368, -0.9996573249755577040, 0.0005718809247485686070 ) ) ;
#109078 = ORIENTED_EDGE ( 'NONE', *, *, #110075, .T. ) ;
#109079 = ORIENTED_EDGE ( 'NONE', *, *, #29511, .F. ) ;
#109080 = CARTESIAN_POINT ( 'NONE',  ( -27.01382282590000017, 1451.969727051930022, 134.9184453750980026 ) ) ;
#109081 = CARTESIAN_POINT ( 'NONE',  ( -9.336114142359406287, 1506.539416414647121, 229.1226208970104494 ) ) ;
#109082 = CARTESIAN_POINT ( 'NONE',  ( -2.044458700900000370, 1442.173530875790220, 200.4791613073190035 ) ) ;
#109083 = DIRECTION ( 'NONE',  ( -0.001078628244322317031, -3.766396416021244533E-05, -0.9999994175710984479 ) ) ;
#109084 = CARTESIAN_POINT ( 'NONE',  ( 271.2574323654409909, 11216.44053380570040, 2234.264705616360061 ) ) ;
#109085 = EDGE_CURVE ( 'NONE', #56358, #2071, #25520, .T. ) ;
#109086 = CARTESIAN_POINT ( 'NONE',  ( 27.53661718181439610, 1509.986717858917018, 221.0270820719949256 ) ) ;
#109087 = CARTESIAN_POINT ( 'NONE',  ( -1.253615010250130002, 1508.551704408389924, 220.0817883865630051 ) ) ;
#109088 = CARTESIAN_POINT ( 'NONE',  ( -3.034926079678273325, 1369.200812461397618, 207.6218459616989946 ) ) ;
#109089 = CARTESIAN_POINT ( 'NONE',  ( -37.20393503414990022, 1383.832344231630032, 237.1622210560479971 ) ) ;
#109090 = CARTESIAN_POINT ( 'NONE',  ( -4.554948383327420025, 1508.731373119430145, 206.6339226617529903 ) ) ;
#109091 = CARTESIAN_POINT ( 'NONE',  ( 5.940539708128937058, 1517.051704408389924, 189.0391861795680768 ) ) ;
#109092 = CARTESIAN_POINT ( 'NONE',  ( -2.470168521978398868, 1512.187213306747481, 175.3649660270905315 ) ) ;
#109093 = CARTESIAN_POINT ( 'NONE',  ( 10.51030381764329924, 1491.592991267690195, 212.4264936531670003 ) ) ;
#109095 = ORIENTED_EDGE ( 'NONE', *, *, #18017, .T. ) ;
#109094 = CARTESIAN_POINT ( 'NONE',  ( -1.912679614370000003, 1457.559505151690018, 219.6146910743989906 ) ) ;
#109096 = CARTESIAN_POINT ( 'NONE',  ( 31.97190655716360652, 1524.330813522192102, 216.6896206998345349 ) ) ;
#109097 = AXIS2_PLACEMENT_3D ( 'NONE', #79536, #2301, #89015 ) ;
#109098 = B_SPLINE_SURFACE_WITH_KNOTS ( 'NONE', 5, 5, ( 
 ( #92180, #7074, #83779, #110082, #66460, #41230 ),
 ( #75929, #92722, #13796, #57503, #5973, #101109 ),
 ( #67552, #108432, #83230, #74847, #108991, #47981 ),
 ( #22738, #32813, #5420, #39579, #73751, #56942 ),
 ( #50200, #24406, #65352, #82683, #91071, #31162 ),
 ( #58591, #15998, #107874, #84326, #99460, #7616 ),
 ( #41773, #101654, #14354, #40118, #24942, #110632 ),
 ( #85410, #353, #43993, #17084, #68654, #69202 ),
 ( #94939, #44546, #8159, #43442, #102755, #51278 ) ),
 .UNSPECIFIED., .F., .F., .F.,
 ( 6, 3, 6 ),
 ( 6, 6 ),
 ( 4.382742598350000129, 4.857690652960000577, 5.332638707570000136 ),
 ( 0.000000000000000000, 2.000000000000000000 ),
 .UNSPECIFIED. ) ;
#109099 = CARTESIAN_POINT ( 'NONE',  ( -55.92238506969999889, 1380.972976875320001, 269.5160511658589826 ) ) ;
#109100 = CARTESIAN_POINT ( 'NONE',  ( -17.08792848909999762, 1409.509783999230194, 223.5124184947979984 ) ) ;
#109101 = VERTEX_POINT ( 'NONE', #103062 ) ;
#109102 = ORIENTED_EDGE ( 'NONE', *, *, #45994, .F. ) ;
#109103 = CARTESIAN_POINT ( 'NONE',  ( -8.801669235211798892, 1386.375422881679924, 218.4188921187869994 ) ) ;
#109104 = CARTESIAN_POINT ( 'NONE',  ( -3.465053098240730378, 1515.493282983300105, 205.2090698384729990 ) ) ;
#109106 = DIRECTION ( 'NONE',  ( -0.8023110876747339137, -0.5969061220947440294, 0.000000000000000000 ) ) ;
#109105 = CARTESIAN_POINT ( 'NONE',  ( 3.347801439296143933, 1523.382868172864164, 242.0893193391992497 ) ) ;
#109107 = AXIS2_PLACEMENT_3D ( 'NONE', #97839, #87253, #18918 ) ;
#109108 = CARTESIAN_POINT ( 'NONE',  ( -8.979645201780000363, 1461.875990298290162, 205.2600572402090222 ) ) ;
#109109 = CARTESIAN_POINT ( 'NONE',  ( -105.5449098450000065, 1380.452663771340212, 300.3143822648590344 ) ) ;
#109110 = CARTESIAN_POINT ( 'NONE',  ( -22.08327125186908191, 1523.604703353109699, 233.8169256665491105 ) ) ;
#109111 = B_SPLINE_CURVE_WITH_KNOTS ( 'NONE', 3,
 ( #63240, #80003, #36892, #52609, #38002, #19529, #18411, #72184, #26842, #71085, #10597, #61028, #87872, #86747, #70532, #44208, #104650, #78351, #1660, #44769, #27946, #69981, #61567, #62127, #96254, #53735, #45323, #22260, #29587, #46971, #56461, #38538, #14426, #91701, #39652, #64324, #31242, #91150, #89501, #12793, #72715, #49170, #21161, #31792, #98447, #47510, #48622, #99533, #90594, #73822, #13871, #21715, #65426, #55919, #106838, #48057, #57024, #23386, #63771, #106303, #82192, #108505, #22817, #39079, #107397, #5495, #30693, #107950, #82754, #14975, #100105, #55368, #64879, #6046, #65982, #81093, #90038, #73257, #83302, #40197, #74380, #98986, #57576, #6597, #13315, #4409, #30132, #40747, #97887, #81633, #4935, #85486, #7151, #109613, #58666, #76005, #102839, #26133, #92253, #17719, #58119, #74924, #86064, #92802, #83851, #16612, #9359, #32886, #15523, #59230, #59774, #42968, #68192, #8232, #101740, #51921, #34552, #100638, #93347, #7693, #23925, #8786, #67079, #49719, #41850, #41307, #68735, #42399, #67626, #33999, #84939, #75480, #25028, #60322, #76553, #110709, #102296, #33429, #25581 ),
 .UNSPECIFIED., .F., .F.,
 ( 4, 3, 3, 3, 3, 3, 3, 3, 3, 3, 3, 3, 3, 3, 3, 3, 3, 3, 3, 3, 3, 3, 3, 3, 3, 3, 3, 3, 3, 3, 3, 3, 3, 3, 3, 3, 3, 3, 3, 3, 3, 3, 3, 3, 3, 3, 4 ),
 ( -28.53827112919999820, -26.45221505981819732, -24.01267252766740157, -21.74496381986899962, -19.71304886792480104, -17.83305997891750039, -16.05771537107780134, -14.36033624732730019, -12.75138636564559924, -11.18760895869190009, -9.657646656378112482, -8.173724279849281515, -6.990632790278482389, -5.760582367847380425, -4.497816196510928677, -3.242242590771951427, -1.969189602956539886, -0.6774439780757006702, 0.6566481976939542164, 1.992772157457029181, 3.367048238499528168, 4.341547002844251324, 5.758069219566863239, 7.176877794369772801, 8.618992616491055969, 9.956394040244987309, 11.39760739419979529, 12.72337739229750042, 14.29692855573880195, 15.67372473662510401, 16.59104555840569617, 17.57661266362431007, 18.56849156666920209, 19.56575179944280052, 20.56727088331129494, 21.57175587605299683, 22.57778385006959354, 23.58385892812350448, 24.58711680646079856, 25.58704511002700599, 26.58256055503940019, 27.57272639591489849, 28.57604209978619991, 29.55008166352749299, 30.56803543746379859, 31.52659850778239559, 31.58598921140000471 ),
 .UNSPECIFIED. ) ;
#109112 = CARTESIAN_POINT ( 'NONE',  ( -9.924526517117328694, 1508.551704408389924, 218.3000131550199967 ) ) ;
#109113 = CARTESIAN_POINT ( 'NONE',  ( 9.063831788663421207, 1409.229576367929894, 197.2185231063879769 ) ) ;
#109114 = CARTESIAN_POINT ( 'NONE',  ( 0.5238716732950000621, 1409.870337220530018, 185.0929749023979980 ) ) ;
#109115 = CARTESIAN_POINT ( 'NONE',  ( -108.4578349762840048, 1385.240951097619927, 297.1233463436130364 ) ) ;
#109116 = FACE_OUTER_BOUND ( 'NONE', #71878, .T. ) ;
#109117 = CONICAL_SURFACE ( 'NONE', #8933, 6.911399307709998219, 0.04363323129990067523 ) ;
#109118 = CARTESIAN_POINT ( 'NONE',  ( -13.62133678120479985, 1452.879579795280051, 223.2680741433150047 ) ) ;
#109119 = VERTEX_POINT ( 'NONE', #103634 ) ;
#109120 = B_SPLINE_CURVE_WITH_KNOTS ( 'NONE', 5,
 ( #83212, #73733, #40101, #30604, #31696, #58025 ),
 .UNSPECIFIED., .F., .F.,
 ( 6, 6 ),
 ( 0.000000000000000000, 1.000000000000000000 ),
 .UNSPECIFIED. ) ;
#109121 = CARTESIAN_POINT ( 'NONE',  ( -21.10560967990489090, 1525.661276915132476, 184.9336828786751141 ) ) ;
#109122 = CARTESIAN_POINT ( 'NONE',  ( 18.38772902297059986, 1457.332268191050161, 228.4537576404730146 ) ) ;
#109123 = CARTESIAN_POINT ( 'NONE',  ( -12.06208110920000109, 1434.483679219209989, 150.8899553371979891 ) ) ;
#109124 = B_SPLINE_CURVE_WITH_KNOTS ( 'NONE', 5,
 ( #90753, #66143, #14032, #82364, #6197, #38694 ),
 .UNSPECIFIED., .F., .F.,
 ( 6, 6 ),
 ( 141.6155516059999968, 151.1003634729999874 ),
 .UNSPECIFIED. ) ;
#109125 = CARTESIAN_POINT ( 'NONE',  ( -6.553452772086439930E-09, 1475.392274334100193, 266.1199166997070051 ) ) ;
#109126 = CARTESIAN_POINT ( 'NONE',  ( 1.249673192637140273, 1515.565594798377106, 213.0676417522672637 ) ) ;
#109127 = CARTESIAN_POINT ( 'NONE',  ( -14.86061390519999925, 1420.111516814780089, 213.2229217038190257 ) ) ;
#109128 = CARTESIAN_POINT ( 'NONE',  ( -109.7404430409999918, 1384.933520221859908, 311.3564660812589864 ) ) ;
#109129 = DIRECTION ( 'NONE',  ( -1.000000000000000000, 0.000000000000000000, 0.000000000000000000 ) ) ;
#109130 = CARTESIAN_POINT ( 'NONE',  ( -9.132344861692528681, 1361.764119804333177, 207.6218459616987673 ) ) ;
#109131 = CARTESIAN_POINT ( 'NONE',  ( -46.02992379481870699, 1440.698477837170003, 268.4959868370419827 ) ) ;
#109132 = CARTESIAN_POINT ( 'NONE',  ( 14.12038737319999804, 1509.406339941330089, 234.8413163218980060 ) ) ;
#109133 = CARTESIAN_POINT ( 'NONE',  ( -8.125957766200000876, 1425.045124160440082, 205.5278006110690114 ) ) ;
#109134 = CARTESIAN_POINT ( 'NONE',  ( 0.7468175155120010400, 1517.006509894990131, 209.1147170949500094 ) ) ;
#109135 = ADVANCED_FACE ( 'NONE', ( #44295 ), #10688, .T. ) ;
#109136 = VECTOR ( 'NONE', #12259, 1000.000000000000227 ) ;
#109137 = CARTESIAN_POINT ( 'NONE',  ( 5.451912722298930092, 1408.921438237069879, 222.1546799351359880 ) ) ;
#109138 = B_SPLINE_SURFACE_WITH_KNOTS ( 'NONE', 5, 5, ( 
 ( #54684, #27247, #10443, #44614, #96667, #35089, #19938, #61428, #69271, #54134, #26680, #95551, #18824, #79868, #60879, #3179, #71505, #105624, #9345, #81489, #73684, #98854, #21025, #80960, #63639, #13725, #48480, #47362, #88810, #97753, #5351, #82046, #107256 ),
 ( #4262, #21578, #55786, #40055, #37860, #98302, #91000, #56871, #39511, #107811, #13173, #72046, #89902, #106163, #22670, #46831, #74236, #30551, #29440, #22117, #99392, #64740, #108367, #4790, #38936, #55228, #56315, #90448, #38395, #89358, #47911, #12653, #72571 ),
 ( #106698, #82618, #31098, #73116, #14290, #65280, #5909, #29990, #31648, #65830, #99947, #64181, #23242, #12094, #46288, #80416, #3730, #32210, #59629, #67489, #101593, #42265, #7002, #59086, #75870, #41711, #57441, #92112, #49578, #15388, #108918, #66937, #66391 ),
 ( #6459, #100510, #83709, #32755, #40607, #75336, #23789, #110020, #49031, #50131, #76414, #24878, #57978, #41161, #109477, #93206, #17018, #15930, #91566, #101045, #84799, #50667, #33296, #110568, #33853, #93740, #16476, #8097, #14842, #68044, #24345, #51217, #83166 ),
 ( #92656, #74778, #58528, #84260, #102154, #7556, #42820, #25433, #85348, #8645, #76980, #289, #34414, #68586, #102691, #9223, #10883, #10312, #11436, #51781, #9760, #44486, #36084, #18695, #45607, #27128, #60751, #1374, #103247, #70824, #45055, #78631, #43381 ),
 ( #79749, #18151, #35517, #27674, #70269, #1946, #2505, #78071, #52892, #52346, #104936, #79199, #36626, #104378, #28223, #61859, #87020, #26558, #95979, #94303, #34959, #19240, #3056, #37182, #71379, #831, #103828, #61314, #53450, #85919, #87595, #69143, #77530 ),
 ( #25986, #62411, #96538, #19812, #94874, #86467, #95432, #69709, #54018, #88148, #60186, #43924, #17581, #54563, #107130, #22538, #64055, #89232, #105490, #81919, #37728, #56180, #80835, #71932, #97637, #38267, #72452, #56740, #88697, #4143, #107687, #73553, #90318 ),
 ( #81363, #14164, #65147, #106582, #47785, #106044, #20358, #39378, #48349, #11978, #29869, #38816, #72992, #46705, #98175, #39931, #90875, #20906, #82488, #5225, #21445, #28781, #98727, #62982, #97093, #46159, #55655, #80290, #89778, #99260, #5790, #30421, #3605 ),
 ( #55107, #13047, #64608, #4677, #21988, #30971, #47236, #13596, #12527, #29321, #63521, #58944, #15787, #42137, #84125, #7424, #41590, #66267, #48907, #33169, #57314, #40474, #31516, #75745, #16891, #109889, #66809, #100910, #76287, #108229, #93612, #100384, #67359 ),
 ( #57852, #91441, #101456, #6862, #24745, #32077, #24208, #58394, #14717, #92520, #51096, #93074, #91980, #83034, #16348, #41023, #50546, #23669, #6325, #110437, #84671, #7970, #33715, #15255, #67909, #49989, #102017, #74100, #108784, #49446, #83570, #74649, #75201 ),
 ( #25300, #23110, #109352, #32633, #59501, #85221, #8513, #65698, #99815, #34278, #35383, #27535, #52752, #85781, #34827, #17446, #78496, #2371, #1245, #42686, #51643, #70133, #35947, #61180, #61718, #95840, #79066, #1811, #104245, #76844, #86885, #94735, #44919 ),
 ( #70683, #18558, #62271, #36486, #43788, #19107, #9080, #68459, #87452, #96400, #25856, #52206, #10179, #44354, #18013, #86333, #88018, #28083, #69014, #19676, #53311, #9619, #156, #10747, #102563, #60057, #94175, #77938, #43247, #69571, #104796, #53881, #77396 ),
 ( #698, #103119, #26420, #103691, #26991, #95297, #60612, #96957, #72853, #20764, #64468, #106987, #4543, #106446, #81228, #21849, #20223, #54963, #105910, #98030, #30275, #79612, #29729, #37589, #72314, #54424, #98583, #55507, #89090, #38677, #11840, #46011, #105350 ),
 ( #37033, #56046, #71228, #28640, #80142, #71791, #62844, #29189, #88557, #80698, #2916, #12377, #89635, #63915, #3461, #63380, #97496, #21302, #90173, #46564, #11302, #4008, #12922, #47102, #38133, #14980, #49175, #45470, #36289, #70481, #510, #44716, #52558 ),
 ( #62078, #27895, #35743, #60409, #9986, #17801, #45272, #69371, #96764, #18916, #94527, #10542, #11111, #53114, #20034, #104043, #27335, #52002, #96204, #95649, #54229, #26220, #95098, #87251, #78868, #61521, #88356, #1606, #35186, #86692, #77750, #79410, #19479 ),
 ( #36844, #105157, #2174, #102920, #104602, #44156, #69930, #78292, #43599, #2722, #53681, #28449, #71036, #62643, #87823, #11645, #45822, #1059, #34635, #68819, #86142, #9435, #103480, #26785, #18364, #60973, #82008, #41117, #32168, #108326, #92074, #74195, #65787 ),
 ( #6423, #40015, #74739, #31609, #23755, #47871, #6964, #5313, #99907, #39471, #23203, #37402, #90405, #108877, #58487, #101008, #24307, #56275, #48442, #75296, #32720, #40568, #64699, #66354, #66901, #73643, #90965, #83125, #91529, #57402, #57942, #22626, #14807 ),
 ( #109441, #15347, #48993, #49542, #92615, #107773, #100472, #14252, #83667, #15892, #71601, #79955, #99351, #3272, #31059, #105722, #30509, #98817, #22079, #13684, #65240, #56830, #82582, #5873, #39861, #81847, #4612, #38746, #108713, #72924, #22471, #107063, #99191 ),
 ( #57238, #21919, #74025, #90807, #56671, #72385, #30347, #64538, #98654, #12987, #5151, #47170, #48834, #30896, #49369, #48277, #74577, #108158, #81298, #98102, #65075, #13530, #91369, #14088, #39306, #21374, #31448, #55583, #65631, #100312, #82422, #56115, #106514 ),
 ( #99745, #5716, #14648, #82957, #32004, #23036, #6251, #29803, #40400, #47717, #66192, #63991, #23597, #57786, #91904, #15181, #83496, #73479, #6792, #90248, #89706, #107612, #60539, #24130, #50478, #85153, #8439, #93000, #84602, #86259, #26343, #67287, #94661 ),
 ( #25230, #51019, #33637, #17932, #42065, #75675, #16276, #7353, #85704, #76765, #40953, #42612, #7893, #43173, #75130, #34205, #68945, #16818, #52130, #625, #76215, #94102, #84054, #66738, #9000, #109279, #58321, #110360, #75, #68389, #67832, #101942, #32562 ),
 ( #100841, #51571, #59433, #92444, #102496, #15719, #49920, #41516, #93545, #109819, #25786, #34756, #103045, #59985, #33098, #17373, #101379, #24672, #77326, #58870, #19602, #96324, #98385, #61640, #2297, #35874, #55864, #30071, #106780, #62197, #89985, #53804, #87941 ),
 ( #95221, #79533, #103618, #86816, #77870, #11232, #64823, #45394, #36408, #70600, #13258, #43718, #30636, #1735, #2836, #36957, #71152, #19036, #52679, #10107, #47448, #44280, #104718, #78424, #28009, #1179, #18483, #64261, #98931, #22204, #56400, #70058, #87379 ),
 ( #104169, #61104, #53237, #27455, #21656, #78994, #9548, #81572, #4875, #39018, #95770, #35309, #73195, #10673, #107340, #69496, #44839, #26916, #15465, #39592, #92192, #7629, #49108, #74317, #90532, #67016, #22752, #41243, #65914, #56956, #82695, #23323, #7087 ),
 ( #100032, #91083, #5985, #57516, #91640, #41787, #73763, #14916, #92738, #58605, #75416, #109554, #83242, #107886, #6536, #31177, #24420, #48559, #75945, #109005, #65366, #100582, #101123, #32290, #110097, #40688, #74861, #99472, #32826, #66474, #33372, #5434, #108447 ),
 ( #83793, #47994, #13808, #82131, #23864, #14365, #58058, #50214, #67566, #49658, #40133, #16013, #101670, #31727, #84341, #24959, #69218, #35040, #35593, #370, #51861, #85425, #103902, #78147, #44008, #915, #27202, #103328, #26635, #60831, #51291, #33931, #18225 ),
 ( #77061, #94955, #59710, #18773, #9843, #85997, #69784, #9296, #43459, #42341, #77607, #2023, #93288, #25516, #93823, #1448, #102774, #52420, #17098, #68128, #61384, #86547, #95503, #52971, #8725, #87103, #10391, #44561, #59169, #42904, #34495, #68670, #110645 ),
 ( #8172, #78710, #76494, #102241, #26065, #60260, #94379, #17660, #36158, #70342, #50741, #104454, #16551, #84877, #70897, #19885, #2581, #63591, #98256, #97159, #27746, #36703, #87668, #29390, #55737, #20430, #11511, #61938, #4214, #105014, #89311, #3132, #28304 ),
 ( #97708, #20981, #96057, #72000, #79825, #29943, #19326, #55185, #89859, #3685, #47312, #21525, #28862, #80916, #62497, #53528, #72523, #81435, #10957, #37262, #106113, #12606, #71460, #105574, #73071, #13128, #54092, #4746, #38344, #63055, #45129, #46786, #79271 ),
 ( #54637, #96618, #88768, #38889, #88217, #106652, #45686, #64135, #12052, #46236, #80369, #37811, #6411, #83117, #83657, #48432, #99895, #22616, #41109, #15337, #92065, #48984, #75286, #40557, #74731, #108865, #99341, #81996, #66345, #90394, #73633, #64689, #32158 ),
 ( #57932, #23193, #6952, #57392, #91518, #13672, #14798, #50081, #30500, #107764, #31048, #49532, #40006, #100461, #65230, #5303, #109432, #23744, #32709, #66890, #56820, #100999, #24295, #58478, #107212, #90956, #14243, #82573, #47862, #5865, #39461, #92605, #56265 ),
 ( #74184, #108315, #31599, #65778, #15878, #98807, #84210, #7506, #41668, #22068, #67997, #68544, #60139, #59037, #94259, #18648, #109976, #42220, #110521, #94826, #8600, #85871, #33803, #50622, #78023, #9172, #43337, #60702, #25388, #77485, #17533, #51735, #75825 ),
 ( #785, #34915, #93159, #101543, #69660, #9712, #24832, #84755, #102109, #51173, #16430, #93694, #8052, #69100, #67444, #102643, #18102, #103202, #76372, #59581, #16974, #26507, #35470, #34370, #33253, #85302, #52297, #86422, #43879, #1330, #103783, #27084, #61269 ) ),
 .UNSPECIFIED., .F., .F., .F.,
 ( 6, 3, 3, 3, 3, 3, 3, 3, 3, 3, 6 ),
 ( 6, 3, 3, 3, 3, 3, 3, 3, 3, 3, 6 ),
 ( 0.000000000000000000, 1.936717162300000128, 3.873434324599999812, 4.841792905749999321, 5.810151486899999718, 7.746868649199999624, 9.683585811500000418, 10.65194439270000082, 11.62030297379999944, 13.55702013610000023, 15.49373729840000102 ),
 ( 0.000000000000000000, 1.936717162300000128, 3.873434324599999812, 4.841792905749999321, 5.810151486899999718, 7.746868649199999624, 9.683585811500000418, 10.65194439270000082, 11.62030297379999944, 13.55702013610000023, 15.49373729840000102 ),
 .UNSPECIFIED. ) ;
#109139 = CARTESIAN_POINT ( 'NONE',  ( 11.43480838300000002, 1425.837049133330083, 122.9428393764980001 ) ) ;
#109140 = CARTESIAN_POINT ( 'NONE',  ( 7.513327647825819966, 1425.400186687669930, 212.2206837014999792 ) ) ;
#109141 = ORIENTED_EDGE ( 'NONE', *, *, #7673, .T. ) ;
#109142 = CARTESIAN_POINT ( 'NONE',  ( 8.200031714130000537, 1420.268578394229962, 225.6600891460980165 ) ) ;
#109144 = CARTESIAN_POINT ( 'NONE',  ( -16.19188927940000156, 1409.478493620530116, 194.5079787952979871 ) ) ;
#109143 = CARTESIAN_POINT ( 'NONE',  ( -12.02051106306990036, 1491.153688555679992, 206.6632162730240054 ) ) ;
#109145 = CARTESIAN_POINT ( 'NONE',  ( -19.41751478759999827, 1465.673884635790273, 205.2708586912889928 ) ) ;
#109146 = VECTOR ( 'NONE', #21026, 1000.000000000000114 ) ;
#109147 = DIRECTION ( 'NONE',  ( 0.000000000000000000, 0.000000000000000000, -1.000000000000000000 ) ) ;
#109148 = EDGE_CURVE ( 'NONE', #8406, #70030, #95235, .T. ) ;
#109149 = CARTESIAN_POINT ( 'NONE',  ( -1.463139458404679960, 1452.861966431559949, 152.4924432263949825 ) ) ;
#109150 = CARTESIAN_POINT ( 'NONE',  ( -18.96325319869999859, 1416.831305841230005, 208.0005775078080035 ) ) ;
#109151 = EDGE_LOOP ( 'NONE', ( #106785, #49689, #12686, #95532 ) ) ;
#109152 = CARTESIAN_POINT ( 'NONE',  ( -2.500000000000000000, 1419.382958344190001, 144.1003752082409903 ) ) ;
#109153 = CARTESIAN_POINT ( 'NONE',  ( 4.823329535264199886E-05, 1409.206609320529878, 270.3713713915270205 ) ) ;
#109154 = CARTESIAN_POINT ( 'NONE',  ( 16.42440859496330319, 1423.292924526380148, 228.6634581238010071 ) ) ;
#109155 = CARTESIAN_POINT ( 'NONE',  ( 10.92766316885620093, 1501.618323021010156, 205.6861136770480130 ) ) ;
#109156 = EDGE_LOOP ( 'NONE', ( #90598, #90818, #46227, #53187 ) ) ;
#109157 = ORIENTED_EDGE ( 'NONE', *, *, #27042, .T. ) ;
#109158 = CARTESIAN_POINT ( 'NONE',  ( -62.46146343959999570, 1384.944962066419976, 249.2984044847590042 ) ) ;
#109159 = CARTESIAN_POINT ( 'NONE',  ( -23.59803273300959958, 1410.014125045500123, 208.9302168428020252 ) ) ;
#109160 = CARTESIAN_POINT ( 'NONE',  ( -3.903576985680000000, 1424.789296738229950, 185.8774067644979766 ) ) ;
#109161 = CARTESIAN_POINT ( 'NONE',  ( -0.4151546846821903003, 1512.187213306747481, 175.3106345060153046 ) ) ;
#109162 = CARTESIAN_POINT ( 'NONE',  ( -32.38845791999490586, 1518.913060387330006, 216.1254071228449902 ) ) ;
#109163 = CARTESIAN_POINT ( 'NONE',  ( -3.194354728630000029, 1498.350177541130051, 236.3803358245980064 ) ) ;
#109164 = CARTESIAN_POINT ( 'NONE',  ( 4.833436809398059530, 1508.551704408489968, 212.3463955241550138 ) ) ;
#109165 = ORIENTED_EDGE ( 'NONE', *, *, #74271, .T. ) ;
#109166 = CARTESIAN_POINT ( 'NONE',  ( 43.55151698956129991, 1452.829994745100066, 267.0610574176429850 ) ) ;
#109167 = CARTESIAN_POINT ( 'NONE',  ( -4.987080977031280504, 1508.551704408389924, 205.1632012944579913 ) ) ;
#109168 = CARTESIAN_POINT ( 'NONE',  ( -0.02483341509479999876, 1420.438468297229974, 183.3023409683979992 ) ) ;
#109169 = CARTESIAN_POINT ( 'NONE',  ( 4.028630584655000568, 1516.812923327049930, 205.6617440802170051 ) ) ;
#109170 = VERTEX_POINT ( 'NONE', #34774 ) ;
#109171 = CARTESIAN_POINT ( 'NONE',  ( 18.93983199967145126, 1457.591331553862574, 226.8224651722836995 ) ) ;
#109172 = CARTESIAN_POINT ( 'NONE',  ( 15.29936282157690108, 1512.951873711579992, 195.2879060687520223 ) ) ;
#109173 = AXIS2_PLACEMENT_3D ( 'NONE', #26939, #8462, #9569 ) ;
#109174 = CARTESIAN_POINT ( 'NONE',  ( 17.22533712008139872, 1431.108080386279880, 215.5140119622810175 ) ) ;
#109175 = EDGE_LOOP ( 'NONE', ( #78873, #97560, #93373, #76377 ) ) ;
#109176 = CARTESIAN_POINT ( 'NONE',  ( -10.68155123028649989, 1480.766592174720017, 209.7229870821389852 ) ) ;
#109177 = EDGE_CURVE ( 'NONE', #78889, #110373, #12247, .T. ) ;
#109178 = CARTESIAN_POINT ( 'NONE',  ( 26.89135176257029869, 1451.907621766309830, 135.4131197746179964 ) ) ;
#109179 = CARTESIAN_POINT ( 'NONE',  ( -14.49132061573049945, 1513.569700116999911, 194.0178397853109971 ) ) ;
#109180 = CARTESIAN_POINT ( 'NONE',  ( 9.991870921357078217, 1503.103680341759855, 217.0222761520359711 ) ) ;
#109181 = ADVANCED_FACE ( 'NONE', ( #52144 ), #9697, .T. ) ;
#109182 = CARTESIAN_POINT ( 'NONE',  ( 8.202111252990000878, 1421.417609776869767, 196.1188898363990063 ) ) ;
#109183 = CARTESIAN_POINT ( 'NONE',  ( 0.8357676597613630243, 1431.531542961990226, 218.5749032632120077 ) ) ;
#109184 = CARTESIAN_POINT ( 'NONE',  ( 10.02558921254980007, 1480.462737418800089, 205.8973177429729731 ) ) ;
#109185 = CARTESIAN_POINT ( 'NONE',  ( 1.871191615658170049, 1408.978403838410031, 186.8925371725070192 ) ) ;
#109187 = CARTESIAN_POINT ( 'NONE',  ( 29.86461515634920971, 1525.960063244517187, 220.9690070206020494 ) ) ;
#109186 = CARTESIAN_POINT ( 'NONE',  ( -13.79715687802010038, 1434.979310490669832, 148.5442485412900169 ) ) ;
#109188 = CARTESIAN_POINT ( 'NONE',  ( 10.67226526208479775, 1424.091373414049940, 206.6618934297929968 ) ) ;
#109189 = EDGE_CURVE ( 'NONE', #51052, #44714, #60263, .T. ) ;
#109190 = CARTESIAN_POINT ( 'NONE',  ( -12.82201593589999966, 1380.181586896640056, 214.4577599001689805 ) ) ;
#109191 = CARTESIAN_POINT ( 'NONE',  ( 3.005276066430000448, 1369.205039411269809, 207.6218459616989946 ) ) ;
#109192 = VERTEX_POINT ( 'NONE', #29129 ) ;
#109193 = CARTESIAN_POINT ( 'NONE',  ( 0.7266811465689989591, 1473.184386732089934, 216.5181915634790073 ) ) ;
#109194 = AXIS2_PLACEMENT_3D ( 'NONE', #43457, #33929, #77604 ) ;
#109195 = CARTESIAN_POINT ( 'NONE',  ( 10.79382269979189957, 1414.913060387349788, 222.1041130917409987 ) ) ;
#109196 = CARTESIAN_POINT ( 'NONE',  ( 3.552713678799999608E-15, 1415.677402202029953, 209.1218459616989946 ) ) ;
#109197 = EDGE_CURVE ( 'NONE', #8806, #14678, #34858, .T. ) ;
#109198 = CARTESIAN_POINT ( 'NONE',  ( -9.439187927669999922, 1387.430105989039930, 200.7363142262489930 ) ) ;
#109199 = CARTESIAN_POINT ( 'NONE',  ( 10.96051199111599850, 1427.774010562269950, 210.4713807161799934 ) ) ;
#109200 = CARTESIAN_POINT ( 'NONE',  ( 11.41161631220640160, 1425.396560188790090, 202.9572278001960228 ) ) ;
#109201 = CARTESIAN_POINT ( 'NONE',  ( -10.95711598477149806, 1462.675152724350028, 207.6879324179139985 ) ) ;
#109202 = CARTESIAN_POINT ( 'NONE',  ( 4.304798037349998904E-15, 1432.353341358199941, 150.3995506339979897 ) ) ;
#109203 = CARTESIAN_POINT ( 'NONE',  ( -9.046479669355809605, 1384.024798239620168, 218.5728259558869979 ) ) ;
#109204 = CARTESIAN_POINT ( 'NONE',  ( -12.39573405564623165, 1522.051704408389924, 199.6750929870061668 ) ) ;
#109205 = CARTESIAN_POINT ( 'NONE',  ( 28.02005514660000074, 1440.913060387330006, 248.0989693021979861 ) ) ;
#109206 = CARTESIAN_POINT ( 'NONE',  ( 13.15726442530000107, 1416.237488680629895, 196.4123356676979881 ) ) ;
#109207 = VECTOR ( 'NONE', #92985, 1000.000000000000114 ) ;
#109208 = CARTESIAN_POINT ( 'NONE',  ( -118.5497409066653773, 1305.913060387290216, 301.4085296778973202 ) ) ;
#109209 = CARTESIAN_POINT ( 'NONE',  ( -109.4150851273395091, 1387.231176170051413, 297.3550453227194339 ) ) ;
#109210 = CARTESIAN_POINT ( 'NONE',  ( 4.789658230336130806, 1465.867910918690086, 219.0701299224020033 ) ) ;
#109211 = CARTESIAN_POINT ( 'NONE',  ( -10.25237617670000034, 1481.942191864189908, 205.9184019755789734 ) ) ;
#109212 = CIRCLE ( 'NONE', #89532, 7.016581249619902039 ) ;
#109213 = CARTESIAN_POINT ( 'NONE',  ( 4.853172208638510732, 1474.073916305050034, 219.4636496197130100 ) ) ;
#109214 = CARTESIAN_POINT ( 'NONE',  ( -17.22268207119999772, 1410.011820319130038, 225.6635735971980239 ) ) ;
#109215 = ADVANCED_FACE ( 'NONE', ( #47590 ), #103567, .F. ) ;
#109216 = CARTESIAN_POINT ( 'NONE',  ( 23.55087209250000058, 1410.914164809929844, 211.6928269362679771 ) ) ;
#109217 = CARTESIAN_POINT ( 'NONE',  ( -17.31562880812650107, 1410.013633825039960, 192.7163598956479689 ) ) ;
#109218 = CARTESIAN_POINT ( 'NONE',  ( 0.7223987349950009573, 1515.137743094390089, 204.7943074541789770 ) ) ;
#109219 = CARTESIAN_POINT ( 'NONE',  ( -2.180465155517639531, 1524.667648926078755, 173.9851435850430335 ) ) ;
#109220 = DIRECTION ( 'NONE',  ( -0.9942586961433751425, 0.000000000000000000, 0.1070030146457376097 ) ) ;
#109221 = ADVANCED_FACE ( 'NONE', ( #71468 ), #12060, .F. ) ;
#109222 = CARTESIAN_POINT ( 'NONE',  ( -10.54743214440000010, 1416.216739748429973, 223.6935680435979918 ) ) ;
#109223 = CARTESIAN_POINT ( 'NONE',  ( 0.1907346795993619948, 1468.290221018919965, 182.5972501460889816 ) ) ;
#109225 = ORIENTED_EDGE ( 'NONE', *, *, #92721, .T. ) ;
#109224 = CARTESIAN_POINT ( 'NONE',  ( 9.905242068095489572, 1468.560492227489931, 207.6656469818879884 ) ) ;
#109226 = CARTESIAN_POINT ( 'NONE',  ( -23.84533141485470153, 1452.080363065020038, 136.9869391916130041 ) ) ;
#109227 = AXIS2_PLACEMENT_3D ( 'NONE', #7131, #59751, #110684 ) ;
#109228 = CARTESIAN_POINT ( 'NONE',  ( 34.18677586421189574, 1512.187213306747481, 219.7932833225211766 ) ) ;
#109229 = CARTESIAN_POINT ( 'NONE',  ( 17.68237282055029880, 1517.051704408389924, 212.5589510568480023 ) ) ;
#109230 = CARTESIAN_POINT ( 'NONE',  ( -41.34669637373799844, 1445.942886885710095, 134.0999999985539830 ) ) ;
#109231 = CARTESIAN_POINT ( 'NONE',  ( -110.0631564100000048, 1384.903609496989930, 296.9512625404590267 ) ) ;
#109232 = ORIENTED_EDGE ( 'NONE', *, *, #66618, .F. ) ;
#109233 = CARTESIAN_POINT ( 'NONE',  ( -1.227669779950000040, 1484.909253711390193, 198.3212086688990041 ) ) ;
#109234 = DIRECTION ( 'NONE',  ( -0.7074300732573280959, 0.02470400251971149874, 0.7063514732133270302 ) ) ;
#109235 = CARTESIAN_POINT ( 'NONE',  ( -108.6616353267809956, 1383.758284946439971, 311.0749865448200353 ) ) ;
#109236 = SPHERICAL_SURFACE ( 'NONE', #85633, 2.000000000000000000 ) ;
#109237 = CARTESIAN_POINT ( 'NONE',  ( -7.817296349952290946, 1435.611607423119949, 212.8323433814960026 ) ) ;
#109238 = CARTESIAN_POINT ( 'NONE',  ( 40.50350722682676263, 1425.156443366132180, 269.1155502198245131 ) ) ;
#109239 = CARTESIAN_POINT ( 'NONE',  ( -15.27521432969999893, 1416.121557574000008, 211.5121764755990057 ) ) ;
#109240 = CARTESIAN_POINT ( 'NONE',  ( -13.07882001760000179, 1380.090973434839952, 209.8378495415080067 ) ) ;
#109241 = DIRECTION ( 'NONE',  ( 0.000000000000000000, 8.545517954889998490E-18, 1.000000000000000000 ) ) ;
#109242 = CARTESIAN_POINT ( 'NONE',  ( -55.50096278363709956, 1385.040616669380142, 234.7978539123299981 ) ) ;
#109243 = CARTESIAN_POINT ( 'NONE',  ( -10.98637326466459996, 1391.913060387289988, 212.5523432083540172 ) ) ;
#109244 = CARTESIAN_POINT ( 'NONE',  ( 10.80336067484410023, 1425.743873502309953, 206.7465275332850183 ) ) ;
#109245 = ORIENTED_EDGE ( 'NONE', *, *, #25491, .F. ) ;
#109246 = CARTESIAN_POINT ( 'NONE',  ( -32.05911432779999615, 1450.505517766510138, 136.2999930999980052 ) ) ;
#109247 = CARTESIAN_POINT ( 'NONE',  ( -16.33521701716129826, 1410.862700950380031, 226.6351052317230028 ) ) ;
#109249 = ORIENTED_EDGE ( 'NONE', *, *, #48761, .F. ) ;
#109248 = CARTESIAN_POINT ( 'NONE',  ( 1.494261883209599739, 1437.570713977159812, 227.6107760732709835 ) ) ;
#109250 = CARTESIAN_POINT ( 'NONE',  ( 3.296903354329999480, 1473.033302177089809, 218.8000070911390083 ) ) ;
#109251 = CARTESIAN_POINT ( 'NONE',  ( 9.992887457760350145, 1469.445556547170099, 210.2216697196110147 ) ) ;
#109252 =( BOUNDED_CURVE ( )  B_SPLINE_CURVE ( 3, ( #9677, #61236, #8570, #25911 ),
 .UNSPECIFIED., .F., .F. ) 
 B_SPLINE_CURVE_WITH_KNOTS ( ( 4, 4 ),
 ( 1.005056174319898021, 2.136536482083220001 ),
 .UNSPECIFIED. ) 
 CURVE ( )  GEOMETRIC_REPRESENTATION_ITEM ( )  RATIONAL_B_SPLINE_CURVE ( ( 1.000000000000000000, 0.8961280526803196977, 0.8961280526803196977, 1.000000000000000000 ) ) 
 REPRESENTATION_ITEM ( '' )  );
#109253 = FACE_OUTER_BOUND ( 'NONE', #95088, .T. ) ;
#109254 = CARTESIAN_POINT ( 'NONE',  ( -109.4849127990000142, 1384.882923849199869, 311.2840631412590255 ) ) ;
#109255 = CARTESIAN_POINT ( 'NONE',  ( -11.20854081390000090, 1414.996444526030018, 195.7122653627979787 ) ) ;
#109256 = CARTESIAN_POINT ( 'NONE',  ( 23.20232703090000115, 1411.083540124029923, 212.8787804838979980 ) ) ;
#109257 = CARTESIAN_POINT ( 'NONE',  ( -113.4825880485180960, 1391.913060387289988, 307.7208714236175524 ) ) ;
#109258 = CARTESIAN_POINT ( 'NONE',  ( -16.00015186889999796, 1423.003814079930180, 228.7447940140980052 ) ) ;
#109259 = CARTESIAN_POINT ( 'NONE',  ( -5.130014241433883626, 1511.406470015445620, 200.5554185186313134 ) ) ;
#109260 = CARTESIAN_POINT ( 'NONE',  ( -14.01398736212220086, 1379.590348564800024, 211.9184487047760115 ) ) ;
#109261 = CARTESIAN_POINT ( 'NONE',  ( -105.2220350095120551, 1311.832804576489707, 308.6894887031868393 ) ) ;
#109262 = CARTESIAN_POINT ( 'NONE',  ( 3.487133837120000024, 1431.113060387329824, 227.6029907049980068 ) ) ;
#109263 = CARTESIAN_POINT ( 'NONE',  ( -0.2489806300479990020, 1456.626617263189928, 199.4885384397790062 ) ) ;
#109264 = CARTESIAN_POINT ( 'NONE',  ( 1.119439089684999944, 1517.026534522949987, 205.8528207963470038 ) ) ;
#109265 = CARTESIAN_POINT ( 'NONE',  ( 2.500000000000000000, 1448.229591938679960, 165.9681890900980079 ) ) ;
#109266 = VERTEX_POINT ( 'NONE', #18784 ) ;
#109267 = AXIS2_PLACEMENT_3D ( 'NONE', #23853, #98921, #65901 ) ;
#109268 = CARTESIAN_POINT ( 'NONE',  ( 16.87240902346729854, 1409.502257893559772, 222.1138755377239988 ) ) ;
#109269 = DIRECTION ( 'NONE',  ( 0.6670494068259388287, 0.5110419776299538475, 0.5421080943439499089 ) ) ;
#109271 = ORIENTED_EDGE ( 'NONE', *, *, #45240, .F. ) ;
#109270 = CARTESIAN_POINT ( 'NONE',  ( -68.61722315264249517, 1379.747600866859784, 280.2192988058840228 ) ) ;
#109272 = CARTESIAN_POINT ( 'NONE',  ( -18.26675480510339966, 1424.840341062940070, 227.6848255537819909 ) ) ;
#109273 = EDGE_LOOP ( 'NONE', ( #5391, #14233, #82414 ) ) ;
#109274 = CARTESIAN_POINT ( 'NONE',  ( -16.75056594176211533, 1513.749562442875913, 222.7143392581427008 ) ) ;
#109275 = CARTESIAN_POINT ( 'NONE',  ( 12.17354065289999987, 1500.378712179390050, 207.7715712704689963 ) ) ;
#109276 = B_SPLINE_CURVE_WITH_KNOTS ( 'NONE', 3,
 ( #57714, #48757, #91830, #91286 ),
 .UNSPECIFIED., .F., .F.,
 ( 4, 4 ),
 ( 0.000000000000000000, 0.003000049121573633397 ),
 .UNSPECIFIED. ) ;
#109278 = CARTESIAN_POINT ( 'NONE',  ( 15.93865550815479892, 1409.469629138669916, 193.0036447647779880 ) ) ;
#109277 = CARTESIAN_POINT ( 'NONE',  ( -11.41539857968949967, 1425.494006463380174, 142.6748587622950026 ) ) ;
#109279 = CARTESIAN_POINT ( 'NONE',  ( -4.026777524084999449, 1516.718889242609976, 211.4189316860469887 ) ) ;
#109280 = CIRCLE ( 'NONE', #61020, 1.000000000000002442 ) ;
#109281 = CARTESIAN_POINT ( 'NONE',  ( 39.08639746099999712, 1439.774711833670153, 136.7053848153979914 ) ) ;
#109282 = CARTESIAN_POINT ( 'NONE',  ( -11.73702549210000079, 1426.695992139529835, 144.1699184476980236 ) ) ;
#109283 = DIRECTION ( 'NONE',  ( 0.5877852522924709167, 0.000000000000000000, 0.8090169943749491166 ) ) ;
#109284 = CARTESIAN_POINT ( 'NONE',  ( 2.902343876856320115, 1466.632250330839952, 234.1422825383600070 ) ) ;
#109285 = CARTESIAN_POINT ( 'NONE',  ( 13.95592155805312906, 1416.839570625517808, 196.3344139125129857 ) ) ;
#109286 = CARTESIAN_POINT ( 'NONE',  ( -22.08622291482368283, 1518.913060387330006, 184.4183880513178337 ) ) ;
#109287 = ORIENTED_EDGE ( 'NONE', *, *, #23751, .T. ) ;
#109288 = CARTESIAN_POINT ( 'NONE',  ( -13.32684882476630150, 1469.522643478239843, 191.9925929742840083 ) ) ;
#109289 = CARTESIAN_POINT ( 'NONE',  ( 4.487249775049700240, 1509.038615934839981, 206.6339108193819811 ) ) ;
#109290 = ORIENTED_EDGE ( 'NONE', *, *, #30977, .F. ) ;
#109291 = EDGE_LOOP ( 'NONE', ( #22387, #26243, #60916, #90062 ) ) ;
#109292 = CARTESIAN_POINT ( 'NONE',  ( -29.75012120250000081, 1509.993914124430148, 208.5595671623779879 ) ) ;
#109293 = CARTESIAN_POINT ( 'NONE',  ( 10.52582308400029909, 1452.864387279470066, 210.3124659236350169 ) ) ;
#109294 = CIRCLE ( 'NONE', #37753, 1.999999999999999556 ) ;
#109295 = CARTESIAN_POINT ( 'NONE',  ( 0.1171482500689999956, 1451.168562942830249, 182.5358585629980155 ) ) ;
#109296 = CARTESIAN_POINT ( 'NONE',  ( -3.321445554160000313, 1484.261041720429830, 183.3707341603979728 ) ) ;
#109297 = DIRECTION ( 'NONE',  ( 0.000000000000000000, -1.000000000000000000, 0.000000000000000000 ) ) ;
#109298 = DIRECTION ( 'NONE',  ( -1.000000000000000000, 0.000000000000000000, 0.000000000000000000 ) ) ;
#109299 = CARTESIAN_POINT ( 'NONE',  ( -12.33566090380000091, 1378.557429905330082, 208.8728726537019895 ) ) ;
#109300 = CARTESIAN_POINT ( 'NONE',  ( 38.81202643689640297, 1436.797832322039994, 134.7402662745759869 ) ) ;
#109301 = CARTESIAN_POINT ( 'NONE',  ( 2.116101361519879820, 1421.168810873590019, 183.1883719185100006 ) ) ;
#109302 = CARTESIAN_POINT ( 'NONE',  ( 26.44808090420000113, 1439.564396612150176, 137.2471738511979993 ) ) ;
#109303 = CARTESIAN_POINT ( 'NONE',  ( -10.82294938829999964, 1391.816256682959875, 214.1756021292690093 ) ) ;
#109304 = CARTESIAN_POINT ( 'NONE',  ( -81.68753388954969807, 1384.802559585820063, 285.2219065580749771 ) ) ;
#109305 = ORIENTED_EDGE ( 'NONE', *, *, #38125, .F. ) ;
#109306 = CARTESIAN_POINT ( 'NONE',  ( -4.035490750684999739, 1516.630499592039996, 201.4102952541169884 ) ) ;
#109307 = CARTESIAN_POINT ( 'NONE',  ( -3.462835665494999660, 1517.038650117239968, 208.0021282158369900 ) ) ;
#109308 = ORIENTED_EDGE ( 'NONE', *, *, #47446, .T. ) ;
#109309 = DIRECTION ( 'NONE',  ( -1.755985294532469921E-16, 1.000000000000000000, -1.338183447452831989E-16 ) ) ;
#109310 = AXIS2_PLACEMENT_3D ( 'NONE', #102166, #93751, #78641 ) ;
#109311 = CARTESIAN_POINT ( 'NONE',  ( 4.607425546304328989, 1511.399183828327523, 217.5145368139657478 ) ) ;
#109312 = ORIENTED_EDGE ( 'NONE', *, *, #13962, .F. ) ;
#109313 = CARTESIAN_POINT ( 'NONE',  ( -13.29661090509999966, 1415.048591087029763, 220.6690200173979974 ) ) ;
#109314 = EDGE_CURVE ( 'NONE', #34791, #81429, #52351, .T. ) ;
#109315 = CARTESIAN_POINT ( 'NONE',  ( -11.72314552038290003, 1432.337468424269900, 150.7717712668979857 ) ) ;
#109316 = CARTESIAN_POINT ( 'NONE',  ( -0.7950258152958181723, 1426.814114633998997, 137.0999999982234385 ) ) ;
#109317 = AXIS2_PLACEMENT_3D ( 'NONE', #68054, #57450, #75346 ) ;
#109318 = CARTESIAN_POINT ( 'NONE',  ( -9.301208406426139774, 1461.161189386590195, 206.3998599881980169 ) ) ;
#109319 = CARTESIAN_POINT ( 'NONE',  ( -12.99738333980000071, 1429.131617844829861, 222.4366461256979903 ) ) ;
#109320 = CARTESIAN_POINT ( 'NONE',  ( 9.916409037356570977, 1468.767901124550008, 207.5969806327450158 ) ) ;
#109321 = CARTESIAN_POINT ( 'NONE',  ( -2.130922739038390024, 1467.954349360780043, 220.0452206896550251 ) ) ;
#109322 = CARTESIAN_POINT ( 'NONE',  ( -14.20380459391698302, 1410.782058423236776, 190.3118870790858637 ) ) ;
#109323 = CARTESIAN_POINT ( 'NONE',  ( -15.22920806200000143, 1462.589963187330113, 223.3216945802979865 ) ) ;
#109325 = CARTESIAN_POINT ( 'NONE',  ( 2.487935141041626164, 1508.731359867455012, 213.6768079671783198 ) ) ;
#109324 = CARTESIAN_POINT ( 'NONE',  ( 16.63395562619999879, 1459.015801707430001, 231.1847121254979811 ) ) ;
#109326 = CARTESIAN_POINT ( 'NONE',  ( -4.958647264046995851, 1422.537331718762516, 184.8308287925253524 ) ) ;
#109327 = CARTESIAN_POINT ( 'NONE',  ( -3.453544863754999472, 1517.106845464700200, 216.4586906126469898 ) ) ;
#109328 = ORIENTED_EDGE ( 'NONE', *, *, #110238, .F. ) ;
#109329 = AXIS2_PLACEMENT_3D ( 'NONE', #78894, #79437, #86720 ) ;
#109330 = CARTESIAN_POINT ( 'NONE',  ( -22.70988283845126787, 1409.706100392974804, 208.9686675985246325 ) ) ;
#109331 = DIRECTION ( 'NONE',  ( -0.000000000000000000, -1.000000000000000000, -0.000000000000000000 ) ) ;
#109332 = EDGE_CURVE ( 'NONE', #10122, #55469, #17585, .T. ) ;
#109333 = CARTESIAN_POINT ( 'NONE',  ( 5.008848199894999631, 1516.858456333729919, 214.1219297979669989 ) ) ;
#109334 = CARTESIAN_POINT ( 'NONE',  ( 3.465053098240360008, 1515.493282983300105, 213.0346220849250187 ) ) ;
#109335 = CARTESIAN_POINT ( 'NONE',  ( 0.000000000000000000, 1511.187213306747708, 209.1218459616979999 ) ) ;
#109336 = B_SPLINE_CURVE_WITH_KNOTS ( 'NONE', 3,
 ( #24946, #13935, #47566, #16540 ),
 .UNSPECIFIED., .F., .F.,
 ( 4, 4 ),
 ( -20.28790011219829736, -6.722899290939999162 ),
 .UNSPECIFIED. ) ;
#109338 = ORIENTED_EDGE ( 'NONE', *, *, #29311, .T. ) ;
#109337 = CARTESIAN_POINT ( 'NONE',  ( 4.987078416403489811, 1508.551704408389924, 212.6094303565780024 ) ) ;
#109339 = CARTESIAN_POINT ( 'NONE',  ( 1.119642440080000023, 1434.994542537360076, 189.3593017752980074 ) ) ;
#109340 = DIRECTION ( 'NONE',  ( 1.000000000000000000, 0.000000000000000000, 0.000000000000000000 ) ) ;
#109341 = ADVANCED_FACE ( 'NONE', ( #255 ), #69647, .T. ) ;
#109342 = CARTESIAN_POINT ( 'NONE',  ( -11.86543074620000127, 1432.295683013649978, 150.3972177407979984 ) ) ;
#109343 = CARTESIAN_POINT ( 'NONE',  ( 1.984413551915469975, 1522.051704408389924, 198.9129232538419956 ) ) ;
#109344 = CARTESIAN_POINT ( 'NONE',  ( -5.494590086983840216, 1440.608783345210213, 202.1972241445429859 ) ) ;
#109345 = CARTESIAN_POINT ( 'NONE',  ( 3.134082760970000159, 1421.411057458130017, 144.1516174827979739 ) ) ;
#109346 = CARTESIAN_POINT ( 'NONE',  ( -7.177114193734159819, 1426.187286780010027, 203.1778547286869809 ) ) ;
#109347 = CARTESIAN_POINT ( 'NONE',  ( 4.367506823990000342, 1410.393541147229826, 231.4170693631980100 ) ) ;
#109349 = CARTESIAN_POINT ( 'NONE',  ( -6.061273928713842629, 1422.611328064380359, 137.0999999980751340 ) ) ;
#109348 = CARTESIAN_POINT ( 'NONE',  ( -23.05235012189999821, 1482.723166241629997, 221.7956923970979801 ) ) ;
#109350 = CARTESIAN_POINT ( 'NONE',  ( -28.77730030020000029, 1509.917985857730173, 212.2396942135479776 ) ) ;
#109351 = ORIENTED_EDGE ( 'NONE', *, *, #65192, .T. ) ;
#109352 = CARTESIAN_POINT ( 'NONE',  ( 6.934528529765000116, 1516.588006113850042, 206.2478870805069846 ) ) ;
#109353 = CARTESIAN_POINT ( 'NONE',  ( 4.952595917969999206, 1406.456499948729970, 269.2856872263980108 ) ) ;
#109354 = COLOUR_RGB ( '', 0.66274510, 0.83137255, 0.94901961) ;
#109355 = CARTESIAN_POINT ( 'NONE',  ( -32.38845791999490586, 1523.382868172864164, 216.1254071228449902 ) ) ;
#109356 = CARTESIAN_POINT ( 'NONE',  ( 21.09738187590000180, 1410.867002981430005, 200.0903158484080109 ) ) ;
#109357 = DIRECTION ( 'NONE',  ( 0.9858563016761853204, 0.000000000000000000, 0.1675928174038331386 ) ) ;
#109358 = CARTESIAN_POINT ( 'NONE',  ( -9.835648583419363433, 1390.019383093769193, 216.6175827202515336 ) ) ;
#109359 = LINE ( 'NONE', #23675, #93310 ) ;
#109361 = ADVANCED_FACE ( 'NONE', ( #73517 ), #57278, .F. ) ;
#109360 = CIRCLE ( 'NONE', #61106, 6.500000000000000000 ) ;
#109362 = DIRECTION ( 'NONE',  ( -0.9455185755993178454, 0.000000000000000000, 0.3255681544571537578 ) ) ;
#109363 = CARTESIAN_POINT ( 'NONE',  ( -15.13370552100000133, 1417.513322374810059, 204.2902361586989741 ) ) ;
#109364 = CARTESIAN_POINT ( 'NONE',  ( -13.79526254970000032, 1445.853624484049760, 188.3960237689979920 ) ) ;
#109365 = DIRECTION ( 'NONE',  ( 0.9396491905462577288, 0.3023466567524009108, 0.1601433665701099407 ) ) ;
#109366 = CARTESIAN_POINT ( 'NONE',  ( -8.645398683972508991, 1437.369593462749890, 208.8432647735320131 ) ) ;
#109367 = CARTESIAN_POINT ( 'NONE',  ( 3.196891693280000002, 1407.733286134229957, 270.1354749225980072 ) ) ;
#109368 = CARTESIAN_POINT ( 'NONE',  ( 0.3811431543340009775, 1478.039055931090161, 201.4703185268089953 ) ) ;
#109369 = FACE_OUTER_BOUND ( 'NONE', #16658, .T. ) ;
#109370 = CARTESIAN_POINT ( 'NONE',  ( 11.02941167081014484, 1424.908287015548240, 138.1869667496993088 ) ) ;
#109371 = CARTESIAN_POINT ( 'NONE',  ( 21.76695791008653558, 1524.152349020271004, 234.8391556417741697 ) ) ;
#109372 = VECTOR ( 'NONE', #33193, 1000.000000000000114 ) ;
#109373 = CARTESIAN_POINT ( 'NONE',  ( -2.778684086150000176, 1476.048032409329835, 267.8507713580979726 ) ) ;
#109374 = CARTESIAN_POINT ( 'NONE',  ( -4.222051551403209757, 1446.225887192099890, 170.2164200388130268 ) ) ;
#109375 = CARTESIAN_POINT ( 'NONE',  ( -12.99081176452876285, 1513.436191188001885, 192.3341863405429990 ) ) ;
#109376 = CARTESIAN_POINT ( 'NONE',  ( 32.02808312589916540, 1511.187213306747708, 197.2787714533495489 ) ) ;
#109377 = CARTESIAN_POINT ( 'NONE',  ( -43.14089593232999675, 1384.773049472099956, 247.9047009284290084 ) ) ;
#109378 = CARTESIAN_POINT ( 'NONE',  ( -30.61619818474167687, 1525.211477436245787, 221.5983981500683058 ) ) ;
#109379 = CARTESIAN_POINT ( 'NONE',  ( -6.655787406570000009, 1441.606255579999925, 154.8401361813980088 ) ) ;
#109380 = CARTESIAN_POINT ( 'NONE',  ( 19.63722818192610120, 1519.551704408389924, 218.2362632616380154 ) ) ;
#109381 = CARTESIAN_POINT ( 'NONE',  ( 4.226426730299999157, 1515.477082009390188, 209.1218459616989946 ) ) ;
#109382 = CARTESIAN_POINT ( 'NONE',  ( -45.63712966311000230, 1440.913059426480004, 268.9747523979869470 ) ) ;
#109383 = CARTESIAN_POINT ( 'NONE',  ( -21.36941021309999655, 1409.659296635530154, 204.4057705028979797 ) ) ;
#109384 = CARTESIAN_POINT ( 'NONE',  ( -10.94870340160153965, 1379.126484780772671, 203.4065785939058060 ) ) ;
#109385 = CARTESIAN_POINT ( 'NONE',  ( -15.97531815300800062, 1420.724455713108000, 227.0315652133519961 ) ) ;
#109386 = CARTESIAN_POINT ( 'NONE',  ( 10.17851409671319907, 1480.182533543850013, 206.4481411506540098 ) ) ;
#109387 = ORIENTED_EDGE ( 'NONE', *, *, #14089, .T. ) ;
#109388 = CARTESIAN_POINT ( 'NONE',  ( -2.234923082067399758, 1512.341036938790012, 201.5226187867249905 ) ) ;
#109389 = CARTESIAN_POINT ( 'NONE',  ( -19.86686180190000073, 1444.169376520590049, 213.3106045261990005 ) ) ;
#109390 = CARTESIAN_POINT ( 'NONE',  ( -7.459190136973458785, 1510.844697586386246, 215.3093670277948775 ) ) ;
#109391 = CARTESIAN_POINT ( 'NONE',  ( 20.75865325816559803, 1455.056399775050068, 207.3304373731819794 ) ) ;
#109392 =( BOUNDED_CURVE ( )  B_SPLINE_CURVE ( 3, ( #9312, #61952, #79837, #43474 ),
 .UNSPECIFIED., .F., .T. ) 
 B_SPLINE_CURVE_WITH_KNOTS ( ( 4, 4 ),
 ( 4.042232613224455484, 4.145962736327015286 ),
 .UNSPECIFIED. ) 
 CURVE ( )  GEOMETRIC_REPRESENTATION_ITEM ( )  RATIONAL_B_SPLINE_CURVE ( ( 1.000000000000000000, 0.9991035394458830377, 0.9991035394458830377, 1.000000000000000000 ) ) 
 REPRESENTATION_ITEM ( '' )  );
#109394 = CARTESIAN_POINT ( 'NONE',  ( -15.02579306586500074, 1513.907445464720013, 193.7166317783670024 ) ) ;
#109393 = DIRECTION ( 'NONE',  ( -0.000000000000000000, -1.000000000000000000, -0.000000000000000000 ) ) ;
#109395 = CARTESIAN_POINT ( 'NONE',  ( 16.48227125551174765, 1525.651285554128663, 236.6829039301441924 ) ) ;
#109396 = CARTESIAN_POINT ( 'NONE',  ( 3.829620113550000315, 1515.051704408389924, 209.0973262533439936 ) ) ;
#109397 = CARTESIAN_POINT ( 'NONE',  ( -8.044397765300001168, 1452.253295118390042, 204.1782792353590139 ) ) ;
#109398 = LINE ( 'NONE', #8564, #14437 ) ;
#109399 = CARTESIAN_POINT ( 'NONE',  ( -0.01171164408179850049, 1516.939568781210028, 202.5649949355269825 ) ) ;
#109400 = DIRECTION ( 'NONE',  ( -1.000000000000000000, 0.000000000000000000, -1.254859372443971704E-14 ) ) ;
#109401 = CARTESIAN_POINT ( 'NONE',  ( -11.68471933269640672, 1398.259520849452201, 203.4197633266676633 ) ) ;
#109402 = CARTESIAN_POINT ( 'NONE',  ( 15.99263752353499690, 1514.225267046429963, 194.0679338807670149 ) ) ;
#109403 = CARTESIAN_POINT ( 'NONE',  ( -17.55845490061370029, 1419.966211264809999, 204.6173968078139751 ) ) ;
#109404 = CARTESIAN_POINT ( 'NONE',  ( -18.16996689059999781, 1377.005697473339978, 212.7263676204689773 ) ) ;
#109405 = CARTESIAN_POINT ( 'NONE',  ( 19.89552987158740294, 1507.835503131050018, 229.1917664541709883 ) ) ;
#109407 = ORIENTED_EDGE ( 'NONE', *, *, #81894, .F. ) ;
#109406 = CARTESIAN_POINT ( 'NONE',  ( -40.54664627463470339, 1379.659233182239859, 229.3558487376700157 ) ) ;
#109408 = EDGE_LOOP ( 'NONE', ( #24101, #58313, #69934, #1064 ) ) ;
#109409 = CARTESIAN_POINT ( 'NONE',  ( 12.00417144290479854, 1433.690309434259916, 149.9471367831160080 ) ) ;
#109410 = CARTESIAN_POINT ( 'NONE',  ( -12.84602301340000174, 1397.681121324029846, 211.4929570555379996 ) ) ;
#109411 = CARTESIAN_POINT ( 'NONE',  ( -20.70585539609999870, 1409.636124800530069, 216.1314882506880224 ) ) ;
#109412 = VERTEX_POINT ( 'NONE', #89744 ) ;
#109413 = CARTESIAN_POINT ( 'NONE',  ( -13.13987858127485531, 1444.766776377808810, 169.3999092927280117 ) ) ;
#109414 = FACE_OUTER_BOUND ( 'NONE', #53624, .T. ) ;
#109415 = CARTESIAN_POINT ( 'NONE',  ( 3.778540308873199915, 1515.551842517600107, 205.7532741663330000 ) ) ;
#109417 = CARTESIAN_POINT ( 'NONE',  ( -14.04733786781709881, 1509.155471822469963, 183.5477982220859872 ) ) ;
#109416 = CARTESIAN_POINT ( 'NONE',  ( 3.601839739459999912, 1444.840594719589944, 200.9001243581789993 ) ) ;
#109418 = CARTESIAN_POINT ( 'NONE',  ( 1.819731560309999940, 1449.239545743680083, 183.7033410088979792 ) ) ;
#109419 = CARTESIAN_POINT ( 'NONE',  ( -5.208614297041160413, 1464.433914205869996, 199.4042851730860093 ) ) ;
#109420 = DIRECTION ( 'NONE',  ( 0.7074300732573259864, -0.02470400251981139106, 0.7063514732133259200 ) ) ;
#109421 = CARTESIAN_POINT ( 'NONE',  ( 6.882111520678369843, 1396.153389082980084, 200.4809898212910184 ) ) ;
#109422 = CARTESIAN_POINT ( 'NONE',  ( 2.500000000000000000, 1419.493307454862588, 138.7644438434529377 ) ) ;
#109423 = CARTESIAN_POINT ( 'NONE',  ( 11.86496431830000020, 1432.256597482460165, 149.9819972498980007 ) ) ;
#109424 = CARTESIAN_POINT ( 'NONE',  ( 5.674678682617919634, 1509.116656018666845, 180.2329421256601449 ) ) ;
#109425 = ORIENTED_EDGE ( 'NONE', *, *, #23434, .T. ) ;
#109426 = CARTESIAN_POINT ( 'NONE',  ( 13.06728979724060125, 1434.812079778950192, 149.1114618806330157 ) ) ;
#109427 = VERTEX_POINT ( 'NONE', #30384 ) ;
#109428 = VERTEX_POINT ( 'NONE', #72418 ) ;
#109429 = CARTESIAN_POINT ( 'NONE',  ( 13.49167004114784163, 1444.154101332126402, 169.3566519967024533 ) ) ;
#109430 = CARTESIAN_POINT ( 'NONE',  ( -13.14000772899999880, 1461.232465199529770, 232.8227670808980179 ) ) ;
#109431 = CARTESIAN_POINT ( 'NONE',  ( -107.7563153173368704, 1389.383687039567803, 309.7269953625564085 ) ) ;
#109432 = CARTESIAN_POINT ( 'NONE',  ( 0.01126491619350150110, 1516.939530130779985, 216.0663127125970107 ) ) ;
#109433 = CARTESIAN_POINT ( 'NONE',  ( -8.071183553683329848, 1511.586636681201526, 212.7277961325115143 ) ) ;
#109434 = ORIENTED_EDGE ( 'NONE', *, *, #89772, .T. ) ;
#109435 = CARTESIAN_POINT ( 'NONE',  ( -12.20495830810000015, 1503.566102511789950, 208.5052324830940051 ) ) ;
#109436 = CARTESIAN_POINT ( 'NONE',  ( -1.804213505890000180, 1410.351307731129964, 186.0507930254979954 ) ) ;
#109437 = CARTESIAN_POINT ( 'NONE',  ( -19.16011841990000164, 1375.603804398499960, 208.8610751811249884 ) ) ;
#109438 = VERTEX_POINT ( 'NONE', #13017 ) ;
#109439 = CARTESIAN_POINT ( 'NONE',  ( -5.011678876155000850, 1516.989560013210166, 205.8658785457569991 ) ) ;
#109440 = VERTEX_POINT ( 'NONE', #48313 ) ;
#109441 = CARTESIAN_POINT ( 'NONE',  ( 7.724874613184999461, 1517.139320148880188, 209.8621665372610039 ) ) ;
#109442 = CARTESIAN_POINT ( 'NONE',  ( -7.846715645779529069, 1452.866283417570003, 204.0807684293459943 ) ) ;
#109443 = CARTESIAN_POINT ( 'NONE',  ( -11.00811277969999935, 1409.800196935129861, 189.0350722840979927 ) ) ;
#109444 = CARTESIAN_POINT ( 'NONE',  ( 6.560424596724999446, 1512.053281741910041, 217.7862930670369792 ) ) ;
#109446 = VERTEX_POINT ( 'NONE', #47203 ) ;
#109445 = CARTESIAN_POINT ( 'NONE',  ( 0.1956065449380390009, 1414.913060387399810, 225.1861166566439749 ) ) ;
#109447 = CARTESIAN_POINT ( 'NONE',  ( 22.49274844409999830, 1431.770720225350033, 217.6924115464580041 ) ) ;
#109448 = CARTESIAN_POINT ( 'NONE',  ( -5.311724842150000292, 1500.891271500089942, 229.7588813323989996 ) ) ;
#109449 = CARTESIAN_POINT ( 'NONE',  ( -59.23371022229999738, 1384.698177673139980, 279.9261678725590059 ) ) ;
#109450 = CARTESIAN_POINT ( 'NONE',  ( 20.83491851400000172, 1494.467306230789973, 206.1460450736289829 ) ) ;
#109451 = CIRCLE ( 'NONE', #66543, 5.499916801759985319 ) ;
#109452 = CARTESIAN_POINT ( 'NONE',  ( 5.319674812860000657, 1408.795128090730032, 270.4258975186979796 ) ) ;
#109453 = CARTESIAN_POINT ( 'NONE',  ( 6.559798056295000457, 1516.987478262539980, 213.7368632980669929 ) ) ;
#109454 = CARTESIAN_POINT ( 'NONE',  ( 24.14539179490000365, 1411.115351439130109, 209.1808261004410099 ) ) ;
#109455 = CARTESIAN_POINT ( 'NONE',  ( -20.61546995289999984, 1508.365016819430139, 190.3615313974979983 ) ) ;
#109456 = CARTESIAN_POINT ( 'NONE',  ( 12.07459970771560087, 1492.710845711899992, 211.7408674243640121 ) ) ;
#109457 = CARTESIAN_POINT ( 'NONE',  ( -3.827327156165859723, 1424.046157831530081, 184.1455916618039907 ) ) ;
#109458 = CARTESIAN_POINT ( 'NONE',  ( 0.01012488564660149991, 1516.989863902050047, 210.2497743036369968 ) ) ;
#109459 = CARTESIAN_POINT ( 'NONE',  ( -2.738674389556827293, 1448.013728860840047, 154.7582013136732542 ) ) ;
#109460 = CARTESIAN_POINT ( 'NONE',  ( 0.2110708091519999940, 1420.488442819130114, 182.7547195189980016 ) ) ;
#109461 = CARTESIAN_POINT ( 'NONE',  ( 1.355725611670679509, 1410.152069949700717, 232.6326878827337339 ) ) ;
#109463 = EDGE_LOOP ( 'NONE', ( #89904, #49541, #12275, #31168 ) ) ;
#109462 = CARTESIAN_POINT ( 'NONE',  ( -65.92084310709999784, 1389.515675200419764, 264.7571888138589316 ) ) ;
#109465 = AXIS2_PLACEMENT_3D ( 'NONE', #54276, #95699, #62689 ) ;
#109464 = CARTESIAN_POINT ( 'NONE',  ( -44.14048389105859371, 1385.157692499700033, 249.8217694268669788 ) ) ;
#109466 = CARTESIAN_POINT ( 'NONE',  ( 18.64646854140000087, 1416.843576337130116, 209.6840263561229847 ) ) ;
#109467 = CARTESIAN_POINT ( 'NONE',  ( -3.347801439296150150, 1523.382868172864164, 242.0893193391992497 ) ) ;
#109468 = FACE_OUTER_BOUND ( 'NONE', #89964, .T. ) ;
#109469 = CARTESIAN_POINT ( 'NONE',  ( -5.468507174450000896, 1438.698907215800091, 154.7381958892980265 ) ) ;
#109470 = CARTESIAN_POINT ( 'NONE',  ( -22.74837831800000032, 1450.248907260850046, 218.8546552101780094 ) ) ;
#109471 = CARTESIAN_POINT ( 'NONE',  ( 11.12931921223499998, 1512.151624459629829, 224.9062103328670048 ) ) ;
#109473 = CARTESIAN_POINT ( 'NONE',  ( -8.297292677819999795, 1384.885217424269740, 218.7035352472190084 ) ) ;
#109472 = CARTESIAN_POINT ( 'NONE',  ( -3.454172653555000139, 1517.122088787240045, 216.8462693643270143 ) ) ;
#109474 = CARTESIAN_POINT ( 'NONE',  ( -9.521726183726670456, 1448.210812606100035, 209.8762788027680131 ) ) ;
#109475 = CARTESIAN_POINT ( 'NONE',  ( 11.13055623967079377, 1375.886883438980021, 203.9732913815154234 ) ) ;
#109476 = ORIENTED_EDGE ( 'NONE', *, *, #13717, .T. ) ;
#109477 = CARTESIAN_POINT ( 'NONE',  ( 1.124289655455000148, 1517.184063036290127, 202.5579304082170040 ) ) ;
#109478 = CIRCLE ( 'NONE', #93390, 12.38732017200242019 ) ;
#109479 = CARTESIAN_POINT ( 'NONE',  ( -0.04719682667970000189, 1477.415580660429896, 229.9352398341980006 ) ) ;
#109480 = CARTESIAN_POINT ( 'NONE',  ( 20.40554580410000085, 1454.562377498930118, 223.2165941418979855 ) ) ;
#109481 = CARTESIAN_POINT ( 'NONE',  ( 7.129538283582470548, 1439.009953491013448, 154.1072895365704767 ) ) ;
#109482 = CARTESIAN_POINT ( 'NONE',  ( -4.649632279085039954, 1420.176633138330089, 186.4708453798239987 ) ) ;
#109483 = CARTESIAN_POINT ( 'NONE',  ( 4.380514181050000566, 1467.321765115789958, 218.0672140897789859 ) ) ;
#109484 = CARTESIAN_POINT ( 'NONE',  ( 15.29810743031686116, 1420.788480698754483, 227.8099671849163599 ) ) ;
#109485 = CARTESIAN_POINT ( 'NONE',  ( 30.86131756593869824, 1435.574936792159860, 135.5979777996759879 ) ) ;
#109486 = CARTESIAN_POINT ( 'NONE',  ( -106.1567580175403265, 1391.062840735999316, 301.1121656807407021 ) ) ;
#109487 = CARTESIAN_POINT ( 'NONE',  ( -22.59076341920000175, 1432.096319160770008, 217.4686915984279949 ) ) ;
#109488 = CARTESIAN_POINT ( 'NONE',  ( -3.415174198469128619, 1451.477971282471344, 184.8447311170799594 ) ) ;
#109489 = CARTESIAN_POINT ( 'NONE',  ( -1.441213829320000084, 1430.262570393590067, 200.5314639573489899 ) ) ;
#109490 = CARTESIAN_POINT ( 'NONE',  ( -15.82983165089999922, 1415.825112219430139, 226.8803080324979931 ) ) ;
#109491 = CARTESIAN_POINT ( 'NONE',  ( 19.39983987835422496, 1501.977400791986611, 239.2921289694223219 ) ) ;
#109492 = DIRECTION ( 'NONE',  ( 0.000000000000000000, 0.000000000000000000, 1.000000000000000000 ) ) ;
#109493 = ORIENTED_EDGE ( 'NONE', *, *, #63363, .T. ) ;
#109494 = DIRECTION ( 'NONE',  ( 0.000000000000000000, 1.000000000000000000, 0.000000000000000000 ) ) ;
#109495 = CARTESIAN_POINT ( 'NONE',  ( 1.514738106409309948, 1507.606285602550088, 186.2052147526660235 ) ) ;
#109496 = EDGE_CURVE ( 'NONE', #100644, #50057, #39484, .T. ) ;
#109497 = DIRECTION ( 'NONE',  ( 0.9455185755993178454, 0.000000000000000000, -0.3255681544571537578 ) ) ;
#109498 = CARTESIAN_POINT ( 'NONE',  ( 11.12031993019763121, 1427.725797866641187, 210.2198567556694684 ) ) ;
#109499 = CARTESIAN_POINT ( 'NONE',  ( 11.60004869885203682, 1428.513469990230988, 134.1600495453299402 ) ) ;
#109500 = CARTESIAN_POINT ( 'NONE',  ( -12.94242690632408710, 1444.911164871706660, 186.2050248885010433 ) ) ;
#109501 = DIRECTION ( 'NONE',  ( -0.5161917810414702323, 0.8564730265368752926, 0.000000000000000000 ) ) ;
#109502 = CARTESIAN_POINT ( 'NONE',  ( -2.329898369990449858, 1515.064791341159889, 213.4512947646889813 ) ) ;
#109503 = CARTESIAN_POINT ( 'NONE',  ( -6.462952837710792764, 1416.600481159538049, 231.5900835776368183 ) ) ;
#109504 = CARTESIAN_POINT ( 'NONE',  ( -20.69862370072165447, 1450.958657178972317, 144.8102315378076526 ) ) ;
#109505 = CARTESIAN_POINT ( 'NONE',  ( 25.56060455230000272, 1435.581316386610069, 136.3167502477979838 ) ) ;
#109506 = CARTESIAN_POINT ( 'NONE',  ( -12.95247382709503547, 1442.920873375600650, 169.4286589542791432 ) ) ;
#109508 = ORIENTED_EDGE ( 'NONE', *, *, #65823, .T. ) ;
#109507 = CARTESIAN_POINT ( 'NONE',  ( -13.86092848849999903, 1410.765486861730096, 227.1170286483979908 ) ) ;
#109509 = CARTESIAN_POINT ( 'NONE',  ( 1.032249311045119855, 1415.090956648730071, 191.5469134311629773 ) ) ;
#109510 = CARTESIAN_POINT ( 'NONE',  ( 21.47555099491460595, 1509.121809344517942, 226.4561570876979317 ) ) ;
#109511 = VERTEX_POINT ( 'NONE', #30935 ) ;
#109512 = VERTEX_POINT ( 'NONE', #82997 ) ;
#109513 = CARTESIAN_POINT ( 'NONE',  ( 33.36586802512179162, 1511.187213306747708, 216.3367586934468818 ) ) ;
#109514 = CARTESIAN_POINT ( 'NONE',  ( -18.66420869458028520, 1526.382868172864164, 232.7837831374281166 ) ) ;
#109516 = CARTESIAN_POINT ( 'NONE',  ( -25.90364837339999937, 1446.091283352949858, 225.2740410894980130 ) ) ;
#109515 = CARTESIAN_POINT ( 'NONE',  ( -11.74015320060000001, 1428.979986575930070, 144.1938086916980239 ) ) ;
#109517 = CARTESIAN_POINT ( 'NONE',  ( -4.989228071470000359, 1445.489057496590249, 216.9515723730989976 ) ) ;
#109518 = CARTESIAN_POINT ( 'NONE',  ( -11.84754656309999987, 1433.385444766480077, 150.5314318111979901 ) ) ;
#109519 = CARTESIAN_POINT ( 'NONE',  ( -12.30515845580959855, 1378.366303543320100, 209.8813026182200190 ) ) ;
#109520 = CARTESIAN_POINT ( 'NONE',  ( 9.688259743311579797, 1463.788314065760233, 210.6196158358079913 ) ) ;
#109521 = CARTESIAN_POINT ( 'NONE',  ( 7.089203542179999928, 1424.901038349889859, 213.0569889132190156 ) ) ;
#109522 = CARTESIAN_POINT ( 'NONE',  ( -24.86519793529999944, 1440.000684534039920, 210.4205762286579784 ) ) ;
#109523 = FACE_BOUND ( 'NONE', #45126, .T. ) ;
#109524 = CARTESIAN_POINT ( 'NONE',  ( 1.245430209930000087, 1451.852423490530100, 183.2837323295979957 ) ) ;
#109525 = CARTESIAN_POINT ( 'NONE',  ( 7.285242456129513045, 1363.166718125769876, 210.6218459617142003 ) ) ;
#109526 = CARTESIAN_POINT ( 'NONE',  ( -26.22910734341959227, 1509.942088455394014, 194.4759448834997215 ) ) ;
#109528 = ORIENTED_EDGE ( 'NONE', *, *, #69348, .F. ) ;
#109527 = CARTESIAN_POINT ( 'NONE',  ( -1.401184754297550056E-09, 1416.469379747089988, 239.0597315746249762 ) ) ;
#109529 = ORIENTED_EDGE ( 'NONE', *, *, #32373, .F. ) ;
#109530 = CARTESIAN_POINT ( 'NONE',  ( -11.79634470412839953, 1428.064288700699990, 147.9921703239390069 ) ) ;
#109531 = EDGE_CURVE ( 'NONE', #46077, #53580, #74938, .T. ) ;
#109532 = EDGE_CURVE ( 'NONE', #67527, #105623, #72377, .T. ) ;
#109533 = CARTESIAN_POINT ( 'NONE',  ( -13.61181236409999862, 1504.842419174190127, 227.7680708624989734 ) ) ;
#109534 = CARTESIAN_POINT ( 'NONE',  ( -6.330345537219999486, 1472.287844838930141, 270.3701849726979844 ) ) ;
#109535 = CARTESIAN_POINT ( 'NONE',  ( -114.5985638465105154, 1391.413060387289988, 306.4158023619849018 ) ) ;
#109536 = CARTESIAN_POINT ( 'NONE',  ( -102.9430107027584285, 1368.558218059088631, 309.9345252466023908 ) ) ;
#109537 = CARTESIAN_POINT ( 'NONE',  ( 41.60492629830280720, 1445.157100822329994, 135.9429468860429893 ) ) ;
#109539 = EDGE_CURVE ( 'NONE', #57941, #43234, #88220, .T. ) ;
#109538 = CARTESIAN_POINT ( 'NONE',  ( 18.48114474329999979, 1431.113060387329824, 205.6347121245780158 ) ) ;
#109540 = CARTESIAN_POINT ( 'NONE',  ( -7.300564999359999696, 1480.050509870389988, 209.3673580074350014 ) ) ;
#109541 = ADVANCED_FACE ( 'NONE', ( #49408 ), #37291, .F. ) ;
#109542 = DIRECTION ( 'NONE',  ( 0.9894978258369474533, 0.04413734309288668695, -0.1376442792441983920 ) ) ;
#109543 = CARTESIAN_POINT ( 'NONE',  ( -10.37617513879240150, 1479.403831811299824, 210.6295454707710064 ) ) ;
#109544 = CARTESIAN_POINT ( 'NONE',  ( 11.03249561956813274, 1364.862809303433096, 207.6218459616987673 ) ) ;
#109545 = CARTESIAN_POINT ( 'NONE',  ( -12.00303979631470064, 1407.670897247700168, 269.4483317826930033 ) ) ;
#109546 = CARTESIAN_POINT ( 'NONE',  ( -13.07010703587889999, 1434.813263339430023, 149.2214592173789640 ) ) ;
#109547 = ORIENTED_EDGE ( 'NONE', *, *, #96805, .T. ) ;
#109548 = CARTESIAN_POINT ( 'NONE',  ( -4.327741874859570181, 1515.129976808890206, 209.8453366680959959 ) ) ;
#109549 = ORIENTED_EDGE ( 'NONE', *, *, #37214, .T. ) ;
#109550 = ORIENTED_EDGE ( 'NONE', *, *, #77112, .F. ) ;
#109551 = CARTESIAN_POINT ( 'NONE',  ( 6.563254890855000134, 1517.139039350860003, 211.6051684241269868 ) ) ;
#109552 = CARTESIAN_POINT ( 'NONE',  ( 4.363122683464830232, 1421.971318488559973, 183.8271341761570170 ) ) ;
#109553 = CARTESIAN_POINT ( 'NONE',  ( 7.361390247576359513, 1424.789603017459967, 194.1635867254269954 ) ) ;
#109555 = CARTESIAN_POINT ( 'NONE',  ( 0.9948947628070290428, 1432.734526706880160, 200.7323199818169996 ) ) ;
#109554 = CARTESIAN_POINT ( 'NONE',  ( 2.492130623175000448, 1516.778761582560037, 212.5675310476169955 ) ) ;
#109556 = CARTESIAN_POINT ( 'NONE',  ( -16.86146284859999867, 1470.469775084729918, 188.9038085686979969 ) ) ;
#109557 = CARTESIAN_POINT ( 'NONE',  ( -16.64506479750550128, 1498.345588598390123, 229.8579787729229906 ) ) ;
#109558 = ORIENTED_EDGE ( 'NONE', *, *, #8261, .F. ) ;
#109559 = CARTESIAN_POINT ( 'NONE',  ( -101.9775983549999978, 1378.556086106449811, 301.8221755499590699 ) ) ;
#109560 =( BOUNDED_SURFACE ( )  B_SPLINE_SURFACE ( 2, 1, ( 
 ( #106842, #31249 ),
 ( #39659, #91156 ),
 ( #64884, #22824 ),
 ( #29591, #73828 ),
 ( #12242, #106308 ),
 ( #97352, #46975 ),
 ( #46431, #65432 ),
 ( #80563, #13877 ),
 ( #90043, #54827 ),
 ( #107955, #72189 ),
 ( #48062, #29060 ) ),
 .UNSPECIFIED., .T., .F., .F. ) 
 B_SPLINE_SURFACE_WITH_KNOTS ( ( 3, 2, 2, 2, 2, 3 ),
 ( 2, 2 ),
 ( 1.721761971665900504, 3.141592653589790007, 4.712388980384689674, 6.283185307179590673, 7.853981633974480125, 8.004947278845490288 ),
 ( -18.71423869390639894, 37.42847738632139709 ),
 .UNSPECIFIED. ) 
 GEOMETRIC_REPRESENTATION_ITEM ( )  RATIONAL_B_SPLINE_SURFACE ( (
 ( 0.9491121336701159317, 0.9491121336701159317),
 ( 0.7352560790313820149, 0.7352560790313820149),
 ( 1.000000000000000000, 1.000000000000000000),
 ( 0.7071067811865510144, 0.7071067811865510144),
 ( 1.000000000000000000, 1.000000000000000000),
 ( 0.7071067811865510144, 0.7071067811865510144),
 ( 1.000000000000000000, 1.000000000000000000),
 ( 0.7071067811865510144, 0.7071067811865510144),
 ( 1.000000000000000000, 1.000000000000000000),
 ( 0.9718507021551689995, 0.9718507021551689995),
 ( 0.9491121336701159317, 0.9491121336701159317) ) ) 
 REPRESENTATION_ITEM ( '' )  SURFACE ( )  );
#109561 = ADVANCED_FACE ( 'NONE', ( #87413 ), #35909, .F. ) ;
#109562 = CARTESIAN_POINT ( 'NONE',  ( -3.455378015385000001, 1516.627618683580067, 202.1863880069169852 ) ) ;
#109563 = CARTESIAN_POINT ( 'NONE',  ( 1.399926847669999974, 1507.072115598929940, 236.8180522793980174 ) ) ;
#109564 = EDGE_CURVE ( 'NONE', #43369, #86466, #71666, .T. ) ;
#109565 = CARTESIAN_POINT ( 'NONE',  ( -38.17413872016189913, 1384.577420189890063, 211.2523201417219809 ) ) ;
#109566 = CARTESIAN_POINT ( 'NONE',  ( -44.13014295924060093, 1440.913052153659919, 270.2165797975040391 ) ) ;
#109567 = DIRECTION ( 'NONE',  ( 0.1930015070322609605, 0.3681831545501960123, -0.9095007328137468816 ) ) ;
#109569 = ORIENTED_EDGE ( 'NONE', *, *, #53884, .T. ) ;
#109568 = DIRECTION ( 'NONE',  ( -0.000000000000000000, -1.000000000000000000, -0.000000000000000000 ) ) ;
#109570 = ADVANCED_FACE ( 'NONE', ( #62801 ), #52635, .T. ) ;
#109571 = CARTESIAN_POINT ( 'NONE',  ( 11.55169038159974271, 1474.014209610494845, 269.6090286003602614 ) ) ;
#109572 = DIRECTION ( 'NONE',  ( 0.000000000000000000, 6.429975905516270088E-12, -1.000000000000000000 ) ) ;
#109573 = FACE_OUTER_BOUND ( 'NONE', #51585, .T. ) ;
#109574 = CARTESIAN_POINT ( 'NONE',  ( 0.1595995995380000143, 1486.508831850330125, 181.8147405652979671 ) ) ;
#109575 = B_SPLINE_CURVE_WITH_KNOTS ( 'NONE', 5,
 ( #59522, #32100, #33738, #66829, #58964, #100935, #67932, #15809, #84693, #50014, #84146, #41610 ),
 .UNSPECIFIED., .F., .F.,
 ( 6, 3, 3, 6 ),
 ( 6.548035129179999636, 6.565483659539999906, 9.290526163740000953, 11.10277561180000028 ),
 .UNSPECIFIED. ) ;
#109576 = CARTESIAN_POINT ( 'NONE',  ( -4.608021707265000266, 1516.660388280709867, 210.8351633799069873 ) ) ;
#109577 = CARTESIAN_POINT ( 'NONE',  ( -68.78035664479999411, 1379.747944962379961, 280.2443459286590155 ) ) ;
#109578 = CARTESIAN_POINT ( 'NONE',  ( -1.958690691882010393, 1484.245883193570080, 182.9456708303659696 ) ) ;
#109579 = CARTESIAN_POINT ( 'NONE',  ( 8.231849866949039196, 1438.595873408519992, 212.0577543541930368 ) ) ;
#109580 = CARTESIAN_POINT ( 'NONE',  ( -13.10647016826960076, 1414.913527292460003, 220.1876821406260092 ) ) ;
#109581 = CARTESIAN_POINT ( 'NONE',  ( -1.136814071995000175, 1516.854133554269993, 206.8377924607469822 ) ) ;
#109582 = ORIENTED_EDGE ( 'NONE', *, *, #12621, .T. ) ;
#109583 = CARTESIAN_POINT ( 'NONE',  ( -36.37832874669049232, 1435.767865795990019, 134.4203393042459993 ) ) ;
#109584 = CARTESIAN_POINT ( 'NONE',  ( -8.611763555213059362, 1437.722137921690091, 208.1397161665540239 ) ) ;
#109585 =( BOUNDED_CURVE ( )  B_SPLINE_CURVE ( 3, ( #34211, #45398, #17939, #632 ),
 .UNSPECIFIED., .F., .T. ) 
 B_SPLINE_CURVE_WITH_KNOTS ( ( 4, 4 ),
 ( 5.097274796035865307, 5.883015582179621283 ),
 .UNSPECIFIED. ) 
 CURVE ( )  GEOMETRIC_REPRESENTATION_ITEM ( )  RATIONAL_B_SPLINE_CURVE ( ( 1.000000000000000000, 0.9492093072870055881, 0.9492093072870055881, 1.000000000000000000 ) ) 
 REPRESENTATION_ITEM ( '' )  );
#109586 = CARTESIAN_POINT ( 'NONE',  ( -20.86320816170745474, 1455.053565070798186, 223.5191233675945739 ) ) ;
#109587 = ORIENTED_EDGE ( 'NONE', *, *, #23926, .T. ) ;
#109588 = CARTESIAN_POINT ( 'NONE',  ( -3.355893228018326457, 1523.847248782568613, 242.0621646443070745 ) ) ;
#109589 = B_SPLINE_CURVE_WITH_KNOTS ( 'NONE', 3,
 ( #98953, #65938, #48583, #82717, #23349, #107363, #22776, #92214, #22226, #91113, #14389, #57540, #83265, #30659, #39039, #7113, #58081, #91663, #65389, #24440 ),
 .UNSPECIFIED., .F., .F.,
 ( 4, 2, 2, 2, 1, 1, 1, 1, 2, 2, 2, 4 ),
 ( 0.000000000000000000, 0.2500000000004283796, 0.3750000000006425971, 0.4375000000007521206, 0.4687500000008068546, 0.4843750000008363310, 0.4921875000008418821, 0.4960937500008518741, 0.4980468750008568146, 0.5000000000008617551, 0.7500000000004308776, 1.000000000000000000 ),
 .UNSPECIFIED. ) ;
#109590 = CARTESIAN_POINT ( 'NONE',  ( 12.80285994373759983, 1434.672508522010048, 149.2809111413529877 ) ) ;
#109591 = CARTESIAN_POINT ( 'NONE',  ( -4.102557340004683084, 1441.363217865950901, 184.4172454785974367 ) ) ;
#109592 = CARTESIAN_POINT ( 'NONE',  ( 16.81464677261734764, 1526.382868172863937, 183.7052044321627022 ) ) ;
#109593 = CARTESIAN_POINT ( 'NONE',  ( 2.455820327400000114, 1434.541746329560056, 150.3615916412979914 ) ) ;
#109594 = CARTESIAN_POINT ( 'NONE',  ( 6.244159553780000316, 1487.029148873190024, 200.2607382902990025 ) ) ;
#109595 = DIRECTION ( 'NONE',  ( 0.4794255386042031719, 0.000000000000000000, 0.8775825618903726477 ) ) ;
#109596 = CARTESIAN_POINT ( 'NONE',  ( 4.220605471363215067, 1441.596061467261961, 170.5366720304299974 ) ) ;
#109598 = CARTESIAN_POINT ( 'NONE',  ( -11.86716023049999968, 1432.353341358199941, 147.6509521729980179 ) ) ;
#109597 = CARTESIAN_POINT ( 'NONE',  ( 3.264778779384999829, 1516.727068157269969, 214.1190961241369735 ) ) ;
#109599 = FACE_OUTER_BOUND ( 'NONE', #90548, .T. ) ;
#109600 = CARTESIAN_POINT ( 'NONE',  ( 2.486474742745000022, 1516.560253536979872, 216.0557253731069807 ) ) ;
#109601 = EDGE_LOOP ( 'NONE', ( #24183, #27739, #23167, #51451, #84296 ) ) ;
#109602 = CARTESIAN_POINT ( 'NONE',  ( -11.09581607415159965, 1414.913057834419988, 196.3422273742110065 ) ) ;
#109603 = CARTESIAN_POINT ( 'NONE',  ( 15.73570983720359884, 1409.462563483369877, 192.9527024472970140 ) ) ;
#109604 = CARTESIAN_POINT ( 'NONE',  ( 0.8523351540679999783, 1420.041841627029953, 184.5195079189979879 ) ) ;
#109605 = FACE_OUTER_BOUND ( 'NONE', #35304, .T. ) ;
#109606 = CARTESIAN_POINT ( 'NONE',  ( 3.017180836140621825, 1525.408327360769817, 176.9098388056617068 ) ) ;
#109607 = CARTESIAN_POINT ( 'NONE',  ( -7.545120860308170307, 1384.909328162950032, 219.0876147414010120 ) ) ;
#109608 = CARTESIAN_POINT ( 'NONE',  ( -11.38457156623280220, 1470.946925340780126, 208.3536595213249996 ) ) ;
#109609 = CARTESIAN_POINT ( 'NONE',  ( -6.245546245917391381, 1508.324562708814938, 220.0345331073419572 ) ) ;
#109610 = CARTESIAN_POINT ( 'NONE',  ( -0.01912654351157340102, 1347.931987472819856, 209.1220808601199792 ) ) ;
#109611 = CARTESIAN_POINT ( 'NONE',  ( 18.27629796897370440, 1425.362760113053127, 224.8572713904561624 ) ) ;
#109612 = DIRECTION ( 'NONE',  ( 0.01559023541505519597, -0.9998783230245037457, -0.0005326400372547868437 ) ) ;
#109613 = CARTESIAN_POINT ( 'NONE',  ( 37.44600398157700027, 1440.913060385919835, 255.3774732117640269 ) ) ;
#109615 = CARTESIAN_POINT ( 'NONE',  ( 4.328845283827350343, 1515.087839320550074, 207.8437208991539933 ) ) ;
#109614 = CARTESIAN_POINT ( 'NONE',  ( -6.589996145302899677, 1420.351519938529918, 194.7646280328370096 ) ) ;
#109616 = CARTESIAN_POINT ( 'NONE',  ( 13.14582612660000116, 1426.028273205230107, 222.1471477697979822 ) ) ;
#109617 = EDGE_LOOP ( 'NONE', ( #91893, #8048, #80657, #1749 ) ) ;
#109618 = ORIENTED_EDGE ( 'NONE', *, *, #15380, .T. ) ;
#109619 = EDGE_CURVE ( 'NONE', #82949, #40736, #109626, .T. ) ;
#109620 = CARTESIAN_POINT ( 'NONE',  ( -11.11084040270383611, 1506.426094286139914, 228.0935513073362415 ) ) ;
#109621 = CARTESIAN_POINT ( 'NONE',  ( -28.26671300199999948, 1509.671138065330069, 211.0443893778979998 ) ) ;
#109622 = CARTESIAN_POINT ( 'NONE',  ( 7.500754515229999697, 1423.062356241809766, 195.6521582632990146 ) ) ;
#109623 = EDGE_CURVE ( 'NONE', #71455, #16677, #66812, .T. ) ;
#109624 = CARTESIAN_POINT ( 'NONE',  ( -12.74111629470790064, 1416.830086716310007, 221.9830696278120001 ) ) ;
#109625 = DIRECTION ( 'NONE',  ( -1.000000000000000000, 0.000000000000000000, 0.000000000000000000 ) ) ;
#109626 = B_SPLINE_CURVE_WITH_KNOTS ( 'NONE', 3,
 ( #90695, #82308, #106951, #105871, #97458, #47068, #97993, #22365 ),
 .UNSPECIFIED., .F., .F.,
 ( 4, 2, 2, 4 ),
 ( 2.428612866367530240E-17, 0.001073044933456045527, 0.001609567400184072844, 0.002146089866912100162 ),
 .UNSPECIFIED. ) ;
#109627 = LINE ( 'NONE', #100117, #104091 ) ;
#109628 = CARTESIAN_POINT ( 'NONE',  ( -4.324479010949999314, 1515.254596385190098, 208.3983727628749989 ) ) ;
#109629 = CARTESIAN_POINT ( 'NONE',  ( -54.59994543616350171, 1383.804537930590186, 270.6530719560610123 ) ) ;
#109630 = CARTESIAN_POINT ( 'NONE',  ( 25.25200601139999890, 1450.804212501519942, 137.6134970599979965 ) ) ;
#109631 = DIRECTION ( 'NONE',  ( 0.000000000000000000, -1.000000000000000000, 6.123233995736769734E-17 ) ) ;
#109632 = CARTESIAN_POINT ( 'NONE',  ( 11.94675882516600041, 1492.833009754569957, 212.2903486444920134 ) ) ;
#109634 = ORIENTED_EDGE ( 'NONE', *, *, #70906, .T. ) ;
#109633 = CARTESIAN_POINT ( 'NONE',  ( 1.326713953160000070, 1454.806608698389937, 218.4390644836289823 ) ) ;
#109635 = CARTESIAN_POINT ( 'NONE',  ( -1.275851396490000011, 1451.568339848330197, 183.5777291321979874 ) ) ;
#109636 = ADVANCED_FACE ( 'NONE', ( #72818 ), #71738, .T. ) ;
#109637 = CARTESIAN_POINT ( 'NONE',  ( -39.62519685099999833, 1379.010909650270150, 224.0738340640590138 ) ) ;
#109638 = CARTESIAN_POINT ( 'NONE',  ( -1.602167524609999782, 1430.706703968889997, 217.3531761583190018 ) ) ;
#109639 = ORIENTED_EDGE ( 'NONE', *, *, #84388, .T. ) ;
#109640 = ORIENTED_EDGE ( 'NONE', *, *, #12765, .F. ) ;
#109641 = CARTESIAN_POINT ( 'NONE',  ( -8.200736117659999991, 1501.216938893890074, 208.7100876187340077 ) ) ;
#109642 = CARTESIAN_POINT ( 'NONE',  ( -2.329898367295349715, 1515.064791340959800, 204.7923971591859811 ) ) ;
#109644 = CARTESIAN_POINT ( 'NONE',  ( -16.79355120555579717, 1420.470915846049820, 203.2250788671829866 ) ) ;
#109643 = DIRECTION ( 'NONE',  ( 0.000000000000000000, 1.000000000000000000, 0.000000000000000000 ) ) ;
#109645 = CARTESIAN_POINT ( 'NONE',  ( 11.75431539821480165, 1479.716031737669937, 209.9331422352859988 ) ) ;
#109646 = CARTESIAN_POINT ( 'NONE',  ( -107.9473430369999960, 1380.764990262600122, 298.5035467044589836 ) ) ;
#109647 = CARTESIAN_POINT ( 'NONE',  ( 0.2017839417000019953, 1448.939945588189858, 190.0257811526990110 ) ) ;
#109648 = FACE_OUTER_BOUND ( 'NONE', #98339, .T. ) ;
#109649 = CARTESIAN_POINT ( 'NONE',  ( -16.32163182381450284, 1508.551704408389924, 213.4489841974129831 ) ) ;
#109650 = CARTESIAN_POINT ( 'NONE',  ( 0.7028133466986099531, 1507.119929753229826, 180.9953409562019715 ) ) ;
#109651 = EDGE_CURVE ( 'NONE', #49504, #67084, #65528, .T. ) ;
#109652 = CARTESIAN_POINT ( 'NONE',  ( 18.52299501639999946, 1425.669522579430122, 225.2536361859980047 ) ) ;
#109653 = DIRECTION ( 'NONE',  ( 0.000000000000000000, 0.8724564897876694314, -0.4886917979947875135 ) ) ;
#109654 = CARTESIAN_POINT ( 'NONE',  ( 8.177528389328550418, 1433.974668205089984, 204.5575942349009892 ) ) ;
#109655 = CARTESIAN_POINT ( 'NONE',  ( -2.499999926692149987, 1440.210506878179785, 168.7266372007799760 ) ) ;
#109656 = CARTESIAN_POINT ( 'NONE',  ( -2.907244326632850040, 1451.960134957139871, 184.7555981325950256 ) ) ;
#109657 = ORIENTED_EDGE ( 'NONE', *, *, #4657, .F. ) ;
#109658 = ADVANCED_FACE ( 'NONE', ( #71754 ), #56566, .F. ) ;
#109659 = CARTESIAN_POINT ( 'NONE',  ( 16.68062049856724016, 1524.382868172863937, 236.8314524626096045 ) ) ;
#109660 = CARTESIAN_POINT ( 'NONE',  ( 18.39490484120650038, 1457.283212162220025, 229.1081970229850242 ) ) ;
#109661 = B_SPLINE_CURVE_WITH_KNOTS ( 'NONE', 3,
 ( #52824, #35452, #102624, #70752, #25925, #26487, #86954, #19747, #95364, #79132 ),
 .UNSPECIFIED., .F., .F.,
 ( 4, 2, 2, 2, 4 ),
 ( -0.1158481289682099930, -0.06677386518054599651, -0.02553295751034780070, -0.01160833233004980591, -1.224380319353457480E-11 ),
 .UNSPECIFIED. ) ;
#109662 = ADVANCED_FACE ( 'NONE', ( #13982 ), #25148, .T. ) ;
#109663 = FACE_OUTER_BOUND ( 'NONE', #47268, .T. ) ;
#109664 = CARTESIAN_POINT ( 'NONE',  ( -8.904037867643029100E-09, 1472.816589274460057, 260.8417418167990149 ) ) ;
#109665 = CARTESIAN_POINT ( 'NONE',  ( -0.6209246912237348370, 1515.589587247160352, 213.1417529444950105 ) ) ;
#109666 = CARTESIAN_POINT ( 'NONE',  ( 2.008229287959999887, 1477.194275967190151, 198.7982270578989983 ) ) ;
#109667 = CARTESIAN_POINT ( 'NONE',  ( -105.3787933579999958, 1390.956730496739965, 305.3341016426589931 ) ) ;
#109668 = CARTESIAN_POINT ( 'NONE',  ( -7.546131077396060149, 1510.764648358900104, 214.9767338929050027 ) ) ;
#109669 = CARTESIAN_POINT ( 'NONE',  ( -11.01845241045810120, 1362.383112808261785, 208.3718459617010978 ) ) ;
#109670 = DIRECTION ( 'NONE',  ( -1.755985294532469921E-16, 1.000000000000000000, -1.338183447452831989E-16 ) ) ;
#109671 = CARTESIAN_POINT ( 'NONE',  ( 14.06094701564179950, 1509.398387556550006, 234.7098584303389828 ) ) ;
#109672 = CARTESIAN_POINT ( 'NONE',  ( -8.370248062009999046, 1424.386071264410020, 207.6999102099590004 ) ) ;
#109673 = EDGE_CURVE ( 'NONE', #1894, #60389, #42797, .T. ) ;
#109674 = CARTESIAN_POINT ( 'NONE',  ( 7.713648834184999359, 1516.710624944440042, 208.3691743819339877 ) ) ;
#109675 = CARTESIAN_POINT ( 'NONE',  ( -5.392707179739999468, 1433.241571820989975, 154.6274174169979858 ) ) ;
#109676 = CARTESIAN_POINT ( 'NONE',  ( 11.00428676220000135, 1425.778354413130046, 91.15517427569778874 ) ) ;
#109677 = CARTESIAN_POINT ( 'NONE',  ( 7.467787984152029601, 1426.091549560359908, 212.4046628816660132 ) ) ;
#109678 = ADVANCED_FACE ( 'NONE', ( #22924 ), #5606, .T. ) ;
#109679 = CARTESIAN_POINT ( 'NONE',  ( -25.97192969330459889, 1450.951951750279932, 136.6899769078980000 ) ) ;
#109680 = ORIENTED_EDGE ( 'NONE', *, *, #44798, .F. ) ;
#109681 = CARTESIAN_POINT ( 'NONE',  ( 27.37758288899999926, 1435.465027219049944, 231.9164972690979880 ) ) ;
#109683 = CARTESIAN_POINT ( 'NONE',  ( -17.41030370700000063, 1410.018619281429892, 194.3499987567980156 ) ) ;
#109682 = CARTESIAN_POINT ( 'NONE',  ( -2.700472180932728783, 1524.678541297861329, 176.3823254397200344 ) ) ;
#109684 = CARTESIAN_POINT ( 'NONE',  ( -1.987375205934570177, 1419.504246183010082, 185.8126813929330012 ) ) ;
#109685 = CARTESIAN_POINT ( 'NONE',  ( -16.65350847794880451, 1508.454466938620271, 213.7226249311669903 ) ) ;
#109686 = CARTESIAN_POINT ( 'NONE',  ( -4.633397096295920115, 1377.913060387289988, 213.8868415672910146 ) ) ;
#109687 = CARTESIAN_POINT ( 'NONE',  ( -20.83123093438729967, 1452.185617773610147, 142.1974481988970069 ) ) ;
#109688 = DIRECTION ( 'NONE',  ( 1.989737444810000148E-13, 6.825857443600000379E-15, -1.000000000000000000 ) ) ;
#109689 = EDGE_LOOP ( 'NONE', ( #21907, #85865, #58371, #74333, #3020 ) ) ;
#109690 = CARTESIAN_POINT ( 'NONE',  ( -4.438186827019999854E-16, 1395.913060387330006, 217.1218459616979999 ) ) ;
#109691 = CARTESIAN_POINT ( 'NONE',  ( 15.69186927393040065, 1421.413580593060033, 227.6163148024349994 ) ) ;
#109692 = CARTESIAN_POINT ( 'NONE',  ( -7.989567385690000023, 1384.306347471770096, 199.5291465469090042 ) ) ;
#109693 = ORIENTED_EDGE ( 'NONE', *, *, #20739, .F. ) ;
#109694 = EDGE_LOOP ( 'NONE', ( #13385, #33369, #45887, #98382 ) ) ;
#109695 = EDGE_CURVE ( 'NONE', #3640, #5600, #69603, .T. ) ;
#109696 = CARTESIAN_POINT ( 'NONE',  ( -84.12715333319998479, 1385.173288781940073, 288.0594686105589517 ) ) ;
#109697 = CARTESIAN_POINT ( 'NONE',  ( -23.32686250069690104, 1409.842844829079922, 209.2659248779790175 ) ) ;
#109698 = EDGE_LOOP ( 'NONE', ( #38339, #59030, #5989, #61805, #40942 ) ) ;
#109699 = CARTESIAN_POINT ( 'NONE',  ( -109.9852174251870025, 1384.905086218720044, 311.4561813548020268 ) ) ;
#109700 = CARTESIAN_POINT ( 'NONE',  ( -43.43522585315017892, 1430.093246065128596, 266.2528640357818404 ) ) ;
#109701 = ADVANCED_FACE ( 'NONE', ( #6141 ), #44602, .T. ) ;
#109702 = CARTESIAN_POINT ( 'NONE',  ( -2.843430457760000252, 1498.350673094430022, 236.4627852063980242 ) ) ;
#109703 = CARTESIAN_POINT ( 'NONE',  ( -20.28645208769999897, 1410.869633620929790, 220.2088169694980024 ) ) ;
#109704 = ORIENTED_EDGE ( 'NONE', *, *, #68530, .T. ) ;
#109705 = CARTESIAN_POINT ( 'NONE',  ( 43.63532980919219995, 1452.867011165669965, 267.6831642553480037 ) ) ;
#109706 = CARTESIAN_POINT ( 'NONE',  ( -3.822978263369920082, 1508.729442836390035, 204.5649349435400097 ) ) ;
#109707 = CARTESIAN_POINT ( 'NONE',  ( -17.00189750847108172, 1422.035433323501366, 226.8094376528395344 ) ) ;
#109708 = CARTESIAN_POINT ( 'NONE',  ( 4.998515157294999511, 1516.787536375099990, 205.0819486540370065 ) ) ;
#109709 = ORIENTED_EDGE ( 'NONE', *, *, #13601, .F. ) ;
#109710 = CARTESIAN_POINT ( 'NONE',  ( 18.99566638059803481, 1457.358491571087598, 226.5903252133678620 ) ) ;
#109711 = CARTESIAN_POINT ( 'NONE',  ( 15.26795440090729983, 1513.114148093550057, 195.0970705441609994 ) ) ;
#109712 = CARTESIAN_POINT ( 'NONE',  ( 0.6825862493659989871, 1429.440998290589960, 214.6621653640990246 ) ) ;
#109713 = ORIENTED_EDGE ( 'NONE', *, *, #24086, .T. ) ;
#109714 = DIRECTION ( 'NONE',  ( -1.755985294532469921E-16, 1.000000000000000000, -1.338183447452831989E-16 ) ) ;
#109715 = CARTESIAN_POINT ( 'NONE',  ( 26.77909383400000110, 1451.812801000929994, 135.6496118224980023 ) ) ;
#109716 = CARTESIAN_POINT ( 'NONE',  ( 0.000000000000000000, 1378.913060387289988, 209.1218459616989946 ) ) ;
#109717 = CARTESIAN_POINT ( 'NONE',  ( 11.91507101810570113, 1501.870660809160199, 213.5943109225670185 ) ) ;
#109718 = CARTESIAN_POINT ( 'NONE',  ( 8.157055013780000863, 1421.297622302039827, 196.0511713190989838 ) ) ;
#109719 = CARTESIAN_POINT ( 'NONE',  ( -0.3337973666484369550, 1431.965207721749948, 218.6129415553859872 ) ) ;
#109720 = CARTESIAN_POINT ( 'NONE',  ( -5.301603799309999587, 1495.069284652189936, 198.4487960541990219 ) ) ;
#109721 = CARTESIAN_POINT ( 'NONE',  ( 6.511209069565670582, 1409.140436818330045, 188.5236114198380051 ) ) ;
#109723 = DIRECTION ( 'NONE',  ( -1.000000000000000000, 0.000000000000000000, -4.657385588302535823E-10 ) ) ;
#109722 = CARTESIAN_POINT ( 'NONE',  ( 30.16752008203805602, 1524.964158026966061, 196.5181576271968140 ) ) ;
#109724 = CARTESIAN_POINT ( 'NONE',  ( 11.71723861691340041, 1426.603203500050085, 206.5361617024459804 ) ) ;
#109725 = B_SPLINE_CURVE_WITH_KNOTS ( 'NONE', 3,
 ( #93214, #7010, #23795, #93747, #41169, #15396, #7562, #50672, #76421, #65837, #8104, #16483, #91575 ),
 .UNSPECIFIED., .F., .F.,
 ( 4, 2, 2, 1, 2, 2, 4 ),
 ( 0.000000000000000000, 0.2499999999999756306, 0.3749999999999817368, 0.4374999999999787947, 0.4687499999999667488, 0.4999999999999547029, 1.000000000000000000 ),
 .UNSPECIFIED. ) ;
#109726 = CARTESIAN_POINT ( 'NONE',  ( -11.00250985070000098, 1379.595586062069970, 215.1074884732990142 ) ) ;
#109727 = CARTESIAN_POINT ( 'NONE',  ( 11.43480838300000002, 1425.837049133330083, 122.9428393764980001 ) ) ;
#109728 = ORIENTED_EDGE ( 'NONE', *, *, #78018, .T. ) ;
#109729 = CARTESIAN_POINT ( 'NONE',  ( 12.57878310069559902, 1415.943166310999914, 222.1097011578140155 ) ) ;
#109730 = CARTESIAN_POINT ( 'NONE',  ( -5.513264357029999729, 1374.913060387289988, 214.9370262455390161 ) ) ;
#109731 = CARTESIAN_POINT ( 'NONE',  ( -11.33780467209640008, 1482.838548967459701, 205.4682982156419939 ) ) ;
#109732 = FACE_OUTER_BOUND ( 'NONE', #72664, .T. ) ;
#109733 = FACE_OUTER_BOUND ( 'NONE', #58124, .T. ) ;
#109734 = CARTESIAN_POINT ( 'NONE',  ( 11.31726009937499988, 1422.350445949510004, 203.3738828430369665 ) ) ;
#109735 = CARTESIAN_POINT ( 'NONE',  ( 10.25304830813499990, 1513.301704408390151, 203.8185450922669872 ) ) ;
#109736 = CARTESIAN_POINT ( 'NONE',  ( -31.32742177469999945, 1440.913060387330006, 255.3819207742980097 ) ) ;
#109737 = CARTESIAN_POINT ( 'NONE',  ( -8.960270527080961500, 1384.233187754379969, 218.6195202797470074 ) ) ;
#109738 = CARTESIAN_POINT ( 'NONE',  ( 11.70984135820000027, 1433.749505160629951, 151.0000356945979831 ) ) ;
#109739 = CARTESIAN_POINT ( 'NONE',  ( 40.73184307449999864, 1445.563106277920042, 268.3665355199980240 ) ) ;
#109740 = CARTESIAN_POINT ( 'NONE',  ( -9.663432460078139385, 1460.495846937979877, 209.0938806983130007 ) ) ;
#109741 = DIRECTION ( 'NONE',  ( 0.4547561197925752419, 0.8635678785390505929, 0.2178242196514530993 ) ) ;
#109742 = CARTESIAN_POINT ( 'NONE',  ( 7.733708448627369059, 1421.053201843950092, 195.5966628498169939 ) ) ;
#109743 = AXIS2_PLACEMENT_3D ( 'NONE', #62925, #20299, #54503 ) ;
#109744 = CARTESIAN_POINT ( 'NONE',  ( 9.272480241026579861, 1463.528063730330132, 214.3122284173120136 ) ) ;
#109745 = B_SPLINE_CURVE_WITH_KNOTS ( 'NONE', 3,
 ( #56588, #64455, #81217, #89076, #12362, #31367 ),
 .UNSPECIFIED., .F., .F.,
 ( 4, 2, 4 ),
 ( 0.000000000000000000, 0.4999999999999998890, 1.000000000000000000 ),
 .UNSPECIFIED. ) ;
#109746 = EDGE_CURVE ( 'NONE', #72223, #41356, #66365, .T. ) ;
#109747 = CARTESIAN_POINT ( 'NONE',  ( -18.85310169809999792, 1486.003537439730053, 189.4173365011979797 ) ) ;
#109748 = CARTESIAN_POINT ( 'NONE',  ( -1.065774218729999975E-16, 1426.566393376330097, 144.1938086916980239 ) ) ;
#109749 = CARTESIAN_POINT ( 'NONE',  ( -17.22714485659999895, 1409.679743144430176, 224.9962836928979755 ) ) ;
#109750 = CARTESIAN_POINT ( 'NONE',  ( 23.51192877309999929, 1410.913812945130076, 211.8293362867379983 ) ) ;
#109751 = VECTOR ( 'NONE', #10570, 1000.000000000000000 ) ;
#109752 = DIRECTION ( 'NONE',  ( 0.000000000000000000, 1.000000000000000000, 0.000000000000000000 ) ) ;
#109753 = LINE ( 'NONE', #33031, #34313 ) ;
#109754 = CARTESIAN_POINT ( 'NONE',  ( 9.549998149862538810, 1451.222071596379919, 207.5451647876320180 ) ) ;
#109755 = CARTESIAN_POINT ( 'NONE',  ( -2.456601303385837820, 1523.611961620354123, 175.3003469896239039 ) ) ;
#109756 = CARTESIAN_POINT ( 'NONE',  ( -109.2297890131749938, 1384.978503039539873, 295.1339919130639942 ) ) ;
#109757 = CARTESIAN_POINT ( 'NONE',  ( -11.80290349340000056, 1415.088016306429836, 221.3076619498979767 ) ) ;
#109758 = CARTESIAN_POINT ( 'NONE',  ( -15.45163273801909831, 1421.121908474589873, 203.4374413400199728 ) ) ;
#109759 = CARTESIAN_POINT ( 'NONE',  ( 0.2066550540702130068, 1459.231929753809936, 182.9860342603810182 ) ) ;
#109761 = ORIENTED_EDGE ( 'NONE', *, *, #50292, .F. ) ;
#109760 = DIRECTION ( 'NONE',  ( 0.000000000000000000, 0.000000000000000000, -1.000000000000000000 ) ) ;
#109762 = CARTESIAN_POINT ( 'NONE',  ( -27.73716673060003757, 1443.913060387329097, 175.8274728504979976 ) ) ;
#109763 = EDGE_CURVE ( 'NONE', #17568, #85887, #2984, .T. ) ;
#109764 = CARTESIAN_POINT ( 'NONE',  ( 34.18677586421189574, 1522.382868172863937, 219.7932833225211766 ) ) ;
#109765 = CARTESIAN_POINT ( 'NONE',  ( -17.71193100849139768, 1517.151704408390060, 221.5709757781449980 ) ) ;
#109766 = CARTESIAN_POINT ( 'NONE',  ( -41.56910739857319470, 1442.487573087369810, 134.0999999980959956 ) ) ;
#109767 = CARTESIAN_POINT ( 'NONE',  ( -109.8948235710000034, 1384.907847270719913, 297.0284604404590141 ) ) ;
#109768 = EDGE_LOOP ( 'NONE', ( #11203, #106859, #62450, #66468, #90491 ) ) ;
#109769 = B_SPLINE_CURVE_WITH_KNOTS ( 'NONE', 5,
 ( #29300, #64035, #87574, #80816, #71356, #11417 ),
 .UNSPECIFIED., .F., .F.,
 ( 6, 6 ),
 ( 0.000000000000000000, 1.000000000000000000 ),
 .UNSPECIFIED. ) ;
#109770 = B_SPLINE_SURFACE_WITH_KNOTS ( 'NONE', 5, 5, ( 
 ( #92699, #50177, #84305, #59674, #59131, #50708 ),
 ( #84839, #108409, #25482, #7050, #83754, #49621 ),
 ( #23285, #6498, #31691, #65874, #92157, #99994 ),
 ( #76458, #32254, #66977, #41208, #66434, #57481 ),
 ( #15430, #75378, #109517, #8139, #42305, #83209 ),
 ( #91606, #101088, #23830, #68090, #74821, #58570 ),
 ( #33337, #7596, #24387, #100550, #41751, #14883 ),
 ( #75910, #40098, #67532, #101632, #24921, #110612 ),
 ( #33894, #93253, #16518, #17061, #82662, #5953 ) ),
 .UNSPECIFIED., .F., .F., .F.,
 ( 6, 3, 6 ),
 ( 6, 6 ),
 ( 11.46419780020000090, 17.35795963829999877, 30.62292852850000102 ),
 ( 0.000000000000000000, 2.000000000000000000 ),
 .UNSPECIFIED. ) ;
#109771 = CARTESIAN_POINT ( 'NONE',  ( -0.8557946027419990331, 1485.901655772089953, 197.2260526041989976 ) ) ;
#109772 = CARTESIAN_POINT ( 'NONE',  ( -16.43158050010680071, 1420.644938884899830, 203.2808245233400157 ) ) ;
#109773 = DIRECTION ( 'NONE',  ( 8.727810504445229884E-47, -1.000000000000000000, 1.836970198721029688E-16 ) ) ;
#109774 = TOROIDAL_SURFACE ( 'NONE', #70482, 1.000000000000000000, 1.000000000000000000 ) ;
#109775 = EDGE_CURVE ( 'NONE', #86349, #101781, #48156, .T. ) ;
#109776 = CARTESIAN_POINT ( 'NONE',  ( 6.520094218474939751, 1467.947603753620115, 206.8052153602889973 ) ) ;
#109777 = CARTESIAN_POINT ( 'NONE',  ( -13.74310390781900004, 1517.051704408389924, 201.1531303618569950 ) ) ;
#109778 = CARTESIAN_POINT ( 'NONE',  ( 21.30047364570000212, 1471.312091223629977, 210.0334653296820022 ) ) ;
#109779 = CARTESIAN_POINT ( 'NONE',  ( -5.362304121457834860, 1422.288402133340242, 142.1498578916476561 ) ) ;
#109780 = CARTESIAN_POINT ( 'NONE',  ( 32.38114538885250226, 1523.604703353109699, 202.1233279672528624 ) ) ;
#109781 = B_SPLINE_SURFACE_WITH_KNOTS ( 'NONE', 5, 5, ( 
 ( #101354, #49345, #100288, #109254, #57762, #99714 ),
 ( #99160, #49897, #84029, #40927, #82929, #75106 ),
 ( #31419, #22440, #73995, #5119, #48806, #15154 ),
 ( #23568, #32537, #83471, #39275, #56642, #47689 ),
 ( #14059, #73449, #6221, #109792, #90776, #75653 ),
 ( #7330, #48246, #6765, #91334, #23007, #31977 ),
 ( #41493, #66709, #81817, #40373, #107582, #100817 ),
 ( #24104, #14619, #33071, #74552, #58296, #67262 ),
 ( #82389, #30868, #65601, #108685, #66167, #65045 ) ),
 .UNSPECIFIED., .F., .F., .F.,
 ( 6, 3, 6 ),
 ( 6, 6 ),
 ( 3.112795738710000037, 3.535848030919999996, 3.958900323119999953 ),
 ( 0.000000000000000000, 2.000000000000000000 ),
 .UNSPECIFIED. ) ;
#109782 = CARTESIAN_POINT ( 'NONE',  ( -51.62800087644459524, 1385.024991398460088, 227.8640657499650217 ) ) ;
#109783 = CARTESIAN_POINT ( 'NONE',  ( -10.57737777167070092, 1391.913060387289988, 213.4296204213179919 ) ) ;
#109784 = CARTESIAN_POINT ( 'NONE',  ( 10.78065115729800105, 1422.571582845389912, 208.5037857000629913 ) ) ;
#109785 = ORIENTED_EDGE ( 'NONE', *, *, #41772, .F. ) ;
#109786 = CARTESIAN_POINT ( 'NONE',  ( -32.69751076149999847, 1451.617800104529806, 135.6222252852979864 ) ) ;
#109787 = DIRECTION ( 'NONE',  ( 0.000000000000000000, 0.000000000000000000, 1.000000000000000000 ) ) ;
#109789 = ORIENTED_EDGE ( 'NONE', *, *, #34350, .F. ) ;
#109788 = CARTESIAN_POINT ( 'NONE',  ( 2.370970874524633398, 1427.002265528473799, 137.0999999980980135 ) ) ;
#109790 = CARTESIAN_POINT ( 'NONE',  ( 4.221033085759999359, 1472.290285735790121, 218.3905899716789918 ) ) ;
#109791 = CARTESIAN_POINT ( 'NONE',  ( -19.66031314052480994, 1410.960623777707269, 221.6379339483827664 ) ) ;
#109792 = CARTESIAN_POINT ( 'NONE',  ( -109.4849921600000044, 1384.708507898549897, 311.2789825532589703 ) ) ;
#109793 = CARTESIAN_POINT ( 'NONE',  ( -5.215695275219999871, 1495.379823515289900, 198.7908128922989874 ) ) ;
#109794 = EDGE_CURVE ( 'NONE', #105489, #36910, #64855, .T. ) ;
#109795 = CARTESIAN_POINT ( 'NONE',  ( 41.79939186130401652, 1444.333674645975179, 269.6436966550891157 ) ) ;
#109796 = CYLINDRICAL_SURFACE ( 'NONE', #21291, 0.4999999999999449329 ) ;
#109797 = CARTESIAN_POINT ( 'NONE',  ( 17.96451342846462396, 1434.943382339013397, 215.4098532707286040 ) ) ;
#109798 = CARTESIAN_POINT ( 'NONE',  ( 7329.274061526074547, -2340.220200558883789, 11096.25664408519697 ) ) ;
#109799 = CARTESIAN_POINT ( 'NONE',  ( -2.613924617009112605, 1516.542698304417627, 201.4125944022433714 ) ) ;
#109800 = CARTESIAN_POINT ( 'NONE',  ( -128.4815115702338915, 1331.448250124728247, 295.9827786358457615 ) ) ;
#109801 = EDGE_CURVE ( 'NONE', #57731, #77826, #52998, .T. ) ;
#109802 = DIRECTION ( 'NONE',  ( 0.9996573249755517088, -0.02617694830808747070, 0.000000000000000000 ) ) ;
#109803 = CARTESIAN_POINT ( 'NONE',  ( -0.3879872414129990066, 1457.041586684089907, 199.5965184120390177 ) ) ;
#109804 = EDGE_CURVE ( 'NONE', #3293, #5019, #57489, .T. ) ;
#109805 = CARTESIAN_POINT ( 'NONE',  ( -5.787477032644999575, 1517.070197312179971, 206.2521524731670013 ) ) ;
#109806 = FACE_OUTER_BOUND ( 'NONE', #104879, .T. ) ;
#109807 = EDGE_LOOP ( 'NONE', ( #96860, #62357, #48535, #42767, #64969 ) ) ;
#109808 = CARTESIAN_POINT ( 'NONE',  ( -109.1340195298539868, 1384.837378371770001, 311.2641337568139761 ) ) ;
#109809 = CARTESIAN_POINT ( 'NONE',  ( 14.00912983899999986, 1416.839648759230158, 196.3913567892980154 ) ) ;
#109811 = ORIENTED_EDGE ( 'NONE', *, *, #69860, .T. ) ;
#109810 = CARTESIAN_POINT ( 'NONE',  ( -68.63115668882700504, 1379.747695794610081, 280.2278140600810161 ) ) ;
#109812 = EDGE_CURVE ( 'NONE', #81031, #56488, #107925, .T. ) ;
#109813 = CARTESIAN_POINT ( 'NONE',  ( -8.155564057308037462, 1382.295710237911635, 218.5042669288760351 ) ) ;
#109814 = ORIENTED_EDGE ( 'NONE', *, *, #88704, .T. ) ;
#109815 = CARTESIAN_POINT ( 'NONE',  ( -16.50477756776011518, 1512.979858876863773, 220.9284238778866438 ) ) ;
#109816 = CARTESIAN_POINT ( 'NONE',  ( -23.61553526509999656, 1410.914738123429970, 206.7820667545679783 ) ) ;
#109818 = CARTESIAN_POINT ( 'NONE',  ( 16.23605858256030032, 1409.581384769300030, 192.4955713889560229 ) ) ;
#109817 = CARTESIAN_POINT ( 'NONE',  ( -11.71570024223670003, 1426.293107577299907, 142.6799693210089970 ) ) ;
#109819 = CARTESIAN_POINT ( 'NONE',  ( 3.268859396054999866, 1516.922519270759949, 211.5998327024669834 ) ) ;
#109820 = CARTESIAN_POINT ( 'NONE',  ( 40.27308140560000282, 1443.612049536910035, 137.1163288290979949 ) ) ;
#109821 = CARTESIAN_POINT ( 'NONE',  ( -19.16279443490000034, 1411.291491730330108, 262.3396854780979766 ) ) ;
#109822 = DIRECTION ( 'NONE',  ( 0.000000000000000000, 1.000000000000000000, 0.000000000000000000 ) ) ;
#109823 = CARTESIAN_POINT ( 'NONE',  ( 14.10180166660902046, 1462.573205505089845, 230.5089236422518582 ) ) ;
#109824 = CARTESIAN_POINT ( 'NONE',  ( 34.94829774772319553, 1451.625365366340020, 134.0999999983029909 ) ) ;
#109825 = CARTESIAN_POINT ( 'NONE',  ( -35.95777000360060072, 1437.416693626100141, 136.5372231441070028 ) ) ;
#109826 = VERTEX_POINT ( 'NONE', #100077 ) ;
#109827 = CARTESIAN_POINT ( 'NONE',  ( 24.11200186056320049, 1496.633625139249943, 206.8275369771670000 ) ) ;
#109828 = EDGE_CURVE ( 'NONE', #22768, #66538, #41321, .T. ) ;
#109829 = CARTESIAN_POINT ( 'NONE',  ( 3.313501335607582643, 1397.551704408390151, 215.1871694724064810 ) ) ;
#109830 = ORIENTED_EDGE ( 'NONE', *, *, #16426, .F. ) ;
#109831 = ORIENTED_EDGE ( 'NONE', *, *, #37764, .T. ) ;
#109832 = CIRCLE ( 'NONE', #20446, 1.999999999999998668 ) ;
#109833 = CARTESIAN_POINT ( 'NONE',  ( 3.160865718646527434, 1370.358796302880364, 211.5724212009420739 ) ) ;
#109834 = CARTESIAN_POINT ( 'NONE',  ( 14.45119567767109992, 1485.899027755930092, 225.7245081177429995 ) ) ;
#109835 = CARTESIAN_POINT ( 'NONE',  ( -4.822785920201220655, 1507.731391114710050, 221.0789200719150074 ) ) ;
#109836 = CARTESIAN_POINT ( 'NONE',  ( -14.15978805234909998, 1508.551704406640056, 210.0665490177079846 ) ) ;
#109837 = EDGE_CURVE ( 'NONE', #84627, #105413, #44197, .T. ) ;
#109838 = CARTESIAN_POINT ( 'NONE',  ( 11.16717556649999921, 1414.661898229710005, 205.5169791222290030 ) ) ;
#109839 = AXIS2_PLACEMENT_3D ( 'NONE', #24652, #48816, #109802 ) ;
#109840 = B_SPLINE_CURVE_WITH_KNOTS ( 'NONE', 3,
 ( #57519, #64826, #4879, #99475, #55868, #56403, #46919, #108451, #107890, #82699, #13812, #14369, #48562, #65917, #31182, #65369, #13262, #5988, #30639, #39594, #81575, #40137, #90535, #5437, #14919 ),
 .UNSPECIFIED., .F., .F.,
 ( 4, 2, 2, 1, 1, 2, 2, 2, 2, 1, 1, 1, 2, 2, 4 ),
 ( 0.000000000000000000, 0.2499999999954249930, 0.3749999999931376005, 0.4374999999919982896, 0.4687499999916037163, 0.4843749999914018223, 0.4999999999911999282, 0.6249999999875969214, 0.6874999999857954736, 0.7187499999850445187, 0.7343749999848121490, 0.7421874999846904686, 0.7460937499846346244, 0.7499999999845787801, 1.000000000000000000 ),
 .UNSPECIFIED. ) ;
#109841 = CARTESIAN_POINT ( 'NONE',  ( -5.135284114272939959, 1454.993527858050129, 201.2217254690109769 ) ) ;
#109842 = CARTESIAN_POINT ( 'NONE',  ( 33.91369114129039986, 1451.728768196330066, 134.7402677064790169 ) ) ;
#109843 = CARTESIAN_POINT ( 'NONE',  ( 12.78752272718304184, 1416.843574568078566, 222.7044121896790898 ) ) ;
#109844 = CARTESIAN_POINT ( 'NONE',  ( 26.26433425849999992, 1440.617482597780054, 137.6222147125980086 ) ) ;
#109845 = ADVANCED_FACE ( 'NONE', ( #67051 ), #6020, .F. ) ;
#109846 = CARTESIAN_POINT ( 'NONE',  ( -10.57531603410000010, 1391.913060387289988, 213.4590788534990224 ) ) ;
#109847 = CARTESIAN_POINT ( 'NONE',  ( -70.69354556520289634, 1384.741626837030026, 267.3362997785129664 ) ) ;
#109848 = VERTEX_POINT ( 'NONE', #69076 ) ;
#109849 = CARTESIAN_POINT ( 'NONE',  ( -6.942344729965000738, 1516.810037859429940, 201.4055938791270250 ) ) ;
#109850 = CARTESIAN_POINT ( 'NONE',  ( -7.724874651314999952, 1517.139320148880188, 208.3815253650730028 ) ) ;
#109851 = VERTEX_POINT ( 'NONE', #47026 ) ;
#109852 = CARTESIAN_POINT ( 'NONE',  ( 11.76320837242760042, 1426.958789830729984, 145.9773750732420012 ) ) ;
#109853 = CARTESIAN_POINT ( 'NONE',  ( 4.936023922893961746, 1511.397677005970309, 217.6234439496228958 ) ) ;
#109854 = ORIENTED_EDGE ( 'NONE', *, *, #102818, .F. ) ;
#109855 = CARTESIAN_POINT ( 'NONE',  ( -13.46339118210000052, 1415.263254644630024, 221.0797442403980142 ) ) ;
#109856 = CARTESIAN_POINT ( 'NONE',  ( -14.26333330936780008, 1452.396687514240057, 223.0069981058830137 ) ) ;
#109857 = DIRECTION ( 'NONE',  ( 0.9455185755993178454, 0.000000000000000000, -0.3255681544571537578 ) ) ;
#109858 = CARTESIAN_POINT ( 'NONE',  ( 23.96695357696606266, 1411.114076150693109, 208.3039881944807803 ) ) ;
#109859 = CARTESIAN_POINT ( 'NONE',  ( -13.15607067979999911, 1416.813004075730078, 221.9084248872979970 ) ) ;
#109860 = CARTESIAN_POINT ( 'NONE',  ( 10.69573263740039870, 1470.053339629819902, 207.0568841171169936 ) ) ;
#109861 = LINE ( 'NONE', #93584, #94258 ) ;
#109862 = CARTESIAN_POINT ( 'NONE',  ( -16.30342780150716209, 1410.854766001639064, 191.5161596899749838 ) ) ;
#109863 = CARTESIAN_POINT ( 'NONE',  ( -63.97154863419999771, 1379.735362472459883, 270.2946752427589558 ) ) ;
#109864 = CARTESIAN_POINT ( 'NONE',  ( 22.94534059460660202, 1420.146124040419863, 206.2024909355390037 ) ) ;
#109866 = CARTESIAN_POINT ( 'NONE',  ( 5.336874482553809251, 1467.014048226709974, 199.3769685164120062 ) ) ;
#109865 = CARTESIAN_POINT ( 'NONE',  ( 17.39940665230000150, 1459.341270389529882, 228.5023076377979976 ) ) ;
#109867 = CARTESIAN_POINT ( 'NONE',  ( -4.785922751469102288, 1422.261607323150656, 184.7437580134849782 ) ) ;
#109868 = CARTESIAN_POINT ( 'NONE',  ( -2.485205687335000135, 1517.181921232829836, 216.8478361320569832 ) ) ;
#109869 = VERTEX_POINT ( 'NONE', #4466 ) ;
#109870 = CARTESIAN_POINT ( 'NONE',  ( 18.33041286839819861, 1424.507522803520033, 223.5605584007410016 ) ) ;
#109871 = CARTESIAN_POINT ( 'NONE',  ( -21.42841630977142131, 1524.678872986499073, 234.0212620058165385 ) ) ;
#109872 = CARTESIAN_POINT ( 'NONE',  ( 6.947377783174999877, 1517.009964551830080, 213.7374907746170152 ) ) ;
#109873 = CARTESIAN_POINT ( 'NONE',  ( -3.011021552054556238, 1485.803647523245445, 182.4970978269045929 ) ) ;
#109874 = CARTESIAN_POINT ( 'NONE',  ( -11.31259290968401743, 1425.497384986706493, 138.7251079064614032 ) ) ;
#109876 = ORIENTED_EDGE ( 'NONE', *, *, #101553, .F. ) ;
#109875 = CARTESIAN_POINT ( 'NONE',  ( -11.59032152810750027, 1501.222894206809997, 211.2547116848260202 ) ) ;
#109877 = CARTESIAN_POINT ( 'NONE',  ( -9.095131050099999115, 1384.919789133580025, 199.9427535748389744 ) ) ;
#109878 = CARTESIAN_POINT ( 'NONE',  ( -1.565724986139999997, 1508.487491088089882, 220.5488880004989767 ) ) ;
#109879 = CARTESIAN_POINT ( 'NONE',  ( -10.84157467490000037, 1425.079916389830032, 146.2720446874980098 ) ) ;
#109880 = CARTESIAN_POINT ( 'NONE',  ( 19.04231260082879729, 1456.923026149589759, 225.4260409396169962 ) ) ;
#109881 = DIRECTION ( 'NONE',  ( 0.000000000000000000, 1.000000000000000000, 0.000000000000000000 ) ) ;
#109882 = DIRECTION ( 'NONE',  ( 0.9455185755993178454, 0.000000000000000000, -0.3255681544571539243 ) ) ;
#109883 = DIRECTION ( 'NONE',  ( -0.000000000000000000, -1.000000000000000000, -0.000000000000000000 ) ) ;
#109884 = CARTESIAN_POINT ( 'NONE',  ( 7.269326417459999412, 1410.392938076930022, 230.7475538776979818 ) ) ;
#109886 = CARTESIAN_POINT ( 'NONE',  ( -3.912719417411558709, 1422.010005319424181, 137.0999999983282862 ) ) ;
#109885 = CARTESIAN_POINT ( 'NONE',  ( -23.22700599630000085, 1495.365700136630039, 222.7559110526980248 ) ) ;
#109887 = CARTESIAN_POINT ( 'NONE',  ( -32.28466283162143213, 1511.187213306747708, 219.1752493337717738 ) ) ;
#109888 = ORIENTED_EDGE ( 'NONE', *, *, #94937, .T. ) ;
#109889 = CARTESIAN_POINT ( 'NONE',  ( -4.042417815834999928, 1516.904492006980036, 205.6736390534169914 ) ) ;
#109890 = CARTESIAN_POINT ( 'NONE',  ( 6.204617315079999251, 1406.081877976730084, 268.4675683214979927 ) ) ;
#109891 = CARTESIAN_POINT ( 'NONE',  ( -32.38601978689771244, 1523.530870145309336, 216.1237258104784758 ) ) ;
#109892 = B_SPLINE_SURFACE_WITH_KNOTS ( 'NONE', 5, 5, ( 
 ( #59729, #6557, #109030, #32313, #75965, #23884, #49679, #50765, #92211, #57536, #110117, #84362 ),
 ( #93849, #85445, #40708, #67036, #84900, #42926, #101143, #76512, #41263, #110662, #34511, #33955 ),
 ( #51308, #17120, #391, #24437, #68689, #91660, #14935, #15483, #83262, #74880, #100602, #66496 ),
 ( #58625, #92756, #35060, #95524, #1477, #27768, #27221, #70361, #36724, #94398, #78165, #61959 ),
 ( #52439, #78729, #61402, #87125, #18795, #26652, #44584, #60851, #937, #69804, #36177, #45148 ),
 ( #86567, #69242, #103922, #53547, #52991, #60280, #87694, #77625, #43480, #51881, #96074, #9861 ),
 ( #10414, #44029, #103350, #10975, #2044, #35609, #104474, #94976, #105034, #18244, #28324, #19348 ),
 ( #79289, #86017, #70918, #9317, #2599, #102794, #26091, #17678, #56961, #15470, #73202, #98391 ),
 ( #100039, #83247, #108453, #2840, #64828, #40140, #82701, #6542, #13814, #21661, #107892, #49665 ),
 ( #90537, #66479, #36963, #55870, #14371, #5439, #72658, #31734, #48564, #57521, #22757, #91646 ),
 ( #23329, #92197, #30641, #32295, #5990, #14921, #98936, #47999, #47453, #56405, #107346, #74323 ),
 ( #22210, #49115, #65919, #40694, #4881, #74866, #109012, #81577, #106786, #82138, #64268, #100588 ) ),
 .UNSPECIFIED., .F., .F., .F.,
 ( 6, 3, 3, 6 ),
 ( 6, 3, 3, 6 ),
 ( 12.92374750619999979, 13.99906740309999975, 15.76224410990000102, 17.24244726289999718 ),
 ( 0.000000000000000000, 0.3239695544339999955, 0.9719086633019999866, 1.551787865330000127 ),
 .UNSPECIFIED. ) ;
#109893 = CARTESIAN_POINT ( 'NONE',  ( 19.90169804190000136, 1430.300817687629888, 195.1941537691980102 ) ) ;
#109894 = CARTESIAN_POINT ( 'NONE',  ( 19.36767678366642897, 1425.674430346010013, 222.2074193912012277 ) ) ;
#109895 = CARTESIAN_POINT ( 'NONE',  ( -8.203619622988481908, 1387.619530229529573, 218.4591758698915385 ) ) ;
#109896 =( BOUNDED_CURVE ( )  B_SPLINE_CURVE ( 3, ( #34664, #540, #35217, #69403 ),
 .UNSPECIFIED., .F., .F. ) 
 B_SPLINE_CURVE_WITH_KNOTS ( ( 4, 4 ),
 ( 4.160324501940654507, 5.264453772624229977 ),
 .UNSPECIFIED. ) 
 CURVE ( )  GEOMETRIC_REPRESENTATION_ITEM ( )  RATIONAL_B_SPLINE_CURVE ( ( 1.000000000000000000, 0.9009623648433412457, 0.9009623648433412457, 1.000000000000000000 ) ) 
 REPRESENTATION_ITEM ( '' )  );
#109897 = CARTESIAN_POINT ( 'NONE',  ( -1.584158815879999960, 1451.558453897129993, 184.0315954900979989 ) ) ;
#109898 = DIRECTION ( 'NONE',  ( 0.9455185755993177343, 0.000000000000000000, -0.3255681544571540909 ) ) ;
#109899 = CARTESIAN_POINT ( 'NONE',  ( -14.46903053109999959, 1416.198242731890105, 203.7983957840089886 ) ) ;
#109900 = CARTESIAN_POINT ( 'NONE',  ( -14.26903107030000051, 1444.886608432469984, 188.6883752183980221 ) ) ;
#109901 = CARTESIAN_POINT ( 'NONE',  ( -4.004834694394450167, 1485.215656302600109, 197.9145253210909914 ) ) ;
#109902 = CARTESIAN_POINT ( 'NONE',  ( -16.22196899596580266, 1419.732669852162189, 209.9109564629500824 ) ) ;
#109903 = CARTESIAN_POINT ( 'NONE',  ( -4.158099799109999495, 1497.082135898890101, 220.0114517002990056 ) ) ;
#109904 = CARTESIAN_POINT ( 'NONE',  ( 1.458953924596269935, 1496.945680665030068, 181.5568043570760324 ) ) ;
#109905 = CYLINDRICAL_SURFACE ( 'NONE', #97976, 2.999999999999995115 ) ;
#109906 = CIRCLE ( 'NONE', #32997, 2.000000000000001776 ) ;
#109907 = CARTESIAN_POINT ( 'NONE',  ( 10.57472631152969988, 1481.432876148939840, 209.0048588833070085 ) ) ;
#109908 = LINE ( 'NONE', #34296, #39970 ) ;
#109909 = CARTESIAN_POINT ( 'NONE',  ( -7.053447956369999439, 1475.362404503930065, 269.0260191948979696 ) ) ;
#109910 = CARTESIAN_POINT ( 'NONE',  ( -30.15954682509861584, 1524.412928176728883, 195.8337490977937989 ) ) ;
#109911 = CARTESIAN_POINT ( 'NONE',  ( -13.20758818459541395, 1513.543667424516116, 192.3358642619628256 ) ) ;
#109912 = AXIS2_PLACEMENT_3D ( 'NONE', #35655, #60893, #87169 ) ;
#109913 = CARTESIAN_POINT ( 'NONE',  ( 17.60566278643909754, 1410.878816881569946, 223.9222694885750116 ) ) ;
#109914 = CARTESIAN_POINT ( 'NONE',  ( -48.31785227133409677, 1384.748160175390012, 258.2760858809979823 ) ) ;
#109915 = CARTESIAN_POINT ( 'NONE',  ( -107.4307047400000101, 1391.913060387289988, 300.8770155100590387 ) ) ;
#109916 = AXIS2_PLACEMENT_3D ( 'NONE', #16365, #67929, #76307 ) ;
#109917 = CARTESIAN_POINT ( 'NONE',  ( 12.15368974863659979, 1416.134159098650116, 223.4664122540619928 ) ) ;
#109918 = B_SPLINE_SURFACE_WITH_KNOTS ( 'NONE', 5, 5, ( 
 ( #72059, #106175, #55799, #29455, #56331, #63651, #38408, #97766, #21038 ),
 ( #46845, #89374, #80974, #106712, #30002, #4804, #73129, #49592, #74792 ),
 ( #76428, #59642, #84811, #24891, #7570, #34427, #51228, #6471, #75884 ),
 ( #40621, #91581, #58543, #59098, #15946, #32767, #17030, #42833, #102168 ),
 ( #41724, #24357, #110032, #68057, #33308, #67502, #93222, #68600, #7019 ),
 ( #16489, #76994, #15403, #83181, #50679, #66950, #8656, #101606, #8110 ) ),
 .UNSPECIFIED., .F., .F., .F.,
 ( 6, 6 ),
 ( 6, 3, 6 ),
 ( 32.85731390589999990, 45.45696239520000148 ),
 ( 0.000000000000000000, 1.000000000000000000, 2.000000000000000000 ),
 .UNSPECIFIED. ) ;
#109919 = CARTESIAN_POINT ( 'NONE',  ( -107.2490594869999967, 1379.226189117420063, 299.5843691631590104 ) ) ;
#109920 = DIRECTION ( 'NONE',  ( -1.755985294532469921E-16, 1.000000000000000000, -1.338183447452831989E-16 ) ) ;
#109921 = DIRECTION ( 'NONE',  ( 0.000000000000000000, 1.000000000000000000, 0.000000000000000000 ) ) ;
#109922 = CARTESIAN_POINT ( 'NONE',  ( -20.89362284670000136, 1409.642681774629864, 203.1985663301079796 ) ) ;
#109923 = CARTESIAN_POINT ( 'NONE',  ( -9.715864373837542090, 1380.601324416629950, 201.4379534463959089 ) ) ;
#109924 = EDGE_CURVE ( 'NONE', #48151, #68701, #102043, .T. ) ;
#109925 = CARTESIAN_POINT ( 'NONE',  ( 12.45034049356619832, 1421.619540909540092, 207.5029415923690124 ) ) ;
#109926 = CARTESIAN_POINT ( 'NONE',  ( 10.46048277684489847, 1479.162378809809979, 206.0229427181779727 ) ) ;
#109927 = EDGE_CURVE ( 'NONE', #22669, #22237, #102988, .T. ) ;
#109928 = B_SPLINE_SURFACE_WITH_KNOTS ( 'NONE', 5, 5, ( 
 ( #41308, #81634, #49171, #107951, #107398, #74925 ),
 ( #31243, #48624, #14427, #21716, #31793, #6598 ),
 ( #65427, #91151, #82755, #108506, #58120, #6047 ),
 ( #40198, #75481, #83852, #13316, #23387, #47511 ),
 ( #100106, #30694, #109075, #30134, #65984, #57577 ),
 ( #91703, #39080, #14976, #99534, #64325, #4936 ),
 ( #22261, #66535, #100640, #92254, #56462, #15524 ),
 ( #90595, #7152, #13872, #24481, #58667, #8233 ),
 ( #43524, #60894, #93348, #33430, #92803, #8787 ) ),
 .UNSPECIFIED., .F., .F., .F.,
 ( 6, 3, 6 ),
 ( 6, 6 ),
 ( 2.998553390235009886, 5.159116185979999436, 7.319678981714989874 ),
 ( -0.0004280697249928139899, 2.000000000000000000 ),
 .UNSPECIFIED. ) ;
#109929 = CARTESIAN_POINT ( 'NONE',  ( 0.8167354255590000278, 1432.353341358199941, 150.3995506339979897 ) ) ;
#109930 = CARTESIAN_POINT ( 'NONE',  ( -17.47028495609999865, 1442.689969983390029, 219.3627138812989870 ) ) ;
#109931 = CARTESIAN_POINT ( 'NONE',  ( 16.49871405536215363, 1525.320849883639994, 181.2023611689214135 ) ) ;
#109932 = CARTESIAN_POINT ( 'NONE',  ( -16.53114280955439952, 1465.611523215409989, 220.7423225738290000 ) ) ;
#109934 = DIRECTION ( 'NONE',  ( -1.000000000000000000, 0.000000000000000000, 0.000000000000000000 ) ) ;
#109933 = CARTESIAN_POINT ( 'NONE',  ( -16.14867264346439768, 1416.534170367229990, 209.2886075942629986 ) ) ;
#109935 = CARTESIAN_POINT ( 'NONE',  ( 11.71530569028189994, 1426.709924042370176, 142.6142981130810199 ) ) ;
#109936 = CARTESIAN_POINT ( 'NONE',  ( 16.92737834737011582, 1525.317349363549965, 236.7941106564731513 ) ) ;
#109937 = CARTESIAN_POINT ( 'NONE',  ( -4.517196230222677578, 1517.051704408389924, 190.6118719775071781 ) ) ;
#109938 = CARTESIAN_POINT ( 'NONE',  ( 7.543547206879660294, 1448.836622091779873, 202.0922639109040233 ) ) ;
#109939 = CARTESIAN_POINT ( 'NONE',  ( -17.12480635412540053, 1507.616838219199963, 224.4390396745509975 ) ) ;
#109940 = CARTESIAN_POINT ( 'NONE',  ( 5.001338628314999646, 1516.911981270829983, 203.3378372969070256 ) ) ;
#109941 = FACE_OUTER_BOUND ( 'NONE', #30534, .T. ) ;
#109942 = CARTESIAN_POINT ( 'NONE',  ( -10.63125103579607078, 1398.228151311645888, 201.6093364865327544 ) ) ;
#109943 = CARTESIAN_POINT ( 'NONE',  ( 15.65821248573499780, 1513.518111364920060, 194.4220667106669964 ) ) ;
#109944 = FACE_BOUND ( 'NONE', #85673, .T. ) ;
#109945 = CARTESIAN_POINT ( 'NONE',  ( -40.62420891447809623, 1380.117468965909893, 228.1401504654660073 ) ) ;
#109946 = CARTESIAN_POINT ( 'NONE',  ( 20.84681744068790010, 1509.577347247510033, 229.6818225510970137 ) ) ;
#109948 = EDGE_LOOP ( 'NONE', ( #106643, #77036, #88095, #68216 ) ) ;
#109947 = CARTESIAN_POINT ( 'NONE',  ( -43.37329540369329806, 1379.677816877510168, 233.3348431341099740 ) ) ;
#109949 = EDGE_LOOP ( 'NONE', ( #26201, #818, #90987, #55394 ) ) ;
#109950 = CARTESIAN_POINT ( 'NONE',  ( 11.49040827066960091, 1434.209370592019923, 151.3710404996469947 ) ) ;
#109951 = CARTESIAN_POINT ( 'NONE',  ( -4.919915858649999585, 1396.145435506330159, 220.1243708699980175 ) ) ;
#109952 = ORIENTED_EDGE ( 'NONE', *, *, #7636, .T. ) ;
#109953 = CARTESIAN_POINT ( 'NONE',  ( -106.4659219139999919, 1378.913060387289988, 306.4416122446589839 ) ) ;
#109954 = VECTOR ( 'NONE', #46209, 1000.000000000000114 ) ;
#109955 = CARTESIAN_POINT ( 'NONE',  ( 22.20822569604427343, 1509.700626114282386, 228.6180359268219320 ) ) ;
#109956 = CARTESIAN_POINT ( 'NONE',  ( -4.987078442593329441, 1508.551704408389924, 211.6097810465890063 ) ) ;
#109958 = CARTESIAN_POINT ( 'NONE',  ( -14.35518320136639936, 1509.483853104240097, 182.9676327163749932 ) ) ;
#109957 = CARTESIAN_POINT ( 'NONE',  ( 2.156155154889999981, 1445.629270856190033, 199.6471593918289784 ) ) ;
#109959 = DIRECTION ( 'NONE',  ( 0.000000000000000000, 0.000000000000000000, 1.000000000000000000 ) ) ;
#109960 = CARTESIAN_POINT ( 'NONE',  ( 1.151973313230000073, 1429.774640056330099, 184.3913675471979730 ) ) ;
#109961 = LINE ( 'NONE', #33240, #60453 ) ;
#109962 = CARTESIAN_POINT ( 'NONE',  ( -2.795964621609999590, 1422.864594294989956, 191.4386244948990168 ) ) ;
#109963 =( NAMED_UNIT ( * ) PLANE_ANGLE_UNIT ( ) SI_UNIT ( $, .RADIAN. ) );
#109964 = CARTESIAN_POINT ( 'NONE',  ( 3.572247405320189806, 1396.037806015820024, 198.6941501537289980 ) ) ;
#109966 = CIRCLE ( 'NONE', #97489, 1.500287545630077490 ) ;
#109965 = CARTESIAN_POINT ( 'NONE',  ( 1.552659050380000183, 1415.628674276829770, 190.6570100179979761 ) ) ;
#109967 = CARTESIAN_POINT ( 'NONE',  ( 11.29851010420000001, 1432.096855580479996, 151.5187265218980315 ) ) ;
#109968 = CARTESIAN_POINT ( 'NONE',  ( 17.22592475670000312, 1443.501467202829872, 162.9227486557980171 ) ) ;
#109969 = ORIENTED_EDGE ( 'NONE', *, *, #30123, .F. ) ;
#109970 = CARTESIAN_POINT ( 'NONE',  ( 13.09831360813569923, 1434.825884568560241, 149.1955092924029884 ) ) ;
#109971 = ORIENTED_EDGE ( 'NONE', *, *, #69870, .F. ) ;
#109972 = ORIENTED_EDGE ( 'NONE', *, *, #18142, .T. ) ;
#109973 = CARTESIAN_POINT ( 'NONE',  ( -18.54207416890000104, 1507.885690544229874, 229.7224895538980149 ) ) ;
#109974 = CARTESIAN_POINT ( 'NONE',  ( -8.652254019400000828, 1463.299883665429888, 235.0794778895980244 ) ) ;
#109975 = CARTESIAN_POINT ( 'NONE',  ( 21.08794113720000141, 1497.248615914389802, 211.1864905400789780 ) ) ;
#109976 = CARTESIAN_POINT ( 'NONE',  ( 0.01073129396420149928, 1516.939491476980038, 216.4539099096770087 ) ) ;
#109977 = CARTESIAN_POINT ( 'NONE',  ( -7.902635355081809365, 1511.989348023233788, 212.1516878991907333 ) ) ;
#109978 = EDGE_CURVE ( 'NONE', #72755, #14771, #85999, .T. ) ;
#109979 = CARTESIAN_POINT ( 'NONE',  ( -12.33321046680000066, 1502.561053867989813, 208.9929973234150111 ) ) ;
#109980 = DIRECTION ( 'NONE',  ( -0.4544580288560248760, -1.636314548565651616E-16, -0.8907681516580486791 ) ) ;
#109981 = CARTESIAN_POINT ( 'NONE',  ( -25.65041448810000091, 1375.250345454859826, 213.2122020707489867 ) ) ;
#109982 = ADVANCED_FACE ( 'NONE', ( #7217 ), #5562, .F. ) ;
#109983 = ORIENTED_EDGE ( 'NONE', *, *, #61139, .T. ) ;
#109984 = CARTESIAN_POINT ( 'NONE',  ( 1.702405985064999960, 1516.999105586269934, 205.8518611507970206 ) ) ;
#109985 = ORIENTED_EDGE ( 'NONE', *, *, #20651, .F. ) ;
#109986 = CARTESIAN_POINT ( 'NONE',  ( -104.1899534433839989, 1379.825714327339938, 304.5166623431679795 ) ) ;
#109987 = CARTESIAN_POINT ( 'NONE',  ( -18.64442766460000200, 1507.939506224430033, 229.7217055948979976 ) ) ;
#109988 = CARTESIAN_POINT ( 'NONE',  ( -2.747668638985504952, 1410.389839720919781, 269.3346462040586857 ) ) ;
#109989 = CARTESIAN_POINT ( 'NONE',  ( 7.855403984495000103, 1514.254015528269974, 215.9093767484969817 ) ) ;
#109991 = EDGE_LOOP ( 'NONE', ( #20157, #73103, #73211, #32533 ) ) ;
#109990 = CARTESIAN_POINT ( 'NONE',  ( -0.1222452018727299833, 1415.427621830080170, 226.6817715979609886 ) ) ;
#109992 = CARTESIAN_POINT ( 'NONE',  ( 24.46211382750000141, 1438.319209241250064, 213.4123708239580139 ) ) ;
#109993 = CARTESIAN_POINT ( 'NONE',  ( -0.03314839539225959697, 1508.987035968580130, 209.1276091456630013 ) ) ;
#109994 = AXIS2_PLACEMENT_3D ( 'NONE', #6125, #48154, #47054 ) ;
#109995 = DIRECTION ( 'NONE',  ( 1.000000000000000000, 0.000000000000000000, 0.000000000000000000 ) ) ;
#109996 = DIRECTION ( 'NONE',  ( -0.9996573249755574819, 0.02617694830786557875, 0.000000000000000000 ) ) ;
#109997 = CARTESIAN_POINT ( 'NONE',  ( -2.285487619494999567, 1517.001127920769704, 213.1661676502270097 ) ) ;
#109998 = CARTESIAN_POINT ( 'NONE',  ( 24.05620271129999921, 1410.714389761430084, 209.4728325500950348 ) ) ;
#109999 = CARTESIAN_POINT ( 'NONE',  ( -22.37111836880000126, 1509.698977978930088, 189.8981514860979871 ) ) ;
#110000 = CARTESIAN_POINT ( 'NONE',  ( -16.66966706706500290, 1516.995662938509895, 194.6788146269670108 ) ) ;
#110001 = CARTESIAN_POINT ( 'NONE',  ( -3.251611363945000388, 1516.779243033999819, 211.4202154400570066 ) ) ;
#110002 = CARTESIAN_POINT ( 'NONE',  ( 9.785296660211628250, 1435.228160504780135, 208.4213188007680060 ) ) ;
#110003 = CARTESIAN_POINT ( 'NONE',  ( 0.06395050066389999788, 1420.208574609930110, 183.9020924998980036 ) ) ;
#110004 = CARTESIAN_POINT ( 'NONE',  ( 0.9810389212584773588, 1409.219252835773659, 232.2248046168253381 ) ) ;
#110006 = ORIENTED_EDGE ( 'NONE', *, *, #40792, .T. ) ;
#110005 = CARTESIAN_POINT ( 'NONE',  ( -64.63783698019999235, 1389.443172118360053, 283.2195019318589857 ) ) ;
#110007 = CARTESIAN_POINT ( 'NONE',  ( -52.46234346565999829, 1385.107285400780029, 266.7644260104040086 ) ) ;
#110008 = B_SPLINE_SURFACE_WITH_KNOTS ( 'NONE', 5, 1, ( 
 ( #28073, #10737 ),
 ( #20214, #71217 ),
 ( #36475, #80688 ),
 ( #28630, #30267 ),
 ( #105341, #106979 ),
 ( #53301, #62261 ) ),
 .UNSPECIFIED., .F., .F., .F.,
 ( 6, 6 ),
 ( 2, 2 ),
 ( 0.000000000000000000, 3.599196727790000327 ),
 ( 0.000000000000000000, 14.00000000000000000 ),
 .UNSPECIFIED. ) ;
#110009 = CARTESIAN_POINT ( 'NONE',  ( -1.621602494910000178E-09, 1472.348800621829923, 259.9484879168979887 ) ) ;
#110010 = CARTESIAN_POINT ( 'NONE',  ( -113.4000000000000057, 1309.713060387289943, 304.2218459572590064 ) ) ;
#110011 = SPHERICAL_SURFACE ( 'NONE', #87996, 18.16666666670000296 ) ;
#110012 = CARTESIAN_POINT ( 'NONE',  ( -5.429836194910000025, 1436.698278407169937, 154.7014982151980291 ) ) ;
#110013 = CARTESIAN_POINT ( 'NONE',  ( -23.75643893390000017, 1446.680031664370063, 215.2230810373079919 ) ) ;
#110014 = CARTESIAN_POINT ( 'NONE',  ( 4.363122647530000009, 1407.471318475729959, 121.6099336315979969 ) ) ;
#110016 = CARTESIAN_POINT ( 'NONE',  ( -8.023236064449998040, 1384.902848846080133, 218.7875339973990094 ) ) ;
#110015 = CARTESIAN_POINT ( 'NONE',  ( -5.779627092215000594, 1516.977993847330026, 216.8424961055369806 ) ) ;
#110017 = CARTESIAN_POINT ( 'NONE',  ( -9.942029349575120634, 1448.220099355010007, 209.0865656338810084 ) ) ;
#110018 = CARTESIAN_POINT ( 'NONE',  ( -108.2726263712360009, 1382.330192459420005, 310.4990597502870173 ) ) ;
#110019 = EDGE_LOOP ( 'NONE', ( #91059, #65183, #12709, #96050 ) ) ;
#110020 = CARTESIAN_POINT ( 'NONE',  ( 4.033653264325000265, 1517.028034847769959, 202.5611037067669997 ) ) ;
#110021 = CARTESIAN_POINT ( 'NONE',  ( 28.77213280029999964, 1509.917805404229966, 206.8662417159980293 ) ) ;
#110022 = CARTESIAN_POINT ( 'NONE',  ( -4.494715636143079854E-06, 1472.045054924830083, 270.0713875376969781 ) ) ;
#110023 = FACE_OUTER_BOUND ( 'NONE', #101534, .T. ) ;
#110024 = DIRECTION ( 'NONE',  ( -0.8090169943751635007, 0.000000000000000000, -0.5877852522921759304 ) ) ;
#110025 = CARTESIAN_POINT ( 'NONE',  ( 4.216418746870000511, 1466.253355729990062, 218.9008380672689782 ) ) ;
#110026 = CARTESIAN_POINT ( 'NONE',  ( 14.68860525048159715, 1420.364114750980889, 228.1328174510751694 ) ) ;
#110027 = CARTESIAN_POINT ( 'NONE',  ( 29.68682351698860344, 1436.863057280969997, 136.6924149577619971 ) ) ;
#110028 = CARTESIAN_POINT ( 'NONE',  ( 39.55339567453099647, 1446.835654864889875, 136.6686472316449965 ) ) ;
#110029 = CARTESIAN_POINT ( 'NONE',  ( 20.23078144684548718, 1506.575640308540414, 218.0217183349242589 ) ) ;
#110030 = CARTESIAN_POINT ( 'NONE',  ( -43.12842832595762133, 1452.290486921479896, 269.0450826265717410 ) ) ;
#110031 = CARTESIAN_POINT ( 'NONE',  ( -109.1662451990000022, 1385.640949607019820, 297.1854764981590051 ) ) ;
#110032 = CARTESIAN_POINT ( 'NONE',  ( 10.69931594910000072, 1509.229557744529984, 182.5718536335980104 ) ) ;
#110033 = CARTESIAN_POINT ( 'NONE',  ( -21.78062404853642064, 1524.843178112495480, 184.6507237701596580 ) ) ;
#110034 = AXIS2_PLACEMENT_3D ( 'NONE', #51594, #66762, #74600 ) ;
#110035 =( BOUNDED_CURVE ( )  B_SPLINE_CURVE ( 3, ( #58310, #24659, #30884, #99732 ),
 .UNSPECIFIED., .F., .F. ) 
 B_SPLINE_CURVE_WITH_KNOTS ( ( 4, 4 ),
 ( 0.003816089188682000085, 0.02499446558039379943 ),
 .UNSPECIFIED. ) 
 CURVE ( )  GEOMETRIC_REPRESENTATION_ITEM ( )  RATIONAL_B_SPLINE_CURVE ( ( 1.000000000000000000, 0.9999626233803757813, 0.9999626233803757813, 1.000000000000000000 ) ) 
 REPRESENTATION_ITEM ( '' )  );
#110036 = CARTESIAN_POINT ( 'NONE',  ( -38.81129961821237373, 1452.619208713947955, 269.5899325438009555 ) ) ;
#110037 = ORIENTED_EDGE ( 'NONE', *, *, #97878, .T. ) ;
#110038 = LINE ( 'NONE', #24895, #1447 ) ;
#110039 = CARTESIAN_POINT ( 'NONE',  ( -42.31040111291903827, 1428.094689011069022, 269.0673684584702414 ) ) ;
#110040 = CARTESIAN_POINT ( 'NONE',  ( -3.803002609304670045, 1508.880967335730247, 213.6144902421019935 ) ) ;
#110041 = CARTESIAN_POINT ( 'NONE',  ( 16.74002313133309983, 1501.349413233449923, 188.2918665645719614 ) ) ;
#110042 = CARTESIAN_POINT ( 'NONE',  ( -0.1199520561000000096, 1415.404073712830041, 233.4412207362979927 ) ) ;
#110043 = CARTESIAN_POINT ( 'NONE',  ( 11.46977278200000150, 1502.214325488189843, 209.8002689844269923 ) ) ;
#110044 = CARTESIAN_POINT ( 'NONE',  ( -13.09467007730180832, 1444.805799845968522, 186.4212311027728219 ) ) ;
#110045 = B_SPLINE_SURFACE_WITH_KNOTS ( 'NONE', 5, 5, ( 
 ( #67487, #25984, #51215, #34412, #85346, #42263, #1372, #68584, #103826 ),
 ( #9758, #43379, #86465, #18693, #76411, #102689, #8642, #94872, #102152 ),
 ( #43922, #93738, #9221, #110565, #35514, #18149, #77528, #42818, #60749 ),
 ( #59084, #60184, #52890, #87018, #110018, #52344, #10310, #33294, #50665 ),
 ( #34957, #17016, #69707, #94301, #103245, #25431, #69141, #17578, #51779 ),
 ( #68042, #59627, #85917, #16474, #27126, #84797, #75868, #101590, #24876 ),
 ( #93204, #45605, #29319, #80287, #3603, #104934, #46157, #88146, #62408 ),
 ( #97091, #70267, #62979, #97635, #11434, #36624, #44483, #37180, #27672 ),
 ( #20904, #71376, #36082, #79747, #96536, #3054, #19810, #53447, #63519 ),
 ( #55105, #89229, #71930, #20356, #37726, #12525, #87593, #105488, #54016 ),
 ( #2503, #11976, #106042, #28221, #28779, #10881, #46703, #80833, #54561 ),
 ( #78629, #1944, #88695, #104376, #61857, #95977, #19238, #45053, #79197 ),
 ( #70822, #60715, #794, #85880, #42782, #43346, #27094, #69672, #103794 ),
 ( #16983, #51182, #94267, #75836, #34379, #93168, #109986, #94836, #33263 ),
 ( #42232, #84219, #50632, #77494, #78032, #102652, #41677, #76941, #34923 ) ),
 .UNSPECIFIED., .F., .F., .F.,
 ( 6, 3, 3, 3, 6 ),
 ( 6, 3, 6 ),
 ( 7.295781771626849377, 12.20883758960000165, 16.12185770279999986, 21.25293827189999973, 26.14845333426159968 ),
 ( 0.000000000000000000, 1.000000000000000000, 2.002578320861649885 ),
 .UNSPECIFIED. ) ;
#110046 = CARTESIAN_POINT ( 'NONE',  ( -9.872142711616779920, 1438.638380141409925, 210.3201327332649839 ) ) ;
#110047 = CARTESIAN_POINT ( 'NONE',  ( -3.829164871871630016, 1515.551704201149960, 211.4518032920690018 ) ) ;
#110048 = DIRECTION ( 'NONE',  ( -0.9455185755993178454, 0.000000000000000000, 0.3255681544571539243 ) ) ;
#110049 = CARTESIAN_POINT ( 'NONE',  ( -7.843739966816699827, 1451.394674706588376, 152.9912049652007795 ) ) ;
#110050 = CARTESIAN_POINT ( 'NONE',  ( -16.40028066370599902, 1414.913057860449953, 208.9659912899270182 ) ) ;
#110051 = CARTESIAN_POINT ( 'NONE',  ( 25.44703061359999907, 1435.463407790350175, 136.0943506319979974 ) ) ;
#110052 = CARTESIAN_POINT ( 'NONE',  ( 2.325731103684999912, 1511.751588929339960, 216.7056378762670192 ) ) ;
#110053 = EDGE_LOOP ( 'NONE', ( #36279, #31286, #38096, #45556, #77654, #57388, #43380, #6280, #22783 ) ) ;
#110054 = CARTESIAN_POINT ( 'NONE',  ( -0.3610913072858399908, 1416.520646088689773, 191.0797031976740072 ) ) ;
#110055 = CARTESIAN_POINT ( 'NONE',  ( 2.907016575484743903, 1493.671177366619531, 219.9120732454466918 ) ) ;
#110056 = ORIENTED_EDGE ( 'NONE', *, *, #90057, .T. ) ;
#110057 = ORIENTED_EDGE ( 'NONE', *, *, #13060, .F. ) ;
#110058 = CARTESIAN_POINT ( 'NONE',  ( 2.876961725570000183, 1499.580235354990009, 230.2170217437989947 ) ) ;
#110059 = CARTESIAN_POINT ( 'NONE',  ( 6.149909982967501243, 1516.731221219415374, 204.8276256237976440 ) ) ;
#110061 = CARTESIAN_POINT ( 'NONE',  ( -27.78550214639999894, 1444.553010677309885, 231.7059331051979996 ) ) ;
#110060 = CARTESIAN_POINT ( 'NONE',  ( 3.899433454979999603, 1454.070828365190209, 217.6618255207390007 ) ) ;
#110062 = CARTESIAN_POINT ( 'NONE',  ( -20.60186841840000227, 1507.925363662629934, 190.3874517655979730 ) ) ;
#110063 = CARTESIAN_POINT ( 'NONE',  ( -0.2658540493943280514, 1507.120020986029886, 237.3289608297170048 ) ) ;
#110064 = CARTESIAN_POINT ( 'NONE',  ( -12.31034457511139912, 1378.376182853990031, 209.7966525762110166 ) ) ;
#110065 = CARTESIAN_POINT ( 'NONE',  ( -2.497537340894446789, 1421.157573660655089, 184.9539988175752114 ) ) ;
#110066 = CARTESIAN_POINT ( 'NONE',  ( 7.012556801809999740, 1423.949223476430006, 213.3686902051989875 ) ) ;
#110067 = CARTESIAN_POINT ( 'NONE',  ( -24.68077627620000314, 1437.736158917830153, 210.5119845518579780 ) ) ;
#110068 = CARTESIAN_POINT ( 'NONE',  ( -3.932260160163730145, 1453.946481855800130, 199.4130354687199826 ) ) ;
#110069 = CARTESIAN_POINT ( 'NONE',  ( 1.812234975289999994, 1451.648984562529904, 183.4223051748979856 ) ) ;
#110070 = CARTESIAN_POINT ( 'NONE',  ( 6.502686550879601235, 1362.555198829660185, 207.6218459616988241 ) ) ;
#110071 = CARTESIAN_POINT ( 'NONE',  ( -7.082378735300329353, 1478.706589098139830, 211.5813507964070084 ) ) ;
#110073 = ORIENTED_EDGE ( 'NONE', *, *, #65043, .T. ) ;
#110072 = DIRECTION ( 'NONE',  ( -1.755985294532469921E-16, 1.000000000000000000, -1.338183447452831989E-16 ) ) ;
#110074 = ORIENTED_EDGE ( 'NONE', *, *, #77433, .F. ) ;
#110075 = EDGE_CURVE ( 'NONE', #41356, #22976, #31855, .T. ) ;
#110076 = CIRCLE ( 'NONE', #61843, 0.9999999999999074074 ) ;
#110077 = DIRECTION ( 'NONE',  ( -1.755985294532469921E-16, 1.000000000000000000, -1.338183447452831989E-16 ) ) ;
#110078 = CARTESIAN_POINT ( 'NONE',  ( -4.112861762809999711, 1471.442216374229929, 269.6167275226979996 ) ) ;
#110079 = CARTESIAN_POINT ( 'NONE',  ( 13.01067395679109318, 1434.788365234622461, 146.9710503661439134 ) ) ;
#110080 = CARTESIAN_POINT ( 'NONE',  ( -113.4000000000000057, 1314.643966242390206, 314.8853230801589689 ) ) ;
#110081 = CARTESIAN_POINT ( 'NONE',  ( 17.23446452470000168, 1453.313060387329870, 198.3385369815979971 ) ) ;
#110082 = CARTESIAN_POINT ( 'NONE',  ( -8.604091700990000646, 1384.887133332230178, 199.8687248843490067 ) ) ;
#110083 = ADVANCED_FACE ( 'NONE', ( #48684 ), #99881, .T. ) ;
#110084 = B_SPLINE_SURFACE_WITH_KNOTS ( 'NONE', 5, 5, ( 
 ( #81313, #81865, #6808, #23050, #32579, #72938 ),
 ( #22485, #66755, #48852, #65644, #100329, #39876 ),
 ( #5166, #6269, #109295, #39324, #40967, #31464 ),
 ( #30915, #65094, #64555, #99206, #56685, #57258 ),
 ( #40416, #99760, #23614, #90264, #108172, #75147 ),
 ( #4628, #91923, #38764, #107078, #90821, #14103 ) ),
 .UNSPECIFIED., .F., .F., .F.,
 ( 6, 6 ),
 ( 6, 6 ),
 ( 0.8310181115189999579, 1.360694072900000107 ),
 ( 0.000000000000000000, 2.000000000000000000 ),
 .UNSPECIFIED. ) ;
#110085 = CARTESIAN_POINT ( 'NONE',  ( 0.000000000000000000, 0.000000000000000000, 0.000000000000000000 ) ) ;
#110086 = DIRECTION ( 'NONE',  ( 0.000000000000000000, -1.000000000000000000, 0.000000000000000000 ) ) ;
#110087 = CARTESIAN_POINT ( 'NONE',  ( 6.765843366259869818, 1369.561165281723333, 210.6218459617030021 ) ) ;
#110088 = CARTESIAN_POINT ( 'NONE',  ( 28.77729953137099983, 1509.917985831029910, 206.0039978706130057 ) ) ;
#110089 = CARTESIAN_POINT ( 'NONE',  ( -8.302495336826780203, 1407.043756550310036, 269.4752719639240013 ) ) ;
#110090 = CARTESIAN_POINT ( 'NONE',  ( -13.47774476437770019, 1434.953314453749954, 149.0527405834899923 ) ) ;
#110091 = ORIENTED_EDGE ( 'NONE', *, *, #44010, .F. ) ;
#110092 = CARTESIAN_POINT ( 'NONE',  ( -12.56636063060000019, 1391.397300678690044, 209.2272092290610033 ) ) ;
#110093 = VERTEX_POINT ( 'NONE', #69065 ) ;
#110094 = ORIENTED_EDGE ( 'NONE', *, *, #20171, .T. ) ;
#110095 = CARTESIAN_POINT ( 'NONE',  ( 4.743542324458120518, 1422.215256140715837, 184.1963053778127914 ) ) ;
#110096 = CARTESIAN_POINT ( 'NONE',  ( 9.862951377358559313, 1522.051704408389924, 189.8497022443989977 ) ) ;
#110097 = CARTESIAN_POINT ( 'NONE',  ( -3.447264387095000160, 1516.858765657450249, 212.5828932618570093 ) ) ;
#110098 = CARTESIAN_POINT ( 'NONE',  ( -18.56504074879999777, 1470.474274205130087, 190.0315648486979967 ) ) ;
#110099 = CARTESIAN_POINT ( 'NONE',  ( -17.91320311087370243, 1507.617078275819949, 229.7141967011020256 ) ) ;
#110100 = VERTEX_POINT ( 'NONE', #24259 ) ;
#110101 = DIRECTION ( 'NONE',  ( 1.000000000000000000, 0.000000000000000000, 0.000000000000000000 ) ) ;
#110102 = AXIS2_PLACEMENT_3D ( 'NONE', #103981, #61459, #86627 ) ;
#110103 = CARTESIAN_POINT ( 'NONE',  ( 7.714371502985000184, 1516.738222552470233, 203.3422428319769892 ) ) ;
#110104 = B_SPLINE_CURVE_WITH_KNOTS ( 'NONE', 3,
 ( #39619, #100066, #16574, #108472, #41815, #74887, #16041, #15489, #109037, #84369, #75971, #75444, #6565 ),
 .UNSPECIFIED., .F., .F.,
 ( 4, 2, 2, 1, 2, 2, 4 ),
 ( 0.000000000000000000, 0.2500000000001970091, 0.3750000000002713385, 0.4375000000003243517, 0.4687500000002935430, 0.5000000000002627898, 1.000000000000000000 ),
 .UNSPECIFIED. ) ;
#110105 = CARTESIAN_POINT ( 'NONE',  ( -27.89972997509999786, 1508.077281474930032, 206.8466243103179920 ) ) ;
#110106 = CARTESIAN_POINT ( 'NONE',  ( -4.270560985520866382, 1421.938260711448493, 185.0877191533315909 ) ) ;
#110108 = CIRCLE ( 'NONE', #88454, 0.9999999999999956701 ) ;
#110107 = CARTESIAN_POINT ( 'NONE',  ( -44.53110276769830023, 1384.597785574959971, 217.7731154659030040 ) ) ;
#110109 = CARTESIAN_POINT ( 'NONE',  ( -5.563412915829999861, 1409.046699355029887, 195.8153601168980060 ) ) ;
#110110 = CARTESIAN_POINT ( 'NONE',  ( -116.0327476856711115, 1377.913060387289988, 302.7835693414463663 ) ) ;
#110112 = ORIENTED_EDGE ( 'NONE', *, *, #81848, .T. ) ;
#110111 = DIRECTION ( 'NONE',  ( 0.000000000000000000, 0.000000000000000000, 1.000000000000000000 ) ) ;
#110113 = LINE ( 'NONE', #34508, #15343 ) ;
#110114 = CARTESIAN_POINT ( 'NONE',  ( 21.52036871800000029, 1488.680653137030049, 224.0828341895980031 ) ) ;
#110115 = DIRECTION ( 'NONE',  ( 0.000000000000000000, 1.000000000000000000, 0.000000000000000000 ) ) ;
#110116 = CARTESIAN_POINT ( 'NONE',  ( -10.51083736151210068, 1480.296936587089931, 210.9545377047529939 ) ) ;
#110117 = CARTESIAN_POINT ( 'NONE',  ( -24.97886932509999980, 1436.441184281979986, 137.9166797883979996 ) ) ;
#110118 = CARTESIAN_POINT ( 'NONE',  ( -0.2610041142439999962, 1485.912415289430101, 181.7937759989980009 ) ) ;
#110119 = CARTESIAN_POINT ( 'NONE',  ( 1.717084711415000076, 1516.819260244609950, 211.5980165671369946 ) ) ;
#110120 = CARTESIAN_POINT ( 'NONE',  ( -68.13004150250000635, 1379.747519519559773, 278.8017379516589926 ) ) ;
#110121 = CARTESIAN_POINT ( 'NONE',  ( 5.477776093029999238, 1439.067881875560033, 154.7441050454979745 ) ) ;
#110122 = CARTESIAN_POINT ( 'NONE',  ( 8.927134929145720932, 1436.767706396419953, 210.5802712642290260 ) ) ;
#110123 = CARTESIAN_POINT ( 'NONE',  ( -13.20369377719999981, 1414.913528139930122, 220.1254046489979999 ) ) ;
#110124 = CARTESIAN_POINT ( 'NONE',  ( -7.337297350114999617, 1517.135701590510052, 208.3821536943570152 ) ) ;
#110125 = ORIENTED_EDGE ( 'NONE', *, *, #106228, .F. ) ;
#110126 = CARTESIAN_POINT ( 'NONE',  ( -42.60628462810000627, 1443.705283505679745, 134.0999992373979808 ) ) ;
#110127 = CARTESIAN_POINT ( 'NONE',  ( -10.16145782839999967, 1473.012443313389895, 208.1237237223820387 ) ) ;
#110128 = DIRECTION ( 'NONE',  ( 0.9995238204273075855, -0.03085664269485739394, -3.333398116331567129E-08 ) ) ;
#110129 = ORIENTED_EDGE ( 'NONE', *, *, #38046, .F. ) ;
#110130 = CARTESIAN_POINT ( 'NONE',  ( 20.05410099200000218, 1476.341259462790049, 212.1028602122389941 ) ) ;
#110131 = CARTESIAN_POINT ( 'NONE',  ( -22.81398894436890856, 1509.728857822366308, 227.9950205443984714 ) ) ;
#110132 = CARTESIAN_POINT ( 'NONE',  ( -4.094299838186481466, 1441.313231385115614, 184.5078324159681529 ) ) ;
#110133 = CARTESIAN_POINT ( 'NONE',  ( -15.00213922130000022, 1416.331168602359867, 208.3054305177020069 ) ) ;
#110134 = DIRECTION ( 'NONE',  ( 0.1402804634178727861, 0.9901118076173351934, 0.000000000000000000 ) ) ;
#110135 = CARTESIAN_POINT ( 'NONE',  ( 4.127868055549999582, 1487.366509936789953, 197.8725145131990075 ) ) ;
#110136 = DIRECTION ( 'NONE',  ( -1.156023075842281927E-31, 1.000000000000000000, -1.698192320643030073E-16 ) ) ;
#110137 = CARTESIAN_POINT ( 'NONE',  ( -15.08447935729999934, 1409.953164787530113, 226.5286084827979778 ) ) ;
#110139 = DIRECTION ( 'NONE',  ( 1.000000000000000000, 0.000000000000000000, 0.000000000000000000 ) ) ;
#110138 = CARTESIAN_POINT ( 'NONE',  ( -2.480813923114999930, 1517.051603658920158, 214.1347848340070072 ) ) ;
#110140 = CARTESIAN_POINT ( 'NONE',  ( 20.28559703379999846, 1508.605287559729959, 189.2542286951979804 ) ) ;
#110141 = CARTESIAN_POINT ( 'NONE',  ( -4.615017365965000451, 1516.987478262539980, 215.6816440265270103 ) ) ;
#110142 = ORIENTED_EDGE ( 'NONE', *, *, #65451, .F. ) ;
#110143 = CARTESIAN_POINT ( 'NONE',  ( -12.61618840270000064, 1416.831305841230005, 194.9199445040979981 ) ) ;
#110144 = CARTESIAN_POINT ( 'NONE',  ( -17.05626209599999754, 1420.313787275360028, 203.5730941281789796 ) ) ;
#110145 = CARTESIAN_POINT ( 'NONE',  ( 0.8012822335670000129, 1420.474755016030258, 184.0519104804979804 ) ) ;
#110146 = VECTOR ( 'NONE', #61955, 1000.000000000000114 ) ;
#110147 = CIRCLE ( 'NONE', #92243, 5.301724629749982043 ) ;
#110148 = EDGE_CURVE ( 'NONE', #31391, #102452, #82410, .T. ) ;
#110149 = FILL_AREA_STYLE ('',( #10448 ) ) ;
#110150 = CARTESIAN_POINT ( 'NONE',  ( -103.5806803890000083, 1389.940350142260058, 304.1776731731589507 ) ) ;
#110151 = CARTESIAN_POINT ( 'NONE',  ( 8602.628222781668228, 50.13405481564041821, -10923.45535519340592 ) ) ;
#110152 = CARTESIAN_POINT ( 'NONE',  ( 18.19590854888146580, 1512.187213306747481, 180.0410247165184217 ) ) ;
#110153 = CARTESIAN_POINT ( 'NONE',  ( -5.137024739602960466, 1508.240697825915277, 220.3835027126725379 ) ) ;
#110154 = CARTESIAN_POINT ( 'NONE',  ( -32.28466283162165240, 1512.187213306747481, 199.0684425896249081 ) ) ;
#110155 = EDGE_CURVE ( 'NONE', #40901, #76159, #102069, .T. ) ;
#110156 = CARTESIAN_POINT ( 'NONE',  ( 12.03449227190490056, 1491.353386486839781, 206.6667661091970274 ) ) ;
#110157 = CARTESIAN_POINT ( 'NONE',  ( -11.94046459599999999, 1438.194204504490017, 147.6340003373980210 ) ) ;
#110159 = EDGE_CURVE ( 'NONE', #100575, #9577, #101462, .T. ) ;
#110158 = DIRECTION ( 'NONE',  ( 0.9417419115949662300, -0.2378257470769920556, 0.2378257470769920556 ) ) ;
#110160 = CARTESIAN_POINT ( 'NONE',  ( -13.37434658702809998, 1416.899496760530155, 201.3810223920989984 ) ) ;
#110161 = DIRECTION ( 'NONE',  ( 1.755985294532464991E-16, -1.000000000000000000, 1.338183447452830017E-16 ) ) ;
#110162 = ORIENTED_EDGE ( 'NONE', *, *, #34584, .T. ) ;
#110163 = VERTEX_POINT ( 'NONE', #6915 ) ;
#110164 = CARTESIAN_POINT ( 'NONE',  ( 1.546990765144379942, 1416.765224585179794, 190.2255853430220043 ) ) ;
#110165 = FACE_OUTER_BOUND ( 'NONE', #25545, .T. ) ;
#110166 = CARTESIAN_POINT ( 'NONE',  ( -24.40604034560000102, 1441.493461323560041, 212.0691198047580031 ) ) ;
#110167 = CYLINDRICAL_SURFACE ( 'NONE', #36630, 2.000000000000003553 ) ;
#110168 = CARTESIAN_POINT ( 'NONE',  ( -740.1067050508938792, 11216.44053380570222, -1627.040744446347389 ) ) ;
#110169 = CARTESIAN_POINT ( 'NONE',  ( -112.2014361534894817, 1306.413060387289988, 302.0278895525330540 ) ) ;
#110171 = VECTOR ( 'NONE', #51302, 1000.000000000000114 ) ;
#110170 = DIRECTION ( 'NONE',  ( 0.000000000000000000, 1.000000000000000000, -6.123233995736769734E-17 ) ) ;
#110172 = CARTESIAN_POINT ( 'NONE',  ( -17.51543252019589758, 1417.552277257849937, 206.7803077767080140 ) ) ;
#110173 = CARTESIAN_POINT ( 'NONE',  ( -62.79534954047180406, 1383.793091064959981, 285.1732082431380491 ) ) ;
#110174 = CARTESIAN_POINT ( 'NONE',  ( 7.282399919470000427, 1452.222616508330020, 153.1973960492980211 ) ) ;
#110175 = CARTESIAN_POINT ( 'NONE',  ( -26.86204968941349946, 1508.007394745769943, 212.0120970035400205 ) ) ;
#110176 = CARTESIAN_POINT ( 'NONE',  ( 11.57342425378350015, 1492.618401364529973, 211.9083419029999789 ) ) ;
#110178 = VERTEX_POINT ( 'NONE', #32674 ) ;
#110177 = CARTESIAN_POINT ( 'NONE',  ( -14.28619595012664156, 1517.015067828383053, 225.9483486273336155 ) ) ;
#110179 = CARTESIAN_POINT ( 'NONE',  ( 12.78776258895000062, 1416.851343899079893, 222.7045348340550106 ) ) ;
#110180 = CARTESIAN_POINT ( 'NONE',  ( -64.43287619839999536, 1383.188014472239956, 254.0808989357590235 ) ) ;
#110181 = CARTESIAN_POINT ( 'NONE',  ( 4.948068031341160022, 1508.551704408389924, 206.1941938154730281 ) ) ;
#110182 = ORIENTED_EDGE ( 'NONE', *, *, #59709, .T. ) ;
#110183 = ORIENTED_EDGE ( 'NONE', *, *, #4553, .T. ) ;
#110184 = CARTESIAN_POINT ( 'NONE',  ( 15.16579360867039838, 1509.443749158599985, 234.3045273943520215 ) ) ;
#110185 = CARTESIAN_POINT ( 'NONE',  ( -7.973011292860630483, 1385.871086923890061, 218.7772657474099844 ) ) ;
#110186 = CARTESIAN_POINT ( 'NONE',  ( 40.00035472543419957, 1441.740890375260051, 136.9051897632780026 ) ) ;
#110187 = CARTESIAN_POINT ( 'NONE',  ( 4.967684365510000255, 1469.890599266690060, 189.7939106698990201 ) ) ;
#110188 = CARTESIAN_POINT ( 'NONE',  ( 11.70397832847810093, 1479.895218179510039, 210.5107915740969986 ) ) ;
#110189 = CARTESIAN_POINT ( 'NONE',  ( -106.6038969349999945, 1381.976044154610008, 298.3535665123590093 ) ) ;
#110190 = DIRECTION ( 'NONE',  ( 0.000000000000000000, -1.000000000000000000, 0.000000000000000000 ) ) ;
#110191 = CARTESIAN_POINT ( 'NONE',  ( -12.84238138274280061, 1435.935700660240400, 150.8114831378814245 ) ) ;
#110192 = CARTESIAN_POINT ( 'NONE',  ( -14.83447489583599932, 1508.551704408389924, 215.0596454497180048 ) ) ;
#110193 = FACE_OUTER_BOUND ( 'NONE', #41790, .T. ) ;
#110194 = CARTESIAN_POINT ( 'NONE',  ( 2.776832761270000116, 1409.010029526630206, 186.6898676387980061 ) ) ;
#110195 = CARTESIAN_POINT ( 'NONE',  ( 2.669590603778499993, 1486.875611465459997, 197.4822887014510115 ) ) ;
#110196 = CARTESIAN_POINT ( 'NONE',  ( -2.711917821514580051, 1440.323576713389912, 158.1830662651330215 ) ) ;
#110197 = FACE_OUTER_BOUND ( 'NONE', #59647, .T. ) ;
#110198 = ORIENTED_EDGE ( 'NONE', *, *, #13773, .T. ) ;
#110199 = SHAPE_REPRESENTATION ( 'Handle Mounting Screw', ( #21632 ), #107481 ) ;
#110200 = CARTESIAN_POINT ( 'NONE',  ( 20.65265016900000106, 1477.900423433889955, 217.6009028526389955 ) ) ;
#110201 = CARTESIAN_POINT ( 'NONE',  ( -2.446787376320000096, 1432.353341358199941, 150.2884730787980061 ) ) ;
#110202 = CARTESIAN_POINT ( 'NONE',  ( -23.69678315977305871, 1436.213473500231430, 212.2034013915424566 ) ) ;
#110203 = CARTESIAN_POINT ( 'NONE',  ( 22.06852505278052234, 1506.535970898695041, 209.0957427188783981 ) ) ;
#110204 = DIRECTION ( 'NONE',  ( 0.000000000000000000, 1.000000000000000000, 0.000000000000000000 ) ) ;
#110205 = CARTESIAN_POINT ( 'NONE',  ( -3.496551860115360160E-09, 1471.729463454729967, 258.3617253003269525 ) ) ;
#110206 = CARTESIAN_POINT ( 'NONE',  ( -19.96725921898470091, 1487.369853937069820, 190.9830490477359888 ) ) ;
#110208 = EDGE_CURVE ( 'NONE', #81551, #71185, #50290, .T. ) ;
#110207 = CARTESIAN_POINT ( 'NONE',  ( -2.149974513279420130, 1421.471342383219962, 193.6364440172239938 ) ) ;
#110209 = CARTESIAN_POINT ( 'NONE',  ( -0.8130780850230000523, 1417.377578703830068, 235.4819908353979940 ) ) ;
#110210 = CARTESIAN_POINT ( 'NONE',  ( -3.076049692719999840, 1475.159716291190080, 198.5224444241989943 ) ) ;
#110211 = CARTESIAN_POINT ( 'NONE',  ( -107.5382083149999914, 1388.218888600149967, 309.8897308892589990 ) ) ;
#110212 = CARTESIAN_POINT ( 'NONE',  ( 10.01013843233299916, 1469.369181467840008, 209.9819040969830155 ) ) ;
#110213 = CARTESIAN_POINT ( 'NONE',  ( -7.590039838923934745, 1360.846950907609425, 207.6218459616987673 ) ) ;
#110214 = CARTESIAN_POINT ( 'NONE',  ( -46.23755058181890121, 1439.409989939530078, 267.5908672125710268 ) ) ;
#110215 = CARTESIAN_POINT ( 'NONE',  ( 13.50635050315699992, 1508.609632639959955, 233.4266690729490108 ) ) ;
#110216 = CARTESIAN_POINT ( 'NONE',  ( -8.749325254410001307, 1423.947972453919874, 207.8877631365490117 ) ) ;
#110217 = CARTESIAN_POINT ( 'NONE',  ( -2.491655763544999846, 1516.977504706749869, 208.3867361609839861 ) ) ;
#110218 = CARTESIAN_POINT ( 'NONE',  ( 0.000000000000000000, 1413.913060387330006, 217.1218459616979999 ) ) ;
#110219 = CARTESIAN_POINT ( 'NONE',  ( -33.28034951413935971, 1522.382868172863937, 200.8029765415142549 ) ) ;
#110220 = CARTESIAN_POINT ( 'NONE',  ( 7.538936308525870267, 1425.689389508179829, 212.1914861486659731 ) ) ;
#110221 = CARTESIAN_POINT ( 'NONE',  ( -26.59992281200619857, 1451.967265226159952, 135.1794589613959943 ) ) ;
#110222 = ORIENTED_EDGE ( 'NONE', *, *, #18438, .F. ) ;
#110223 = CARTESIAN_POINT ( 'NONE',  ( 3.960029701070000296, 1420.509147081630090, 221.4103262571979940 ) ) ;
#110225 = FACE_OUTER_BOUND ( 'NONE', #74725, .T. ) ;
#110224 = CARTESIAN_POINT ( 'NONE',  ( -10.97486499478319999, 1492.422550449080063, 207.2127083187249923 ) ) ;
#110226 = CARTESIAN_POINT ( 'NONE',  ( 14.45750538832999865, 1416.828039266780024, 196.8520486936070029 ) ) ;
#110227 = CARTESIAN_POINT ( 'NONE',  ( -7.332394679680000704E-08, 1421.529510530429889, 216.2239750317280311 ) ) ;
#110228 = CARTESIAN_POINT ( 'NONE',  ( 17.24398683809999966, 1428.425037375490092, 203.1706303392290067 ) ) ;
#110229 = DIRECTION ( 'NONE',  ( -0.6736849260863841948, 0.000000000000000000, 0.7390186874254148774 ) ) ;
#110230 = CARTESIAN_POINT ( 'NONE',  ( 49.24962907673571522, 1524.382868172863937, 10.34030387146701813 ) ) ;
#110231 = ORIENTED_EDGE ( 'NONE', *, *, #64063, .T. ) ;
#110232 = CARTESIAN_POINT ( 'NONE',  ( -1.204647661935780212, 1410.042122733069846, 269.8655116434729848 ) ) ;
#110233 = CARTESIAN_POINT ( 'NONE',  ( 15.46640642006999933, 1422.315519798870127, 228.3555397929160051 ) ) ;
#110234 = DIRECTION ( 'NONE',  ( -5.980589973904019347E-17, 1.000000000000000000, -1.736889445713099699E-16 ) ) ;
#110235 = ORIENTED_EDGE ( 'NONE', *, *, #87921, .T. ) ;
#110236 = EDGE_LOOP ( 'NONE', ( #6212, #89736, #50115, #97562 ) ) ;
#110237 = CARTESIAN_POINT ( 'NONE',  ( -23.97615151247089926, 1411.113891529490047, 209.8899454678769985 ) ) ;
#110238 = EDGE_CURVE ( 'NONE', #36007, #5947, #184, .T. ) ;
#110239 = ORIENTED_EDGE ( 'NONE', *, *, #2998, .T. ) ;
#110240 = DIRECTION ( 'NONE',  ( 0.000000000000000000, 0.000000000000000000, 1.000000000000000000 ) ) ;
#110241 = DIRECTION ( 'NONE',  ( 0.000000000000000000, 1.000000000000000000, 0.000000000000000000 ) ) ;
#110242 = CARTESIAN_POINT ( 'NONE',  ( -20.44190531641500286, 1488.934990366839884, 192.7748267833920011 ) ) ;
#110244 = CIRCLE ( 'NONE', #101265, 7.975189853890007896 ) ;
#110243 = CARTESIAN_POINT ( 'NONE',  ( -20.24945462270000007, 1415.849806780530116, 220.8573330491979902 ) ) ;
#110245 = B_SPLINE_CURVE_WITH_KNOTS ( 'NONE', 3,
 ( #93039, #15218, #108749, #41555, #7390, #92482, #93580, #8476, #42650, #24710 ),
 .UNSPECIFIED., .F., .F.,
 ( 4, 2, 2, 2, 4 ),
 ( 0.000000000000000000, 0.0007189769279726049766, 0.001437953855945209953, 0.002156930783917814821, 0.002875907711890419906 ),
 .UNSPECIFIED. ) ;
#110246 = CARTESIAN_POINT ( 'NONE',  ( 37.03850270579130211, 1462.024743436390054, 267.2720586370879801 ) ) ;
#110247 = CARTESIAN_POINT ( 'NONE',  ( -4.369720495665090354, 1508.879003890470131, 205.0024468196820067 ) ) ;
#110248 = CARTESIAN_POINT ( 'NONE',  ( -16.45994915654801360, 1421.286113174233151, 226.9925930846744677 ) ) ;
#110249 = CARTESIAN_POINT ( 'NONE',  ( -2.491188396525000126, 1516.733363207009916, 205.0947945262969938 ) ) ;
#110250 = ORIENTED_EDGE ( 'NONE', *, *, #55112, .F. ) ;
#110251 = DIRECTION ( 'NONE',  ( 5.980589973904019347E-17, -1.000000000000000000, 1.736889445713099699E-16 ) ) ;
#110252 = CARTESIAN_POINT ( 'NONE',  ( 15.30266648242040084, 1512.633419863009976, 195.7156704886770342 ) ) ;
#110253 = CARTESIAN_POINT ( 'NONE',  ( 22.71667399460000425, 1409.715173893529936, 208.6485712393049994 ) ) ;
#110254 = VERTEX_POINT ( 'NONE', #205 ) ;
#110255 = CARTESIAN_POINT ( 'NONE',  ( -11.38448554521469980, 1481.434469010069961, 209.9556807158220124 ) ) ;
#110256 = CARTESIAN_POINT ( 'NONE',  ( 27.01380162286760012, 1450.681224429609983, 136.4483868285099959 ) ) ;
#110257 = CARTESIAN_POINT ( 'NONE',  ( -3.930410876235079787, 1508.551704408389924, 213.6518643025299866 ) ) ;
#110258 = CARTESIAN_POINT ( 'NONE',  ( -9.656246557070002012, 1389.622605478320111, 203.2012388434289960 ) ) ;
#110259 = CARTESIAN_POINT ( 'NONE',  ( 7.447014729250000187, 1422.296623052599898, 195.6434364388990161 ) ) ;
#110260 = CARTESIAN_POINT ( 'NONE',  ( -1.315863322207099895, 1432.366940000970089, 218.5411383834640162 ) ) ;
#110261 = CARTESIAN_POINT ( 'NONE',  ( -4.858768762960000487, 1495.519531265289970, 198.6104072793989985 ) ) ;
#110262 = CARTESIAN_POINT ( 'NONE',  ( 6.718545715849139732, 1409.147677173569946, 188.6149336500920128 ) ) ;
#110264 = CARTESIAN_POINT ( 'NONE',  ( 3.945738874322921141, 1515.565581977719148, 210.3719421152130167 ) ) ;
#110263 = CARTESIAN_POINT ( 'NONE',  ( 30.24979188206187786, 1524.075000532257036, 195.7694503965884394 ) ) ;
#110265 = CARTESIAN_POINT ( 'NONE',  ( 1.131675640069840005, 1451.349608238679821, 182.9318126509270144 ) ) ;
#110266 = B_SPLINE_CURVE_WITH_KNOTS ( 'NONE', 3,
 ( #10777, #85813, #105387, #51676, #44949, #69604, #2405, #36522, #71267, #103722 ),
 .UNSPECIFIED., .F., .F.,
 ( 4, 2, 2, 2, 4 ),
 ( 0.000000000000000000, 0.2500000000000000000, 0.5000000000000000000, 0.7500000000000000000, 1.000000000000000000 ),
 .UNSPECIFIED. ) ;
#110267 = CARTESIAN_POINT ( 'NONE',  ( -13.01267508979999832, 1379.476792316909950, 212.2796297140689887 ) ) ;
#110268 = CARTESIAN_POINT ( 'NONE',  ( 3.062921356683458551, 1525.320849883635901, 241.4068844367821782 ) ) ;
#110269 = ORIENTED_EDGE ( 'NONE', *, *, #35755, .T. ) ;
#110270 = CARTESIAN_POINT ( 'NONE',  ( -32.86802468363566732, 1523.481610118013805, 201.0396662541351418 ) ) ;
#110271 = DIRECTION ( 'NONE',  ( -0.9122148146285387060, -0.3835045346744238581, 0.1441818430190649758 ) ) ;
#110272 = CARTESIAN_POINT ( 'NONE',  ( -12.00997496865170788, 1508.551704408370824, 210.3182342545297843 ) ) ;
#110273 = EDGE_CURVE ( 'NONE', #102658, #19773, #109398, .T. ) ;
#110274 = CARTESIAN_POINT ( 'NONE',  ( -12.85016526419999927, 1389.184315283510159, 203.6059765727289914 ) ) ;
#110275 = EDGE_CURVE ( 'NONE', #59045, #101455, #56081, .T. ) ;
#110276 = CARTESIAN_POINT ( 'NONE',  ( 8.933680575207208818, 1427.300831583419949, 211.2763433717070143 ) ) ;
#110277 = B_SPLINE_CURVE_WITH_KNOTS ( 'NONE', 3,
 ( #90890, #14731, #14175, #4153, #48360, #74665, #6339, #46719, #82501, #80851, #65709, #5802, #29879, #108244, #108799, #5236, #64620, #90330, #72463, #39943, #4688, #21458, #74113, #99831, #23122, #48919, #83046, #63533, #20919, #38827, #89791, #55121, #89244, #98740, #12540, #38280, #106593, #22001, #13063, #47247, #56196, #91992, #42150 ),
 .UNSPECIFIED., .F., .F.,
 ( 4, 3, 3, 3, 3, 3, 3, 3, 3, 3, 3, 3, 3, 3, 4 ),
 ( 0.7655572723410000169, 0.9910019213816629868, 1.224379696548280050, 1.462078613726470078, 1.704827352691050013, 1.793853281190000093, 2.038466588041509819, 2.281256468864029330, 2.316155491860000026, 2.583989317140000352, 2.855920917859990027, 3.139267311770200131, 3.387490792979999554, 3.680707213613719553, 3.835724788389999418 ),
 .UNSPECIFIED. ) ;
#110278 = CARTESIAN_POINT ( 'NONE',  ( 11.59968585941729913, 1421.929632843320178, 203.4071348278239952 ) ) ;
#110279 = EDGE_CURVE ( 'NONE', #28182, #105296, #10666, .T. ) ;
#110280 = PLANE ( 'NONE',  #106750 ) ;
#110281 = CARTESIAN_POINT ( 'NONE',  ( 3.108624468949999707E-15, 1472.413060387330006, 271.1218459616979999 ) ) ;
#110282 = CARTESIAN_POINT ( 'NONE',  ( -8.868004540950760628, 1384.633249023989947, 218.6740787338979999 ) ) ;
#110283 = ADVANCED_FACE ( 'NONE', ( #102606 ), #47351, .F. ) ;
#110284 = CARTESIAN_POINT ( 'NONE',  ( 11.11059101190000042, 1433.900907478189765, 151.6798154798979965 ) ) ;
#110285 = CARTESIAN_POINT ( 'NONE',  ( 17.83186622649999720, 1447.284048007059937, 214.3676144203579952 ) ) ;
#110287 = EDGE_CURVE ( 'NONE', #105125, #37624, #77507, .T. ) ;
#110286 = CARTESIAN_POINT ( 'NONE',  ( 12.56955872636179983, 1415.089118586289942, 197.3775234796719928 ) ) ;
#110288 = CARTESIAN_POINT ( 'NONE',  ( -29.33952678943997228, 1526.382868172864164, 201.1028049641089694 ) ) ;
#110289 = CARTESIAN_POINT ( 'NONE',  ( 10.61677160567779943, 1423.423170255460036, 201.7579950878699719 ) ) ;
#110290 = CARTESIAN_POINT ( 'NONE',  ( 9.472111571387470619, 1463.349806330050114, 213.0242536977909822 ) ) ;
#110291 = EDGE_CURVE ( 'NONE', #39608, #106390, #64237, .T. ) ;
#110292 = DIRECTION ( 'NONE',  ( -1.603425251594204954E-18, 0.000000000000000000, 1.000000000000000000 ) ) ;
#110293 = CARTESIAN_POINT ( 'NONE',  ( -13.86092847646930082, 1410.765486861110048, 227.1170286572800023 ) ) ;
#110294 = FACE_OUTER_BOUND ( 'NONE', #94839, .T. ) ;
#110295 = CARTESIAN_POINT ( 'NONE',  ( 24.05801048009999832, 1430.354717876130053, 212.9167368799780036 ) ) ;
#110296 = VECTOR ( 'NONE', #43952, 1000.000000000000114 ) ;
#110297 = CARTESIAN_POINT ( 'NONE',  ( -1.682334239950061150, 1477.245458038868037, 198.8259265945336267 ) ) ;
#110298 = CARTESIAN_POINT ( 'NONE',  ( 3.530785927030000097E-16, 1427.166763959530044, 147.9649995502979891 ) ) ;
#110299 = CARTESIAN_POINT ( 'NONE',  ( 3.194122154841241290, 1508.524191963859948, 219.6292475936541564 ) ) ;
#110300 = CARTESIAN_POINT ( 'NONE',  ( -5.138230509358902687, 1391.881841899301889, 203.8075142969990168 ) ) ;
#110301 = CARTESIAN_POINT ( 'NONE',  ( -20.36853079741129946, 1464.956632542119905, 210.9458194320050097 ) ) ;
#110302 = CARTESIAN_POINT ( 'NONE',  ( 0.01327404799950150129, 1516.939877939420057, 212.5773418040870126 ) ) ;
#110303 = EDGE_CURVE ( 'NONE', #74686, #88920, #79476, .T. ) ;
#110304 = CARTESIAN_POINT ( 'NONE',  ( -16.74123569586150140, 1419.926558681200049, 209.1244132309280133 ) ) ;
#110305 = CARTESIAN_POINT ( 'NONE',  ( 0.2037710401876630106, 1460.860033808869957, 182.9161712545850094 ) ) ;
#110307 = VERTEX_POINT ( 'NONE', #73464 ) ;
#110306 = CARTESIAN_POINT ( 'NONE',  ( 1.393816646507355150, 1511.187213306747708, 243.1385343369520342 ) ) ;
#110308 = DIRECTION ( 'NONE',  ( -0.1070030146457317810, 0.000000000000000000, 0.9942586961433755866 ) ) ;
#110309 = LINE ( 'NONE', #59385, #72996 ) ;
#110310 = FACE_OUTER_BOUND ( 'NONE', #88264, .T. ) ;
#110311 = CARTESIAN_POINT ( 'NONE',  ( -39.75236484342700294, 1448.901857781610261, 134.0999999981239910 ) ) ;
#110312 = CARTESIAN_POINT ( 'NONE',  ( -31.06561261703210164, 1445.948172401960164, 137.1228040888619830 ) ) ;
#110313 = EDGE_LOOP ( 'NONE', ( #47835, #93799, #89739, #33906 ) ) ;
#110315 = EDGE_CURVE ( 'NONE', #34413, #55324, #52123, .T. ) ;
#110314 = CARTESIAN_POINT ( 'NONE',  ( 10.10004869885203682, 1422.222932908421853, 135.5999999980978430 ) ) ;
#110316 = CARTESIAN_POINT ( 'NONE',  ( 9.158757463789999775, 1480.005755715189935, 203.7772472770490140 ) ) ;
#110317 = CARTESIAN_POINT ( 'NONE',  ( -14.45747005360000159, 1416.828040559430065, 221.3917074983979774 ) ) ;
#110318 = CARTESIAN_POINT ( 'NONE',  ( 2.038847259689231084, 1501.977400791986611, 244.9330574173806951 ) ) ;
#110319 = EDGE_CURVE ( 'NONE', #74404, #64216, #44490, .T. ) ;
#110320 = CARTESIAN_POINT ( 'NONE',  ( -4.973371544095850361, 1432.678537253299965, 216.0289570334049927 ) ) ;
#110321 = CARTESIAN_POINT ( 'NONE',  ( -108.4550367074038633, 1381.313848681411628, 310.3901933583101140 ) ) ;
#110322 = CARTESIAN_POINT ( 'NONE',  ( -16.86653121810000044, 1418.408574706249965, 208.1493301914530036 ) ) ;
#110323 = AXIS2_PLACEMENT_3D ( 'NONE', #6971, #41125, #75305 ) ;
#110324 = DIRECTION ( 'NONE',  ( -0.000000000000000000, -1.000000000000000000, -0.000000000000000000 ) ) ;
#110325 = CARTESIAN_POINT ( 'NONE',  ( -11.06863488910000015, 1391.913060387289988, 206.1140686093889940 ) ) ;
#110326 = CARTESIAN_POINT ( 'NONE',  ( -83.57052189370659789, 1385.171097491720047, 287.3315033242400318 ) ) ;
#110327 = CARTESIAN_POINT ( 'NONE',  ( -10.95274535029249918, 1391.913060387289988, 212.6322721876839807 ) ) ;
#110328 = CARTESIAN_POINT ( 'NONE',  ( 10.86989896834730018, 1426.593996385999844, 207.8838144468849976 ) ) ;
#110329 = ORIENTED_EDGE ( 'NONE', *, *, #28861, .T. ) ;
#110330 = ADVANCED_FACE ( 'NONE', ( #32547 ), #37951, .F. ) ;
#110331 = CARTESIAN_POINT ( 'NONE',  ( -32.67729582440000513, 1451.771913520829912, 134.7516611205979871 ) ) ;
#110332 = CARTESIAN_POINT ( 'NONE',  ( 17.11778670694504711, 1443.086052842848176, 162.7557629363845990 ) ) ;
#110334 = VERTEX_POINT ( 'NONE', #57771 ) ;
#110333 = DIRECTION ( 'NONE',  ( -1.000000000000000000, 0.000000000000000000, 0.000000000000000000 ) ) ;
#110335 = CARTESIAN_POINT ( 'NONE',  ( 1.988015751190000069, 1473.864677161789814, 219.3075819037990186 ) ) ;
#110336 = CARTESIAN_POINT ( 'NONE',  ( 18.20258715539999983, 1429.723789929190161, 209.1218459616989946 ) ) ;
#110337 = CARTESIAN_POINT ( 'NONE',  ( -7.351830250119061105, 1364.179456836979853, 209.6218459617148824 ) ) ;
#110338 = CARTESIAN_POINT ( 'NONE',  ( -8.944365594689999810, 1494.493485459390058, 202.2793638724489824 ) ) ;
#110339 = CARTESIAN_POINT ( 'NONE',  ( 41.37929573993505983, 1446.359370807621190, 269.6357249233665812 ) ) ;
#110340 = CARTESIAN_POINT ( 'NONE',  ( 2.714430905872757815, 1517.051704408389924, 201.2325484332300221 ) ) ;
#110341 = CARTESIAN_POINT ( 'NONE',  ( 18.04593430210184835, 1435.112856754830091, 215.2521370104431355 ) ) ;
#110342 = FACE_OUTER_BOUND ( 'NONE', #17017, .T. ) ;
#110343 = DIRECTION ( 'NONE',  ( -0.000000000000000000, -1.000000000000000000, -0.000000000000000000 ) ) ;
#110344 = CARTESIAN_POINT ( 'NONE',  ( 11.34090880850000005, 1475.513060387329915, 227.1982711657979905 ) ) ;
#110345 = CARTESIAN_POINT ( 'NONE',  ( -30.90487439922528168, 1525.907212628473644, 216.4335774778784582 ) ) ;
#110346 = CARTESIAN_POINT ( 'NONE',  ( 6.934528529765000116, 1516.588006113850042, 206.2478870805069846 ) ) ;
#110347 = VECTOR ( 'NONE', #35352, 1000.000000000000114 ) ;
#110348 = CARTESIAN_POINT ( 'NONE',  ( 17.60627563539999940, 1410.895669412530196, 224.1775087544979783 ) ) ;
#110349 = CARTESIAN_POINT ( 'NONE',  ( 1.341950105200000021, 1416.837177087930058, 190.1629993749980088 ) ) ;
#110350 = FACE_OUTER_BOUND ( 'NONE', #19635, .T. ) ;
#110352 = ORIENTED_EDGE ( 'NONE', *, *, #76182, .F. ) ;
#110351 = CARTESIAN_POINT ( 'NONE',  ( -68.62231159920000323, 1379.747791814530046, 280.2140134006589847 ) ) ;
#110353 = ADVANCED_FACE ( 'NONE', ( #100826 ), #70559, .T. ) ;
#110354 = CARTESIAN_POINT ( 'NONE',  ( -10.78658054680221134, 1378.764302627705092, 215.1167326068625414 ) ) ;
#110355 = EDGE_LOOP ( 'NONE', ( #72841, #83119, #97455, #7155 ) ) ;
#110356 = CARTESIAN_POINT ( 'NONE',  ( -16.77006247923849358, 1513.317537406934207, 221.8555522796357877 ) ) ;
#110357 = CARTESIAN_POINT ( 'NONE',  ( -25.44333967360000059, 1449.802117277580010, 207.3037693659879892 ) ) ;
#110359 = CARTESIAN_POINT ( 'NONE',  ( 16.34779635269999787, 1409.733112109830017, 192.2574716150980123 ) ) ;
#110358 = CARTESIAN_POINT ( 'NONE',  ( -11.10862876709039959, 1425.650570261519761, 121.9042659590140119 ) ) ;
#110360 = CARTESIAN_POINT ( 'NONE',  ( -4.995726007844999650, 1516.651306816259876, 211.4173314712770093 ) ) ;
#110361 = EDGE_CURVE ( 'NONE', #79447, #6969, #6683, .T. ) ;
#110362 = CARTESIAN_POINT ( 'NONE',  ( 29.05308715847724699, 1510.038487003683258, 201.6439600875852420 ) ) ;
#110363 = CARTESIAN_POINT ( 'NONE',  ( -18.89959452430000297, 1416.839692140830039, 207.5749784653779955 ) ) ;
#110364 = CARTESIAN_POINT ( 'NONE',  ( 18.19796256645700083, 1509.563185887230020, 232.4213084367889905 ) ) ;
#110365 = CARTESIAN_POINT ( 'NONE',  ( 12.69817581368640091, 1500.644936277410125, 209.5553692708770086 ) ) ;
#110366 = APPLICATION_PROTOCOL_DEFINITION ( 'draft international standard', 'automotive_design', 1998, #108540 ) ;
#110367 = CARTESIAN_POINT ( 'NONE',  ( 3.345283522277380239, 1508.551704408389924, 213.9586846534960216 ) ) ;
#110368 = CARTESIAN_POINT ( 'NONE',  ( -37.75814923816869850, 1438.428394211809973, 136.5932668144599802 ) ) ;
#110369 = ORIENTED_EDGE ( 'NONE', *, *, #93993, .T. ) ;
#110370 = CARTESIAN_POINT ( 'NONE',  ( 8.904014029423381160, 1397.867934375250115, 219.0684523409199755 ) ) ;
#110371 = CARTESIAN_POINT ( 'NONE',  ( -18.87100397050000211, 1456.815141881530053, 228.5333397625980183 ) ) ;
#110372 = ORIENTED_EDGE ( 'NONE', *, *, #31065, .T. ) ;
#110373 = VERTEX_POINT ( 'NONE', #68931 ) ;
#110374 = VECTOR ( 'NONE', #94300, 1000.000000000000000 ) ;
#110375 = CARTESIAN_POINT ( 'NONE',  ( 2.122041310277463566, 1370.144953969707558, 211.3659795828131109 ) ) ;
#110376 = CARTESIAN_POINT ( 'NONE',  ( -11.86590160489819823, 1432.348284114390026, 151.0567667500760081 ) ) ;
#110377 = ADVANCED_FACE ( 'NONE', ( #10092 ), #78408, .F. ) ;
#110378 = B_SPLINE_CURVE_WITH_KNOTS ( 'NONE', 3,
 ( #97505, #73964, #4017, #46573, #54975, #39804, #12931, #21314, #81238, #48217, #63925, #82356, #90184, #99681, #106997, #30838, #89645, #65014, #80708, #20774, #4554, #98594, #30286, #108095, #22973, #89100, #38687, #56611, #98040, #55517, #12388, #72862, #5087, #6190, #39240, #64478, #57179, #73415, #99131, #21858, #65570, #106455, #38143, #72325, #29738, #22409, #91301, #14584, #48773, #71802, #92388, #67772, #100783, #109759, #23537, #83440, #57729, #7299, #40893, #94049, #85094, #15661, #25730, #76157, #49314, #6735, #32508, #110305, #66678, #75074, #67228, #101885, #68338, #74523, #33580, #109223, #59932, #31941, #16221, #66136, #42554, #58809, #8385, #50966, #18, #34152, #100257, #33040, #50426, #49865, #85643, #25177, #51510, #41464, #91848, #92949, #108654, #16763, #76705, #84551, #83999, #102444, #75625, #24076, #42008, #40342, #15125, #59381, #101324, #58266, #24614, #7840, #93492, #17316, #102993, #27962, #104114, #2244, #27401, #44785, #105227, #44224, #60479, #573, #61584, #104667, #87889, #36357, #8943, #69440, #78935, #87322, #11180, #18425, #26290, #1676, #68891, #35256, #28514, #10617, #20103, #103555, #70548, #77816, #43116, #95717, #78368, #62145, #26858, #96271, #94597, #17876, #61046, #35816, #95169, #53755, #52625 ),
 .UNSPECIFIED., .F., .F.,
 ( 4, 3, 3, 3, 3, 3, 3, 3, 3, 3, 3, 3, 3, 3, 3, 3, 3, 3, 3, 3, 3, 3, 3, 3, 3, 3, 3, 3, 3, 3, 3, 3, 3, 3, 3, 3, 3, 3, 3, 3, 3, 3, 3, 3, 3, 3, 3, 3, 3, 3, 3, 3, 4 ),
 ( 24.28183316541300130, 24.71881649057640118, 25.16768965757360021, 25.63067172750350053, 26.11087491490579993, 26.61294145909250020, 27.16470443015920111, 27.77145901019460084, 28.47376813613320223, 29.29751198064149875, 29.94171883040609927, 30.50707339981829946, 31.03088294720540219, 31.53498744032980028, 32.00161556922130046, 32.45443727351199925, 32.89561208257300251, 33.32674843685160226, 33.76099105068869477, 34.17209352077410500, 34.57743404036049384, 34.97544006220940105, 35.06371889219999360, 39.13045466909090209, 43.63534274978590588, 49.28827455502730004, 54.45493433082799584, 58.82551417691030338, 62.91385627785520285, 66.62310817775708927, 67.00219837880000284, 67.58345923580628778, 68.17364255231809977, 68.77363305402450067, 69.38449005478119602, 70.00750236436559248, 70.64426827910560291, 71.29681654595110274, 71.96779783973650524, 72.67405307691460337, 73.40992868474920385, 74.18468017158738803, 75.01465558537010736, 75.96352105172489644, 77.28110059534179754, 78.31061113875900048, 79.18396656175289650, 79.98558190753520591, 80.73137701487929974, 81.44186439771650043, 82.13175408128769561, 82.79775432491919673, 82.96876233691149594 ),
 .UNSPECIFIED. ) ;
#110379 = CARTESIAN_POINT ( 'NONE',  ( 2.986193535308999891, 1369.126893976419979, 209.1220808601199792 ) ) ;
#110380 = CARTESIAN_POINT ( 'NONE',  ( -11.47747972145789142, 1417.728687405828850, 198.8488469395149991 ) ) ;
#110381 = CARTESIAN_POINT ( 'NONE',  ( 4.138543391159999807, 1515.492058413689847, 210.9648081929590262 ) ) ;
#110382 = CIRCLE ( 'NONE', #74677, 39.61497827612718936 ) ;
#110383 = CARTESIAN_POINT ( 'NONE',  ( -6.466661620000779820, 1454.065070619989910, 202.3287932644439877 ) ) ;
#110384 = CARTESIAN_POINT ( 'NONE',  ( 33.91369107978050579, 1451.728768198530133, 135.3769930381369875 ) ) ;
#110385 = CARTESIAN_POINT ( 'NONE',  ( 0.4435022289555869968, 1418.672171135500093, 184.7048927309859891 ) ) ;
#110386 = DIRECTION ( 'NONE',  ( -1.000000000000000000, 0.000000000000000000, 0.000000000000000000 ) ) ;
#110387 = CARTESIAN_POINT ( 'NONE',  ( -9.809994181400000457, 1391.913060387289988, 214.8154632703889888 ) ) ;
#110388 = CARTESIAN_POINT ( 'NONE',  ( -93.79108000015780533, 1384.853053930580018, 294.4783922775349652 ) ) ;
#110389 = ORIENTED_EDGE ( 'NONE', *, *, #37244, .F. ) ;
#110390 = CARTESIAN_POINT ( 'NONE',  ( 5.003220727074999985, 1516.983995446890049, 202.1750974131470286 ) ) ;
#110391 = CARTESIAN_POINT ( 'NONE',  ( -4.037051035714999792, 1516.939819969850078, 209.1350663277499962 ) ) ;
#110392 = ORIENTED_EDGE ( 'NONE', *, *, #82360, .T. ) ;
#110393 = CARTESIAN_POINT ( 'NONE',  ( 11.79159303035750028, 1427.856769254729898, 147.7337906482489984 ) ) ;
#110394 = EDGE_CURVE ( 'NONE', #64966, #75650, #81437, .T. ) ;
#110395 = CARTESIAN_POINT ( 'NONE',  ( 4.551262986272157640, 1511.401878033069579, 217.4960750013443374 ) ) ;
#110396 = ORIENTED_EDGE ( 'NONE', *, *, #16591, .T. ) ;
#110397 = CARTESIAN_POINT ( 'NONE',  ( -14.00211218169999938, 1416.535385209229844, 221.8386906309980020 ) ) ;
#110398 = CARTESIAN_POINT ( 'NONE',  ( -16.90742463042001376, 1442.831169986190844, 162.4348201727408991 ) ) ;
#110399 = CARTESIAN_POINT ( 'NONE',  ( -6.065469208827907188, 1433.485399230374014, 215.0992432421768683 ) ) ;
#110400 = CARTESIAN_POINT ( 'NONE',  ( -10.55208896769630122, 1462.421637114440045, 208.2011304212279867 ) ) ;
#110401 = CARTESIAN_POINT ( 'NONE',  ( 21.90143050737389885, 1409.902695463000100, 206.2994855651969885 ) ) ;
#110402 = EDGE_CURVE ( 'NONE', #59275, #101819, #13407, .T. ) ;
#110403 = CARTESIAN_POINT ( 'NONE',  ( 14.36661330029840045, 1436.257348211630188, 150.0159985837800036 ) ) ;
#110404 = CARTESIAN_POINT ( 'NONE',  ( -8.603211701180001114, 1469.317673379189955, 216.5015782100589945 ) ) ;
#110405 = CARTESIAN_POINT ( 'NONE',  ( -10.47439550540000042, 1490.889281562089991, 212.4388770995890070 ) ) ;
#110406 = CARTESIAN_POINT ( 'NONE',  ( -54.48829305249999777, 1379.705335535419863, 248.9076988030590201 ) ) ;
#110407 = CARTESIAN_POINT ( 'NONE',  ( -15.02388101939999920, 1462.596411967030008, 223.3218936951980140 ) ) ;
#110409 = CARTESIAN_POINT ( 'NONE',  ( -5.371346839171279974, 1516.551188146539971, 218.7599618298110045 ) ) ;
#110408 = CARTESIAN_POINT ( 'NONE',  ( 17.24203588439999990, 1458.670886926930052, 229.0945275712979878 ) ) ;
#110410 = CARTESIAN_POINT ( 'NONE',  ( -4.969838499002304566, 1423.248872364527642, 184.7412924219641184 ) ) ;
#110411 = AXIS2_PLACEMENT_3D ( 'NONE', #87734, #96676, #19949 ) ;
#110412 = CARTESIAN_POINT ( 'NONE',  ( -5.468855732409769743, 1422.747406303380103, 121.8314839712469961 ) ) ;
#110413 = ORIENTED_EDGE ( 'NONE', *, *, #1488, .F. ) ;
#110414 = CARTESIAN_POINT ( 'NONE',  ( -4.115863335914074383, 1509.032014613820593, 204.7576463065119299 ) ) ;
#110415 = CARTESIAN_POINT ( 'NONE',  ( 0.4918342890736275841, 1516.791933468850175, 216.8376239430565136 ) ) ;
#110416 = CARTESIAN_POINT ( 'NONE',  ( -6.937338783705000012, 1516.706638732659940, 213.7399656364970042 ) ) ;
#110417 = EDGE_CURVE ( 'NONE', #91877, #31461, #92166, .T. ) ;
#110418 = CARTESIAN_POINT ( 'NONE',  ( -2.901755129351373252, 1484.493861582726140, 183.2929701160953471 ) ) ;
#110419 = CARTESIAN_POINT ( 'NONE',  ( -16.66101146819999812, 1410.867390116229899, 191.7375337716979971 ) ) ;
#110421 = EDGE_LOOP ( 'NONE', ( #32052, #107759, #57399, #25812, #932 ) ) ;
#110420 = CARTESIAN_POINT ( 'NONE',  ( -11.33943867567700003, 1500.720461424150017, 211.0488575539550027 ) ) ;
#110422 = CARTESIAN_POINT ( 'NONE',  ( -7.966081158779999782, 1384.918389535180040, 199.4892681704289998 ) ) ;
#110423 = CARTESIAN_POINT ( 'NONE',  ( -2.188073835520000010, 1508.020975839189987, 220.9453034226989985 ) ) ;
#110424 = EDGE_CURVE ( 'NONE', #7555, #21042, #64450, .T. ) ;
#110425 = CARTESIAN_POINT ( 'NONE',  ( -11.72873588490000074, 1429.311224835630128, 150.0544550291980102 ) ) ;
#110426 = CARTESIAN_POINT ( 'NONE',  ( 19.27780332526499762, 1456.939258528880146, 224.7012343488810018 ) ) ;
#110427 = CARTESIAN_POINT ( 'NONE',  ( -10.98402802510699949, 1462.124134087619950, 210.0291763056419825 ) ) ;
#110428 = DIRECTION ( 'NONE',  ( -0.7384854939282339270, 4.128709092058508552E-17, 0.6742693640212139572 ) ) ;
#110429 = CARTESIAN_POINT ( 'NONE',  ( 3.750000000000000000, 1512.051704408390151, 209.1218459616989946 ) ) ;
#110430 = CARTESIAN_POINT ( 'NONE',  ( 0.2681867035651760434, 1457.296285398379950, 189.0031676906399980 ) ) ;
#110431 = EDGE_CURVE ( 'NONE', #42994, #41235, #33442, .T. ) ;
#110433 = CARTESIAN_POINT ( 'NONE',  ( -10.51083735039999922, 1480.296936571690139, 210.9545376977389992 ) ) ;
#110432 = CARTESIAN_POINT ( 'NONE',  ( -19.66165407200000104, 1482.732718108530207, 227.7681860883980107 ) ) ;
#110435 = CARTESIAN_POINT ( 'NONE',  ( -16.78634058370699833, 1460.263302320530101, 228.3352825267500066 ) ) ;
#110434 = CIRCLE ( 'NONE', #10286, 7.868384924639995504 ) ;
#110436 = VERTEX_POINT ( 'NONE', #12722 ) ;
#110437 = CARTESIAN_POINT ( 'NONE',  ( -1.715704529104999931, 1516.757508073510053, 205.8704515699670026 ) ) ;
#110438 = CARTESIAN_POINT ( 'NONE',  ( 29.78004744509999924, 1414.955384726930106, 269.3615102554980467 ) ) ;
#110439 = CARTESIAN_POINT ( 'NONE',  ( 1.701332460469982433, 1456.209741179828598, 218.8708370859535819 ) ) ;
#110440 = CARTESIAN_POINT ( 'NONE',  ( 18.44722761019999879, 1449.736698785399994, 191.1486972741980139 ) ) ;
#110441 = EDGE_CURVE ( 'NONE', #40151, #47989, #91356, .T. ) ;
#110442 = EDGE_CURVE ( 'NONE', #68144, #7608, #94957, .T. ) ;
#110443 = CARTESIAN_POINT ( 'NONE',  ( -0.01845360631625059950, 1508.137092213139795, 237.5627139155050145 ) ) ;
#110444 = CARTESIAN_POINT ( 'NONE',  ( 15.95383384960000228, 1506.798305107329952, 193.5571554442980187 ) ) ;
#110445 = CARTESIAN_POINT ( 'NONE',  ( -1.387227658650000084, 1451.254490850629963, 183.6670524069980104 ) ) ;
#110446 = CARTESIAN_POINT ( 'NONE',  ( 17.69066643606209155, 1458.123854326780929, 230.3917304478115682 ) ) ;
#110447 = CARTESIAN_POINT ( 'NONE',  ( -15.39508542709999794, 1416.424718227980065, 206.7259350337689909 ) ) ;
#110448 = CARTESIAN_POINT ( 'NONE',  ( -13.58279026639999998, 1443.465488095079991, 187.7936867102980045 ) ) ;
#110449 = CARTESIAN_POINT ( 'NONE',  ( -5.418330280727370329, 1484.891209372279945, 198.5201634387589991 ) ) ;
#110450 = CARTESIAN_POINT ( 'NONE',  ( -5.264763130462112528, 1496.215617598504195, 199.2138358744504103 ) ) ;
#110451 = CARTESIAN_POINT ( 'NONE',  ( 5.035691840050000145, 1407.858053359329915, 270.1320510971980298 ) ) ;
#110452 = CARTESIAN_POINT ( 'NONE',  ( 1.452806739154890003, 1502.997517574160156, 181.2928522130929991 ) ) ;
#110453 = CARTESIAN_POINT ( 'NONE',  ( -5.502752162680000225, 1437.219209177789935, 209.1105472058980013 ) ) ;
#110454 = EDGE_CURVE ( 'NONE', #52345, #81409, #101676, .T. ) ;
#110455 = AXIS2_PLACEMENT_3D ( 'NONE', #56197, #57865, #14732 ) ;
#110456 = CARTESIAN_POINT ( 'NONE',  ( 11.45115712805808172, 1425.807404925399624, 139.1344848049184293 ) ) ;
#110457 = CARTESIAN_POINT ( 'NONE',  ( -12.17955882736053930, 1377.723645317214277, 210.9225509704534716 ) ) ;
#110458 = CARTESIAN_POINT ( 'NONE',  ( -12.73803555039999935, 1474.798601776230043, 267.7854995676979684 ) ) ;
#110459 = CARTESIAN_POINT ( 'NONE',  ( 29.30029655192942073, 1525.907212628473644, 196.8717316207784620 ) ) ;
#110460 = CARTESIAN_POINT ( 'NONE',  ( -14.86632106490745109, 1514.624316683434927, 192.9203402940289038 ) ) ;
#110461 = EDGE_CURVE ( 'NONE', #43348, #93138, #75309, .T. ) ;
#110462 = CARTESIAN_POINT ( 'NONE',  ( 18.42623971653249981, 1424.510075577899897, 223.4209876132420050 ) ) ;
#110463 = CARTESIAN_POINT ( 'NONE',  ( -49.22008464409690021, 1384.743802012480046, 260.1336803388579710 ) ) ;
#110464 = CARTESIAN_POINT ( 'NONE',  ( -4.329448781177520189, 1515.064792686469900, 210.9648092169189795 ) ) ;
#110465 = CARTESIAN_POINT ( 'NONE',  ( -11.96661585360000046, 1440.449248668989867, 150.8629738177980073 ) ) ;
#110466 = CARTESIAN_POINT ( 'NONE',  ( -24.64468664290339817, 1457.436562328650098, 211.7678147391609969 ) ) ;
#110467 = CARTESIAN_POINT ( 'NONE',  ( -2.127049456059860066, 1416.948096802419968, 197.4354557404840307 ) ) ;
#110468 = DIRECTION ( 'NONE',  ( 0.000000000000000000, 0.000000000000000000, 1.000000000000000000 ) ) ;
#110469 = AXIS2_PLACEMENT_3D ( 'NONE', #71985, #71443, #63577 ) ;
#110470 = CARTESIAN_POINT ( 'NONE',  ( -23.36711103019999669, 1410.650541193030222, 205.9586710055679930 ) ) ;
#110471 = CARTESIAN_POINT ( 'NONE',  ( -8.465783460212520595, 1382.621316526051260, 200.0067512675162504 ) ) ;
#110472 = CARTESIAN_POINT ( 'NONE',  ( 4.800520365470000606, 1485.026014063289949, 218.8652762536089824 ) ) ;
#110473 = CARTESIAN_POINT ( 'NONE',  ( 10.78014379640850073, 1479.477604915960001, 207.2887695641769881 ) ) ;
#110474 = FACE_OUTER_BOUND ( 'NONE', #108189, .T. ) ;
#110475 = CARTESIAN_POINT ( 'NONE',  ( -8.149274592039999376, 1439.839152417889864, 228.6706535942990115 ) ) ;
#110476 = CARTESIAN_POINT ( 'NONE',  ( 16.99777429700839093, 1524.964158026965379, 181.1932245048199377 ) ) ;
#110477 = CARTESIAN_POINT ( 'NONE',  ( 10.96015508933500016, 1512.830284628050094, 225.0317485278669949 ) ) ;
#110479 = CARTESIAN_POINT ( 'NONE',  ( 1.756561144747210293E-16, 1391.913060387289988, 209.1218459572589836 ) ) ;
#110478 = CARTESIAN_POINT ( 'NONE',  ( 14.44303130513500122, 1516.995662938509895, 192.4521789031669812 ) ) ;
#110480 = CARTESIAN_POINT ( 'NONE',  ( 11.69994194908459839, 1426.720164485290070, 141.5157594407809825 ) ) ;
#110481 = CARTESIAN_POINT ( 'NONE',  ( 3.552713678799999608E-15, 1413.913060387330006, 209.1218459616989946 ) ) ;
#110482 = DIRECTION ( 'NONE',  ( 0.000000000000000000, 0.000000000000000000, 1.000000000000000000 ) ) ;
#110483 = FACE_OUTER_BOUND ( 'NONE', #55464, .T. ) ;
#110484 = DIRECTION ( 'NONE',  ( -0.06728379684271972028, -0.9969860201949397593, 0.03862338952348403492 ) ) ;
#110485 = CARTESIAN_POINT ( 'NONE',  ( 4.613762356885000138, 1516.939574742129935, 203.3372076122869885 ) ) ;
#110486 = CARTESIAN_POINT ( 'NONE',  ( -9.373950541344154175, 1512.187213306747481, 228.8708405320809902 ) ) ;
#110488 = CARTESIAN_POINT ( 'NONE',  ( -4.225531567558850732, 1398.039136736335195, 221.4159458655357753 ) ) ;
#110487 = AXIS2_PLACEMENT_3D ( 'NONE', #52234, #19708, #18585 ) ;
#110489 = CARTESIAN_POINT ( 'NONE',  ( 1.547463896846929865, 1414.913060387349788, 192.3096116128920130 ) ) ;
#110490 = CARTESIAN_POINT ( 'NONE',  ( 15.04135733889389925, 1432.105820058640120, 219.6911068266909979 ) ) ;
#110491 = CARTESIAN_POINT ( 'NONE',  ( -21.38516915558007625, 1512.187213306747481, 180.3939891059723664 ) ) ;
#110492 = CARTESIAN_POINT ( 'NONE',  ( 3.756023522790000069, 1369.098589419769951, 207.6218459616989946 ) ) ;
#110494 = ORIENTED_EDGE ( 'NONE', *, *, #31975, .F. ) ;
#110493 = CARTESIAN_POINT ( 'NONE',  ( -29.69371359589970183, 1379.627920369189951, 218.1711912100410018 ) ) ;
#110495 = ORIENTED_EDGE ( 'NONE', *, *, #31181, .F. ) ;
#110496 = CARTESIAN_POINT ( 'NONE',  ( 11.82498356950000051, 1433.974774860679872, 150.8894406338980048 ) ) ;
#110497 = CARTESIAN_POINT ( 'NONE',  ( -5.039302881340000262, 1396.270828050830005, 220.4040175563980313 ) ) ;
#110498 = VERTEX_POINT ( 'NONE', #65353 ) ;
#110499 = CARTESIAN_POINT ( 'NONE',  ( -106.2815828819999950, 1378.913060986889832, 306.5512043212590356 ) ) ;
#110500 = CARTESIAN_POINT ( 'NONE',  ( -23.45874307799999769, 1509.732257746930145, 193.0693562410979780 ) ) ;
#110501 = CARTESIAN_POINT ( 'NONE',  ( 4.020406191785269812, 1515.375307391110027, 205.5795572779110216 ) ) ;
#110503 = CARTESIAN_POINT ( 'NONE',  ( 17.83884855390000013, 1421.695374127529931, 225.9258521583979871 ) ) ;
#110502 = CARTESIAN_POINT ( 'NONE',  ( 16.03737488143600132, 1422.958007463530294, 191.1431703812559988 ) ) ;
#110504 = CARTESIAN_POINT ( 'NONE',  ( 17.00378010880389823, 1488.410040644369928, 230.1592669151310133 ) ) ;
#110505 = B_SPLINE_CURVE_WITH_KNOTS ( 'NONE', 5,
 ( #92013, #92549, #15817, #187, #42165, #84154 ),
 .UNSPECIFIED., .F., .F.,
 ( 6, 6 ),
 ( -95.99024502151270610, -20.17942402910439625 ),
 .UNSPECIFIED. ) ;
#110506 = CARTESIAN_POINT ( 'NONE',  ( 4.549407228569999795, 1449.234560512250027, 184.4437958230980144 ) ) ;
#110507 = CARTESIAN_POINT ( 'NONE',  ( -0.1955981715909999863, 1414.913060387329779, 193.0575580938979954 ) ) ;
#110508 = CYLINDRICAL_SURFACE ( 'NONE', #96546, 2.000000000000022204 ) ;
#110509 = CARTESIAN_POINT ( 'NONE',  ( 1.951953247971109917, 1395.981224096749884, 198.2838940656170053 ) ) ;
#110510 = CARTESIAN_POINT ( 'NONE',  ( 14.41907353320999974, 1416.449138231070037, 196.8916081074650037 ) ) ;
#110511 = CARTESIAN_POINT ( 'NONE',  ( 11.76661577670000014, 1432.114831257029891, 150.8088909320979951 ) ) ;
#110512 = CARTESIAN_POINT ( 'NONE',  ( 7.645353494405000561, 1513.311928781869938, 201.7433401170069942 ) ) ;
#110513 = EDGE_LOOP ( 'NONE', ( #70669, #2052, #65675, #68212 ) ) ;
#110514 = CARTESIAN_POINT ( 'NONE',  ( 13.52509826555950134, 1435.477190311279855, 150.1367605865879682 ) ) ;
#110515 = B_SPLINE_CURVE_WITH_KNOTS ( 'NONE', 3,
 ( #49863, #23536, #49313, #65013 ),
 .UNSPECIFIED., .F., .F.,
 ( 4, 4 ),
 ( 0.000000000000000000, 1.000000000000000000 ),
 .UNSPECIFIED. ) ;
#110516 = VERTEX_POINT ( 'NONE', #91072 ) ;
#110517 = ORIENTED_EDGE ( 'NONE', *, *, #1118, .T. ) ;
#110518 = CARTESIAN_POINT ( 'NONE',  ( 13.50811536235293353, 1444.049332424179056, 169.3527944688763114 ) ) ;
#110519 = CARTESIAN_POINT ( 'NONE',  ( -9.099053347499999944, 1464.323907318429974, 232.8359173459980127 ) ) ;
#110520 = CARTESIAN_POINT ( 'NONE',  ( -6.163969623551973420, 1475.687477306443270, 200.8053095011335927 ) ) ;
#110521 = CARTESIAN_POINT ( 'NONE',  ( -1.125509888415000104, 1517.203017563489766, 216.4609531728469847 ) ) ;
#110522 = CARTESIAN_POINT ( 'NONE',  ( -7.948115392449770944, 1511.813433987433200, 212.3186854298990340 ) ) ;
#110523 = CARTESIAN_POINT ( 'NONE',  ( 11.30087886326580104, 1422.109560457819953, 210.2596498238989966 ) ) ;
#110524 = CARTESIAN_POINT ( 'NONE',  ( 2.500000000000000000, 1448.204022878760043, 169.8583767613770021 ) ) ;
#110525 = CARTESIAN_POINT ( 'NONE',  ( -3.771520295670000245, 1377.889610323579973, 206.3143083597190071 ) ) ;
#110526 = ORIENTED_EDGE ( 'NONE', *, *, #72771, .F. ) ;
#110527 = CARTESIAN_POINT ( 'NONE',  ( -7.337793750624999944, 1517.145312756229941, 206.2496372219370073 ) ) ;
#110528 = ORIENTED_EDGE ( 'NONE', *, *, #54069, .F. ) ;
#110529 = CARTESIAN_POINT ( 'NONE',  ( 19.72684292035980036, 1440.913060387330006, 214.6106658576619850 ) ) ;
#110530 = CARTESIAN_POINT ( 'NONE',  ( -19.48412118799999959, 1509.357564148129995, 230.4874557228980052 ) ) ;
#110531 = CARTESIAN_POINT ( 'NONE',  ( -4.387270951399999674, 1410.444783042529934, 186.8284482498980026 ) ) ;
#110532 = CARTESIAN_POINT ( 'NONE',  ( 7.466890166705000276, 1513.600111798359876, 215.7706967346870215 ) ) ;
#110534 = ORIENTED_EDGE ( 'NONE', *, *, #43589, .F. ) ;
#110533 = CARTESIAN_POINT ( 'NONE',  ( -1.940673996872300133, 1422.484488249149990, 192.6009970386809869 ) ) ;
#110535 = CARTESIAN_POINT ( 'NONE',  ( 21.70470943100000127, 1430.163002639730166, 219.7457352202980019 ) ) ;
#110536 = DIRECTION ( 'NONE',  ( -0.7026931535931751904, 0.02432541744852609669, -0.7110770745560801576 ) ) ;
#110538 = DIRECTION ( 'NONE',  ( 0.9858563016761853204, 0.000000000000000000, 0.1675928174038331386 ) ) ;
#110537 = AXIS2_PLACEMENT_3D ( 'NONE', #76555, #93349, #67628 ) ;
#110539 = CARTESIAN_POINT ( 'NONE',  ( 0.003780032387689030195, 1466.769817337830091, 235.6257279122189914 ) ) ;
#110540 = CARTESIAN_POINT ( 'NONE',  ( 20.98221433429012350, 1524.841055067851130, 181.0917269138614358 ) ) ;
#110541 = AXIS2_PLACEMENT_3D ( 'NONE', #92977, #24643, #57761 ) ;
#110542 = CARTESIAN_POINT ( 'NONE',  ( -7.714371541114999786, 1516.738222552470233, 214.9014490703569891 ) ) ;
#110543 = AXIS2_PLACEMENT_3D ( 'NONE', #59643, #6603, #40753 ) ;
#110544 = CARTESIAN_POINT ( 'NONE',  ( -3.325048289822069680, 1428.738726997929916, 200.3675363921470307 ) ) ;
#110545 = CARTESIAN_POINT ( 'NONE',  ( -20.59469742430000139, 1507.767255104930200, 190.2244918928979871 ) ) ;
#110546 = AXIS2_PLACEMENT_3D ( 'NONE', #51459, #16175, #24020 ) ;
#110547 = CARTESIAN_POINT ( 'NONE',  ( 7.512750234783659664, 1509.038617475689989, 214.6350457605470012 ) ) ;
#110548 = CARTESIAN_POINT ( 'NONE',  ( 5.013274961385000061, 1517.068517094990057, 211.4089302402969963 ) ) ;
#110549 = CARTESIAN_POINT ( 'NONE',  ( 9.778038872353379318, 1435.196923564789813, 208.3424860689369780 ) ) ;
#110550 = CARTESIAN_POINT ( 'NONE',  ( 14.72054272970000000, 1409.427113070929863, 192.5180613899979960 ) ) ;
#110551 =( BOUNDED_CURVE ( )  B_SPLINE_CURVE ( 3, ( #61439, #44068, #63112, #53590 ),
 .UNSPECIFIED., .F., .T. ) 
 B_SPLINE_CURVE_WITH_KNOTS ( ( 4, 4 ),
 ( 4.243850967066803648, 4.610002426280772170 ),
 .UNSPECIFIED. ) 
 CURVE ( )  GEOMETRIC_REPRESENTATION_ITEM ( )  RATIONAL_B_SPLINE_CURVE ( ( 1.000000000000000000, 0.9888589289762730328, 0.9888589289762730328, 1.000000000000000000 ) ) 
 REPRESENTATION_ITEM ( '' )  );
#110552 = CARTESIAN_POINT ( 'NONE',  ( 10.97130333569999827, 1432.456475934739956, 151.7700838859979910 ) ) ;
#110554 = ORIENTED_EDGE ( 'NONE', *, *, #40661, .T. ) ;
#110553 = CARTESIAN_POINT ( 'NONE',  ( -49.59345295620000371, 1385.124330617979922, 260.9076469794590025 ) ) ;
#110555 = CARTESIAN_POINT ( 'NONE',  ( -74.11717081736961177, 1385.010645261289937, 299.2649584196010437 ) ) ;
#110556 = CARTESIAN_POINT ( 'NONE',  ( 20.04382680870000044, 1471.636491243529917, 264.7217811306979911 ) ) ;
#110557 = EDGE_CURVE ( 'NONE', #65578, #93757, #25303, .T. ) ;
#110558 = CARTESIAN_POINT ( 'NONE',  ( -7.588802720235000798, 1511.942942747529969, 211.3806715220270007 ) ) ;
#110559 = CARTESIAN_POINT ( 'NONE',  ( 1.702416261868870073, 1493.957958506549858, 220.1113518634800243 ) ) ;
#110560 = CARTESIAN_POINT ( 'NONE',  ( -23.89130367779999986, 1445.918201964170066, 214.2695373320979968 ) ) ;
#110561 = CARTESIAN_POINT ( 'NONE',  ( -0.1681681984989999989, 1405.973120458229914, 146.1721969590979882 ) ) ;
#110563 = CARTESIAN_POINT ( 'NONE',  ( 19.03110457509999875, 1457.047041243630019, 226.1578386332979846 ) ) ;
#110562 = CARTESIAN_POINT ( 'NONE',  ( 1.128757561074999805, 1516.608208975040043, 216.8328129478670121 ) ) ;
#110564 = CARTESIAN_POINT ( 'NONE',  ( -9.208813132158530479, 1450.227655483129865, 208.7826788825430242 ) ) ;
#110565 = CARTESIAN_POINT ( 'NONE',  ( -108.8094171845170024, 1382.492531679610011, 310.7655809651279810 ) ) ;
#110566 = VECTOR ( 'NONE', #78116, 1000.000000000000000 ) ;
#110567 = ORIENTED_EDGE ( 'NONE', *, *, #62887, .T. ) ;
#110568 = CARTESIAN_POINT ( 'NONE',  ( -3.262264688434999726, 1516.633288330999903, 202.5742890007669814 ) ) ;
#110569 = CARTESIAN_POINT ( 'NONE',  ( 8.217213021130000279E-10, 1406.066315318429815, 269.0456997843980389 ) ) ;
#110570 = CARTESIAN_POINT ( 'NONE',  ( -0.1675834497249999722, 1467.614897612030063, 229.5904413177980246 ) ) ;
#110571 = EDGE_CURVE ( 'NONE', #23046, #70982, #60060, .T. ) ;
#110572 = CARTESIAN_POINT ( 'NONE',  ( 12.87923822840000021, 1419.814314491729874, 222.7980798877980249 ) ) ;
#110573 = CARTESIAN_POINT ( 'NONE',  ( -34.09113935471027190, 1523.429859730330918, 219.7507174562243506 ) ) ;
#110574 = CARTESIAN_POINT ( 'NONE',  ( -13.50530508558610165, 1506.272574391458193, 209.1324396371510659 ) ) ;
#110575 = CARTESIAN_POINT ( 'NONE',  ( 3.887546720220000029, 1467.073181280790095, 218.4203203200989947 ) ) ;
#110576 = CARTESIAN_POINT ( 'NONE',  ( 15.06727053545517947, 1420.624436962964637, 227.9341869482010452 ) ) ;
#110577 = CARTESIAN_POINT ( 'NONE',  ( 32.66532558909530337, 1435.798634193749876, 135.9825271959909969 ) ) ;
#110578 = CARTESIAN_POINT ( 'NONE',  ( 40.04800941360640110, 1445.544085285030178, 136.8743094025140010 ) ) ;
#110579 = CARTESIAN_POINT ( 'NONE',  ( 2.601599038695280157E-15, 1470.145267143019964, 266.9202418870810334 ) ) ;
#110580 = CARTESIAN_POINT ( 'NONE',  ( -2.451814001629999851, 1429.700538548090208, 200.7967559036290197 ) ) ;
#110581 = DIRECTION ( 'NONE',  ( 1.755985294532464991E-16, -1.000000000000000000, 1.338183447452830017E-16 ) ) ;
#110582 = FACE_OUTER_BOUND ( 'NONE', #27096, .T. ) ;
#110583 = CARTESIAN_POINT ( 'NONE',  ( -38.89734685438744322, 1452.468859951071181, 269.5913801711774340 ) ) ;
#110584 = EDGE_LOOP ( 'NONE', ( #57508, #15730, #30251, #38624, #84751 ) ) ;
#110585 = CARTESIAN_POINT ( 'NONE',  ( -10.10023367162169983, 1517.051704408389924, 185.1638560673330005 ) ) ;
#110586 = DIRECTION ( 'NONE',  ( 1.836970198721029688E-16, 1.000000000000000000, 0.000000000000000000 ) ) ;
#110587 = CARTESIAN_POINT ( 'NONE',  ( -4.491288185863250071, 1508.884219112060009, 212.6094329811639909 ) ) ;
#110588 = CARTESIAN_POINT ( 'NONE',  ( 15.56176417158150116, 1464.171868028719928, 189.4544269278800073 ) ) ;
#110589 = CARTESIAN_POINT ( 'NONE',  ( -4.343257420380000298E-10, 1475.319450600630034, 269.4986873273979882 ) ) ;
#110591 = CARTESIAN_POINT ( 'NONE',  ( -10.99273638689999899, 1491.630725208689910, 209.8916735729859795 ) ) ;
#110590 = CARTESIAN_POINT ( 'NONE',  ( 11.47835457579999918, 1502.362092611190064, 208.5873688113690037 ) ) ;
#110592 = CARTESIAN_POINT ( 'NONE',  ( -28.83249086449999865, 1509.587594257930050, 209.3213971828919853 ) ) ;
#110594 = EDGE_CURVE ( 'NONE', #55445, #95431, #57504, .T. ) ;
#110593 = EDGE_CURVE ( 'NONE', #15508, #24424, #27905, .T. ) ;
#110595 = CARTESIAN_POINT ( 'NONE',  ( 9.190770083770001264, 1428.225163806190039, 212.7760827912590003 ) ) ;
#110596 = CARTESIAN_POINT ( 'NONE',  ( 1.702403487548299843, 1493.957943060129992, 220.1113531599900170 ) ) ;
#110597 = FACE_OUTER_BOUND ( 'NONE', #72915, .T. ) ;
#110598 = CARTESIAN_POINT ( 'NONE',  ( -7.331526522911103072, 1451.412073465244930, 153.1354536431154827 ) ) ;
#110599 = CARTESIAN_POINT ( 'NONE',  ( -17.97082642953529685, 1416.218047878440075, 209.4769703680670148 ) ) ;
#110600 = CARTESIAN_POINT ( 'NONE',  ( 24.58760858760000190, 1435.374942484849953, 136.3398539886979961 ) ) ;
#110602 = EDGE_CURVE ( 'NONE', #51820, #43618, #91629, .T. ) ;
#110601 = CARTESIAN_POINT ( 'NONE',  ( -10.76975510178520068, 1396.289148523040012, 206.5700517074710092 ) ) ;
#110603 = VERTEX_POINT ( 'NONE', #32278 ) ;
#110604 = CARTESIAN_POINT ( 'NONE',  ( -0.3443494227043759626, 1415.932840154009909, 191.2798020189869987 ) ) ;
#110605 = CARTESIAN_POINT ( 'NONE',  ( -9.486449711069932178, 1409.244334510940007, 228.2930016997800067 ) ) ;
#110606 = ORIENTED_EDGE ( 'NONE', *, *, #10300, .F. ) ;
#110607 = VERTEX_POINT ( 'NONE', #15999 ) ;
#110608 = DIRECTION ( 'NONE',  ( -0.7414773880254761362, 0.000000000000000000, -0.6709778558543624261 ) ) ;
#110609 = CARTESIAN_POINT ( 'NONE',  ( -15.30083054224856554, 1416.035659937719629, 206.6105554433750626 ) ) ;
#110611 = CARTESIAN_POINT ( 'NONE',  ( -23.73182569189999924, 1445.711889770029984, 212.0244532444880008 ) ) ;
#110610 = CARTESIAN_POINT ( 'NONE',  ( 11.00605459009999976, 1426.944683675330225, 91.15821214469779932 ) ) ;
#110612 = CARTESIAN_POINT ( 'NONE',  ( -9.318458176530000969, 1446.292171852890078, 213.7041144372790313 ) ) ;
#110613 = CARTESIAN_POINT ( 'NONE',  ( -11.71362335670000121, 1433.059942302950276, 150.8500997151980130 ) ) ;
#110614 = CARTESIAN_POINT ( 'NONE',  ( -12.29553027537570031, 1378.313034645889957, 210.0045240490580056 ) ) ;
#110615 = CARTESIAN_POINT ( 'NONE',  ( -2.617672629425792152, 1420.510773938307011, 185.8077901307954107 ) ) ;
#110616 = FACE_OUTER_BOUND ( 'NONE', #85421, .T. ) ;
#110617 = CARTESIAN_POINT ( 'NONE',  ( -24.32551817709999753, 1439.446294773350019, 211.3365414780779759 ) ) ;
#110618 = CARTESIAN_POINT ( 'NONE',  ( 8.878920243399999634, 1509.223121094930093, 181.5151187545980065 ) ) ;
#110619 = CARTESIAN_POINT ( 'NONE',  ( 2.157135272340000132, 1450.193356149409965, 182.5998694718979891 ) ) ;
#110620 = CIRCLE ( 'NONE', #81998, 0.9999999999999997780 ) ;
#110621 = CARTESIAN_POINT ( 'NONE',  ( 6.907476780246043724, 1362.740070248910570, 207.6218459616988241 ) ) ;
#110622 = CARTESIAN_POINT ( 'NONE',  ( -27.93181393147919067, 1510.000215323476596, 198.1739204093250635 ) ) ;
#110624 = ORIENTED_EDGE ( 'NONE', *, *, #26171, .T. ) ;
#110623 = LINE ( 'NONE', #50190, #21047 ) ;
#110625 = ORIENTED_EDGE ( 'NONE', *, *, #30281, .F. ) ;
#110626 = CARTESIAN_POINT ( 'NONE',  ( -11.78247531003460047, 1427.502628522240002, 147.2054527168990035 ) ) ;
#110627 = CARTESIAN_POINT ( 'NONE',  ( 7.548036962157971708, 1510.518062817387090, 203.4501585446919592 ) ) ;
#110628 = FACE_OUTER_BOUND ( 'NONE', #63195, .T. ) ;
#110629 = CARTESIAN_POINT ( 'NONE',  ( 12.90158639592108258, 1434.732194105914914, 147.0409106621408739 ) ) ;
#110630 = CARTESIAN_POINT ( 'NONE',  ( -122.7187414971600674, 1311.832804576489934, 301.8423806000122909 ) ) ;
#110631 = CARTESIAN_POINT ( 'NONE',  ( 17.49001816009999999, 1408.913060387329779, 205.8268510044480024 ) ) ;
#110632 = CARTESIAN_POINT ( 'NONE',  ( -9.110137399830000149, 1384.581616693699971, 199.9614059229390080 ) ) ;
#110633 = CARTESIAN_POINT ( 'NONE',  ( -18.37215797060000000, 1453.313060387329870, 201.1114320114980103 ) ) ;
#110634 = CARTESIAN_POINT ( 'NONE',  ( 4.501691961449999724, 1368.956319095359959, 207.6218459616989946 ) ) ;
#110635 = CARTESIAN_POINT ( 'NONE',  ( -9.352115965572330936, 1447.735190698479983, 210.9908785053780207 ) ) ;
#110636 = CARTESIAN_POINT ( 'NONE',  ( -18.74185279165999773, 1409.000834736390061, 268.9060467476150507 ) ) ;
#110637 = CARTESIAN_POINT ( 'NONE',  ( -13.86100052414289863, 1434.990764548580046, 148.7478939910440090 ) ) ;
#110638 = VERTEX_POINT ( 'NONE', #40674 ) ;
#110639 = CARTESIAN_POINT ( 'NONE',  ( 2.225543501807631053, 1525.712835404586031, 241.5729910383504659 ) ) ;
#110640 = CARTESIAN_POINT ( 'NONE',  ( 13.48810824839999967, 1444.252978269910045, 187.9321459801979870 ) ) ;
#110641 = ORIENTED_EDGE ( 'NONE', *, *, #72662, .T. ) ;
#110642 = ORIENTED_EDGE ( 'NONE', *, *, #72053, .T. ) ;
#110643 = CARTESIAN_POINT ( 'NONE',  ( -5.432410439472700858, 1391.426148861440197, 203.3415300314919989 ) ) ;
#110644 = CARTESIAN_POINT ( 'NONE',  ( 7.814348457125529279, 1424.914214976869971, 194.3898514750090101 ) ) ;
#110645 = CARTESIAN_POINT ( 'NONE',  ( -7.712490991114999694, 1516.666407245520077, 213.7387074786470009 ) ) ;
#110646 = CARTESIAN_POINT ( 'NONE',  ( -15.16872267709999988, 1470.466736689130130, 187.9100041707980040 ) ) ;
#110647 = CARTESIAN_POINT ( 'NONE',  ( 4.026786250540000722, 1408.413060387330006, 121.6099336315979969 ) ) ;
#110648 = ORIENTED_EDGE ( 'NONE', *, *, #49297, .F. ) ;
#110649 = CARTESIAN_POINT ( 'NONE',  ( -76.99707197885047094, 1524.382868172863937, 398.8876973329340672 ) ) ;
#110650 = CARTESIAN_POINT ( 'NONE',  ( 4.613762356885000138, 1516.939574742129935, 203.3372076122869885 ) ) ;
#110651 = CARTESIAN_POINT ( 'NONE',  ( -28.19177135810000223, 1509.605818728229906, 205.1802907371279900 ) ) ;
#110652 = CARTESIAN_POINT ( 'NONE',  ( -1.326199192210000044, 1477.815017677929973, 230.7694779113980132 ) ) ;
#110653 = CARTESIAN_POINT ( 'NONE',  ( -31.38068168340650033, 1384.559508582369972, 206.3649650040269989 ) ) ;
#110654 = CARTESIAN_POINT ( 'NONE',  ( -14.48104889709779997, 1379.655349290230106, 208.1922004443790115 ) ) ;
#110655 = CARTESIAN_POINT ( 'NONE',  ( -13.30361621630000180, 1409.377632903229824, 226.2974586568980158 ) ) ;
#110657 = VERTEX_POINT ( 'NONE', #74848 ) ;
#110656 = CARTESIAN_POINT ( 'NONE',  ( -10.96771875528765428, 1512.594959757391052, 193.2043797466445199 ) ) ;
#110658 = CARTESIAN_POINT ( 'NONE',  ( -26.64852628982920280, 1469.324129686450078, 209.1558146821249977 ) ) ;
#110659 = CARTESIAN_POINT ( 'NONE',  ( 26.16501621689999624, 1469.244469849229972, 211.4985517754080320 ) ) ;
#110660 = CARTESIAN_POINT ( 'NONE',  ( -48.91304988690782807, 1379.688432508924052, 243.6725008576361802 ) ) ;
#110661 = CARTESIAN_POINT ( 'NONE',  ( -9.526128307108560733, 1440.436522615020067, 205.9995050262249947 ) ) ;
#110662 = CARTESIAN_POINT ( 'NONE',  ( -24.98051366310000176, 1436.289130477859999, 137.7795203887980051 ) ) ;
#110663 = CARTESIAN_POINT ( 'NONE',  ( -4.026777524084999449, 1516.718889242609976, 211.4189316860469887 ) ) ;
#110664 = AXIS2_PLACEMENT_3D ( 'NONE', #42793, #7528, #103221 ) ;
#110665 = CARTESIAN_POINT ( 'NONE',  ( -68.15046949569999413, 1379.746499244090046, 278.7918009234589363 ) ) ;
#110666 = B_SPLINE_CURVE_WITH_KNOTS ( 'NONE', 3,
 ( #95589, #18858, #53054, #10484, #28389, #64632, #5816, #91464, #57876, #89803, #83595, #23692 ),
 .UNSPECIFIED., .F., .F.,
 ( 4, 2, 2, 2, 2, 4 ),
 ( -0.1123552058539349918, -0.09789079797621490220, -0.08345975750763819090, -0.05408602645632740180, -0.02844277172931640452, 0.000000000000000000 ),
 .UNSPECIFIED. ) ;
#110667 = CARTESIAN_POINT ( 'NONE',  ( -14.09270673139999985, 1418.021918129430105, 227.3443978055980210 ) ) ;
#110668 = CARTESIAN_POINT ( 'NONE',  ( 8.652776089875690246, 1511.435001055579960, 203.7363227723449768 ) ) ;
#110669 = CARTESIAN_POINT ( 'NONE',  ( -6.949703372784999722, 1517.130100026000036, 208.3827239650380250 ) ) ;
#110670 = EDGE_LOOP ( 'NONE', ( #90597, #3350, #28724, #2870 ) ) ;
#110671 = CARTESIAN_POINT ( 'NONE',  ( -40.71747597329999735, 1438.773003763620181, 134.0999987698980078 ) ) ;
#110672 = CARTESIAN_POINT ( 'NONE',  ( -10.25433319729999759, 1415.365669972130036, 229.7516580550980052 ) ) ;
#110673 = CARTESIAN_POINT ( 'NONE',  ( -19.80317870211088760, 1456.769327258462909, 225.5394267937573716 ) ) ;
#110674 = ORIENTED_EDGE ( 'NONE', *, *, #67834, .F. ) ;
#110675 = CARTESIAN_POINT ( 'NONE',  ( -12.75453511212650071, 1385.302433149910257, 219.0254989633160108 ) ) ;
#110676 = AXIS2_PLACEMENT_3D ( 'NONE', #41061, #81392, #39413 ) ;
#110677 = CARTESIAN_POINT ( 'NONE',  ( -11.57883448593699782, 1491.718296208979837, 205.0404881661760044 ) ) ;
#110678 = CARTESIAN_POINT ( 'NONE',  ( 12.65761277830709908, 1435.514348419339967, 150.7820475295659719 ) ) ;
#110679 = B_SPLINE_SURFACE_WITH_KNOTS ( 'NONE', 5, 5, ( 
 ( #7426, #6865, #15258, #58946, #6327, #108232 ),
 ( #74102, #58397, #65700, #83037, #33171, #99818 ),
 ( #90878, #40477, #23112, #41025, #100912, #66811 ),
 ( #74651, #48351, #56742, #91982, #49448, #83573 ),
 ( #92522, #49991, #108787, #84127, #73556, #101459 ),
 ( #32079, #48909, #14166, #82491, #39934, #30973 ) ),
 .UNSPECIFIED., .F., .F., .F.,
 ( 6, 6 ),
 ( 6, 6 ),
 ( 7.505253243670000352, 8.371505715449998775 ),
 ( 0.000000000000000000, 1.425510291809999996 ),
 .UNSPECIFIED. ) ;
#110680 = CARTESIAN_POINT ( 'NONE',  ( -4.127449627910051433, 1441.471781363327182, 184.1788307560163958 ) ) ;
#110681 = CARTESIAN_POINT ( 'NONE',  ( -15.03953889140000122, 1416.231637368560087, 208.6543985418939826 ) ) ;
#110682 = DIRECTION ( 'NONE',  ( 0.6677681214262592979, -0.7443693545591762994, 0.000000000000000000 ) ) ;
#110683 = CARTESIAN_POINT ( 'NONE',  ( 8.680261597580001265, 1487.719285257089950, 202.4559307200990190 ) ) ;
#110684 = DIRECTION ( 'NONE',  ( 0.3363363969979658030, 0.9417419115949056119, 0.000000000000000000 ) ) ;
#110685 = CARTESIAN_POINT ( 'NONE',  ( -15.05358279999999915, 1410.831827720429828, 226.7261506157979909 ) ) ;
#110687 = CARTESIAN_POINT ( 'NONE',  ( -18.31482527320000031, 1445.278739201789904, 204.5307550449689984 ) ) ;
#110686 = CARTESIAN_POINT ( 'NONE',  ( 2.295485501044999932, 1516.651306816259876, 214.1175719399469983 ) ) ;
#110688 = CIRCLE ( 'NONE', #44529, 1.999999999999996225 ) ;
#110689 = CARTESIAN_POINT ( 'NONE',  ( 19.97269026569999895, 1507.847566758330004, 189.1149477268980093 ) ) ;
#110690 = CARTESIAN_POINT ( 'NONE',  ( -4.616272334694999202, 1517.030858226499959, 216.4568033268070053 ) ) ;
#110691 = VERTEX_POINT ( 'NONE', #108992 ) ;
#110692 = DIRECTION ( 'NONE',  ( -0.6736849260863839728, 0.000000000000000000, 0.7390186874254150995 ) ) ;
#110693 = CARTESIAN_POINT ( 'NONE',  ( 15.97957002059996157, 1409.471061922630497, 193.0247866931977114 ) ) ;
#110694 = VERTEX_POINT ( 'NONE', #66462 ) ;
#110695 = CARTESIAN_POINT ( 'NONE',  ( 1.959361663749999982, 1419.250139722030099, 185.0399661677979850 ) ) ;
#110696 = EDGE_CURVE ( 'NONE', #75973, #59183, #30609, .T. ) ;
#110697 = CIRCLE ( 'NONE', #85675, 3.000000000000002665 ) ;
#110698 =( LENGTH_UNIT ( ) NAMED_UNIT ( * ) SI_UNIT ( .MILLI., .METRE. ) );
#110700 = B_SPLINE_CURVE_WITH_KNOTS ( 'NONE', 3,
 ( #18799, #80939, #105601, #29417, #95528, #70924, #53552, #38372, #27772, #52995, #63080, #4237, #87129, #2048, #88790 ),
 .UNSPECIFIED., .F., .F.,
 ( 4, 2, 2, 1, 1, 1, 2, 2, 4 ),
 ( 0.000000000000000000, 0.2499999999999507061, 0.3749999999999348299, 0.4374999999999256151, 0.4687499999999210076, 0.4843749999999186762, 0.4921874999999189537, 0.4999999999999191758, 1.000000000000000000 ),
 .UNSPECIFIED. ) ;
#110699 = CARTESIAN_POINT ( 'NONE',  ( 2.708195641335804371, 1524.374578187332872, 176.2568186770878356 ) ) ;
#110701 = UNCERTAINTY_MEASURE_WITH_UNIT (LENGTH_MEASURE( 1.000000000000000082E-05 ), #31586, 'distance_accuracy_value', 'NONE');
#110702 = CARTESIAN_POINT ( 'NONE',  ( -30.51231035492526900, 1526.382868172863937, 200.0858385050243555 ) ) ;
#110703 = CARTESIAN_POINT ( 'NONE',  ( 1.823963636610874239, 1416.770504172074197, 232.7531906332400808 ) ) ;
#110704 = CARTESIAN_POINT ( 'NONE',  ( 18.89315557560000158, 1416.535385209229844, 210.0306673353090048 ) ) ;
#110705 = DIRECTION ( 'NONE',  ( 0.2113515706023144647, 0.000000000000000000, 0.9774101051267757301 ) ) ;
#110706 = CARTESIAN_POINT ( 'NONE',  ( 10.41177509810879975, 1460.024667384750046, 205.9063203302740135 ) ) ;
#110707 = EDGE_CURVE ( 'NONE', #44597, #660, #73184, .T. ) ;
#110708 = CARTESIAN_POINT ( 'NONE',  ( -2.471608048749999842, 1438.194204504490017, 150.4833623973980252 ) ) ;
#110709 = CARTESIAN_POINT ( 'NONE',  ( 45.63129791352729825, 1440.913060379180024, 266.1458157647700205 ) ) ;
#110710 = CARTESIAN_POINT ( 'NONE',  ( -12.85636183069170002, 1417.155669274680122, 200.5510948150419779 ) ) ;
#110711 = CARTESIAN_POINT ( 'NONE',  ( 2.737416067801674124, 1524.382868172804365, 241.6058578387444982 ) ) ;
#110712 = ORIENTED_EDGE ( 'NONE', *, *, #56860, .F. ) ;
#110713 = ORIENTED_EDGE ( 'NONE', *, *, #13323, .T. ) ;
#110714 = DIRECTION ( 'NONE',  ( 0.9858563016923833633, 0.000000000000000000, 0.1675928173085483863 ) ) ;
#110715 = CARTESIAN_POINT ( 'NONE',  ( -19.87678393280335243, 1484.439226788044152, 191.0985201580460000 ) ) ;
#110716 = LINE ( 'NONE', #51361, #91384 ) ;
#110717 = CARTESIAN_POINT ( 'NONE',  ( 12.90804412569774762, 1410.732742728818266, 190.4223191256656094 ) ) ;
#110718 = AXIS2_PLACEMENT_3D ( 'NONE', #23405, #107964, #82769 ) ;
#110719 = CARTESIAN_POINT ( 'NONE',  ( -10.49767250057509926, 1480.215366257469896, 208.4046347607720122 ) ) ;
#110720 = B_SPLINE_SURFACE_WITH_KNOTS ( 'NONE', 4, 5, ( 
 ( #91341, #81821, #98627, #21894, #5124, #39280 ),
 ( #21349, #73455, #74556, #99718, #31424, #14063 ),
 ( #55556, #107586, #89681, #40378, #14623, #90220 ),
 ( #23572, #5692, #108689, #48252, #91884, #13505 ),
 ( #15157, #31981, #39836, #57765, #98078, #30872 ) ),
 .UNSPECIFIED., .F., .F., .F.,
 ( 5, 5 ),
 ( 6, 6 ),
 ( 23.77038316910000049, 36.72447201482209778 ),
 ( -0.0002035811339858509933, 2.000203581245860285 ),
 .UNSPECIFIED. ) ;
#110721 = CARTESIAN_POINT ( 'NONE',  ( 29.61692403811556673, 1526.104292489129421, 220.7563138442888828 ) ) ;
#110722 = LINE ( 'NONE', #17173, #21810 ) ;
#110723 = CARTESIAN_POINT ( 'NONE',  ( -4.138993644619999301, 1515.551749209489799, 209.1218459617069811 ) ) ;
#110724 = CARTESIAN_POINT ( 'NONE',  ( -54.89834970837709704, 1383.804077747929796, 271.2376706240149815 ) ) ;
#110725 = CARTESIAN_POINT ( 'NONE',  ( 6.976610649730000446, 1452.669431775030034, 151.9927557690980109 ) ) ;
#110726 = CARTESIAN_POINT ( 'NONE',  ( 0.1681674884180490159, 1420.473121907760060, 182.7464979049940155 ) ) ;
#110728 = ADVANCED_FACE ( 'NONE', ( #33360, #51847 ), #17646, .F. ) ;
#110727 = CARTESIAN_POINT ( 'NONE',  ( 11.45382141796380004, 1491.761286053230151, 209.6395483024749922 ) ) ;
#110730 = ORIENTED_EDGE ( 'NONE', *, *, #31026, .F. ) ;
#110729 = CARTESIAN_POINT ( 'NONE',  ( 24.06669976739999939, 1509.724642860830045, 193.1379647362979881 ) ) ;
#110731 = CARTESIAN_POINT ( 'NONE',  ( 34.31402925621713962, 1524.244163922423695, 218.0340858097454202 ) ) ;
#110732 = CARTESIAN_POINT ( 'NONE',  ( -57.27373091850000009, 1381.636262940560073, 240.5709706821589862 ) ) ;
#110733 = CARTESIAN_POINT ( 'NONE',  ( -16.48213017202440156, 1409.488629055829961, 224.5375925732930114 ) ) ;
#110734 = EDGE_LOOP ( 'NONE', ( #30023, #14534, #89024, #30473, #74836, #48441, #32441, #32034, #1630, #31798 ) ) ;
#110735 = ORIENTED_EDGE ( 'NONE', *, *, #99829, .F. ) ;
#110736 = CARTESIAN_POINT ( 'NONE',  ( 12.20364748979999980, 1447.059433187239847, 188.0531537431980098 ) ) ;
#110737 = DIRECTION ( 'NONE',  ( 1.402715769532790202E-14, -1.000000000000000000, 4.930380657631320281E-31 ) ) ;
#110738 = CARTESIAN_POINT ( 'NONE',  ( 40.13353682310170001, 1442.269293553509897, 136.9628395507569962 ) ) ;
#110740 = CARTESIAN_POINT ( 'NONE',  ( 31.34137657934008558, 1523.481610426287716, 196.3411265156547358 ) ) ;
#110739 = DIRECTION ( 'NONE',  ( 1.755985294532464991E-16, -1.000000000000000000, 1.338183447452830017E-16 ) ) ;
#110741 = CARTESIAN_POINT ( 'NONE',  ( 11.62073329257960097, 1480.091610248069856, 211.1128523392590068 ) ) ;
#110742 = CARTESIAN_POINT ( 'NONE',  ( -107.5634112720000104, 1382.701802836779962, 297.7923862875589975 ) ) ;
#110743 = CARTESIAN_POINT ( 'NONE',  ( 7.211935934568218798, 1517.051704408389924, 224.6757451961901495 ) ) ;
#110744 = CARTESIAN_POINT ( 'NONE',  ( -12.64492061617493235, 1435.846068781982012, 150.8967598469849065 ) ) ;
#110745 = CARTESIAN_POINT ( 'NONE',  ( -21.83550407203883736, 1523.678648413191695, 234.9693198511253627 ) ) ;
#110746 = B_SPLINE_CURVE_WITH_KNOTS ( 'NONE', 3,
 ( #90071, #38035, #72215, #20120, #82235, #80036, #106337, #64357, #55401, #73855, #3358, #99021, #89533, #4443, #13352, #41890, #16112 ),
 .UNSPECIFIED., .F., .F.,
 ( 4, 2, 2, 2, 2, 1, 2, 2, 4 ),
 ( 0.000000000000000000, 0.2499999999999915623, 0.3749999999999957812, 0.5000000000000000000, 0.6250000000000042188, 0.6875000000000049960, 0.7187500000000053291, 0.7500000000000057732, 1.000000000000000000 ),
 .UNSPECIFIED. ) ;
#110747 = CARTESIAN_POINT ( 'NONE',  ( 5.118312429449999534, 1409.258938051830000, 187.0063209343980191 ) ) ;
#110748 = CARTESIAN_POINT ( 'NONE',  ( 4.527354660830000377, 1423.822069290730269, 184.4238519299979941 ) ) ;
#110749 = CARTESIAN_POINT ( 'NONE',  ( -7.404094510329910506, 1512.905891558379153, 200.7965695454380750 ) ) ;
#110750 = CARTESIAN_POINT ( 'NONE',  ( -3.141092941611050016, 1440.712674293340115, 157.0493854566300058 ) ) ;
#110751 = VECTOR ( 'NONE', #69683, 999.9999999999998863 ) ;
#110752 = CARTESIAN_POINT ( 'NONE',  ( -2.338064766694980090, 1451.283254387899888, 184.5359555560359865 ) ) ;
#110753 = CARTESIAN_POINT ( 'NONE',  ( 1.406054942129999930, 1464.967845642129987, 236.6417686339979980 ) ) ;
#110754 = ORIENTED_EDGE ( 'NONE', *, *, #40817, .F. ) ;
#110755 = CARTESIAN_POINT ( 'NONE',  ( 20.38160163584860030, 1475.532940563729881, 217.9568059512479863 ) ) ;
#110756 = CARTESIAN_POINT ( 'NONE',  ( -1.628202555219999903, 1430.465083930730088, 150.2970716576980124 ) ) ;
#110757 = CARTESIAN_POINT ( 'NONE',  ( -18.02257621027615642, 1524.382868172863937, 182.8951942368373977 ) ) ;
#110758 = DIRECTION ( 'NONE',  ( 0.000000000000000000, 1.000000000000000000, 0.000000000000000000 ) ) ;
#110759 = CARTESIAN_POINT ( 'NONE',  ( 15.53740313620000180, 1449.513310617089928, 190.1957215746979841 ) ) ;
#110760 = CIRCLE ( 'NONE', #10704, 3.000000000000002665 ) ;
#110761 = CARTESIAN_POINT ( 'NONE',  ( -2.034934016457660169E-12, 1470.108503626060156, 254.3105774012479685 ) ) ;
#110762 = CARTESIAN_POINT ( 'NONE',  ( -19.90677659085769946, 1485.410772266320237, 191.0396054904460073 ) ) ;
#110763 = CARTESIAN_POINT ( 'NONE',  ( -1.226570660889999997, 1415.553739809529816, 227.5749953283980176 ) ) ;
#110764 = CARTESIAN_POINT ( 'NONE',  ( -6.356242932690000735, 1416.544486832730172, 231.6503315779980028 ) ) ;
#110765 = CARTESIAN_POINT ( 'NONE',  ( -0.6851706257419990509, 1475.635431348089924, 197.6580713075989877 ) ) ;
#110766 = CARTESIAN_POINT ( 'NONE',  ( -105.7479675089999915, 1388.624540799249871, 309.0709673806589990 ) ) ;
#110767 = CARTESIAN_POINT ( 'NONE',  ( -0.5856906059243432994, 1485.491362865349402, 181.9191849365466283 ) ) ;
#110768 = CARTESIAN_POINT ( 'NONE',  ( 4.262353028403936150, 1360.811275533940034, 210.6218459616991936 ) ) ;
#110769 = CARTESIAN_POINT ( 'NONE',  ( -45.80170866997659829, 1439.242720596339950, 268.7579477620919874 ) ) ;
#110770 = CARTESIAN_POINT ( 'NONE',  ( 13.69935640180099945, 1509.078849000180071, 233.8886703240220015 ) ) ;
#110771 = CARTESIAN_POINT ( 'NONE',  ( -13.04908991647894290, 1414.913372219064286, 220.1077748470152642 ) ) ;
#110772 = EDGE_LOOP ( 'NONE', ( #44834, #35516 ) ) ;
#110773 = CARTESIAN_POINT ( 'NONE',  ( 1.704170714124999986, 1516.927039499179955, 208.3639196453299860 ) ) ;
#110774 = CARTESIAN_POINT ( 'NONE',  ( -2.478470422270000029, 1437.832529885160056, 157.6963859361979985 ) ) ;
#110775 = CARTESIAN_POINT ( 'NONE',  ( -6.647957898892952855, 1470.949127383563791, 216.7466839929853677 ) ) ;
#110776 = CARTESIAN_POINT ( 'NONE',  ( 7.490783964907898884, 1426.014963415389957, 212.3433401526569924 ) ) ;
#110777 = TOROIDAL_SURFACE ( 'NONE', #14213, 30.13701971169416538, 3.000000000000000000 ) ;
#110778 = CARTESIAN_POINT ( 'NONE',  ( -26.78870495038239952, 1451.977601232150164, 134.9148139021100121 ) ) ;
#110779 = ORIENTED_EDGE ( 'NONE', *, *, #68000, .T. ) ;
#110780 = CARTESIAN_POINT ( 'NONE',  ( 4.694071620149999902, 1416.682256071730080, 238.2947578313980159 ) ) ;
#110782 = CARTESIAN_POINT ( 'NONE',  ( -15.25249362911780082, 1513.170547669029929, 223.2087981395630152 ) ) ;
#110781 = CARTESIAN_POINT ( 'NONE',  ( -3.062921356683425245, 1525.320849883635901, 176.8368074866138215 ) ) ;
#110783 = CARTESIAN_POINT ( 'NONE',  ( -1.793335950739999962, 1419.496365638530051, 185.6406336190979971 ) ) ;
#110784 = CARTESIAN_POINT ( 'NONE',  ( 7.894362808210001248, 1424.028044848189893, 212.1595859666189767 ) ) ;
#110785 = CARTESIAN_POINT ( 'NONE',  ( 4.103915387205919529, 1467.926924930979794, 218.2234441087299786 ) ) ;
#110786 = DIRECTION ( 'NONE',  ( -0.3090169943749383474, -0.000000000000000000, 0.9510565162951566398 ) ) ;
#110787 = ORIENTED_EDGE ( 'NONE', *, *, #51620, .T. ) ;
#110788 = CARTESIAN_POINT ( 'NONE',  ( -6.618142395782879994, 1410.137584300400022, 270.0732991173869664 ) ) ;
#110789 = CARTESIAN_POINT ( 'NONE',  ( 10.63558804199830021, 1419.812302066319944, 231.2733509599579804 ) ) ;
#110790 = CARTESIAN_POINT ( 'NONE',  ( 8.379013882420577985, 1435.477853948120128, 206.7290831433529661 ) ) ;
#110791 = ORIENTED_EDGE ( 'NONE', *, *, #53610, .T. ) ;
#110792 = VERTEX_POINT ( 'NONE', #85984 ) ;
#110793 = CARTESIAN_POINT ( 'NONE',  ( -22.62006121466300002, 1409.702956284340189, 209.3923079909519913 ) ) ;
#110794 = CARTESIAN_POINT ( 'NONE',  ( -4.447601775919999945, 1425.243076475230282, 186.2019964394980036 ) ) ;
#110795 = DIRECTION ( 'NONE',  ( -0.1070030146457454923, 0.000000000000000000, -0.9942586961433741433 ) ) ;
#110796 = AXIS2_PLACEMENT_3D ( 'NONE', #82386, #56638, #29228 ) ;
#110797 = CARTESIAN_POINT ( 'NONE',  ( -45.56249212406897442, 1438.493842798003470, 266.1916403547691061 ) ) ;
#110798 = ADVANCED_BREP_SHAPE_REPRESENTATION ( '', ( #84353, #21632 ), #103904 ) ;
#110799 = CARTESIAN_POINT ( 'NONE',  ( -21.03123196678649975, 1507.789098018889945, 192.1781278620359785 ) ) ;
#110800 = CARTESIAN_POINT ( 'NONE',  ( 4.679791025795809745, 1508.610720109290014, 212.2979026938089930 ) ) ;
#110801 = CARTESIAN_POINT ( 'NONE',  ( 41.02605310493780166, 1456.755636601169954, 268.6565615534370295 ) ) ;
#110802 = CARTESIAN_POINT ( 'NONE',  ( -4.832613814269110186, 1508.551704408389924, 205.6342607178579840 ) ) ;
#110803 = CARTESIAN_POINT ( 'NONE',  ( -4.827292224569999846, 1429.041575181189955, 202.2878225452089964 ) ) ;
#110804 = CARTESIAN_POINT ( 'NONE',  ( 4.609673241434999902, 1516.754149861460064, 205.8564388142570181 ) ) ;
#110805 = ORIENTED_EDGE ( 'NONE', *, *, #33532, .T. ) ;
#110806 = CARTESIAN_POINT ( 'NONE',  ( 18.43151930343191580, 1458.912353611211984, 227.6950766328336329 ) ) ;
#110807 = CARTESIAN_POINT ( 'NONE',  ( 1.636696423147410151, 1445.551428100869998, 199.1693562641009976 ) ) ;
#110808 = DIRECTION ( 'NONE',  ( -0.9455185755993178454, 0.000000000000000000, 0.3255681544571539243 ) ) ;
#110809 = ORIENTED_EDGE ( 'NONE', *, *, #12603, .F. ) ;
#110811 = TOROIDAL_SURFACE ( 'NONE', #96525, 7.499828603750000156, 0.5000000000000000000 ) ;
#110810 = CARTESIAN_POINT ( 'NONE',  ( -11.71878239930389931, 1481.302890658779916, 210.8565630715119994 ) ) ;
#110812 = CARTESIAN_POINT ( 'NONE',  ( 27.02366518750249824, 1451.037975853650096, 136.3590651249419921 ) ) ;
#110813 = CARTESIAN_POINT ( 'NONE',  ( -3.856607047483139983, 1508.551704408389924, 213.7021005842219949 ) ) ;
#110814 = CARTESIAN_POINT ( 'NONE',  ( -6.355004502469999927, 1386.605327393260040, 199.7233850259690087 ) ) ;
#110815 = CARTESIAN_POINT ( 'NONE',  ( 7.682163124739999738, 1421.658071144350060, 195.7645034974990210 ) ) ;
#110817 = B_SPLINE_SURFACE_WITH_KNOTS ( 'NONE', 5, 1, ( 
 ( #58674, #67635 ),
 ( #92809, #25035 ),
 ( #50286, #36642 ),
 ( #54576, #19825 ),
 ( #79212, #70838 ),
 ( #37746, #88711 ) ),
 .UNSPECIFIED., .F., .F., .F.,
 ( 6, 6 ),
 ( 2, 2 ),
 ( 0.000000000000000000, 3.542454554009999868 ),
 ( 0.000000000000000000, 14.00000000000000000 ),
 .UNSPECIFIED. ) ;
#110816 = CARTESIAN_POINT ( 'NONE',  ( -3.220674668504990290, 1433.265634988960073, 218.1214075394389909 ) ) ;
#110818 = CARTESIAN_POINT ( 'NONE',  ( -3.617578910780000268, 1497.333807970789849, 198.4503654230989866 ) ) ;
#110819 = CARTESIAN_POINT ( 'NONE',  ( 9.139323887128899315, 1409.232212610100078, 189.8042143963789954 ) ) ;
#110821 = CARTESIAN_POINT ( 'NONE',  ( 11.60004869885203682, 1411.254281879943164, 135.5999999980979851 ) ) ;
#110820 = CARTESIAN_POINT ( 'NONE',  ( 30.12464261468161197, 1524.523992613102564, 195.8613510089864747 ) ) ;
#110822 = CARTESIAN_POINT ( 'NONE',  ( 15.60455980150000066, 1409.457983623130076, 225.4781096464980124 ) ) ;
#110823 = CARTESIAN_POINT ( 'NONE',  ( -13.88938984930000053, 1379.665435272789864, 212.4763918038889869 ) ) ;
#110824 = CARTESIAN_POINT ( 'NONE',  ( 14.83523515338253418, 1422.059756969527143, 230.2894810269289394 ) ) ;
#110825 = ORIENTED_EDGE ( 'NONE', *, *, #17348, .F. ) ;
#110826 = CARTESIAN_POINT ( 'NONE',  ( 11.29419939621850055, 1414.913057855109855, 221.1598003036660032 ) ) ;
#110827 = CARTESIAN_POINT ( 'NONE',  ( 4.930158634465010792, 1484.410507904570068, 219.1064042044509392 ) ) ;
#110828 = CARTESIAN_POINT ( 'NONE',  ( -10.30348281067860050, 1483.409064405780100, 203.1509397556989995 ) ) ;
#110829 = B_SPLINE_SURFACE_WITH_KNOTS ( 'NONE', 5, 5, ( 
 ( #32107, #68487, #7999, #66293, #100409, #23693 ),
 ( #57878, #110466, #49474, #92011, #32657, #33744 ),
 ( #15281, #67939, #83596, #6895, #41051, #66834 ),
 ( #58421, #727, #78531, #104279, #26450, #86920 ),
 ( #96433, #1276, #9111, #79647, #2951, #70716 ),
 ( #77969, #104830, #37070, #1842, #10211, #60643 ) ),
 .UNSPECIFIED., .F., .F., .F.,
 ( 6, 6 ),
 ( 6, 6 ),
 ( 78.04565204464360306, 167.5290185466710113 ),
 ( -0.0009444657940283349628, 2.000944465795519989 ),
 .UNSPECIFIED. ) ;
#110830 = CARTESIAN_POINT ( 'NONE',  ( -13.43109441729999887, 1390.552119206370207, 208.3926299382939931 ) ) ;
#110831 = CARTESIAN_POINT ( 'NONE',  ( -10.15848451741849878, 1462.015496030800023, 208.6817910193179841 ) ) ;
#110832 = NEXT_ASSEMBLY_USAGE_OCCURRENCE ( 'NAUO1', ' ', ' ', #31601, #25390, $ ) ;
#110833 = NEXT_ASSEMBLY_USAGE_OCCURRENCE ( 'NAUO2', ' ', ' ', #31601, #82922, $ ) ;
#110834 = NEXT_ASSEMBLY_USAGE_OCCURRENCE ( 'NAUO3', ' ', ' ', #31601, #102745, $ ) ;
#110835 = NEXT_ASSEMBLY_USAGE_OCCURRENCE ( 'NAUO4', ' ', ' ', #31601, #93161, $ ) ;
#110836 = NEXT_ASSEMBLY_USAGE_OCCURRENCE ( 'NAUO5', ' ', ' ', #31601, #21967, $ ) ;
#110837 = NEXT_ASSEMBLY_USAGE_OCCURRENCE ( 'NAUO6', ' ', ' ', #31601, #41841, $ ) ;
#110838 = NEXT_ASSEMBLY_USAGE_OCCURRENCE ( 'NAUO7', ' ', ' ', #31601, #61723, $ ) ;
#110839 = NEXT_ASSEMBLY_USAGE_OCCURRENCE ( 'NAUO8', ' ', ' ', #31601, #11756, $ ) ;
#110840 = NEXT_ASSEMBLY_USAGE_OCCURRENCE ( 'NAUO9', ' ', ' ', #31601, #63131, $ ) ;
ENDSEC;
END-ISO-10303-21;
